#108957=AXIS2_PLACEMENT_3D('',#247452,#135985,#135986);
#108958=AXIS2_PLACEMENT_3D('',#247453,#135987,#135988);
#108959=AXIS2_PLACEMENT_3D('',#247454,#135989,#135990);
#108960=AXIS2_PLACEMENT_3D('',#247455,#135991,#135992);
#108961=AXIS2_PLACEMENT_3D('',#247456,#135993,#135994);
#108962=AXIS2_PLACEMENT_3D('',#247469,#135995,#135996);
#108963=AXIS2_PLACEMENT_3D('',#247470,#135997,#135998);
#108964=AXIS2_PLACEMENT_3D('',#247471,#135999,#136000);
#108965=AXIS2_PLACEMENT_3D('',#247472,#136001,#136002);
#108966=AXIS2_PLACEMENT_3D('',#247473,#136003,#136004);
#108967=AXIS2_PLACEMENT_3D('',#247486,#136005,#136006);
#108968=AXIS2_PLACEMENT_3D('',#247499,#136007,#136008);
#108969=AXIS2_PLACEMENT_3D('',#247500,#136009,#136010);
#108970=AXIS2_PLACEMENT_3D('',#247501,#136011,#136012);
#108971=AXIS2_PLACEMENT_3D('',#247502,#136013,#136014);
#108972=AXIS2_PLACEMENT_3D('',#247503,#136015,#136016);
#108973=AXIS2_PLACEMENT_3D('',#247522,#136017,#136018);
#108974=AXIS2_PLACEMENT_3D('',#247523,#136019,#136020);
#108975=AXIS2_PLACEMENT_3D('',#247524,#136021,#136022);
#108976=AXIS2_PLACEMENT_3D('',#247525,#136023,#136024);
#108977=AXIS2_PLACEMENT_3D('',#247526,#136025,#136026);
#108978=AXIS2_PLACEMENT_3D('',#247539,#136027,#136028);
#108979=AXIS2_PLACEMENT_3D('',#247558,#136029,#136030);
#108980=AXIS2_PLACEMENT_3D('',#247559,#136031,#136032);
#108981=AXIS2_PLACEMENT_3D('',#247560,#136033,#136034);
#108982=AXIS2_PLACEMENT_3D('',#247561,#136035,#136036);
#108983=AXIS2_PLACEMENT_3D('',#247562,#136037,#136038);
#108984=AXIS2_PLACEMENT_3D('',#247581,#136039,#136040);
#108985=AXIS2_PLACEMENT_3D('',#247594,#136041,#136042);
#108986=AXIS2_PLACEMENT_3D('',#247595,#136043,#136044);
#108987=AXIS2_PLACEMENT_3D('',#247596,#136045,#136046);
#108988=AXIS2_PLACEMENT_3D('',#247597,#136047,#136048);
#108989=AXIS2_PLACEMENT_3D('',#247598,#136049,#136050);
#108990=AXIS2_PLACEMENT_3D('',#247617,#136051,#136052);
#108991=AXIS2_PLACEMENT_3D('',#247618,#136053,#136054);
#108992=AXIS2_PLACEMENT_3D('',#247619,#136055,#136056);
#108993=AXIS2_PLACEMENT_3D('',#247620,#136057,#136058);
#108994=AXIS2_PLACEMENT_3D('',#247621,#136059,#136060);
#108995=AXIS2_PLACEMENT_3D('',#247634,#136061,#136062);
#108996=AXIS2_PLACEMENT_3D('',#247647,#136063,#136064);
#108997=AXIS2_PLACEMENT_3D('',#247648,#136065,#136066);
#108998=AXIS2_PLACEMENT_3D('',#247649,#136067,#136068);
#108999=AXIS2_PLACEMENT_3D('',#247650,#136069,#136070);
#109000=AXIS2_PLACEMENT_3D('',#247651,#136071,#136072);
#109001=AXIS2_PLACEMENT_3D('',#247664,#136073,#136074);
#109002=AXIS2_PLACEMENT_3D('',#247665,#136075,#136076);
#109003=AXIS2_PLACEMENT_3D('',#247666,#136077,#136078);
#109004=AXIS2_PLACEMENT_3D('',#247667,#136079,#136080);
#109005=AXIS2_PLACEMENT_3D('',#247668,#136081,#136082);
#109006=AXIS2_PLACEMENT_3D('',#247681,#136083,#136084);
#109007=AXIS2_PLACEMENT_3D('',#247682,#136085,#136086);
#109008=AXIS2_PLACEMENT_3D('',#247683,#136087,#136088);
#109009=AXIS2_PLACEMENT_3D('',#247684,#136089,#136090);
#109010=AXIS2_PLACEMENT_3D('',#247685,#136091,#136092);
#109011=AXIS2_PLACEMENT_3D('',#247698,#136093,#136094);
#109012=AXIS2_PLACEMENT_3D('',#247711,#136095,#136096);
#109013=AXIS2_PLACEMENT_3D('',#247712,#136097,#136098);
#109014=AXIS2_PLACEMENT_3D('',#247713,#136099,#136100);
#109015=AXIS2_PLACEMENT_3D('',#247714,#136101,#136102);
#109016=AXIS2_PLACEMENT_3D('',#247715,#136103,#136104);
#109017=AXIS2_PLACEMENT_3D('',#247734,#136105,#136106);
#109018=AXIS2_PLACEMENT_3D('',#247735,#136107,#136108);
#109019=AXIS2_PLACEMENT_3D('',#247736,#136109,#136110);
#109020=AXIS2_PLACEMENT_3D('',#247737,#136111,#136112);
#109021=AXIS2_PLACEMENT_3D('',#247738,#136113,#136114);
#109022=AXIS2_PLACEMENT_3D('',#247751,#136115,#136116);
#109023=AXIS2_PLACEMENT_3D('',#247770,#136117,#136118);
#109024=AXIS2_PLACEMENT_3D('',#247771,#136119,#136120);
#109025=AXIS2_PLACEMENT_3D('',#247772,#136121,#136122);
#109026=AXIS2_PLACEMENT_3D('',#247773,#136123,#136124);
#109027=AXIS2_PLACEMENT_3D('',#247774,#136125,#136126);
#109028=AXIS2_PLACEMENT_3D('',#247793,#136127,#136128);
#109029=AXIS2_PLACEMENT_3D('',#247806,#136129,#136130);
#109030=AXIS2_PLACEMENT_3D('',#247807,#136131,#136132);
#109031=AXIS2_PLACEMENT_3D('',#247808,#136133,#136134);
#109032=AXIS2_PLACEMENT_3D('',#247809,#136135,#136136);
#109033=AXIS2_PLACEMENT_3D('',#247810,#136137,#136138);
#109034=AXIS2_PLACEMENT_3D('',#247829,#136139,#136140);
#109035=AXIS2_PLACEMENT_3D('',#247830,#136141,#136142);
#109036=AXIS2_PLACEMENT_3D('',#247831,#136143,#136144);
#109037=AXIS2_PLACEMENT_3D('',#247832,#136145,#136146);
#109038=AXIS2_PLACEMENT_3D('',#247833,#136147,#136148);
#109039=AXIS2_PLACEMENT_3D('',#247846,#136149,#136150);
#109040=AXIS2_PLACEMENT_3D('',#247859,#136151,#136152);
#109041=AXIS2_PLACEMENT_3D('',#247860,#136153,#136154);
#109042=AXIS2_PLACEMENT_3D('',#247861,#136155,#136156);
#109043=AXIS2_PLACEMENT_3D('',#247862,#136157,#136158);
#109044=AXIS2_PLACEMENT_3D('',#247863,#136159,#136160);
#109045=AXIS2_PLACEMENT_3D('',#247876,#136161,#136162);
#109046=AXIS2_PLACEMENT_3D('',#247877,#136163,#136164);
#109047=AXIS2_PLACEMENT_3D('',#247878,#136165,#136166);
#109048=AXIS2_PLACEMENT_3D('',#247879,#136167,#136168);
#109049=AXIS2_PLACEMENT_3D('',#247880,#136169,#136170);
#109050=AXIS2_PLACEMENT_3D('',#247893,#136171,#136172);
#109051=AXIS2_PLACEMENT_3D('',#247894,#136173,#136174);
#109052=AXIS2_PLACEMENT_3D('',#247895,#136175,#136176);
#109053=AXIS2_PLACEMENT_3D('',#247896,#136177,#136178);
#109054=AXIS2_PLACEMENT_3D('',#247897,#136179,#136180);
#109055=AXIS2_PLACEMENT_3D('',#247910,#136181,#136182);
#109056=AXIS2_PLACEMENT_3D('',#247923,#136183,#136184);
#109057=AXIS2_PLACEMENT_3D('',#247924,#136185,#136186);
#109058=AXIS2_PLACEMENT_3D('',#247925,#136187,#136188);
#109059=AXIS2_PLACEMENT_3D('',#247926,#136189,#136190);
#109060=AXIS2_PLACEMENT_3D('',#247927,#136191,#136192);
#109061=AXIS2_PLACEMENT_3D('',#247946,#136193,#136194);
#109062=AXIS2_PLACEMENT_3D('',#247947,#136195,#136196);
#109063=AXIS2_PLACEMENT_3D('',#247948,#136197,#136198);
#109064=AXIS2_PLACEMENT_3D('',#247949,#136199,#136200);
#109065=AXIS2_PLACEMENT_3D('',#247950,#136201,#136202);
#109066=AXIS2_PLACEMENT_3D('',#247963,#136203,#136204);
#109067=AXIS2_PLACEMENT_3D('',#247982,#136205,#136206);
#109068=AXIS2_PLACEMENT_3D('',#247983,#136207,#136208);
#109069=AXIS2_PLACEMENT_3D('',#247984,#136209,#136210);
#109070=AXIS2_PLACEMENT_3D('',#247985,#136211,#136212);
#109071=AXIS2_PLACEMENT_3D('',#247986,#136213,#136214);
#109072=AXIS2_PLACEMENT_3D('',#248005,#136215,#136216);
#109073=AXIS2_PLACEMENT_3D('',#248018,#136217,#136218);
#109074=AXIS2_PLACEMENT_3D('',#248019,#136219,#136220);
#109075=AXIS2_PLACEMENT_3D('',#248020,#136221,#136222);
#109076=AXIS2_PLACEMENT_3D('',#248021,#136223,#136224);
#109077=AXIS2_PLACEMENT_3D('',#248022,#136225,#136226);
#109078=AXIS2_PLACEMENT_3D('',#248041,#136227,#136228);
#109079=AXIS2_PLACEMENT_3D('',#248042,#136229,#136230);
#109080=AXIS2_PLACEMENT_3D('',#248043,#136231,#136232);
#109081=AXIS2_PLACEMENT_3D('',#248044,#136233,#136234);
#109082=AXIS2_PLACEMENT_3D('',#248045,#136235,#136236);
#109083=AXIS2_PLACEMENT_3D('',#248058,#136237,#136238);
#109084=AXIS2_PLACEMENT_3D('',#248071,#136239,#136240);
#109085=AXIS2_PLACEMENT_3D('',#248072,#136241,#136242);
#109086=AXIS2_PLACEMENT_3D('',#248073,#136243,#136244);
#109087=AXIS2_PLACEMENT_3D('',#248074,#136245,#136246);
#109088=AXIS2_PLACEMENT_3D('',#248075,#136247,#136248);
#109089=AXIS2_PLACEMENT_3D('',#248088,#136249,#136250);
#109090=AXIS2_PLACEMENT_3D('',#248089,#136251,#136252);
#109091=AXIS2_PLACEMENT_3D('',#248090,#136253,#136254);
#109092=AXIS2_PLACEMENT_3D('',#248091,#136255,#136256);
#109093=AXIS2_PLACEMENT_3D('',#248092,#136257,#136258);
#109094=AXIS2_PLACEMENT_3D('',#248105,#136259,#136260);
#109095=AXIS2_PLACEMENT_3D('',#248106,#136261,#136262);
#109096=AXIS2_PLACEMENT_3D('',#248107,#136263,#136264);
#109097=AXIS2_PLACEMENT_3D('',#248108,#136265,#136266);
#109098=AXIS2_PLACEMENT_3D('',#248109,#136267,#136268);
#109099=AXIS2_PLACEMENT_3D('',#248122,#136269,#136270);
#109100=AXIS2_PLACEMENT_3D('',#248135,#136271,#136272);
#109101=AXIS2_PLACEMENT_3D('',#248136,#136273,#136274);
#109102=AXIS2_PLACEMENT_3D('',#248137,#136275,#136276);
#109103=AXIS2_PLACEMENT_3D('',#248138,#136277,#136278);
#109104=AXIS2_PLACEMENT_3D('',#248139,#136279,#136280);
#109105=AXIS2_PLACEMENT_3D('',#248158,#136281,#136282);
#109106=AXIS2_PLACEMENT_3D('',#248159,#136283,#136284);
#109107=AXIS2_PLACEMENT_3D('',#248160,#136285,#136286);
#109108=AXIS2_PLACEMENT_3D('',#248161,#136287,#136288);
#109109=AXIS2_PLACEMENT_3D('',#248162,#136289,#136290);
#109110=AXIS2_PLACEMENT_3D('',#248175,#136291,#136292);
#109111=AXIS2_PLACEMENT_3D('',#248194,#136293,#136294);
#109112=AXIS2_PLACEMENT_3D('',#248195,#136295,#136296);
#109113=AXIS2_PLACEMENT_3D('',#248196,#136297,#136298);
#109114=AXIS2_PLACEMENT_3D('',#248197,#136299,#136300);
#109115=AXIS2_PLACEMENT_3D('',#248198,#136301,#136302);
#109116=AXIS2_PLACEMENT_3D('',#248217,#136303,#136304);
#109117=AXIS2_PLACEMENT_3D('',#248230,#136305,#136306);
#109118=AXIS2_PLACEMENT_3D('',#248231,#136307,#136308);
#109119=AXIS2_PLACEMENT_3D('',#248232,#136309,#136310);
#109120=AXIS2_PLACEMENT_3D('',#248233,#136311,#136312);
#109121=AXIS2_PLACEMENT_3D('',#248234,#136313,#136314);
#109122=AXIS2_PLACEMENT_3D('',#248253,#136315,#136316);
#109123=AXIS2_PLACEMENT_3D('',#248254,#136317,#136318);
#109124=AXIS2_PLACEMENT_3D('',#248255,#136319,#136320);
#109125=AXIS2_PLACEMENT_3D('',#248256,#136321,#136322);
#109126=AXIS2_PLACEMENT_3D('',#248257,#136323,#136324);
#109127=AXIS2_PLACEMENT_3D('',#248270,#136325,#136326);
#109128=AXIS2_PLACEMENT_3D('',#248283,#136327,#136328);
#109129=AXIS2_PLACEMENT_3D('',#248284,#136329,#136330);
#109130=AXIS2_PLACEMENT_3D('',#248285,#136331,#136332);
#109131=AXIS2_PLACEMENT_3D('',#248286,#136333,#136334);
#109132=AXIS2_PLACEMENT_3D('',#248287,#136335,#136336);
#109133=AXIS2_PLACEMENT_3D('',#248300,#136337,#136338);
#109134=AXIS2_PLACEMENT_3D('',#248301,#136339,#136340);
#109135=AXIS2_PLACEMENT_3D('',#248302,#136341,#136342);
#109136=AXIS2_PLACEMENT_3D('',#248303,#136343,#136344);
#109137=AXIS2_PLACEMENT_3D('',#248304,#136345,#136346);
#109138=AXIS2_PLACEMENT_3D('',#248317,#136347,#136348);
#109139=AXIS2_PLACEMENT_3D('',#248318,#136349,#136350);
#109140=AXIS2_PLACEMENT_3D('',#248319,#136351,#136352);
#109141=AXIS2_PLACEMENT_3D('',#248320,#136353,#136354);
#109142=AXIS2_PLACEMENT_3D('',#248321,#136355,#136356);
#109143=AXIS2_PLACEMENT_3D('',#248334,#136357,#136358);
#109144=AXIS2_PLACEMENT_3D('',#248347,#136359,#136360);
#109145=AXIS2_PLACEMENT_3D('',#248348,#136361,#136362);
#109146=AXIS2_PLACEMENT_3D('',#248349,#136363,#136364);
#109147=AXIS2_PLACEMENT_3D('',#248350,#136365,#136366);
#109148=AXIS2_PLACEMENT_3D('',#248351,#136367,#136368);
#109149=AXIS2_PLACEMENT_3D('',#248370,#136369,#136370);
#109150=AXIS2_PLACEMENT_3D('',#248371,#136371,#136372);
#109151=AXIS2_PLACEMENT_3D('',#248372,#136373,#136374);
#109152=AXIS2_PLACEMENT_3D('',#248373,#136375,#136376);
#109153=AXIS2_PLACEMENT_3D('',#248374,#136377,#136378);
#109154=AXIS2_PLACEMENT_3D('',#248387,#136379,#136380);
#109155=AXIS2_PLACEMENT_3D('',#248406,#136381,#136382);
#109156=AXIS2_PLACEMENT_3D('',#248407,#136383,#136384);
#109157=AXIS2_PLACEMENT_3D('',#248408,#136385,#136386);
#109158=AXIS2_PLACEMENT_3D('',#248409,#136387,#136388);
#109159=AXIS2_PLACEMENT_3D('',#248410,#136389,#136390);
#109160=AXIS2_PLACEMENT_3D('',#248429,#136391,#136392);
#109161=AXIS2_PLACEMENT_3D('',#248442,#136393,#136394);
#109162=AXIS2_PLACEMENT_3D('',#248443,#136395,#136396);
#109163=AXIS2_PLACEMENT_3D('',#248444,#136397,#136398);
#109164=AXIS2_PLACEMENT_3D('',#248445,#136399,#136400);
#109165=AXIS2_PLACEMENT_3D('',#248446,#136401,#136402);
#109166=AXIS2_PLACEMENT_3D('',#248465,#136403,#136404);
#109167=AXIS2_PLACEMENT_3D('',#248466,#136405,#136406);
#109168=AXIS2_PLACEMENT_3D('',#248467,#136407,#136408);
#109169=AXIS2_PLACEMENT_3D('',#248468,#136409,#136410);
#109170=AXIS2_PLACEMENT_3D('',#248469,#136411,#136412);
#109171=AXIS2_PLACEMENT_3D('',#248482,#136413,#136414);
#109172=AXIS2_PLACEMENT_3D('',#248495,#136415,#136416);
#109173=AXIS2_PLACEMENT_3D('',#248496,#136417,#136418);
#109174=AXIS2_PLACEMENT_3D('',#248497,#136419,#136420);
#109175=AXIS2_PLACEMENT_3D('',#248498,#136421,#136422);
#109176=AXIS2_PLACEMENT_3D('',#248499,#136423,#136424);
#109177=AXIS2_PLACEMENT_3D('',#248512,#136425,#136426);
#109178=AXIS2_PLACEMENT_3D('',#248513,#136427,#136428);
#109179=AXIS2_PLACEMENT_3D('',#248514,#136429,#136430);
#109180=AXIS2_PLACEMENT_3D('',#248515,#136431,#136432);
#109181=AXIS2_PLACEMENT_3D('',#248516,#136433,#136434);
#109182=AXIS2_PLACEMENT_3D('',#248529,#136435,#136436);
#109183=AXIS2_PLACEMENT_3D('',#248530,#136437,#136438);
#109184=AXIS2_PLACEMENT_3D('',#248531,#136439,#136440);
#109185=AXIS2_PLACEMENT_3D('',#248532,#136441,#136442);
#109186=AXIS2_PLACEMENT_3D('',#248533,#136443,#136444);
#109187=AXIS2_PLACEMENT_3D('',#248546,#136445,#136446);
#109188=AXIS2_PLACEMENT_3D('',#248559,#136447,#136448);
#109189=AXIS2_PLACEMENT_3D('',#248560,#136449,#136450);
#109190=AXIS2_PLACEMENT_3D('',#248561,#136451,#136452);
#109191=AXIS2_PLACEMENT_3D('',#248562,#136453,#136454);
#109192=AXIS2_PLACEMENT_3D('',#248563,#136455,#136456);
#109193=AXIS2_PLACEMENT_3D('',#248582,#136457,#136458);
#109194=AXIS2_PLACEMENT_3D('',#248583,#136459,#136460);
#109195=AXIS2_PLACEMENT_3D('',#248584,#136461,#136462);
#109196=AXIS2_PLACEMENT_3D('',#248585,#136463,#136464);
#109197=AXIS2_PLACEMENT_3D('',#248586,#136465,#136466);
#109198=AXIS2_PLACEMENT_3D('',#248599,#136467,#136468);
#109199=AXIS2_PLACEMENT_3D('',#248618,#136469,#136470);
#109200=AXIS2_PLACEMENT_3D('',#248619,#136471,#136472);
#109201=AXIS2_PLACEMENT_3D('',#248620,#136473,#136474);
#109202=AXIS2_PLACEMENT_3D('',#248621,#136475,#136476);
#109203=AXIS2_PLACEMENT_3D('',#248622,#136477,#136478);
#109204=AXIS2_PLACEMENT_3D('',#248641,#136479,#136480);
#109205=AXIS2_PLACEMENT_3D('',#248654,#136481,#136482);
#109206=AXIS2_PLACEMENT_3D('',#248655,#136483,#136484);
#109207=AXIS2_PLACEMENT_3D('',#248656,#136485,#136486);
#109208=AXIS2_PLACEMENT_3D('',#248657,#136487,#136488);
#109209=AXIS2_PLACEMENT_3D('',#248658,#136489,#136490);
#109210=AXIS2_PLACEMENT_3D('',#248677,#136491,#136492);
#109211=AXIS2_PLACEMENT_3D('',#248678,#136493,#136494);
#109212=AXIS2_PLACEMENT_3D('',#248679,#136495,#136496);
#109213=AXIS2_PLACEMENT_3D('',#248680,#136497,#136498);
#109214=AXIS2_PLACEMENT_3D('',#248681,#136499,#136500);
#109215=AXIS2_PLACEMENT_3D('',#248694,#136501,#136502);
#109216=AXIS2_PLACEMENT_3D('',#248707,#136503,#136504);
#109217=AXIS2_PLACEMENT_3D('',#248708,#136505,#136506);
#109218=AXIS2_PLACEMENT_3D('',#248709,#136507,#136508);
#109219=AXIS2_PLACEMENT_3D('',#248710,#136509,#136510);
#109220=AXIS2_PLACEMENT_3D('',#248711,#136511,#136512);
#109221=AXIS2_PLACEMENT_3D('',#248724,#136513,#136514);
#109222=AXIS2_PLACEMENT_3D('',#248725,#136515,#136516);
#109223=AXIS2_PLACEMENT_3D('',#248726,#136517,#136518);
#109224=AXIS2_PLACEMENT_3D('',#248727,#136519,#136520);
#109225=AXIS2_PLACEMENT_3D('',#248728,#136521,#136522);
#109226=AXIS2_PLACEMENT_3D('',#248741,#136523,#136524);
#109227=AXIS2_PLACEMENT_3D('',#248742,#136525,#136526);
#109228=AXIS2_PLACEMENT_3D('',#248743,#136527,#136528);
#109229=AXIS2_PLACEMENT_3D('',#248744,#136529,#136530);
#109230=AXIS2_PLACEMENT_3D('',#248745,#136531,#136532);
#109231=AXIS2_PLACEMENT_3D('',#248758,#136533,#136534);
#109232=AXIS2_PLACEMENT_3D('',#248771,#136535,#136536);
#109233=AXIS2_PLACEMENT_3D('',#248772,#136537,#136538);
#109234=AXIS2_PLACEMENT_3D('',#248773,#136539,#136540);
#109235=AXIS2_PLACEMENT_3D('',#248774,#136541,#136542);
#109236=AXIS2_PLACEMENT_3D('',#248775,#136543,#136544);
#109237=AXIS2_PLACEMENT_3D('',#248794,#136545,#136546);
#109238=AXIS2_PLACEMENT_3D('',#248795,#136547,#136548);
#109239=AXIS2_PLACEMENT_3D('',#248796,#136549,#136550);
#109240=AXIS2_PLACEMENT_3D('',#248797,#136551,#136552);
#109241=AXIS2_PLACEMENT_3D('',#248798,#136553,#136554);
#109242=AXIS2_PLACEMENT_3D('',#248811,#136555,#136556);
#109243=AXIS2_PLACEMENT_3D('',#248830,#136557,#136558);
#109244=AXIS2_PLACEMENT_3D('',#248831,#136559,#136560);
#109245=AXIS2_PLACEMENT_3D('',#248832,#136561,#136562);
#109246=AXIS2_PLACEMENT_3D('',#248833,#136563,#136564);
#109247=AXIS2_PLACEMENT_3D('',#248834,#136565,#136566);
#109248=AXIS2_PLACEMENT_3D('',#248853,#136567,#136568);
#109249=AXIS2_PLACEMENT_3D('',#248866,#136569,#136570);
#109250=AXIS2_PLACEMENT_3D('',#248867,#136571,#136572);
#109251=AXIS2_PLACEMENT_3D('',#248868,#136573,#136574);
#109252=AXIS2_PLACEMENT_3D('',#248869,#136575,#136576);
#109253=AXIS2_PLACEMENT_3D('',#248870,#136577,#136578);
#109254=AXIS2_PLACEMENT_3D('',#248889,#136579,#136580);
#109255=AXIS2_PLACEMENT_3D('',#248890,#136581,#136582);
#109256=AXIS2_PLACEMENT_3D('',#248891,#136583,#136584);
#109257=AXIS2_PLACEMENT_3D('',#248892,#136585,#136586);
#109258=AXIS2_PLACEMENT_3D('',#248893,#136587,#136588);
#109259=AXIS2_PLACEMENT_3D('',#248906,#136589,#136590);
#109260=AXIS2_PLACEMENT_3D('',#248919,#136591,#136592);
#109261=AXIS2_PLACEMENT_3D('',#248920,#136593,#136594);
#109262=AXIS2_PLACEMENT_3D('',#248921,#136595,#136596);
#109263=AXIS2_PLACEMENT_3D('',#248922,#136597,#136598);
#109264=AXIS2_PLACEMENT_3D('',#248923,#136599,#136600);
#109265=AXIS2_PLACEMENT_3D('',#248936,#136601,#136602);
#109266=AXIS2_PLACEMENT_3D('',#248937,#136603,#136604);
#109267=AXIS2_PLACEMENT_3D('',#248938,#136605,#136606);
#109268=AXIS2_PLACEMENT_3D('',#248939,#136607,#136608);
#109269=AXIS2_PLACEMENT_3D('',#248940,#136609,#136610);
#109270=AXIS2_PLACEMENT_3D('',#248953,#136611,#136612);
#109271=AXIS2_PLACEMENT_3D('',#248954,#136613,#136614);
#109272=AXIS2_PLACEMENT_3D('',#248955,#136615,#136616);
#109273=AXIS2_PLACEMENT_3D('',#248956,#136617,#136618);
#109274=AXIS2_PLACEMENT_3D('',#248957,#136619,#136620);
#109275=AXIS2_PLACEMENT_3D('',#248970,#136621,#136622);
#109276=AXIS2_PLACEMENT_3D('',#248983,#136623,#136624);
#109277=AXIS2_PLACEMENT_3D('',#248984,#136625,#136626);
#109278=AXIS2_PLACEMENT_3D('',#248985,#136627,#136628);
#109279=AXIS2_PLACEMENT_3D('',#248986,#136629,#136630);
#109280=AXIS2_PLACEMENT_3D('',#248987,#136631,#136632);
#109281=AXIS2_PLACEMENT_3D('',#249006,#136633,#136634);
#109282=AXIS2_PLACEMENT_3D('',#249007,#136635,#136636);
#109283=AXIS2_PLACEMENT_3D('',#249008,#136637,#136638);
#109284=AXIS2_PLACEMENT_3D('',#249009,#136639,#136640);
#109285=AXIS2_PLACEMENT_3D('',#249010,#136641,#136642);
#109286=AXIS2_PLACEMENT_3D('',#249023,#136643,#136644);
#109287=AXIS2_PLACEMENT_3D('',#249042,#136645,#136646);
#109288=AXIS2_PLACEMENT_3D('',#249043,#136647,#136648);
#109289=AXIS2_PLACEMENT_3D('',#249044,#136649,#136650);
#109290=AXIS2_PLACEMENT_3D('',#249045,#136651,#136652);
#109291=AXIS2_PLACEMENT_3D('',#249046,#136653,#136654);
#109292=AXIS2_PLACEMENT_3D('',#249065,#136655,#136656);
#109293=AXIS2_PLACEMENT_3D('',#249078,#136657,#136658);
#109294=AXIS2_PLACEMENT_3D('',#249079,#136659,#136660);
#109295=AXIS2_PLACEMENT_3D('',#249080,#136661,#136662);
#109296=AXIS2_PLACEMENT_3D('',#249081,#136663,#136664);
#109297=AXIS2_PLACEMENT_3D('',#249082,#136665,#136666);
#109298=AXIS2_PLACEMENT_3D('',#249101,#136667,#136668);
#109299=AXIS2_PLACEMENT_3D('',#249102,#136669,#136670);
#109300=AXIS2_PLACEMENT_3D('',#249103,#136671,#136672);
#109301=AXIS2_PLACEMENT_3D('',#249104,#136673,#136674);
#109302=AXIS2_PLACEMENT_3D('',#249105,#136675,#136676);
#109303=AXIS2_PLACEMENT_3D('',#249118,#136677,#136678);
#109304=AXIS2_PLACEMENT_3D('',#249131,#136679,#136680);
#109305=AXIS2_PLACEMENT_3D('',#249132,#136681,#136682);
#109306=AXIS2_PLACEMENT_3D('',#249133,#136683,#136684);
#109307=AXIS2_PLACEMENT_3D('',#249134,#136685,#136686);
#109308=AXIS2_PLACEMENT_3D('',#249135,#136687,#136688);
#109309=AXIS2_PLACEMENT_3D('',#249148,#136689,#136690);
#109310=AXIS2_PLACEMENT_3D('',#249149,#136691,#136692);
#109311=AXIS2_PLACEMENT_3D('',#249150,#136693,#136694);
#109312=AXIS2_PLACEMENT_3D('',#249151,#136695,#136696);
#109313=AXIS2_PLACEMENT_3D('',#249152,#136697,#136698);
#109314=AXIS2_PLACEMENT_3D('',#249165,#136699,#136700);
#109315=AXIS2_PLACEMENT_3D('',#249166,#136701,#136702);
#109316=AXIS2_PLACEMENT_3D('',#249167,#136703,#136704);
#109317=AXIS2_PLACEMENT_3D('',#249168,#136705,#136706);
#109318=AXIS2_PLACEMENT_3D('',#249169,#136707,#136708);
#109319=AXIS2_PLACEMENT_3D('',#249182,#136709,#136710);
#109320=AXIS2_PLACEMENT_3D('',#249195,#136711,#136712);
#109321=AXIS2_PLACEMENT_3D('',#249196,#136713,#136714);
#109322=AXIS2_PLACEMENT_3D('',#249197,#136715,#136716);
#109323=AXIS2_PLACEMENT_3D('',#249198,#136717,#136718);
#109324=AXIS2_PLACEMENT_3D('',#249199,#136719,#136720);
#109325=AXIS2_PLACEMENT_3D('',#249218,#136721,#136722);
#109326=AXIS2_PLACEMENT_3D('',#249219,#136723,#136724);
#109327=AXIS2_PLACEMENT_3D('',#249220,#136725,#136726);
#109328=AXIS2_PLACEMENT_3D('',#249221,#136727,#136728);
#109329=AXIS2_PLACEMENT_3D('',#249222,#136729,#136730);
#109330=AXIS2_PLACEMENT_3D('',#249235,#136731,#136732);
#109331=AXIS2_PLACEMENT_3D('',#249254,#136733,#136734);
#109332=AXIS2_PLACEMENT_3D('',#249255,#136735,#136736);
#109333=AXIS2_PLACEMENT_3D('',#249256,#136737,#136738);
#109334=AXIS2_PLACEMENT_3D('',#249257,#136739,#136740);
#109335=AXIS2_PLACEMENT_3D('',#249258,#136741,#136742);
#109336=AXIS2_PLACEMENT_3D('',#249277,#136743,#136744);
#109337=AXIS2_PLACEMENT_3D('',#249290,#136745,#136746);
#109338=AXIS2_PLACEMENT_3D('',#249291,#136747,#136748);
#109339=AXIS2_PLACEMENT_3D('',#249292,#136749,#136750);
#109340=AXIS2_PLACEMENT_3D('',#249293,#136751,#136752);
#109341=AXIS2_PLACEMENT_3D('',#249294,#136753,#136754);
#109342=AXIS2_PLACEMENT_3D('',#249313,#136755,#136756);
#109343=AXIS2_PLACEMENT_3D('',#249314,#136757,#136758);
#109344=AXIS2_PLACEMENT_3D('',#249315,#136759,#136760);
#109345=AXIS2_PLACEMENT_3D('',#249316,#136761,#136762);
#109346=AXIS2_PLACEMENT_3D('',#249317,#136763,#136764);
#109347=AXIS2_PLACEMENT_3D('',#249330,#136765,#136766);
#109348=AXIS2_PLACEMENT_3D('',#249343,#136767,#136768);
#109349=AXIS2_PLACEMENT_3D('',#249344,#136769,#136770);
#109350=AXIS2_PLACEMENT_3D('',#249345,#136771,#136772);
#109351=AXIS2_PLACEMENT_3D('',#249346,#136773,#136774);
#109352=AXIS2_PLACEMENT_3D('',#249347,#136775,#136776);
#109353=AXIS2_PLACEMENT_3D('',#249360,#136777,#136778);
#109354=AXIS2_PLACEMENT_3D('',#249361,#136779,#136780);
#109355=AXIS2_PLACEMENT_3D('',#249362,#136781,#136782);
#109356=AXIS2_PLACEMENT_3D('',#249363,#136783,#136784);
#109357=AXIS2_PLACEMENT_3D('',#249364,#136785,#136786);
#109358=AXIS2_PLACEMENT_3D('',#249377,#136787,#136788);
#109359=AXIS2_PLACEMENT_3D('',#249378,#136789,#136790);
#109360=AXIS2_PLACEMENT_3D('',#249379,#136791,#136792);
#109361=AXIS2_PLACEMENT_3D('',#249380,#136793,#136794);
#109362=AXIS2_PLACEMENT_3D('',#249381,#136795,#136796);
#109363=AXIS2_PLACEMENT_3D('',#249394,#136797,#136798);
#109364=AXIS2_PLACEMENT_3D('',#249407,#136799,#136800);
#109365=AXIS2_PLACEMENT_3D('',#249408,#136801,#136802);
#109366=AXIS2_PLACEMENT_3D('',#249409,#136803,#136804);
#109367=AXIS2_PLACEMENT_3D('',#249410,#136805,#136806);
#109368=AXIS2_PLACEMENT_3D('',#249411,#136807,#136808);
#109369=AXIS2_PLACEMENT_3D('',#249430,#136809,#136810);
#109370=AXIS2_PLACEMENT_3D('',#249431,#136811,#136812);
#109371=AXIS2_PLACEMENT_3D('',#249432,#136813,#136814);
#109372=AXIS2_PLACEMENT_3D('',#249433,#136815,#136816);
#109373=AXIS2_PLACEMENT_3D('',#249434,#136817,#136818);
#109374=AXIS2_PLACEMENT_3D('',#249447,#136819,#136820);
#109375=AXIS2_PLACEMENT_3D('',#249466,#136821,#136822);
#109376=AXIS2_PLACEMENT_3D('',#249467,#136823,#136824);
#109377=AXIS2_PLACEMENT_3D('',#249468,#136825,#136826);
#109378=AXIS2_PLACEMENT_3D('',#249469,#136827,#136828);
#109379=AXIS2_PLACEMENT_3D('',#249470,#136829,#136830);
#109380=AXIS2_PLACEMENT_3D('',#249489,#136831,#136832);
#109381=AXIS2_PLACEMENT_3D('',#249502,#136833,#136834);
#109382=AXIS2_PLACEMENT_3D('',#249503,#136835,#136836);
#109383=AXIS2_PLACEMENT_3D('',#249504,#136837,#136838);
#109384=AXIS2_PLACEMENT_3D('',#249505,#136839,#136840);
#109385=AXIS2_PLACEMENT_3D('',#249506,#136841,#136842);
#109386=AXIS2_PLACEMENT_3D('',#249525,#136843,#136844);
#109387=AXIS2_PLACEMENT_3D('',#249526,#136845,#136846);
#109388=AXIS2_PLACEMENT_3D('',#249527,#136847,#136848);
#109389=AXIS2_PLACEMENT_3D('',#249528,#136849,#136850);
#109390=AXIS2_PLACEMENT_3D('',#249529,#136851,#136852);
#109391=AXIS2_PLACEMENT_3D('',#249542,#136853,#136854);
#109392=AXIS2_PLACEMENT_3D('',#249555,#136855,#136856);
#109393=AXIS2_PLACEMENT_3D('',#249556,#136857,#136858);
#109394=AXIS2_PLACEMENT_3D('',#249557,#136859,#136860);
#109395=AXIS2_PLACEMENT_3D('',#249558,#136861,#136862);
#109396=AXIS2_PLACEMENT_3D('',#249559,#136863,#136864);
#109397=AXIS2_PLACEMENT_3D('',#249572,#136865,#136866);
#109398=AXIS2_PLACEMENT_3D('',#249573,#136867,#136868);
#109399=AXIS2_PLACEMENT_3D('',#249574,#136869,#136870);
#109400=AXIS2_PLACEMENT_3D('',#249575,#136871,#136872);
#109401=AXIS2_PLACEMENT_3D('',#249576,#136873,#136874);
#109402=AXIS2_PLACEMENT_3D('',#249589,#136875,#136876);
#109403=AXIS2_PLACEMENT_3D('',#249590,#136877,#136878);
#109404=AXIS2_PLACEMENT_3D('',#249591,#136879,#136880);
#109405=AXIS2_PLACEMENT_3D('',#249592,#136881,#136882);
#109406=AXIS2_PLACEMENT_3D('',#249593,#136883,#136884);
#109407=AXIS2_PLACEMENT_3D('',#249606,#136885,#136886);
#109408=AXIS2_PLACEMENT_3D('',#249619,#136887,#136888);
#109409=AXIS2_PLACEMENT_3D('',#249620,#136889,#136890);
#109410=AXIS2_PLACEMENT_3D('',#249621,#136891,#136892);
#109411=AXIS2_PLACEMENT_3D('',#249622,#136893,#136894);
#109412=AXIS2_PLACEMENT_3D('',#249623,#136895,#136896);
#109413=AXIS2_PLACEMENT_3D('',#249642,#136897,#136898);
#109414=AXIS2_PLACEMENT_3D('',#249643,#136899,#136900);
#109415=AXIS2_PLACEMENT_3D('',#249644,#136901,#136902);
#109416=AXIS2_PLACEMENT_3D('',#249645,#136903,#136904);
#109417=AXIS2_PLACEMENT_3D('',#249646,#136905,#136906);
#109418=AXIS2_PLACEMENT_3D('',#249659,#136907,#136908);
#109419=AXIS2_PLACEMENT_3D('',#249678,#136909,#136910);
#109420=AXIS2_PLACEMENT_3D('',#249679,#136911,#136912);
#109421=AXIS2_PLACEMENT_3D('',#249680,#136913,#136914);
#109422=AXIS2_PLACEMENT_3D('',#249681,#136915,#136916);
#109423=AXIS2_PLACEMENT_3D('',#249682,#136917,#136918);
#109424=AXIS2_PLACEMENT_3D('',#249701,#136919,#136920);
#109425=AXIS2_PLACEMENT_3D('',#249714,#136921,#136922);
#109426=AXIS2_PLACEMENT_3D('',#249715,#136923,#136924);
#109427=AXIS2_PLACEMENT_3D('',#249716,#136925,#136926);
#109428=AXIS2_PLACEMENT_3D('',#249717,#136927,#136928);
#109429=AXIS2_PLACEMENT_3D('',#249718,#136929,#136930);
#109430=AXIS2_PLACEMENT_3D('',#249737,#136931,#136932);
#109431=AXIS2_PLACEMENT_3D('',#249738,#136933,#136934);
#109432=AXIS2_PLACEMENT_3D('',#249739,#136935,#136936);
#109433=AXIS2_PLACEMENT_3D('',#249740,#136937,#136938);
#109434=AXIS2_PLACEMENT_3D('',#249741,#136939,#136940);
#109435=AXIS2_PLACEMENT_3D('',#249754,#136941,#136942);
#109436=AXIS2_PLACEMENT_3D('',#249767,#136943,#136944);
#109437=AXIS2_PLACEMENT_3D('',#249768,#136945,#136946);
#109438=AXIS2_PLACEMENT_3D('',#249769,#136947,#136948);
#109439=AXIS2_PLACEMENT_3D('',#249770,#136949,#136950);
#109440=AXIS2_PLACEMENT_3D('',#249771,#136951,#136952);
#109441=AXIS2_PLACEMENT_3D('',#249784,#136953,#136954);
#109442=AXIS2_PLACEMENT_3D('',#249785,#136955,#136956);
#109443=AXIS2_PLACEMENT_3D('',#249786,#136957,#136958);
#109444=AXIS2_PLACEMENT_3D('',#249787,#136959,#136960);
#109445=AXIS2_PLACEMENT_3D('',#249788,#136961,#136962);
#109446=AXIS2_PLACEMENT_3D('',#249801,#136963,#136964);
#109447=AXIS2_PLACEMENT_3D('',#249802,#136965,#136966);
#109448=AXIS2_PLACEMENT_3D('',#249803,#136967,#136968);
#109449=AXIS2_PLACEMENT_3D('',#249804,#136969,#136970);
#109450=AXIS2_PLACEMENT_3D('',#249805,#136971,#136972);
#109451=AXIS2_PLACEMENT_3D('',#249818,#136973,#136974);
#109452=AXIS2_PLACEMENT_3D('',#249831,#136975,#136976);
#109453=AXIS2_PLACEMENT_3D('',#249832,#136977,#136978);
#109454=AXIS2_PLACEMENT_3D('',#249833,#136979,#136980);
#109455=AXIS2_PLACEMENT_3D('',#249834,#136981,#136982);
#109456=AXIS2_PLACEMENT_3D('',#249835,#136983,#136984);
#109457=AXIS2_PLACEMENT_3D('',#249854,#136985,#136986);
#109458=AXIS2_PLACEMENT_3D('',#249855,#136987,#136988);
#109459=AXIS2_PLACEMENT_3D('',#249856,#136989,#136990);
#109460=AXIS2_PLACEMENT_3D('',#249857,#136991,#136992);
#109461=AXIS2_PLACEMENT_3D('',#249858,#136993,#136994);
#109462=AXIS2_PLACEMENT_3D('',#249871,#136995,#136996);
#109463=AXIS2_PLACEMENT_3D('',#249890,#136997,#136998);
#109464=AXIS2_PLACEMENT_3D('',#249891,#136999,#137000);
#109465=AXIS2_PLACEMENT_3D('',#249892,#137001,#137002);
#109466=AXIS2_PLACEMENT_3D('',#249893,#137003,#137004);
#109467=AXIS2_PLACEMENT_3D('',#249894,#137005,#137006);
#109468=AXIS2_PLACEMENT_3D('',#249913,#137007,#137008);
#109469=AXIS2_PLACEMENT_3D('',#249926,#137009,#137010);
#109470=AXIS2_PLACEMENT_3D('',#249927,#137011,#137012);
#109471=AXIS2_PLACEMENT_3D('',#249928,#137013,#137014);
#109472=AXIS2_PLACEMENT_3D('',#249929,#137015,#137016);
#109473=AXIS2_PLACEMENT_3D('',#249930,#137017,#137018);
#109474=AXIS2_PLACEMENT_3D('',#249949,#137019,#137020);
#109475=AXIS2_PLACEMENT_3D('',#249950,#137021,#137022);
#109476=AXIS2_PLACEMENT_3D('',#249951,#137023,#137024);
#109477=AXIS2_PLACEMENT_3D('',#249952,#137025,#137026);
#109478=AXIS2_PLACEMENT_3D('',#249953,#137027,#137028);
#109479=AXIS2_PLACEMENT_3D('',#249966,#137029,#137030);
#109480=AXIS2_PLACEMENT_3D('',#249979,#137031,#137032);
#109481=AXIS2_PLACEMENT_3D('',#249980,#137033,#137034);
#109482=AXIS2_PLACEMENT_3D('',#249981,#137035,#137036);
#109483=AXIS2_PLACEMENT_3D('',#249982,#137037,#137038);
#109484=AXIS2_PLACEMENT_3D('',#249983,#137039,#137040);
#109485=AXIS2_PLACEMENT_3D('',#249996,#137041,#137042);
#109486=AXIS2_PLACEMENT_3D('',#249997,#137043,#137044);
#109487=AXIS2_PLACEMENT_3D('',#249998,#137045,#137046);
#109488=AXIS2_PLACEMENT_3D('',#249999,#137047,#137048);
#109489=AXIS2_PLACEMENT_3D('',#250000,#137049,#137050);
#109490=AXIS2_PLACEMENT_3D('',#250013,#137051,#137052);
#109491=AXIS2_PLACEMENT_3D('',#250014,#137053,#137054);
#109492=AXIS2_PLACEMENT_3D('',#250015,#137055,#137056);
#109493=AXIS2_PLACEMENT_3D('',#250016,#137057,#137058);
#109494=AXIS2_PLACEMENT_3D('',#250017,#137059,#137060);
#109495=AXIS2_PLACEMENT_3D('',#250030,#137061,#137062);
#109496=AXIS2_PLACEMENT_3D('',#250043,#137063,#137064);
#109497=AXIS2_PLACEMENT_3D('',#250044,#137065,#137066);
#109498=AXIS2_PLACEMENT_3D('',#250045,#137067,#137068);
#109499=AXIS2_PLACEMENT_3D('',#250046,#137069,#137070);
#109500=AXIS2_PLACEMENT_3D('',#250047,#137071,#137072);
#109501=AXIS2_PLACEMENT_3D('',#250066,#137073,#137074);
#109502=AXIS2_PLACEMENT_3D('',#250067,#137075,#137076);
#109503=AXIS2_PLACEMENT_3D('',#250068,#137077,#137078);
#109504=AXIS2_PLACEMENT_3D('',#250069,#137079,#137080);
#109505=AXIS2_PLACEMENT_3D('',#250070,#137081,#137082);
#109506=AXIS2_PLACEMENT_3D('',#250083,#137083,#137084);
#109507=AXIS2_PLACEMENT_3D('',#250102,#137085,#137086);
#109508=AXIS2_PLACEMENT_3D('',#250103,#137087,#137088);
#109509=AXIS2_PLACEMENT_3D('',#250104,#137089,#137090);
#109510=AXIS2_PLACEMENT_3D('',#250105,#137091,#137092);
#109511=AXIS2_PLACEMENT_3D('',#250106,#137093,#137094);
#109512=AXIS2_PLACEMENT_3D('',#250125,#137095,#137096);
#109513=AXIS2_PLACEMENT_3D('',#250138,#137097,#137098);
#109514=AXIS2_PLACEMENT_3D('',#250139,#137099,#137100);
#109515=AXIS2_PLACEMENT_3D('',#250140,#137101,#137102);
#109516=AXIS2_PLACEMENT_3D('',#250141,#137103,#137104);
#109517=AXIS2_PLACEMENT_3D('',#250142,#137105,#137106);
#109518=AXIS2_PLACEMENT_3D('',#250161,#137107,#137108);
#109519=AXIS2_PLACEMENT_3D('',#250162,#137109,#137110);
#109520=AXIS2_PLACEMENT_3D('',#250163,#137111,#137112);
#109521=AXIS2_PLACEMENT_3D('',#250164,#137113,#137114);
#109522=AXIS2_PLACEMENT_3D('',#250165,#137115,#137116);
#109523=AXIS2_PLACEMENT_3D('',#250178,#137117,#137118);
#109524=AXIS2_PLACEMENT_3D('',#250191,#137119,#137120);
#109525=AXIS2_PLACEMENT_3D('',#250192,#137121,#137122);
#109526=AXIS2_PLACEMENT_3D('',#250193,#137123,#137124);
#109527=AXIS2_PLACEMENT_3D('',#250194,#137125,#137126);
#109528=AXIS2_PLACEMENT_3D('',#250195,#137127,#137128);
#109529=AXIS2_PLACEMENT_3D('',#250208,#137129,#137130);
#109530=AXIS2_PLACEMENT_3D('',#250209,#137131,#137132);
#109531=AXIS2_PLACEMENT_3D('',#250210,#137133,#137134);
#109532=AXIS2_PLACEMENT_3D('',#250211,#137135,#137136);
#109533=AXIS2_PLACEMENT_3D('',#250212,#137137,#137138);
#109534=AXIS2_PLACEMENT_3D('',#250225,#137139,#137140);
#109535=AXIS2_PLACEMENT_3D('',#250226,#137141,#137142);
#109536=AXIS2_PLACEMENT_3D('',#250227,#137143,#137144);
#109537=AXIS2_PLACEMENT_3D('',#250228,#137145,#137146);
#109538=AXIS2_PLACEMENT_3D('',#250229,#137147,#137148);
#109539=AXIS2_PLACEMENT_3D('',#250242,#137149,#137150);
#109540=AXIS2_PLACEMENT_3D('',#250255,#137151,#137152);
#109541=AXIS2_PLACEMENT_3D('',#250256,#137153,#137154);
#109542=AXIS2_PLACEMENT_3D('',#250257,#137155,#137156);
#109543=AXIS2_PLACEMENT_3D('',#250258,#137157,#137158);
#109544=AXIS2_PLACEMENT_3D('',#250259,#137159,#137160);
#109545=AXIS2_PLACEMENT_3D('',#250278,#137161,#137162);
#109546=AXIS2_PLACEMENT_3D('',#250279,#137163,#137164);
#109547=AXIS2_PLACEMENT_3D('',#250292,#137165,#137166);
#109548=AXIS2_PLACEMENT_3D('',#250311,#137167,#137168);
#109549=AXIS2_PLACEMENT_3D('',#250312,#137169,#137170);
#109550=AXIS2_PLACEMENT_3D('',#250313,#137171,#137172);
#109551=AXIS2_PLACEMENT_3D('',#250314,#137173,#137174);
#109552=AXIS2_PLACEMENT_3D('',#250315,#137175,#137176);
#109553=AXIS2_PLACEMENT_3D('',#250346,#137177,#137178);
#109554=AXIS2_PLACEMENT_3D('',#250347,#137179,#137180);
#109555=AXIS2_PLACEMENT_3D('',#250348,#137181,#137182);
#109556=AXIS2_PLACEMENT_3D('',#250367,#137183,#137184);
#109557=AXIS2_PLACEMENT_3D('',#250368,#137185,#137186);
#109558=AXIS2_PLACEMENT_3D('',#250369,#137187,#137188);
#109559=AXIS2_PLACEMENT_3D('',#250370,#137189,#137190);
#109560=AXIS2_PLACEMENT_3D('',#250371,#137191,#137192);
#109561=AXIS2_PLACEMENT_3D('',#250384,#137193,#137194);
#109562=AXIS2_PLACEMENT_3D('',#250397,#137195,#137196);
#109563=AXIS2_PLACEMENT_3D('',#250398,#137197,#137198);
#109564=AXIS2_PLACEMENT_3D('',#250399,#137199,#137200);
#109565=AXIS2_PLACEMENT_3D('',#250400,#137201,#137202);
#109566=AXIS2_PLACEMENT_3D('',#250401,#137203,#137204);
#109567=AXIS2_PLACEMENT_3D('',#250414,#137205,#137206);
#109568=AXIS2_PLACEMENT_3D('',#250415,#137207,#137208);
#109569=AXIS2_PLACEMENT_3D('',#250416,#137209,#137210);
#109570=AXIS2_PLACEMENT_3D('',#250417,#137211,#137212);
#109571=AXIS2_PLACEMENT_3D('',#250418,#137213,#137214);
#109572=AXIS2_PLACEMENT_3D('',#250431,#137215,#137216);
#109573=AXIS2_PLACEMENT_3D('',#250432,#137217,#137218);
#109574=AXIS2_PLACEMENT_3D('',#250433,#137219,#137220);
#109575=AXIS2_PLACEMENT_3D('',#250434,#137221,#137222);
#109576=AXIS2_PLACEMENT_3D('',#250435,#137223,#137224);
#109577=AXIS2_PLACEMENT_3D('',#250448,#137225,#137226);
#109578=AXIS2_PLACEMENT_3D('',#250461,#137227,#137228);
#109579=AXIS2_PLACEMENT_3D('',#250462,#137229,#137230);
#109580=AXIS2_PLACEMENT_3D('',#250463,#137231,#137232);
#109581=AXIS2_PLACEMENT_3D('',#250464,#137233,#137234);
#109582=AXIS2_PLACEMENT_3D('',#250465,#137235,#137236);
#109583=AXIS2_PLACEMENT_3D('',#250484,#137237,#137238);
#109584=AXIS2_PLACEMENT_3D('',#250485,#137239,#137240);
#109585=AXIS2_PLACEMENT_3D('',#250486,#137241,#137242);
#109586=AXIS2_PLACEMENT_3D('',#250487,#137243,#137244);
#109587=AXIS2_PLACEMENT_3D('',#250488,#137245,#137246);
#109588=AXIS2_PLACEMENT_3D('',#250501,#137247,#137248);
#109589=AXIS2_PLACEMENT_3D('',#250520,#137249,#137250);
#109590=AXIS2_PLACEMENT_3D('',#250521,#137251,#137252);
#109591=AXIS2_PLACEMENT_3D('',#250522,#137253,#137254);
#109592=AXIS2_PLACEMENT_3D('',#250523,#137255,#137256);
#109593=AXIS2_PLACEMENT_3D('',#250524,#137257,#137258);
#109594=AXIS2_PLACEMENT_3D('',#250543,#137259,#137260);
#109595=AXIS2_PLACEMENT_3D('',#250556,#137261,#137262);
#109596=AXIS2_PLACEMENT_3D('',#250557,#137263,#137264);
#109597=AXIS2_PLACEMENT_3D('',#250558,#137265,#137266);
#109598=AXIS2_PLACEMENT_3D('',#250559,#137267,#137268);
#109599=AXIS2_PLACEMENT_3D('',#250560,#137269,#137270);
#109600=AXIS2_PLACEMENT_3D('',#250579,#137271,#137272);
#109601=AXIS2_PLACEMENT_3D('',#250580,#137273,#137274);
#109602=AXIS2_PLACEMENT_3D('',#250581,#137275,#137276);
#109603=AXIS2_PLACEMENT_3D('',#250582,#137277,#137278);
#109604=AXIS2_PLACEMENT_3D('',#250583,#137279,#137280);
#109605=AXIS2_PLACEMENT_3D('',#250596,#137281,#137282);
#109606=AXIS2_PLACEMENT_3D('',#250609,#137283,#137284);
#109607=AXIS2_PLACEMENT_3D('',#250610,#137285,#137286);
#109608=AXIS2_PLACEMENT_3D('',#250611,#137287,#137288);
#109609=AXIS2_PLACEMENT_3D('',#250612,#137289,#137290);
#109610=AXIS2_PLACEMENT_3D('',#250613,#137291,#137292);
#109611=AXIS2_PLACEMENT_3D('',#250626,#137293,#137294);
#109612=AXIS2_PLACEMENT_3D('',#250627,#137295,#137296);
#109613=AXIS2_PLACEMENT_3D('',#250628,#137297,#137298);
#109614=AXIS2_PLACEMENT_3D('',#250629,#137299,#137300);
#109615=AXIS2_PLACEMENT_3D('',#250630,#137301,#137302);
#109616=AXIS2_PLACEMENT_3D('',#250643,#137303,#137304);
#109617=AXIS2_PLACEMENT_3D('',#250644,#137305,#137306);
#109618=AXIS2_PLACEMENT_3D('',#250645,#137307,#137308);
#109619=AXIS2_PLACEMENT_3D('',#250646,#137309,#137310);
#109620=AXIS2_PLACEMENT_3D('',#250647,#137311,#137312);
#109621=AXIS2_PLACEMENT_3D('',#250660,#137313,#137314);
#109622=AXIS2_PLACEMENT_3D('',#250673,#137315,#137316);
#109623=AXIS2_PLACEMENT_3D('',#250674,#137317,#137318);
#109624=AXIS2_PLACEMENT_3D('',#250675,#137319,#137320);
#109625=AXIS2_PLACEMENT_3D('',#250676,#137321,#137322);
#109626=AXIS2_PLACEMENT_3D('',#250677,#137323,#137324);
#109627=AXIS2_PLACEMENT_3D('',#250696,#137325,#137326);
#109628=AXIS2_PLACEMENT_3D('',#250697,#137327,#137328);
#109629=AXIS2_PLACEMENT_3D('',#250698,#137329,#137330);
#109630=AXIS2_PLACEMENT_3D('',#250699,#137331,#137332);
#109631=AXIS2_PLACEMENT_3D('',#250700,#137333,#137334);
#109632=AXIS2_PLACEMENT_3D('',#250713,#137335,#137336);
#109633=AXIS2_PLACEMENT_3D('',#250732,#137337,#137338);
#109634=AXIS2_PLACEMENT_3D('',#250733,#137339,#137340);
#109635=AXIS2_PLACEMENT_3D('',#250734,#137341,#137342);
#109636=AXIS2_PLACEMENT_3D('',#250735,#137343,#137344);
#109637=AXIS2_PLACEMENT_3D('',#250736,#137345,#137346);
#109638=AXIS2_PLACEMENT_3D('',#250755,#137347,#137348);
#109639=AXIS2_PLACEMENT_3D('',#250768,#137349,#137350);
#109640=AXIS2_PLACEMENT_3D('',#250769,#137351,#137352);
#109641=AXIS2_PLACEMENT_3D('',#250770,#137353,#137354);
#109642=AXIS2_PLACEMENT_3D('',#250771,#137355,#137356);
#109643=AXIS2_PLACEMENT_3D('',#250772,#137357,#137358);
#109644=AXIS2_PLACEMENT_3D('',#250791,#137359,#137360);
#109645=AXIS2_PLACEMENT_3D('',#250792,#137361,#137362);
#109646=AXIS2_PLACEMENT_3D('',#250793,#137363,#137364);
#109647=AXIS2_PLACEMENT_3D('',#250794,#137365,#137366);
#109648=AXIS2_PLACEMENT_3D('',#250795,#137367,#137368);
#109649=AXIS2_PLACEMENT_3D('',#250808,#137369,#137370);
#109650=AXIS2_PLACEMENT_3D('',#250821,#137371,#137372);
#109651=AXIS2_PLACEMENT_3D('',#250822,#137373,#137374);
#109652=AXIS2_PLACEMENT_3D('',#250823,#137375,#137376);
#109653=AXIS2_PLACEMENT_3D('',#250824,#137377,#137378);
#109654=AXIS2_PLACEMENT_3D('',#250825,#137379,#137380);
#109655=AXIS2_PLACEMENT_3D('',#250838,#137381,#137382);
#109656=AXIS2_PLACEMENT_3D('',#250839,#137383,#137384);
#109657=AXIS2_PLACEMENT_3D('',#250840,#137385,#137386);
#109658=AXIS2_PLACEMENT_3D('',#250841,#137387,#137388);
#109659=AXIS2_PLACEMENT_3D('',#250842,#137389,#137390);
#109660=AXIS2_PLACEMENT_3D('',#250855,#137391,#137392);
#109661=AXIS2_PLACEMENT_3D('',#250856,#137393,#137394);
#109662=AXIS2_PLACEMENT_3D('',#250857,#137395,#137396);
#109663=AXIS2_PLACEMENT_3D('',#250858,#137397,#137398);
#109664=AXIS2_PLACEMENT_3D('',#250859,#137399,#137400);
#109665=AXIS2_PLACEMENT_3D('',#250872,#137401,#137402);
#109666=AXIS2_PLACEMENT_3D('',#250885,#137403,#137404);
#109667=AXIS2_PLACEMENT_3D('',#250886,#137405,#137406);
#109668=AXIS2_PLACEMENT_3D('',#250887,#137407,#137408);
#109669=AXIS2_PLACEMENT_3D('',#250888,#137409,#137410);
#109670=AXIS2_PLACEMENT_3D('',#250889,#137411,#137412);
#109671=AXIS2_PLACEMENT_3D('',#250908,#137413,#137414);
#109672=AXIS2_PLACEMENT_3D('',#250909,#137415,#137416);
#109673=AXIS2_PLACEMENT_3D('',#250910,#137417,#137418);
#109674=AXIS2_PLACEMENT_3D('',#250911,#137419,#137420);
#109675=AXIS2_PLACEMENT_3D('',#250912,#137421,#137422);
#109676=AXIS2_PLACEMENT_3D('',#250925,#137423,#137424);
#109677=AXIS2_PLACEMENT_3D('',#250944,#137425,#137426);
#109678=AXIS2_PLACEMENT_3D('',#250945,#137427,#137428);
#109679=AXIS2_PLACEMENT_3D('',#250946,#137429,#137430);
#109680=AXIS2_PLACEMENT_3D('',#250947,#137431,#137432);
#109681=AXIS2_PLACEMENT_3D('',#250948,#137433,#137434);
#109682=AXIS2_PLACEMENT_3D('',#250967,#137435,#137436);
#109683=AXIS2_PLACEMENT_3D('',#250980,#137437,#137438);
#109684=AXIS2_PLACEMENT_3D('',#250981,#137439,#137440);
#109685=AXIS2_PLACEMENT_3D('',#250982,#137441,#137442);
#109686=AXIS2_PLACEMENT_3D('',#250983,#137443,#137444);
#109687=AXIS2_PLACEMENT_3D('',#250984,#137445,#137446);
#109688=AXIS2_PLACEMENT_3D('',#251003,#137447,#137448);
#109689=AXIS2_PLACEMENT_3D('',#251004,#137449,#137450);
#109690=AXIS2_PLACEMENT_3D('',#251005,#137451,#137452);
#109691=AXIS2_PLACEMENT_3D('',#251006,#137453,#137454);
#109692=AXIS2_PLACEMENT_3D('',#251007,#137455,#137456);
#109693=AXIS2_PLACEMENT_3D('',#251020,#137457,#137458);
#109694=AXIS2_PLACEMENT_3D('',#251033,#137459,#137460);
#109695=AXIS2_PLACEMENT_3D('',#251034,#137461,#137462);
#109696=AXIS2_PLACEMENT_3D('',#251035,#137463,#137464);
#109697=AXIS2_PLACEMENT_3D('',#251036,#137465,#137466);
#109698=AXIS2_PLACEMENT_3D('',#251037,#137467,#137468);
#109699=AXIS2_PLACEMENT_3D('',#251050,#137469,#137470);
#109700=AXIS2_PLACEMENT_3D('',#251051,#137471,#137472);
#109701=AXIS2_PLACEMENT_3D('',#251052,#137473,#137474);
#109702=AXIS2_PLACEMENT_3D('',#251053,#137475,#137476);
#109703=AXIS2_PLACEMENT_3D('',#251054,#137477,#137478);
#109704=AXIS2_PLACEMENT_3D('',#251067,#137479,#137480);
#109705=AXIS2_PLACEMENT_3D('',#251068,#137481,#137482);
#109706=AXIS2_PLACEMENT_3D('',#251069,#137483,#137484);
#109707=AXIS2_PLACEMENT_3D('',#251070,#137485,#137486);
#109708=AXIS2_PLACEMENT_3D('',#251071,#137487,#137488);
#109709=AXIS2_PLACEMENT_3D('',#251084,#137489,#137490);
#109710=AXIS2_PLACEMENT_3D('',#251097,#137491,#137492);
#109711=AXIS2_PLACEMENT_3D('',#251098,#137493,#137494);
#109712=AXIS2_PLACEMENT_3D('',#251099,#137495,#137496);
#109713=AXIS2_PLACEMENT_3D('',#251100,#137497,#137498);
#109714=AXIS2_PLACEMENT_3D('',#251101,#137499,#137500);
#109715=AXIS2_PLACEMENT_3D('',#251120,#137501,#137502);
#109716=AXIS2_PLACEMENT_3D('',#251121,#137503,#137504);
#109717=AXIS2_PLACEMENT_3D('',#251122,#137505,#137506);
#109718=AXIS2_PLACEMENT_3D('',#251123,#137507,#137508);
#109719=AXIS2_PLACEMENT_3D('',#251124,#137509,#137510);
#109720=AXIS2_PLACEMENT_3D('',#251137,#137511,#137512);
#109721=AXIS2_PLACEMENT_3D('',#251156,#137513,#137514);
#109722=AXIS2_PLACEMENT_3D('',#251157,#137515,#137516);
#109723=AXIS2_PLACEMENT_3D('',#251158,#137517,#137518);
#109724=AXIS2_PLACEMENT_3D('',#251159,#137519,#137520);
#109725=AXIS2_PLACEMENT_3D('',#251160,#137521,#137522);
#109726=AXIS2_PLACEMENT_3D('',#251179,#137523,#137524);
#109727=AXIS2_PLACEMENT_3D('',#251192,#137525,#137526);
#109728=AXIS2_PLACEMENT_3D('',#251193,#137527,#137528);
#109729=AXIS2_PLACEMENT_3D('',#251194,#137529,#137530);
#109730=AXIS2_PLACEMENT_3D('',#251195,#137531,#137532);
#109731=AXIS2_PLACEMENT_3D('',#251196,#137533,#137534);
#109732=AXIS2_PLACEMENT_3D('',#251215,#137535,#137536);
#109733=AXIS2_PLACEMENT_3D('',#251216,#137537,#137538);
#109734=AXIS2_PLACEMENT_3D('',#251217,#137539,#137540);
#109735=AXIS2_PLACEMENT_3D('',#251218,#137541,#137542);
#109736=AXIS2_PLACEMENT_3D('',#251219,#137543,#137544);
#109737=AXIS2_PLACEMENT_3D('',#251232,#137545,#137546);
#109738=AXIS2_PLACEMENT_3D('',#251245,#137547,#137548);
#109739=AXIS2_PLACEMENT_3D('',#251246,#137549,#137550);
#109740=AXIS2_PLACEMENT_3D('',#251247,#137551,#137552);
#109741=AXIS2_PLACEMENT_3D('',#251248,#137553,#137554);
#109742=AXIS2_PLACEMENT_3D('',#251249,#137555,#137556);
#109743=AXIS2_PLACEMENT_3D('',#251262,#137557,#137558);
#109744=AXIS2_PLACEMENT_3D('',#251263,#137559,#137560);
#109745=AXIS2_PLACEMENT_3D('',#251264,#137561,#137562);
#109746=AXIS2_PLACEMENT_3D('',#251265,#137563,#137564);
#109747=AXIS2_PLACEMENT_3D('',#251266,#137565,#137566);
#109748=AXIS2_PLACEMENT_3D('',#251279,#137567,#137568);
#109749=AXIS2_PLACEMENT_3D('',#251280,#137569,#137570);
#109750=AXIS2_PLACEMENT_3D('',#251281,#137571,#137572);
#109751=AXIS2_PLACEMENT_3D('',#251282,#137573,#137574);
#109752=AXIS2_PLACEMENT_3D('',#251283,#137575,#137576);
#109753=AXIS2_PLACEMENT_3D('',#251296,#137577,#137578);
#109754=AXIS2_PLACEMENT_3D('',#251309,#137579,#137580);
#109755=AXIS2_PLACEMENT_3D('',#251310,#137581,#137582);
#109756=AXIS2_PLACEMENT_3D('',#251311,#137583,#137584);
#109757=AXIS2_PLACEMENT_3D('',#251312,#137585,#137586);
#109758=AXIS2_PLACEMENT_3D('',#251313,#137587,#137588);
#109759=AXIS2_PLACEMENT_3D('',#251332,#137589,#137590);
#109760=AXIS2_PLACEMENT_3D('',#251333,#137591,#137592);
#109761=AXIS2_PLACEMENT_3D('',#251334,#137593,#137594);
#109762=AXIS2_PLACEMENT_3D('',#251335,#137595,#137596);
#109763=AXIS2_PLACEMENT_3D('',#251336,#137597,#137598);
#109764=AXIS2_PLACEMENT_3D('',#251349,#137599,#137600);
#109765=AXIS2_PLACEMENT_3D('',#251368,#137601,#137602);
#109766=AXIS2_PLACEMENT_3D('',#251369,#137603,#137604);
#109767=AXIS2_PLACEMENT_3D('',#251370,#137605,#137606);
#109768=AXIS2_PLACEMENT_3D('',#251371,#137607,#137608);
#109769=AXIS2_PLACEMENT_3D('',#251372,#137609,#137610);
#109770=AXIS2_PLACEMENT_3D('',#251391,#137611,#137612);
#109771=AXIS2_PLACEMENT_3D('',#251404,#137613,#137614);
#109772=AXIS2_PLACEMENT_3D('',#251405,#137615,#137616);
#109773=AXIS2_PLACEMENT_3D('',#251406,#137617,#137618);
#109774=AXIS2_PLACEMENT_3D('',#251407,#137619,#137620);
#109775=AXIS2_PLACEMENT_3D('',#251408,#137621,#137622);
#109776=AXIS2_PLACEMENT_3D('',#251427,#137623,#137624);
#109777=AXIS2_PLACEMENT_3D('',#251428,#137625,#137626);
#109778=AXIS2_PLACEMENT_3D('',#251429,#137627,#137628);
#109779=AXIS2_PLACEMENT_3D('',#251430,#137629,#137630);
#109780=AXIS2_PLACEMENT_3D('',#251431,#137631,#137632);
#109781=AXIS2_PLACEMENT_3D('',#251444,#137633,#137634);
#109782=AXIS2_PLACEMENT_3D('',#251457,#137635,#137636);
#109783=AXIS2_PLACEMENT_3D('',#251458,#137637,#137638);
#109784=AXIS2_PLACEMENT_3D('',#251459,#137639,#137640);
#109785=AXIS2_PLACEMENT_3D('',#251460,#137641,#137642);
#109786=AXIS2_PLACEMENT_3D('',#251461,#137643,#137644);
#109787=AXIS2_PLACEMENT_3D('',#251474,#137645,#137646);
#109788=AXIS2_PLACEMENT_3D('',#251475,#137647,#137648);
#109789=AXIS2_PLACEMENT_3D('',#251476,#137649,#137650);
#109790=AXIS2_PLACEMENT_3D('',#251477,#137651,#137652);
#109791=AXIS2_PLACEMENT_3D('',#251478,#137653,#137654);
#109792=AXIS2_PLACEMENT_3D('',#251491,#137655,#137656);
#109793=AXIS2_PLACEMENT_3D('',#251492,#137657,#137658);
#109794=AXIS2_PLACEMENT_3D('',#251493,#137659,#137660);
#109795=AXIS2_PLACEMENT_3D('',#251494,#137661,#137662);
#109796=AXIS2_PLACEMENT_3D('',#251495,#137663,#137664);
#109797=AXIS2_PLACEMENT_3D('',#251508,#137665,#137666);
#109798=AXIS2_PLACEMENT_3D('',#251521,#137667,#137668);
#109799=AXIS2_PLACEMENT_3D('',#251522,#137669,#137670);
#109800=AXIS2_PLACEMENT_3D('',#251523,#137671,#137672);
#109801=AXIS2_PLACEMENT_3D('',#251524,#137673,#137674);
#109802=AXIS2_PLACEMENT_3D('',#251525,#137675,#137676);
#109803=AXIS2_PLACEMENT_3D('',#251544,#137677,#137678);
#109804=AXIS2_PLACEMENT_3D('',#251545,#137679,#137680);
#109805=AXIS2_PLACEMENT_3D('',#251546,#137681,#137682);
#109806=AXIS2_PLACEMENT_3D('',#251547,#137683,#137684);
#109807=AXIS2_PLACEMENT_3D('',#251548,#137685,#137686);
#109808=AXIS2_PLACEMENT_3D('',#251561,#137687,#137688);
#109809=AXIS2_PLACEMENT_3D('',#251580,#137689,#137690);
#109810=AXIS2_PLACEMENT_3D('',#251581,#137691,#137692);
#109811=AXIS2_PLACEMENT_3D('',#251582,#137693,#137694);
#109812=AXIS2_PLACEMENT_3D('',#251583,#137695,#137696);
#109813=AXIS2_PLACEMENT_3D('',#251584,#137697,#137698);
#109814=AXIS2_PLACEMENT_3D('',#251603,#137699,#137700);
#109815=AXIS2_PLACEMENT_3D('',#251616,#137701,#137702);
#109816=AXIS2_PLACEMENT_3D('',#251617,#137703,#137704);
#109817=AXIS2_PLACEMENT_3D('',#251618,#137705,#137706);
#109818=AXIS2_PLACEMENT_3D('',#251619,#137707,#137708);
#109819=AXIS2_PLACEMENT_3D('',#251620,#137709,#137710);
#109820=AXIS2_PLACEMENT_3D('',#251639,#137711,#137712);
#109821=AXIS2_PLACEMENT_3D('',#251640,#137713,#137714);
#109822=AXIS2_PLACEMENT_3D('',#251641,#137715,#137716);
#109823=AXIS2_PLACEMENT_3D('',#251642,#137717,#137718);
#109824=AXIS2_PLACEMENT_3D('',#251643,#137719,#137720);
#109825=AXIS2_PLACEMENT_3D('',#251656,#137721,#137722);
#109826=AXIS2_PLACEMENT_3D('',#251669,#137723,#137724);
#109827=AXIS2_PLACEMENT_3D('',#251670,#137725,#137726);
#109828=AXIS2_PLACEMENT_3D('',#251671,#137727,#137728);
#109829=AXIS2_PLACEMENT_3D('',#251672,#137729,#137730);
#109830=AXIS2_PLACEMENT_3D('',#251673,#137731,#137732);
#109831=AXIS2_PLACEMENT_3D('',#251686,#137733,#137734);
#109832=AXIS2_PLACEMENT_3D('',#251687,#137735,#137736);
#109833=AXIS2_PLACEMENT_3D('',#251688,#137737,#137738);
#109834=AXIS2_PLACEMENT_3D('',#251689,#137739,#137740);
#109835=AXIS2_PLACEMENT_3D('',#251690,#137741,#137742);
#109836=AXIS2_PLACEMENT_3D('',#251703,#137743,#137744);
#109837=AXIS2_PLACEMENT_3D('',#251704,#137745,#137746);
#109838=AXIS2_PLACEMENT_3D('',#251705,#137747,#137748);
#109839=AXIS2_PLACEMENT_3D('',#251706,#137749,#137750);
#109840=AXIS2_PLACEMENT_3D('',#251707,#137751,#137752);
#109841=AXIS2_PLACEMENT_3D('',#251720,#137753,#137754);
#109842=AXIS2_PLACEMENT_3D('',#251733,#137755,#137756);
#109843=AXIS2_PLACEMENT_3D('',#251734,#137757,#137758);
#109844=AXIS2_PLACEMENT_3D('',#251735,#137759,#137760);
#109845=AXIS2_PLACEMENT_3D('',#251736,#137761,#137762);
#109846=AXIS2_PLACEMENT_3D('',#251737,#137763,#137764);
#109847=AXIS2_PLACEMENT_3D('',#251756,#137765,#137766);
#109848=AXIS2_PLACEMENT_3D('',#251757,#137767,#137768);
#109849=AXIS2_PLACEMENT_3D('',#251758,#137769,#137770);
#109850=AXIS2_PLACEMENT_3D('',#251759,#137771,#137772);
#109851=AXIS2_PLACEMENT_3D('',#251760,#137773,#137774);
#109852=AXIS2_PLACEMENT_3D('',#251773,#137775,#137776);
#109853=AXIS2_PLACEMENT_3D('',#251792,#137777,#137778);
#109854=AXIS2_PLACEMENT_3D('',#251793,#137779,#137780);
#109855=AXIS2_PLACEMENT_3D('',#251794,#137781,#137782);
#109856=AXIS2_PLACEMENT_3D('',#251795,#137783,#137784);
#109857=AXIS2_PLACEMENT_3D('',#251796,#137785,#137786);
#109858=AXIS2_PLACEMENT_3D('',#251815,#137787,#137788);
#109859=AXIS2_PLACEMENT_3D('',#251828,#137789,#137790);
#109860=AXIS2_PLACEMENT_3D('',#251829,#137791,#137792);
#109861=AXIS2_PLACEMENT_3D('',#251830,#137793,#137794);
#109862=AXIS2_PLACEMENT_3D('',#251831,#137795,#137796);
#109863=AXIS2_PLACEMENT_3D('',#251832,#137797,#137798);
#109864=AXIS2_PLACEMENT_3D('',#251851,#137799,#137800);
#109865=AXIS2_PLACEMENT_3D('',#251852,#137801,#137802);
#109866=AXIS2_PLACEMENT_3D('',#251853,#137803,#137804);
#109867=AXIS2_PLACEMENT_3D('',#251854,#137805,#137806);
#109868=AXIS2_PLACEMENT_3D('',#251855,#137807,#137808);
#109869=AXIS2_PLACEMENT_3D('',#251868,#137809,#137810);
#109870=AXIS2_PLACEMENT_3D('',#251881,#137811,#137812);
#109871=AXIS2_PLACEMENT_3D('',#251882,#137813,#137814);
#109872=AXIS2_PLACEMENT_3D('',#251883,#137815,#137816);
#109873=AXIS2_PLACEMENT_3D('',#251884,#137817,#137818);
#109874=AXIS2_PLACEMENT_3D('',#251885,#137819,#137820);
#109875=AXIS2_PLACEMENT_3D('',#251898,#137821,#137822);
#109876=AXIS2_PLACEMENT_3D('',#251899,#137823,#137824);
#109877=AXIS2_PLACEMENT_3D('',#251900,#137825,#137826);
#109878=AXIS2_PLACEMENT_3D('',#251901,#137827,#137828);
#109879=AXIS2_PLACEMENT_3D('',#251902,#137829,#137830);
#109880=AXIS2_PLACEMENT_3D('',#251915,#137831,#137832);
#109881=AXIS2_PLACEMENT_3D('',#251916,#137833,#137834);
#109882=AXIS2_PLACEMENT_3D('',#251917,#137835,#137836);
#109883=AXIS2_PLACEMENT_3D('',#251918,#137837,#137838);
#109884=AXIS2_PLACEMENT_3D('',#251919,#137839,#137840);
#109885=AXIS2_PLACEMENT_3D('',#251932,#137841,#137842);
#109886=AXIS2_PLACEMENT_3D('',#251945,#137843,#137844);
#109887=AXIS2_PLACEMENT_3D('',#251946,#137845,#137846);
#109888=AXIS2_PLACEMENT_3D('',#251947,#137847,#137848);
#109889=AXIS2_PLACEMENT_3D('',#251948,#137849,#137850);
#109890=AXIS2_PLACEMENT_3D('',#251949,#137851,#137852);
#109891=AXIS2_PLACEMENT_3D('',#251968,#137853,#137854);
#109892=AXIS2_PLACEMENT_3D('',#251969,#137855,#137856);
#109893=AXIS2_PLACEMENT_3D('',#251970,#137857,#137858);
#109894=AXIS2_PLACEMENT_3D('',#251971,#137859,#137860);
#109895=AXIS2_PLACEMENT_3D('',#251972,#137861,#137862);
#109896=AXIS2_PLACEMENT_3D('',#251985,#137863,#137864);
#109897=AXIS2_PLACEMENT_3D('',#252004,#137865,#137866);
#109898=AXIS2_PLACEMENT_3D('',#252005,#137867,#137868);
#109899=AXIS2_PLACEMENT_3D('',#252006,#137869,#137870);
#109900=AXIS2_PLACEMENT_3D('',#252007,#137871,#137872);
#109901=AXIS2_PLACEMENT_3D('',#252008,#137873,#137874);
#109902=AXIS2_PLACEMENT_3D('',#252027,#137875,#137876);
#109903=AXIS2_PLACEMENT_3D('',#252040,#137877,#137878);
#109904=AXIS2_PLACEMENT_3D('',#252041,#137879,#137880);
#109905=AXIS2_PLACEMENT_3D('',#252042,#137881,#137882);
#109906=AXIS2_PLACEMENT_3D('',#252043,#137883,#137884);
#109907=AXIS2_PLACEMENT_3D('',#252044,#137885,#137886);
#109908=AXIS2_PLACEMENT_3D('',#252063,#137887,#137888);
#109909=AXIS2_PLACEMENT_3D('',#252064,#137889,#137890);
#109910=AXIS2_PLACEMENT_3D('',#252065,#137891,#137892);
#109911=AXIS2_PLACEMENT_3D('',#252066,#137893,#137894);
#109912=AXIS2_PLACEMENT_3D('',#252067,#137895,#137896);
#109913=AXIS2_PLACEMENT_3D('',#252080,#137897,#137898);
#109914=AXIS2_PLACEMENT_3D('',#252093,#137899,#137900);
#109915=AXIS2_PLACEMENT_3D('',#252094,#137901,#137902);
#109916=AXIS2_PLACEMENT_3D('',#252095,#137903,#137904);
#109917=AXIS2_PLACEMENT_3D('',#252096,#137905,#137906);
#109918=AXIS2_PLACEMENT_3D('',#252097,#137907,#137908);
#109919=AXIS2_PLACEMENT_3D('',#252110,#137909,#137910);
#109920=AXIS2_PLACEMENT_3D('',#252111,#137911,#137912);
#109921=AXIS2_PLACEMENT_3D('',#252112,#137913,#137914);
#109922=AXIS2_PLACEMENT_3D('',#252113,#137915,#137916);
#109923=AXIS2_PLACEMENT_3D('',#252114,#137917,#137918);
#109924=AXIS2_PLACEMENT_3D('',#252127,#137919,#137920);
#109925=AXIS2_PLACEMENT_3D('',#252128,#137921,#137922);
#109926=AXIS2_PLACEMENT_3D('',#252129,#137923,#137924);
#109927=AXIS2_PLACEMENT_3D('',#252130,#137925,#137926);
#109928=AXIS2_PLACEMENT_3D('',#252131,#137927,#137928);
#109929=AXIS2_PLACEMENT_3D('',#252144,#137929,#137930);
#109930=AXIS2_PLACEMENT_3D('',#252157,#137931,#137932);
#109931=AXIS2_PLACEMENT_3D('',#252158,#137933,#137934);
#109932=AXIS2_PLACEMENT_3D('',#252159,#137935,#137936);
#109933=AXIS2_PLACEMENT_3D('',#252160,#137937,#137938);
#109934=AXIS2_PLACEMENT_3D('',#252161,#137939,#137940);
#109935=AXIS2_PLACEMENT_3D('',#252180,#137941,#137942);
#109936=AXIS2_PLACEMENT_3D('',#252181,#137943,#137944);
#109937=AXIS2_PLACEMENT_3D('',#252182,#137945,#137946);
#109938=AXIS2_PLACEMENT_3D('',#252183,#137947,#137948);
#109939=AXIS2_PLACEMENT_3D('',#252184,#137949,#137950);
#109940=AXIS2_PLACEMENT_3D('',#252197,#137951,#137952);
#109941=AXIS2_PLACEMENT_3D('',#252216,#137953,#137954);
#109942=AXIS2_PLACEMENT_3D('',#252217,#137955,#137956);
#109943=AXIS2_PLACEMENT_3D('',#252218,#137957,#137958);
#109944=AXIS2_PLACEMENT_3D('',#252219,#137959,#137960);
#109945=AXIS2_PLACEMENT_3D('',#252220,#137961,#137962);
#109946=AXIS2_PLACEMENT_3D('',#252239,#137963,#137964);
#109947=AXIS2_PLACEMENT_3D('',#252252,#137965,#137966);
#109948=AXIS2_PLACEMENT_3D('',#252253,#137967,#137968);
#109949=AXIS2_PLACEMENT_3D('',#252254,#137969,#137970);
#109950=AXIS2_PLACEMENT_3D('',#252255,#137971,#137972);
#109951=AXIS2_PLACEMENT_3D('',#252256,#137973,#137974);
#109952=AXIS2_PLACEMENT_3D('',#252275,#137975,#137976);
#109953=AXIS2_PLACEMENT_3D('',#252276,#137977,#137978);
#109954=AXIS2_PLACEMENT_3D('',#252277,#137979,#137980);
#109955=AXIS2_PLACEMENT_3D('',#252278,#137981,#137982);
#109956=AXIS2_PLACEMENT_3D('',#252279,#137983,#137984);
#109957=AXIS2_PLACEMENT_3D('',#252292,#137985,#137986);
#109958=AXIS2_PLACEMENT_3D('',#252305,#137987,#137988);
#109959=AXIS2_PLACEMENT_3D('',#252306,#137989,#137990);
#109960=AXIS2_PLACEMENT_3D('',#252307,#137991,#137992);
#109961=AXIS2_PLACEMENT_3D('',#252308,#137993,#137994);
#109962=AXIS2_PLACEMENT_3D('',#252309,#137995,#137996);
#109963=AXIS2_PLACEMENT_3D('',#252322,#137997,#137998);
#109964=AXIS2_PLACEMENT_3D('',#252323,#137999,#138000);
#109965=AXIS2_PLACEMENT_3D('',#252324,#138001,#138002);
#109966=AXIS2_PLACEMENT_3D('',#252325,#138003,#138004);
#109967=AXIS2_PLACEMENT_3D('',#252326,#138005,#138006);
#109968=AXIS2_PLACEMENT_3D('',#252339,#138007,#138008);
#109969=AXIS2_PLACEMENT_3D('',#252340,#138009,#138010);
#109970=AXIS2_PLACEMENT_3D('',#252341,#138011,#138012);
#109971=AXIS2_PLACEMENT_3D('',#252342,#138013,#138014);
#109972=AXIS2_PLACEMENT_3D('',#252343,#138015,#138016);
#109973=AXIS2_PLACEMENT_3D('',#252356,#138017,#138018);
#109974=AXIS2_PLACEMENT_3D('',#252369,#138019,#138020);
#109975=AXIS2_PLACEMENT_3D('',#252370,#138021,#138022);
#109976=AXIS2_PLACEMENT_3D('',#252371,#138023,#138024);
#109977=AXIS2_PLACEMENT_3D('',#252372,#138025,#138026);
#109978=AXIS2_PLACEMENT_3D('',#252373,#138027,#138028);
#109979=AXIS2_PLACEMENT_3D('',#252392,#138029,#138030);
#109980=AXIS2_PLACEMENT_3D('',#252393,#138031,#138032);
#109981=AXIS2_PLACEMENT_3D('',#252394,#138033,#138034);
#109982=AXIS2_PLACEMENT_3D('',#252395,#138035,#138036);
#109983=AXIS2_PLACEMENT_3D('',#252396,#138037,#138038);
#109984=AXIS2_PLACEMENT_3D('',#252409,#138039,#138040);
#109985=AXIS2_PLACEMENT_3D('',#252428,#138041,#138042);
#109986=AXIS2_PLACEMENT_3D('',#252429,#138043,#138044);
#109987=AXIS2_PLACEMENT_3D('',#252430,#138045,#138046);
#109988=AXIS2_PLACEMENT_3D('',#252431,#138047,#138048);
#109989=AXIS2_PLACEMENT_3D('',#252432,#138049,#138050);
#109990=AXIS2_PLACEMENT_3D('',#252451,#138051,#138052);
#109991=AXIS2_PLACEMENT_3D('',#252464,#138053,#138054);
#109992=AXIS2_PLACEMENT_3D('',#252465,#138055,#138056);
#109993=AXIS2_PLACEMENT_3D('',#252466,#138057,#138058);
#109994=AXIS2_PLACEMENT_3D('',#252467,#138059,#138060);
#109995=AXIS2_PLACEMENT_3D('',#252468,#138061,#138062);
#109996=AXIS2_PLACEMENT_3D('',#252487,#138063,#138064);
#109997=AXIS2_PLACEMENT_3D('',#252488,#138065,#138066);
#109998=AXIS2_PLACEMENT_3D('',#252489,#138067,#138068);
#109999=AXIS2_PLACEMENT_3D('',#252490,#138069,#138070);
#110000=AXIS2_PLACEMENT_3D('',#252491,#138071,#138072);
#110001=AXIS2_PLACEMENT_3D('',#252504,#138073,#138074);
#110002=AXIS2_PLACEMENT_3D('',#252517,#138075,#138076);
#110003=AXIS2_PLACEMENT_3D('',#252518,#138077,#138078);
#110004=AXIS2_PLACEMENT_3D('',#252519,#138079,#138080);
#110005=AXIS2_PLACEMENT_3D('',#252520,#138081,#138082);
#110006=AXIS2_PLACEMENT_3D('',#252521,#138083,#138084);
#110007=AXIS2_PLACEMENT_3D('',#252534,#138085,#138086);
#110008=AXIS2_PLACEMENT_3D('',#252535,#138087,#138088);
#110009=AXIS2_PLACEMENT_3D('',#252536,#138089,#138090);
#110010=AXIS2_PLACEMENT_3D('',#252537,#138091,#138092);
#110011=AXIS2_PLACEMENT_3D('',#252538,#138093,#138094);
#110012=AXIS2_PLACEMENT_3D('',#252551,#138095,#138096);
#110013=AXIS2_PLACEMENT_3D('',#252552,#138097,#138098);
#110014=AXIS2_PLACEMENT_3D('',#252553,#138099,#138100);
#110015=AXIS2_PLACEMENT_3D('',#252554,#138101,#138102);
#110016=AXIS2_PLACEMENT_3D('',#252555,#138103,#138104);
#110017=AXIS2_PLACEMENT_3D('',#252568,#138105,#138106);
#110018=AXIS2_PLACEMENT_3D('',#252581,#138107,#138108);
#110019=AXIS2_PLACEMENT_3D('',#252582,#138109,#138110);
#110020=AXIS2_PLACEMENT_3D('',#252583,#138111,#138112);
#110021=AXIS2_PLACEMENT_3D('',#252584,#138113,#138114);
#110022=AXIS2_PLACEMENT_3D('',#252585,#138115,#138116);
#110023=AXIS2_PLACEMENT_3D('',#252604,#138117,#138118);
#110024=AXIS2_PLACEMENT_3D('',#252605,#138119,#138120);
#110025=AXIS2_PLACEMENT_3D('',#252606,#138121,#138122);
#110026=AXIS2_PLACEMENT_3D('',#252607,#138123,#138124);
#110027=AXIS2_PLACEMENT_3D('',#252608,#138125,#138126);
#110028=AXIS2_PLACEMENT_3D('',#252621,#138127,#138128);
#110029=AXIS2_PLACEMENT_3D('',#252640,#138129,#138130);
#110030=AXIS2_PLACEMENT_3D('',#252641,#138131,#138132);
#110031=AXIS2_PLACEMENT_3D('',#252642,#138133,#138134);
#110032=AXIS2_PLACEMENT_3D('',#252643,#138135,#138136);
#110033=AXIS2_PLACEMENT_3D('',#252644,#138137,#138138);
#110034=AXIS2_PLACEMENT_3D('',#252663,#138139,#138140);
#110035=AXIS2_PLACEMENT_3D('',#252676,#138141,#138142);
#110036=AXIS2_PLACEMENT_3D('',#252677,#138143,#138144);
#110037=AXIS2_PLACEMENT_3D('',#252678,#138145,#138146);
#110038=AXIS2_PLACEMENT_3D('',#252679,#138147,#138148);
#110039=AXIS2_PLACEMENT_3D('',#252680,#138149,#138150);
#110040=AXIS2_PLACEMENT_3D('',#252699,#138151,#138152);
#110041=AXIS2_PLACEMENT_3D('',#252700,#138153,#138154);
#110042=AXIS2_PLACEMENT_3D('',#252701,#138155,#138156);
#110043=AXIS2_PLACEMENT_3D('',#252702,#138157,#138158);
#110044=AXIS2_PLACEMENT_3D('',#252703,#138159,#138160);
#110045=AXIS2_PLACEMENT_3D('',#252716,#138161,#138162);
#110046=AXIS2_PLACEMENT_3D('',#252729,#138163,#138164);
#110047=AXIS2_PLACEMENT_3D('',#252730,#138165,#138166);
#110048=AXIS2_PLACEMENT_3D('',#252731,#138167,#138168);
#110049=AXIS2_PLACEMENT_3D('',#252732,#138169,#138170);
#110050=AXIS2_PLACEMENT_3D('',#252733,#138171,#138172);
#110051=AXIS2_PLACEMENT_3D('',#252746,#138173,#138174);
#110052=AXIS2_PLACEMENT_3D('',#252747,#138175,#138176);
#110053=AXIS2_PLACEMENT_3D('',#252748,#138177,#138178);
#110054=AXIS2_PLACEMENT_3D('',#252749,#138179,#138180);
#110055=AXIS2_PLACEMENT_3D('',#252750,#138181,#138182);
#110056=AXIS2_PLACEMENT_3D('',#252763,#138183,#138184);
#110057=AXIS2_PLACEMENT_3D('',#252764,#138185,#138186);
#110058=AXIS2_PLACEMENT_3D('',#252765,#138187,#138188);
#110059=AXIS2_PLACEMENT_3D('',#252766,#138189,#138190);
#110060=AXIS2_PLACEMENT_3D('',#252767,#138191,#138192);
#110061=AXIS2_PLACEMENT_3D('',#252780,#138193,#138194);
#110062=AXIS2_PLACEMENT_3D('',#252793,#138195,#138196);
#110063=AXIS2_PLACEMENT_3D('',#252794,#138197,#138198);
#110064=AXIS2_PLACEMENT_3D('',#252795,#138199,#138200);
#110065=AXIS2_PLACEMENT_3D('',#252796,#138201,#138202);
#110066=AXIS2_PLACEMENT_3D('',#252797,#138203,#138204);
#110067=AXIS2_PLACEMENT_3D('',#252816,#138205,#138206);
#110068=AXIS2_PLACEMENT_3D('',#252817,#138207,#138208);
#110069=AXIS2_PLACEMENT_3D('',#252818,#138209,#138210);
#110070=AXIS2_PLACEMENT_3D('',#252819,#138211,#138212);
#110071=AXIS2_PLACEMENT_3D('',#252820,#138213,#138214);
#110072=AXIS2_PLACEMENT_3D('',#252833,#138215,#138216);
#110073=AXIS2_PLACEMENT_3D('',#252852,#138217,#138218);
#110074=AXIS2_PLACEMENT_3D('',#252853,#138219,#138220);
#110075=AXIS2_PLACEMENT_3D('',#252854,#138221,#138222);
#110076=AXIS2_PLACEMENT_3D('',#252855,#138223,#138224);
#110077=AXIS2_PLACEMENT_3D('',#252856,#138225,#138226);
#110078=AXIS2_PLACEMENT_3D('',#252875,#138227,#138228);
#110079=AXIS2_PLACEMENT_3D('',#252888,#138229,#138230);
#110080=AXIS2_PLACEMENT_3D('',#252889,#138231,#138232);
#110081=AXIS2_PLACEMENT_3D('',#252890,#138233,#138234);
#110082=AXIS2_PLACEMENT_3D('',#252891,#138235,#138236);
#110083=AXIS2_PLACEMENT_3D('',#252892,#138237,#138238);
#110084=AXIS2_PLACEMENT_3D('',#252911,#138239,#138240);
#110085=AXIS2_PLACEMENT_3D('',#252912,#138241,#138242);
#110086=AXIS2_PLACEMENT_3D('',#252913,#138243,#138244);
#110087=AXIS2_PLACEMENT_3D('',#252914,#138245,#138246);
#110088=AXIS2_PLACEMENT_3D('',#252915,#138247,#138248);
#110089=AXIS2_PLACEMENT_3D('',#252928,#138249,#138250);
#110090=AXIS2_PLACEMENT_3D('',#252941,#138251,#138252);
#110091=AXIS2_PLACEMENT_3D('',#252942,#138253,#138254);
#110092=AXIS2_PLACEMENT_3D('',#252943,#138255,#138256);
#110093=AXIS2_PLACEMENT_3D('',#252944,#138257,#138258);
#110094=AXIS2_PLACEMENT_3D('',#252945,#138259,#138260);
#110095=AXIS2_PLACEMENT_3D('',#252958,#138261,#138262);
#110096=AXIS2_PLACEMENT_3D('',#252959,#138263,#138264);
#110097=AXIS2_PLACEMENT_3D('',#252960,#138265,#138266);
#110098=AXIS2_PLACEMENT_3D('',#252961,#138267,#138268);
#110099=AXIS2_PLACEMENT_3D('',#252962,#138269,#138270);
#110100=AXIS2_PLACEMENT_3D('',#252975,#138271,#138272);
#110101=AXIS2_PLACEMENT_3D('',#252976,#138273,#138274);
#110102=AXIS2_PLACEMENT_3D('',#252977,#138275,#138276);
#110103=AXIS2_PLACEMENT_3D('',#252978,#138277,#138278);
#110104=AXIS2_PLACEMENT_3D('',#252979,#138279,#138280);
#110105=AXIS2_PLACEMENT_3D('',#252992,#138281,#138282);
#110106=AXIS2_PLACEMENT_3D('',#253005,#138283,#138284);
#110107=AXIS2_PLACEMENT_3D('',#253006,#138285,#138286);
#110108=AXIS2_PLACEMENT_3D('',#253007,#138287,#138288);
#110109=AXIS2_PLACEMENT_3D('',#253008,#138289,#138290);
#110110=AXIS2_PLACEMENT_3D('',#253009,#138291,#138292);
#110111=AXIS2_PLACEMENT_3D('',#253028,#138293,#138294);
#110112=AXIS2_PLACEMENT_3D('',#253029,#138295,#138296);
#110113=AXIS2_PLACEMENT_3D('',#253030,#138297,#138298);
#110114=AXIS2_PLACEMENT_3D('',#253031,#138299,#138300);
#110115=AXIS2_PLACEMENT_3D('',#253032,#138301,#138302);
#110116=AXIS2_PLACEMENT_3D('',#253045,#138303,#138304);
#110117=AXIS2_PLACEMENT_3D('',#253064,#138305,#138306);
#110118=AXIS2_PLACEMENT_3D('',#253065,#138307,#138308);
#110119=AXIS2_PLACEMENT_3D('',#253066,#138309,#138310);
#110120=AXIS2_PLACEMENT_3D('',#253067,#138311,#138312);
#110121=AXIS2_PLACEMENT_3D('',#253068,#138313,#138314);
#110122=AXIS2_PLACEMENT_3D('',#253087,#138315,#138316);
#110123=AXIS2_PLACEMENT_3D('',#253100,#138317,#138318);
#110124=AXIS2_PLACEMENT_3D('',#253101,#138319,#138320);
#110125=AXIS2_PLACEMENT_3D('',#253102,#138321,#138322);
#110126=AXIS2_PLACEMENT_3D('',#253103,#138323,#138324);
#110127=AXIS2_PLACEMENT_3D('',#253104,#138325,#138326);
#110128=AXIS2_PLACEMENT_3D('',#253123,#138327,#138328);
#110129=AXIS2_PLACEMENT_3D('',#253124,#138329,#138330);
#110130=AXIS2_PLACEMENT_3D('',#253125,#138331,#138332);
#110131=AXIS2_PLACEMENT_3D('',#253126,#138333,#138334);
#110132=AXIS2_PLACEMENT_3D('',#253127,#138335,#138336);
#110133=AXIS2_PLACEMENT_3D('',#253140,#138337,#138338);
#110134=AXIS2_PLACEMENT_3D('',#253153,#138339,#138340);
#110135=AXIS2_PLACEMENT_3D('',#253154,#138341,#138342);
#110136=AXIS2_PLACEMENT_3D('',#253155,#138343,#138344);
#110137=AXIS2_PLACEMENT_3D('',#253156,#138345,#138346);
#110138=AXIS2_PLACEMENT_3D('',#253157,#138347,#138348);
#110139=AXIS2_PLACEMENT_3D('',#253170,#138349,#138350);
#110140=AXIS2_PLACEMENT_3D('',#253171,#138351,#138352);
#110141=AXIS2_PLACEMENT_3D('',#253172,#138353,#138354);
#110142=AXIS2_PLACEMENT_3D('',#253173,#138355,#138356);
#110143=AXIS2_PLACEMENT_3D('',#253174,#138357,#138358);
#110144=AXIS2_PLACEMENT_3D('',#253187,#138359,#138360);
#110145=AXIS2_PLACEMENT_3D('',#253188,#138361,#138362);
#110146=AXIS2_PLACEMENT_3D('',#253189,#138363,#138364);
#110147=AXIS2_PLACEMENT_3D('',#253190,#138365,#138366);
#110148=AXIS2_PLACEMENT_3D('',#253191,#138367,#138368);
#110149=AXIS2_PLACEMENT_3D('',#253204,#138369,#138370);
#110150=AXIS2_PLACEMENT_3D('',#253217,#138371,#138372);
#110151=AXIS2_PLACEMENT_3D('',#253218,#138373,#138374);
#110152=AXIS2_PLACEMENT_3D('',#253219,#138375,#138376);
#110153=AXIS2_PLACEMENT_3D('',#253220,#138377,#138378);
#110154=AXIS2_PLACEMENT_3D('',#253221,#138379,#138380);
#110155=AXIS2_PLACEMENT_3D('',#253240,#138381,#138382);
#110156=AXIS2_PLACEMENT_3D('',#253241,#138383,#138384);
#110157=AXIS2_PLACEMENT_3D('',#253242,#138385,#138386);
#110158=AXIS2_PLACEMENT_3D('',#253243,#138387,#138388);
#110159=AXIS2_PLACEMENT_3D('',#253244,#138389,#138390);
#110160=AXIS2_PLACEMENT_3D('',#253257,#138391,#138392);
#110161=AXIS2_PLACEMENT_3D('',#253276,#138393,#138394);
#110162=AXIS2_PLACEMENT_3D('',#253277,#138395,#138396);
#110163=AXIS2_PLACEMENT_3D('',#253278,#138397,#138398);
#110164=AXIS2_PLACEMENT_3D('',#253279,#138399,#138400);
#110165=AXIS2_PLACEMENT_3D('',#253280,#138401,#138402);
#110166=AXIS2_PLACEMENT_3D('',#253299,#138403,#138404);
#110167=AXIS2_PLACEMENT_3D('',#253312,#138405,#138406);
#110168=AXIS2_PLACEMENT_3D('',#253313,#138407,#138408);
#110169=AXIS2_PLACEMENT_3D('',#253314,#138409,#138410);
#110170=AXIS2_PLACEMENT_3D('',#253315,#138411,#138412);
#110171=AXIS2_PLACEMENT_3D('',#253316,#138413,#138414);
#110172=AXIS2_PLACEMENT_3D('',#253335,#138415,#138416);
#110173=AXIS2_PLACEMENT_3D('',#253336,#138417,#138418);
#110174=AXIS2_PLACEMENT_3D('',#253337,#138419,#138420);
#110175=AXIS2_PLACEMENT_3D('',#253338,#138421,#138422);
#110176=AXIS2_PLACEMENT_3D('',#253339,#138423,#138424);
#110177=AXIS2_PLACEMENT_3D('',#253352,#138425,#138426);
#110178=AXIS2_PLACEMENT_3D('',#253365,#138427,#138428);
#110179=AXIS2_PLACEMENT_3D('',#253366,#138429,#138430);
#110180=AXIS2_PLACEMENT_3D('',#253367,#138431,#138432);
#110181=AXIS2_PLACEMENT_3D('',#253368,#138433,#138434);
#110182=AXIS2_PLACEMENT_3D('',#253369,#138435,#138436);
#110183=AXIS2_PLACEMENT_3D('',#253382,#138437,#138438);
#110184=AXIS2_PLACEMENT_3D('',#253383,#138439,#138440);
#110185=AXIS2_PLACEMENT_3D('',#253384,#138441,#138442);
#110186=AXIS2_PLACEMENT_3D('',#253386,#138443,#138444);
#110187=AXIS2_PLACEMENT_3D('',#253388,#138445,#138446);
#110188=AXIS2_PLACEMENT_3D('',#253389,#138447,#138448);
#110189=AXIS2_PLACEMENT_3D('',#253390,#138449,#138450);
#110190=AXIS2_PLACEMENT_3D('',#253392,#138451,#138452);
#110191=AXIS2_PLACEMENT_3D('',#253394,#138453,#138454);
#110192=AXIS2_PLACEMENT_3D('',#253395,#138455,#138456);
#110193=AXIS2_PLACEMENT_3D('',#253396,#138457,#138458);
#110194=AXIS2_PLACEMENT_3D('',#253398,#138459,#138460);
#110195=AXIS2_PLACEMENT_3D('',#253400,#138461,#138462);
#110196=AXIS2_PLACEMENT_3D('',#253402,#138463,#138464);
#110197=AXIS2_PLACEMENT_3D('',#253403,#138465,#138466);
#110198=AXIS2_PLACEMENT_3D('',#253404,#138467,#138468);
#110199=AXIS2_PLACEMENT_3D('',#253406,#138469,#138470);
#110200=AXIS2_PLACEMENT_3D('',#253408,#138472,#138473);
#110201=AXIS2_PLACEMENT_3D('',#253410,#138475,#138476);
#110202=AXIS2_PLACEMENT_3D('',#253412,#138477,#138478);
#110203=AXIS2_PLACEMENT_3D('',#253415,#138480,#138481);
#110204=AXIS2_PLACEMENT_3D('',#253416,#138482,#138483);
#110205=AXIS2_PLACEMENT_3D('',#253417,#138484,#138485);
#110206=AXIS2_PLACEMENT_3D('',#253418,#138486,#138487);
#110207=AXIS2_PLACEMENT_3D('',#253419,#138488,#138489);
#110208=AXIS2_PLACEMENT_3D('',#253421,#138490,#138491);
#110209=AXIS2_PLACEMENT_3D('',#253423,#138492,#138493);
#110210=AXIS2_PLACEMENT_3D('',#253424,#138494,#138495);
#110211=AXIS2_PLACEMENT_3D('',#253425,#138496,#138497);
#110212=AXIS2_PLACEMENT_3D('',#253427,#138498,#138499);
#110213=AXIS2_PLACEMENT_3D('',#253429,#138500,#138501);
#110214=AXIS2_PLACEMENT_3D('',#253430,#138502,#138503);
#110215=AXIS2_PLACEMENT_3D('',#253431,#138504,#138505);
#110216=AXIS2_PLACEMENT_3D('',#253433,#138506,#138507);
#110217=AXIS2_PLACEMENT_3D('',#253435,#138509,#138510);
#110218=AXIS2_PLACEMENT_3D('',#253438,#138512,#138513);
#110219=AXIS2_PLACEMENT_3D('',#253439,#138514,#138515);
#110220=AXIS2_PLACEMENT_3D('',#253440,#138516,#138517);
#110221=AXIS2_PLACEMENT_3D('',#253441,#138518,#138519);
#110222=AXIS2_PLACEMENT_3D('',#253443,#138520,#138521);
#110223=AXIS2_PLACEMENT_3D('',#253445,#138522,#138523);
#110224=AXIS2_PLACEMENT_3D('',#253446,#138524,#138525);
#110225=AXIS2_PLACEMENT_3D('',#253447,#138526,#138527);
#110226=AXIS2_PLACEMENT_3D('',#253450,#138528,#138529);
#110227=AXIS2_PLACEMENT_3D('',#253452,#138530,#138531);
#110228=AXIS2_PLACEMENT_3D('',#253454,#138532,#138533);
#110229=AXIS2_PLACEMENT_3D('',#253455,#138534,#138535);
#110230=AXIS2_PLACEMENT_3D('',#253456,#138536,#138537);
#110231=AXIS2_PLACEMENT_3D('',#253459,#138538,#138539);
#110232=AXIS2_PLACEMENT_3D('',#253461,#138540,#138541);
#110233=AXIS2_PLACEMENT_3D('',#253463,#138542,#138543);
#110234=AXIS2_PLACEMENT_3D('',#253464,#138544,#138545);
#110235=AXIS2_PLACEMENT_3D('',#253465,#138546,#138547);
#110236=AXIS2_PLACEMENT_3D('',#253468,#138548,#138549);
#110237=AXIS2_PLACEMENT_3D('',#253470,#138550,#138551);
#110238=AXIS2_PLACEMENT_3D('',#253472,#138552,#138553);
#110239=AXIS2_PLACEMENT_3D('',#253473,#138554,#138555);
#110240=AXIS2_PLACEMENT_3D('',#253485,#138556,#138557);
#110241=AXIS2_PLACEMENT_3D('',#253487,#138558,#138559);
#110242=AXIS2_PLACEMENT_3D('',#253489,#138560,#138561);
#110243=AXIS2_PLACEMENT_3D('',#253490,#138562,#138563);
#110244=AXIS2_PLACEMENT_3D('',#253502,#138564,#138565);
#110245=AXIS2_PLACEMENT_3D('',#253504,#138566,#138567);
#110246=AXIS2_PLACEMENT_3D('',#253506,#138568,#138569);
#110247=AXIS2_PLACEMENT_3D('',#253507,#138570,#138571);
#110248=AXIS2_PLACEMENT_3D('',#253519,#138572,#138573);
#110249=AXIS2_PLACEMENT_3D('',#253521,#138574,#138575);
#110250=AXIS2_PLACEMENT_3D('',#253523,#138576,#138577);
#110251=AXIS2_PLACEMENT_3D('',#253524,#138578,#138579);
#110252=AXIS2_PLACEMENT_3D('',#253525,#138580,#138581);
#110253=AXIS2_PLACEMENT_3D('',#253527,#138582,#138583);
#110254=AXIS2_PLACEMENT_3D('',#253529,#138584,#138585);
#110255=AXIS2_PLACEMENT_3D('',#253530,#138586,#138587);
#110256=AXIS2_PLACEMENT_3D('',#253541,#138588,#138589);
#110257=AXIS2_PLACEMENT_3D('',#253543,#138590,#138591);
#110258=AXIS2_PLACEMENT_3D('',#253544,#138592,#138593);
#110259=AXIS2_PLACEMENT_3D('',#253545,#138594,#138595);
#110260=AXIS2_PLACEMENT_3D('',#253549,#138597,#138598);
#110261=AXIS2_PLACEMENT_3D('',#253579,#138600,#138601);
#110262=AXIS2_PLACEMENT_3D('',#253629,#138603,#138604);
#110263=AXIS2_PLACEMENT_3D('',#253631,#138606,#138607);
#110264=AXIS2_PLACEMENT_3D('',#253634,#138608,#138609);
#110265=AXIS2_PLACEMENT_3D('',#253639,#138610,#138611);
#110266=AXIS2_PLACEMENT_3D('',#253644,#138612,#138613);
#110267=AXIS2_PLACEMENT_3D('',#253646,#138614,#138615);
#110268=AXIS2_PLACEMENT_3D('',#253649,#138617,#138618);
#110269=AXIS2_PLACEMENT_3D('',#253650,#138619,#138620);
#110270=AXIS2_PLACEMENT_3D('',#253652,#138621,#138622);
#110271=AXIS2_PLACEMENT_3D('',#253655,#138624,#138625);
#110272=AXIS2_PLACEMENT_3D('',#253656,#138626,#138627);
#110273=AXIS2_PLACEMENT_3D('',#253658,#138628,#138629);
#110274=AXIS2_PLACEMENT_3D('',#253661,#138631,#138632);
#110275=AXIS2_PLACEMENT_3D('',#253662,#138633,#138634);
#110276=AXIS2_PLACEMENT_3D('',#253664,#138635,#138636);
#110277=AXIS2_PLACEMENT_3D('',#253667,#138638,#138639);
#110278=AXIS2_PLACEMENT_3D('',#253668,#138640,#138641);
#110279=AXIS2_PLACEMENT_3D('',#253670,#138642,#138643);
#110280=AXIS2_PLACEMENT_3D('',#253673,#138645,#138646);
#110281=AXIS2_PLACEMENT_3D('',#253674,#138647,#138648);
#110282=AXIS2_PLACEMENT_3D('',#253678,#138650,#138651);
#110283=AXIS2_PLACEMENT_3D('',#253680,#138653,#138654);
#110284=AXIS2_PLACEMENT_3D('',#253693,#138655,#138656);
#110285=AXIS2_PLACEMENT_3D('',#253756,#138657,#138658);
#110286=AXIS2_PLACEMENT_3D('',#253873,#138659,#138660);
#110287=AXIS2_PLACEMENT_3D('',#253930,#138661,#138662);
#110288=AXIS2_PLACEMENT_3D('',#253993,#138663,#138664);
#110289=AXIS2_PLACEMENT_3D('',#254050,#138665,#138666);
#110290=AXIS2_PLACEMENT_3D('',#254107,#138667,#138668);
#110291=AXIS2_PLACEMENT_3D('',#254164,#138669,#138670);
#110292=AXIS2_PLACEMENT_3D('',#254175,#138671,#138672);
#110293=AXIS2_PLACEMENT_3D('',#254178,#138673,#138674);
#110294=AXIS2_PLACEMENT_3D('',#254182,#138676,#138677);
#110295=AXIS2_PLACEMENT_3D('',#254193,#138679,#138680);
#110296=AXIS2_PLACEMENT_3D('',#254250,#138682,#138683);
#110297=AXIS2_PLACEMENT_3D('',#254252,#138685,#138686);
#110298=AXIS2_PLACEMENT_3D('',#254255,#138687,#138688);
#110299=AXIS2_PLACEMENT_3D('',#254259,#138690,#138691);
#110300=AXIS2_PLACEMENT_3D('',#254322,#138693,#138694);
#110301=AXIS2_PLACEMENT_3D('',#254379,#138696,#138697);
#110302=AXIS2_PLACEMENT_3D('',#254381,#138699,#138700);
#110303=AXIS2_PLACEMENT_3D('',#254387,#138704,#138705);
#110304=AXIS2_PLACEMENT_3D('',#254390,#138708,#138709);
#110305=AXIS2_PLACEMENT_3D('',#254399,#138714,#138715);
#110306=AXIS2_PLACEMENT_3D('',#254405,#138718,#138719);
#110307=AXIS2_PLACEMENT_3D('',#254464,#138720,#138721);
#110308=AXIS2_PLACEMENT_3D('',#254518,#138722,#138723);
#110309=AXIS2_PLACEMENT_3D('',#254519,#138724,#138725);
#110310=AXIS2_PLACEMENT_3D('',#254525,#138728,#138729);
#110311=AXIS2_PLACEMENT_3D('',#254585,#138730,#138731);
#110312=AXIS2_PLACEMENT_3D('',#254595,#138733,#138734);
#110313=AXIS2_PLACEMENT_3D('',#254596,#138735,#138736);
#110314=AXIS2_PLACEMENT_3D('',#254660,#138740,#138741);
#110315=AXIS2_PLACEMENT_3D('',#254665,#138743,#138744);
#110316=AXIS2_PLACEMENT_3D('',#254668,#138746,#138747);
#110317=AXIS2_PLACEMENT_3D('',#254669,#138748,#138749);
#110318=AXIS2_PLACEMENT_3D('',#254675,#138753,#138754);
#110319=AXIS2_PLACEMENT_3D('',#254677,#138755,#138756);
#110320=AXIS2_PLACEMENT_3D('',#254680,#138758,#138759);
#110321=AXIS2_PLACEMENT_3D('',#254681,#138760,#138761);
#110322=AXIS2_PLACEMENT_3D('',#254687,#138765,#138766);
#110323=AXIS2_PLACEMENT_3D('',#254689,#138767,#138768);
#110324=AXIS2_PLACEMENT_3D('',#254692,#138770,#138771);
#110325=AXIS2_PLACEMENT_3D('',#254693,#138772,#138773);
#110326=AXIS2_PLACEMENT_3D('',#254699,#138777,#138778);
#110327=AXIS2_PLACEMENT_3D('',#254701,#138779,#138780);
#110328=AXIS2_PLACEMENT_3D('',#254704,#138782,#138783);
#110329=AXIS2_PLACEMENT_3D('',#254705,#138784,#138785);
#110330=AXIS2_PLACEMENT_3D('',#254708,#138788,#138789);
#110331=AXIS2_PLACEMENT_3D('',#254759,#138791,#138792);
#110332=AXIS2_PLACEMENT_3D('',#254808,#138794,#138795);
#110333=AXIS2_PLACEMENT_3D('',#254847,#138799,#138800);
#110334=AXIS2_PLACEMENT_3D('',#254848,#138801,#138802);
#110335=AXIS2_PLACEMENT_3D('',#254860,#138805,#138806);
#110336=AXIS2_PLACEMENT_3D('',#254888,#138808,#138809);
#110337=AXIS2_PLACEMENT_3D('',#254889,#138810,#138811);
#110338=AXIS2_PLACEMENT_3D('',#254993,#138812,#138813);
#110339=AXIS2_PLACEMENT_3D('',#254996,#138814,#138815);
#110340=AXIS2_PLACEMENT_3D('',#255000,#138817,#138818);
#110341=AXIS2_PLACEMENT_3D('',#255002,#138820,#138821);
#110342=AXIS2_PLACEMENT_3D('',#255022,#138823,#138824);
#110343=AXIS2_PLACEMENT_3D('',#255024,#138825,#138826);
#110344=AXIS2_PLACEMENT_3D('',#255026,#138828,#138829);
#110345=AXIS2_PLACEMENT_3D('',#255029,#138830,#138831);
#110346=AXIS2_PLACEMENT_3D('',#255048,#138834,#138835);
#110347=AXIS2_PLACEMENT_3D('',#255049,#138836,#138837);
#110348=AXIS2_PLACEMENT_3D('',#255050,#138838,#138839);
#110349=AXIS2_PLACEMENT_3D('',#255053,#138840,#138841);
#110350=AXIS2_PLACEMENT_3D('',#255056,#138844,#138845);
#110351=AXIS2_PLACEMENT_3D('',#255061,#138847,#138848);
#110352=AXIS2_PLACEMENT_3D('',#255064,#138850,#138851);
#110353=AXIS2_PLACEMENT_3D('',#255065,#138852,#138853);
#110354=AXIS2_PLACEMENT_3D('',#255066,#138854,#138855);
#110355=AXIS2_PLACEMENT_3D('',#255067,#138856,#138857);
#110356=AXIS2_PLACEMENT_3D('',#255072,#138859,#138860);
#110357=AXIS2_PLACEMENT_3D('',#255075,#138862,#138863);
#110358=AXIS2_PLACEMENT_3D('',#255076,#138864,#138865);
#110359=AXIS2_PLACEMENT_3D('',#255081,#138867,#138868);
#110360=AXIS2_PLACEMENT_3D('',#255084,#138870,#138871);
#110361=AXIS2_PLACEMENT_3D('',#255085,#138872,#138873);
#110362=AXIS2_PLACEMENT_3D('',#255089,#138875,#138876);
#110363=AXIS2_PLACEMENT_3D('',#255091,#138878,#138879);
#110364=AXIS2_PLACEMENT_3D('',#255095,#138881,#138882);
#110365=AXIS2_PLACEMENT_3D('',#255097,#138884,#138885);
#110366=AXIS2_PLACEMENT_3D('',#255162,#138888,#138889);
#110367=AXIS2_PLACEMENT_3D('',#255224,#138892,#138893);
#110368=AXIS2_PLACEMENT_3D('',#255288,#138896,#138897);
#110369=AXIS2_PLACEMENT_3D('',#255291,#138898,#138899);
#110370=AXIS2_PLACEMENT_3D('',#255295,#138901,#138902);
#110371=AXIS2_PLACEMENT_3D('',#255297,#138904,#138905);
#110372=AXIS2_PLACEMENT_3D('',#255299,#138907,#138908);
#110373=AXIS2_PLACEMENT_3D('',#255360,#138911,#138912);
#110374=AXIS2_PLACEMENT_3D('',#255427,#138916,#138917);
#110375=AXIS2_PLACEMENT_3D('',#255430,#138918,#138919);
#110376=AXIS2_PLACEMENT_3D('',#255434,#138921,#138922);
#110377=AXIS2_PLACEMENT_3D('',#255438,#138924,#138925);
#110378=AXIS2_PLACEMENT_3D('',#255440,#138926,#138927);
#110379=AXIS2_PLACEMENT_3D('',#255442,#138928,#138929);
#110380=AXIS2_PLACEMENT_3D('',#255444,#138931,#138932);
#110381=AXIS2_PLACEMENT_3D('',#255508,#138936,#138937);
#110382=AXIS2_PLACEMENT_3D('',#255574,#138941,#138942);
#110383=AXIS2_PLACEMENT_3D('',#255577,#138943,#138944);
#110384=AXIS2_PLACEMENT_3D('',#255581,#138946,#138947);
#110385=AXIS2_PLACEMENT_3D('',#255584,#138950,#138951);
#110386=AXIS2_PLACEMENT_3D('',#255588,#138953,#138954);
#110387=AXIS2_PLACEMENT_3D('',#255591,#138957,#138958);
#110388=AXIS2_PLACEMENT_3D('',#255592,#138959,#138960);
#110389=AXIS2_PLACEMENT_3D('',#255593,#138961,#138962);
#110390=AXIS2_PLACEMENT_3D('',#255594,#138963,#138964);
#110391=AXIS2_PLACEMENT_3D('',#255595,#138965,#138966);
#110392=AXIS2_PLACEMENT_3D('',#255600,#138967,#138968);
#110393=AXIS2_PLACEMENT_3D('',#255601,#138969,#138970);
#110394=AXIS2_PLACEMENT_3D('',#255606,#138971,#138972);
#110395=AXIS2_PLACEMENT_3D('',#255615,#138973,#138974);
#110396=AXIS2_PLACEMENT_3D('',#255624,#138975,#138976);
#110397=AXIS2_PLACEMENT_3D('',#255626,#138977,#138978);
#110398=AXIS2_PLACEMENT_3D('',#255694,#138979,#138980);
#110399=AXIS2_PLACEMENT_3D('',#255719,#138981,#138982);
#110400=AXIS2_PLACEMENT_3D('',#255788,#138983,#138984);
#110401=AXIS2_PLACEMENT_3D('',#255789,#138985,#138986);
#110402=AXIS2_PLACEMENT_3D('',#255814,#138987,#138988);
#110403=AXIS2_PLACEMENT_3D('',#255816,#138989,#138990);
#110404=AXIS2_PLACEMENT_3D('',#255908,#138991,#138992);
#110405=AXIS2_PLACEMENT_3D('',#255941,#138993,#138994);
#110406=AXIS2_PLACEMENT_3D('',#255966,#138995,#138996);
#110407=AXIS2_PLACEMENT_3D('',#255968,#138997,#138998);
#110408=AXIS2_PLACEMENT_3D('',#256060,#138999,#139000);
#110409=AXIS2_PLACEMENT_3D('',#256129,#139001,#139002);
#110410=AXIS2_PLACEMENT_3D('',#256211,#139003,#139004);
#110411=AXIS2_PLACEMENT_3D('',#256212,#139005,#139006);
#110412=AXIS2_PLACEMENT_3D('',#256213,#139007,#139008);
#110413=AXIS2_PLACEMENT_3D('',#256214,#139009,#139010);
#110414=AXIS2_PLACEMENT_3D('',#256215,#139011,#139012);
#110415=AXIS2_PLACEMENT_3D('',#256216,#139013,#139014);
#110416=AXIS2_PLACEMENT_3D('',#256217,#139015,#139016);
#110417=AXIS2_PLACEMENT_3D('',#256218,#139017,#139018);
#110418=AXIS2_PLACEMENT_3D('',#256228,#139019,#139020);
#110419=AXIS2_PLACEMENT_3D('',#256320,#139021,#139022);
#110420=AXIS2_PLACEMENT_3D('',#256321,#139023,#139024);
#110421=AXIS2_PLACEMENT_3D('',#256322,#139025,#139026);
#110422=AXIS2_PLACEMENT_3D('',#256372,#139027,#139028);
#110423=AXIS2_PLACEMENT_3D('',#256373,#139029,#139030);
#110424=AXIS2_PLACEMENT_3D('',#256416,#139031,#139032);
#110425=AXIS2_PLACEMENT_3D('',#256417,#139033,#139034);
#110426=AXIS2_PLACEMENT_3D('',#256418,#139035,#139036);
#110427=AXIS2_PLACEMENT_3D('',#256419,#139037,#139038);
#110428=AXIS2_PLACEMENT_3D('',#256511,#139039,#139040);
#110429=AXIS2_PLACEMENT_3D('',#256512,#139041,#139042);
#110430=AXIS2_PLACEMENT_3D('',#256513,#139043,#139044);
#110431=AXIS2_PLACEMENT_3D('',#256563,#139045,#139046);
#110432=AXIS2_PLACEMENT_3D('',#256564,#139047,#139048);
#110433=AXIS2_PLACEMENT_3D('',#256607,#139049,#139050);
#110434=AXIS2_PLACEMENT_3D('',#256608,#139051,#139052);
#110435=AXIS2_PLACEMENT_3D('',#256609,#139053,#139054);
#110436=AXIS2_PLACEMENT_3D('',#256610,#139055,#139056);
#110437=AXIS2_PLACEMENT_3D('',#256611,#139057,#139058);
#110438=AXIS2_PLACEMENT_3D('',#256703,#139059,#139060);
#110439=AXIS2_PLACEMENT_3D('',#256704,#139061,#139062);
#110440=AXIS2_PLACEMENT_3D('',#256705,#139063,#139064);
#110441=AXIS2_PLACEMENT_3D('',#256755,#139065,#139066);
#110442=AXIS2_PLACEMENT_3D('',#256756,#139067,#139068);
#110443=AXIS2_PLACEMENT_3D('',#256799,#139069,#139070);
#110444=AXIS2_PLACEMENT_3D('',#256800,#139071,#139072);
#110445=AXIS2_PLACEMENT_3D('',#256843,#139073,#139074);
#110446=AXIS2_PLACEMENT_3D('',#256844,#139075,#139076);
#110447=AXIS2_PLACEMENT_3D('',#256845,#139077,#139078);
#110448=AXIS2_PLACEMENT_3D('',#256846,#139079,#139080);
#110449=AXIS2_PLACEMENT_3D('',#256847,#139081,#139082);
#110450=AXIS2_PLACEMENT_3D('',#256948,#139083,#139084);
#110451=AXIS2_PLACEMENT_3D('',#256949,#139085,#139086);
#110452=AXIS2_PLACEMENT_3D('',#256950,#139087,#139088);
#110453=AXIS2_PLACEMENT_3D('',#256951,#139089,#139090);
#110454=AXIS2_PLACEMENT_3D('',#257052,#139091,#139092);
#110455=AXIS2_PLACEMENT_3D('',#257153,#139093,#139094);
#110456=AXIS2_PLACEMENT_3D('',#257245,#139095,#139096);
#110457=AXIS2_PLACEMENT_3D('',#257346,#139097,#139098);
#110458=AXIS2_PLACEMENT_3D('',#257447,#139099,#139100);
#110459=AXIS2_PLACEMENT_3D('',#257548,#139101,#139102);
#110460=AXIS2_PLACEMENT_3D('',#257549,#139103,#139104);
#110461=AXIS2_PLACEMENT_3D('',#257550,#139105,#139106);
#110462=AXIS2_PLACEMENT_3D('',#257551,#139107,#139108);
#110463=AXIS2_PLACEMENT_3D('',#257889,#139109,#139110);
#110464=AXIS2_PLACEMENT_3D('',#257890,#139111,#139112);
#110465=AXIS2_PLACEMENT_3D('',#257891,#139113,#139114);
#110466=AXIS2_PLACEMENT_3D('',#258357,#139115,#139116);
#110467=AXIS2_PLACEMENT_3D('',#258358,#139117,#139118);
#110468=AXIS2_PLACEMENT_3D('',#258359,#139119,#139120);
#110469=AXIS2_PLACEMENT_3D('',#258825,#139121,#139122);
#110470=AXIS2_PLACEMENT_3D('',#258826,#139123,#139124);
#110471=AXIS2_PLACEMENT_3D('',#258827,#139125,#139126);
#110472=AXIS2_PLACEMENT_3D('',#259006,#139127,#139128);
#110473=AXIS2_PLACEMENT_3D('',#259235,#139129,#139130);
#110474=AXIS2_PLACEMENT_3D('',#259236,#139131,#139132);
#110475=AXIS2_PLACEMENT_3D('',#259237,#139133,#139134);
#110476=AXIS2_PLACEMENT_3D('',#259539,#139135,#139136);
#110477=AXIS2_PLACEMENT_3D('',#259552,#139137,#139138);
#110478=AXIS2_PLACEMENT_3D('',#259553,#139139,#139140);
#110479=AXIS2_PLACEMENT_3D('',#259612,#139141,#139142);
#110480=AXIS2_PLACEMENT_3D('',#259625,#139143,#139144);
#110481=AXIS2_PLACEMENT_3D('',#259626,#139145,#139146);
#110482=AXIS2_PLACEMENT_3D('',#259651,#139147,#139148);
#110483=AXIS2_PLACEMENT_3D('',#259652,#139149,#139150);
#110484=AXIS2_PLACEMENT_3D('',#259671,#139151,#139152);
#110485=AXIS2_PLACEMENT_3D('',#259672,#139153,#139154);
#110486=AXIS2_PLACEMENT_3D('',#259737,#139155,#139156);
#110487=AXIS2_PLACEMENT_3D('',#259810,#139157,#139158);
#110488=AXIS2_PLACEMENT_3D('',#259823,#139159,#139160);
#110489=AXIS2_PLACEMENT_3D('',#259944,#139161,#139162);
#110490=AXIS2_PLACEMENT_3D('',#259957,#139163,#139164);
#110491=AXIS2_PLACEMENT_3D('',#260084,#139165,#139166);
#110492=AXIS2_PLACEMENT_3D('',#260097,#139167,#139168);
#110493=AXIS2_PLACEMENT_3D('',#260218,#139169,#139170);
#110494=AXIS2_PLACEMENT_3D('',#260231,#139171,#139172);
#110495=AXIS2_PLACEMENT_3D('',#260358,#139173,#139174);
#110496=AXIS2_PLACEMENT_3D('',#260371,#139175,#139176);
#110497=AXIS2_PLACEMENT_3D('',#260492,#139177,#139178);
#110498=AXIS2_PLACEMENT_3D('',#260505,#139179,#139180);
#110499=AXIS2_PLACEMENT_3D('',#260530,#139181,#139182);
#110500=AXIS2_PLACEMENT_3D('',#260543,#139183,#139184);
#110501=AXIS2_PLACEMENT_3D('',#260766,#139185,#139186);
#110502=AXIS2_PLACEMENT_3D('',#260779,#139187,#139188);
#110503=AXIS2_PLACEMENT_3D('',#260834,#139189,#139190);
#110504=AXIS2_PLACEMENT_3D('',#260835,#139191,#139192);
#110505=AXIS2_PLACEMENT_3D('',#260892,#139193,#139194);
#110506=AXIS2_PLACEMENT_3D('',#260893,#139195,#139196);
#110507=AXIS2_PLACEMENT_3D('',#260908,#139197,#139198);
#110508=AXIS2_PLACEMENT_3D('',#260909,#139199,#139200);
#110509=AXIS2_PLACEMENT_3D('',#260912,#139201,#139202);
#110510=AXIS2_PLACEMENT_3D('',#260913,#139203,#139204);
#110511=AXIS2_PLACEMENT_3D('',#260916,#139205,#139206);
#110512=AXIS2_PLACEMENT_3D('',#260918,#139207,#139208);
#110513=AXIS2_PLACEMENT_3D('',#260919,#139209,#139210);
#110514=AXIS2_PLACEMENT_3D('',#260920,#139211,#139212);
#110515=AXIS2_PLACEMENT_3D('',#260921,#139213,#139214);
#110516=AXIS2_PLACEMENT_3D('',#260924,#139215,#139216);
#110517=AXIS2_PLACEMENT_3D('',#260926,#139217,#139218);
#110518=AXIS2_PLACEMENT_3D('',#260927,#139219,#139220);
#110519=AXIS2_PLACEMENT_3D('',#260928,#139221,#139222);
#110520=AXIS2_PLACEMENT_3D('',#261224,#139223,#139224);
#110521=AXIS2_PLACEMENT_3D('',#261264,#139225,#139226);
#110522=AXIS2_PLACEMENT_3D('',#261266,#139227,#139228);
#110523=AXIS2_PLACEMENT_3D('',#261273,#139229,#139230);
#110524=AXIS2_PLACEMENT_3D('',#261324,#139231,#139232);
#110525=AXIS2_PLACEMENT_3D('',#261326,#139233,#139234);
#110526=AXIS2_PLACEMENT_3D('',#261329,#139236,#139237);
#110527=AXIS2_PLACEMENT_3D('',#261410,#139238,#139239);
#110528=AXIS2_PLACEMENT_3D('',#261412,#139241,#139242);
#110529=AXIS2_PLACEMENT_3D('',#261414,#139243,#139244);
#110530=AXIS2_PLACEMENT_3D('',#261415,#139245,#139246);
#110531=AXIS2_PLACEMENT_3D('',#261476,#139247,#139248);
#110532=AXIS2_PLACEMENT_3D('',#261479,#139249,#139250);
#110533=AXIS2_PLACEMENT_3D('',#261481,#139251,#139252);
#110534=AXIS2_PLACEMENT_3D('',#261482,#139253,#139254);
#110535=AXIS2_PLACEMENT_3D('',#261483,#139255,#139256);
#110536=AXIS2_PLACEMENT_3D('',#261484,#139257,#139258);
#110537=AXIS2_PLACEMENT_3D('',#261486,#139259,#139260);
#110538=AXIS2_PLACEMENT_3D('',#261488,#139261,#139262);
#110539=AXIS2_PLACEMENT_3D('',#261490,#139263,#139264);
#110540=AXIS2_PLACEMENT_3D('',#261491,#139265,#139266);
#110541=AXIS2_PLACEMENT_3D('',#261492,#139267,#139268);
#110542=AXIS2_PLACEMENT_3D('',#261568,#139270,#139271);
#110543=AXIS2_PLACEMENT_3D('',#261570,#139272,#139273);
#110544=AXIS2_PLACEMENT_3D('',#261572,#139275,#139276);
#110545=AXIS2_PLACEMENT_3D('',#261575,#139278,#139279);
#110546=AXIS2_PLACEMENT_3D('',#261576,#139280,#139281);
#110547=AXIS2_PLACEMENT_3D('',#261577,#139282,#139283);
#110548=AXIS2_PLACEMENT_3D('',#261578,#139284,#139285);
#110549=AXIS2_PLACEMENT_3D('',#261580,#139286,#139287);
#110550=AXIS2_PLACEMENT_3D('',#261582,#139288,#139289);
#110551=AXIS2_PLACEMENT_3D('',#261583,#139290,#139291);
#110552=AXIS2_PLACEMENT_3D('',#261584,#139292,#139293);
#110553=AXIS2_PLACEMENT_3D('',#261586,#139294,#139295);
#110554=AXIS2_PLACEMENT_3D('',#261588,#139296,#139297);
#110555=AXIS2_PLACEMENT_3D('',#261590,#139298,#139299);
#110556=AXIS2_PLACEMENT_3D('',#261591,#139300,#139301);
#110557=AXIS2_PLACEMENT_3D('',#261592,#139302,#139303);
#110558=AXIS2_PLACEMENT_3D('',#261595,#139304,#139305);
#110559=AXIS2_PLACEMENT_3D('',#261596,#139306,#139307);
#110560=AXIS2_PLACEMENT_3D('',#261598,#139308,#139309);
#110561=AXIS2_PLACEMENT_3D('',#261599,#139310,#139311);
#110562=AXIS2_PLACEMENT_3D('',#261600,#139312,#139313);
#110563=AXIS2_PLACEMENT_3D('',#261602,#139314,#139315);
#110564=AXIS2_PLACEMENT_3D('',#261604,#139316,#139317);
#110565=AXIS2_PLACEMENT_3D('',#261605,#139318,#139319);
#110566=AXIS2_PLACEMENT_3D('',#261606,#139320,#139321);
#110567=AXIS2_PLACEMENT_3D('',#261608,#139322,#139323);
#110568=AXIS2_PLACEMENT_3D('',#261610,#139324,#139325);
#110569=AXIS2_PLACEMENT_3D('',#261611,#139326,#139327);
#110570=AXIS2_PLACEMENT_3D('',#261612,#139328,#139329);
#110571=AXIS2_PLACEMENT_3D('',#261614,#139330,#139331);
#110572=AXIS2_PLACEMENT_3D('',#261617,#139333,#139334);
#110573=AXIS2_PLACEMENT_3D('',#261618,#139335,#139336);
#110574=AXIS2_PLACEMENT_3D('',#261620,#139338,#139339);
#110575=AXIS2_PLACEMENT_3D('',#261622,#139341,#139342);
#110576=AXIS2_PLACEMENT_3D('',#261624,#139343,#139344);
#110577=AXIS2_PLACEMENT_3D('',#261626,#139346,#139347);
#110578=AXIS2_PLACEMENT_3D('',#261629,#139349,#139350);
#110579=AXIS2_PLACEMENT_3D('',#261630,#139351,#139352);
#110580=AXIS2_PLACEMENT_3D('',#261632,#139353,#139354);
#110581=AXIS2_PLACEMENT_3D('',#261635,#139356,#139357);
#110582=AXIS2_PLACEMENT_3D('',#261636,#139358,#139359);
#110583=AXIS2_PLACEMENT_3D('',#261637,#139360,#139361);
#110584=AXIS2_PLACEMENT_3D('',#261638,#139362,#139363);
#110585=AXIS2_PLACEMENT_3D('',#261639,#139364,#139365);
#110586=AXIS2_PLACEMENT_3D('',#261640,#139366,#139367);
#110587=AXIS2_PLACEMENT_3D('',#261641,#139368,#139369);
#110588=AXIS2_PLACEMENT_3D('',#261662,#139371,#139372);
#110589=AXIS2_PLACEMENT_3D('',#261678,#139373,#139374);
#110590=AXIS2_PLACEMENT_3D('',#261716,#139376,#139377);
#110591=AXIS2_PLACEMENT_3D('',#261754,#139379,#139380);
#110592=AXIS2_PLACEMENT_3D('',#261792,#139382,#139383);
#110593=AXIS2_PLACEMENT_3D('',#261830,#139385,#139386);
#110594=AXIS2_PLACEMENT_3D('',#261868,#139388,#139389);
#110595=AXIS2_PLACEMENT_3D('',#261883,#139391,#139392);
#110596=AXIS2_PLACEMENT_3D('',#261884,#139393,#139394);
#110597=AXIS2_PLACEMENT_3D('',#261925,#139396,#139397);
#110598=AXIS2_PLACEMENT_3D('',#261938,#139398,#139399);
#110599=AXIS2_PLACEMENT_3D('',#262014,#139401,#139402);
#110600=AXIS2_PLACEMENT_3D('',#262090,#139404,#139405);
#110601=AXIS2_PLACEMENT_3D('',#262166,#139407,#139408);
#110602=AXIS2_PLACEMENT_3D('',#262242,#139410,#139411);
#110603=AXIS2_PLACEMENT_3D('',#262320,#139413,#139414);
#110604=AXIS2_PLACEMENT_3D('',#262325,#139416,#139417);
#110605=AXIS2_PLACEMENT_3D('',#262386,#139418,#139419);
#110606=AXIS2_PLACEMENT_3D('',#262388,#139420,#139421);
#110607=AXIS2_PLACEMENT_3D('',#262390,#139422,#139423);
#110608=AXIS2_PLACEMENT_3D('',#262391,#139424,#139425);
#110609=AXIS2_PLACEMENT_3D('',#262394,#139427,#139428);
#110610=AXIS2_PLACEMENT_3D('',#262395,#139429,#139430);
#110611=AXIS2_PLACEMENT_3D('',#262398,#139431,#139432);
#110612=AXIS2_PLACEMENT_3D('',#262399,#139433,#139434);
#110613=AXIS2_PLACEMENT_3D('',#262400,#139435,#139436);
#110614=AXIS2_PLACEMENT_3D('',#262401,#139437,#139438);
#110615=AXIS2_PLACEMENT_3D('',#262404,#139440,#139441);
#110616=AXIS2_PLACEMENT_3D('',#262405,#139442,#139443);
#110617=AXIS2_PLACEMENT_3D('',#262426,#139444,#139445);
#110618=AXIS2_PLACEMENT_3D('',#262427,#139446,#139447);
#110619=AXIS2_PLACEMENT_3D('',#262430,#139448,#139449);
#110620=AXIS2_PLACEMENT_3D('',#262432,#139450,#139451);
#110621=AXIS2_PLACEMENT_3D('',#262434,#139452,#139453);
#110622=AXIS2_PLACEMENT_3D('',#262436,#139454,#139455);
#110623=AXIS2_PLACEMENT_3D('',#262438,#139456,#139457);
#110624=AXIS2_PLACEMENT_3D('',#262439,#139458,#139459);
#110625=AXIS2_PLACEMENT_3D('',#262440,#139460,#139461);
#110626=AXIS2_PLACEMENT_3D('',#262444,#139462,#139463);
#110627=AXIS2_PLACEMENT_3D('',#262448,#139464,#139465);
#110628=AXIS2_PLACEMENT_3D('',#262452,#139466,#139467);
#110629=AXIS2_PLACEMENT_3D('',#262456,#139468,#139469);
#110630=AXIS2_PLACEMENT_3D('',#262460,#139470,#139471);
#110631=AXIS2_PLACEMENT_3D('',#262464,#139472,#139473);
#110632=AXIS2_PLACEMENT_3D('',#262477,#139480,#139481);
#110633=AXIS2_PLACEMENT_3D('',#262480,#139484,#139485);
#110634=AXIS2_PLACEMENT_3D('',#262482,#139487,#139488);
#110635=AXIS2_PLACEMENT_3D('',#262484,#139490,#139491);
#110636=AXIS2_PLACEMENT_3D('',#262486,#139493,#139494);
#110637=AXIS2_PLACEMENT_3D('',#262488,#139496,#139497);
#110638=AXIS2_PLACEMENT_3D('',#262828,#139498,#139499);
#110639=AXIS2_PLACEMENT_3D('',#263168,#139500,#139501);
#110640=AXIS2_PLACEMENT_3D('',#263189,#139503,#139504);
#110641=AXIS2_PLACEMENT_3D('',#263205,#139505,#139506);
#110642=AXIS2_PLACEMENT_3D('',#263243,#139508,#139509);
#110643=AXIS2_PLACEMENT_3D('',#263281,#139511,#139512);
#110644=AXIS2_PLACEMENT_3D('',#263319,#139514,#139515);
#110645=AXIS2_PLACEMENT_3D('',#263357,#139517,#139518);
#110646=AXIS2_PLACEMENT_3D('',#263395,#139520,#139521);
#110647=AXIS2_PLACEMENT_3D('',#263410,#139523,#139524);
#110648=AXIS2_PLACEMENT_3D('',#263411,#139525,#139526);
#110649=AXIS2_PLACEMENT_3D('',#263452,#139528,#139529);
#110650=AXIS2_PLACEMENT_3D('',#263465,#139530,#139531);
#110651=AXIS2_PLACEMENT_3D('',#263541,#139533,#139534);
#110652=AXIS2_PLACEMENT_3D('',#263617,#139536,#139537);
#110653=AXIS2_PLACEMENT_3D('',#263693,#139539,#139540);
#110654=AXIS2_PLACEMENT_3D('',#263769,#139542,#139543);
#110655=AXIS2_PLACEMENT_3D('',#263847,#139545,#139546);
#110656=AXIS2_PLACEMENT_3D('',#263852,#139548,#139549);
#110657=AXIS2_PLACEMENT_3D('',#263913,#139550,#139551);
#110658=AXIS2_PLACEMENT_3D('',#263915,#139552,#139553);
#110659=AXIS2_PLACEMENT_3D('',#263917,#139554,#139555);
#110660=AXIS2_PLACEMENT_3D('',#263918,#139556,#139557);
#110661=AXIS2_PLACEMENT_3D('',#263921,#139559,#139560);
#110662=AXIS2_PLACEMENT_3D('',#263922,#139561,#139562);
#110663=AXIS2_PLACEMENT_3D('',#263925,#139563,#139564);
#110664=AXIS2_PLACEMENT_3D('',#263926,#139565,#139566);
#110665=AXIS2_PLACEMENT_3D('',#263927,#139567,#139568);
#110666=AXIS2_PLACEMENT_3D('',#263928,#139569,#139570);
#110667=AXIS2_PLACEMENT_3D('',#263931,#139572,#139573);
#110668=AXIS2_PLACEMENT_3D('',#263932,#139574,#139575);
#110669=AXIS2_PLACEMENT_3D('',#263953,#139576,#139577);
#110670=AXIS2_PLACEMENT_3D('',#263954,#139578,#139579);
#110671=AXIS2_PLACEMENT_3D('',#263957,#139580,#139581);
#110672=AXIS2_PLACEMENT_3D('',#263959,#139582,#139583);
#110673=AXIS2_PLACEMENT_3D('',#263961,#139584,#139585);
#110674=AXIS2_PLACEMENT_3D('',#263963,#139586,#139587);
#110675=AXIS2_PLACEMENT_3D('',#263965,#139588,#139589);
#110676=AXIS2_PLACEMENT_3D('',#263966,#139590,#139591);
#110677=AXIS2_PLACEMENT_3D('',#263967,#139592,#139593);
#110678=AXIS2_PLACEMENT_3D('',#263971,#139594,#139595);
#110679=AXIS2_PLACEMENT_3D('',#263975,#139596,#139597);
#110680=AXIS2_PLACEMENT_3D('',#263979,#139598,#139599);
#110681=AXIS2_PLACEMENT_3D('',#263983,#139600,#139601);
#110682=AXIS2_PLACEMENT_3D('',#263987,#139602,#139603);
#110683=AXIS2_PLACEMENT_3D('',#263991,#139604,#139605);
#110684=AXIS2_PLACEMENT_3D('',#264004,#139612,#139613);
#110685=AXIS2_PLACEMENT_3D('',#264007,#139616,#139617);
#110686=AXIS2_PLACEMENT_3D('',#264009,#139619,#139620);
#110687=AXIS2_PLACEMENT_3D('',#264011,#139622,#139623);
#110688=AXIS2_PLACEMENT_3D('',#264013,#139625,#139626);
#110689=AXIS2_PLACEMENT_3D('',#264015,#139628,#139629);
#110690=AXIS2_PLACEMENT_3D('',#264355,#139630,#139631);
#110691=AXIS2_PLACEMENT_3D('',#264695,#139632,#139633);
#110692=AXIS2_PLACEMENT_3D('',#264697,#139634,#139635);
#110693=AXIS2_PLACEMENT_3D('',#264700,#139637,#139638);
#110694=AXIS2_PLACEMENT_3D('',#264701,#139639,#139640);
#110695=AXIS2_PLACEMENT_3D('',#264704,#139641,#139642);
#110696=AXIS2_PLACEMENT_3D('',#264705,#139643,#139644);
#110697=AXIS2_PLACEMENT_3D('',#264708,#139646,#139647);
#110698=AXIS2_PLACEMENT_3D('',#264709,#139648,#139649);
#110699=AXIS2_PLACEMENT_3D('',#264711,#139650,#139651);
#110700=AXIS2_PLACEMENT_3D('',#264714,#139653,#139654);
#110701=AXIS2_PLACEMENT_3D('',#264715,#139655,#139656);
#110702=AXIS2_PLACEMENT_3D('',#264718,#139657,#139658);
#110703=AXIS2_PLACEMENT_3D('',#264719,#139659,#139660);
#110704=AXIS2_PLACEMENT_3D('',#264722,#139662,#139663);
#110705=AXIS2_PLACEMENT_3D('',#264723,#139664,#139665);
#110706=AXIS2_PLACEMENT_3D('',#264804,#139668,#139669);
#110707=AXIS2_PLACEMENT_3D('',#264841,#139671,#139672);
#110708=AXIS2_PLACEMENT_3D('',#264882,#139674,#139675);
#110709=AXIS2_PLACEMENT_3D('',#264885,#139678,#139679);
#110710=AXIS2_PLACEMENT_3D('',#264886,#139680,#139681);
#110711=AXIS2_PLACEMENT_3D('',#264887,#139682,#139683);
#110712=AXIS2_PLACEMENT_3D('',#264889,#139684,#139685);
#110713=AXIS2_PLACEMENT_3D('',#264892,#139687,#139688);
#110714=AXIS2_PLACEMENT_3D('',#264893,#139689,#139690);
#110715=AXIS2_PLACEMENT_3D('',#264895,#139691,#139692);
#110716=AXIS2_PLACEMENT_3D('',#264898,#139694,#139695);
#110717=AXIS2_PLACEMENT_3D('',#264899,#139696,#139697);
#110718=AXIS2_PLACEMENT_3D('',#264901,#139698,#139699);
#110719=AXIS2_PLACEMENT_3D('',#264903,#139700,#139701);
#110720=AXIS2_PLACEMENT_3D('',#264905,#139702,#139703);
#110721=AXIS2_PLACEMENT_3D('',#264906,#139704,#139705);
#110722=AXIS2_PLACEMENT_3D('',#264907,#139706,#139707);
#110723=AXIS2_PLACEMENT_3D('',#264909,#139708,#139709);
#110724=AXIS2_PLACEMENT_3D('',#264911,#139711,#139712);
#110725=AXIS2_PLACEMENT_3D('',#264914,#139713,#139714);
#110726=AXIS2_PLACEMENT_3D('',#264918,#139716,#139717);
#110727=AXIS2_PLACEMENT_3D('',#264920,#139719,#139720);
#110728=AXIS2_PLACEMENT_3D('',#264922,#139721,#139722);
#110729=AXIS2_PLACEMENT_3D('',#264925,#139724,#139725);
#110730=AXIS2_PLACEMENT_3D('',#264926,#139726,#139727);
#110731=AXIS2_PLACEMENT_3D('',#264928,#139728,#139729);
#110732=AXIS2_PLACEMENT_3D('',#264931,#139731,#139732);
#110733=AXIS2_PLACEMENT_3D('',#264932,#139733,#139734);
#110734=AXIS2_PLACEMENT_3D('',#264934,#139735,#139736);
#110735=AXIS2_PLACEMENT_3D('',#264937,#139738,#139739);
#110736=AXIS2_PLACEMENT_3D('',#264938,#139740,#139741);
#110737=AXIS2_PLACEMENT_3D('',#264940,#139742,#139743);
#110738=AXIS2_PLACEMENT_3D('',#264943,#139745,#139746);
#110739=AXIS2_PLACEMENT_3D('',#264944,#139747,#139748);
#110740=AXIS2_PLACEMENT_3D('',#264946,#139749,#139750);
#110741=AXIS2_PLACEMENT_3D('',#264949,#139752,#139753);
#110742=AXIS2_PLACEMENT_3D('',#264950,#139754,#139755);
#110743=AXIS2_PLACEMENT_3D('',#264952,#139756,#139757);
#110744=AXIS2_PLACEMENT_3D('',#264955,#139759,#139760);
#110745=AXIS2_PLACEMENT_3D('',#264956,#139761,#139762);
#110746=AXIS2_PLACEMENT_3D('',#264958,#139763,#139764);
#110747=AXIS2_PLACEMENT_3D('',#264961,#139766,#139767);
#110748=AXIS2_PLACEMENT_3D('',#264962,#139768,#139769);
#110749=AXIS2_PLACEMENT_3D('',#264964,#139770,#139771);
#110750=AXIS2_PLACEMENT_3D('',#264967,#139773,#139774);
#110751=AXIS2_PLACEMENT_3D('',#264968,#139775,#139776);
#110752=AXIS2_PLACEMENT_3D('',#264970,#139777,#139778);
#110753=AXIS2_PLACEMENT_3D('',#264973,#139780,#139781);
#110754=AXIS2_PLACEMENT_3D('',#264974,#139782,#139783);
#110755=AXIS2_PLACEMENT_3D('',#264976,#139784,#139785);
#110756=AXIS2_PLACEMENT_3D('',#264979,#139787,#139788);
#110757=AXIS2_PLACEMENT_3D('',#264980,#139789,#139790);
#110758=AXIS2_PLACEMENT_3D('',#264985,#139792,#139793);
#110759=AXIS2_PLACEMENT_3D('',#264988,#139795,#139796);
#110760=AXIS2_PLACEMENT_3D('',#264989,#139797,#139798);
#110761=AXIS2_PLACEMENT_3D('',#264995,#139802,#139803);
#110762=AXIS2_PLACEMENT_3D('',#264997,#139804,#139805);
#110763=AXIS2_PLACEMENT_3D('',#265000,#139807,#139808);
#110764=AXIS2_PLACEMENT_3D('',#265001,#139809,#139810);
#110765=AXIS2_PLACEMENT_3D('',#265007,#139814,#139815);
#110766=AXIS2_PLACEMENT_3D('',#265009,#139816,#139817);
#110767=AXIS2_PLACEMENT_3D('',#265012,#139819,#139820);
#110768=AXIS2_PLACEMENT_3D('',#265013,#139821,#139822);
#110769=AXIS2_PLACEMENT_3D('',#265019,#139826,#139827);
#110770=AXIS2_PLACEMENT_3D('',#265021,#139828,#139829);
#110771=AXIS2_PLACEMENT_3D('',#265024,#139831,#139832);
#110772=AXIS2_PLACEMENT_3D('',#265025,#139833,#139834);
#110773=AXIS2_PLACEMENT_3D('',#265028,#139837,#139838);
#110774=AXIS2_PLACEMENT_3D('',#265033,#139840,#139841);
#110775=AXIS2_PLACEMENT_3D('',#265037,#139843,#139844);
#110776=AXIS2_PLACEMENT_3D('',#265041,#139846,#139847);
#110777=AXIS2_PLACEMENT_3D('',#265044,#139849,#139850);
#110778=AXIS2_PLACEMENT_3D('',#265045,#139851,#139852);
#110779=AXIS2_PLACEMENT_3D('',#265046,#139853,#139854);
#110780=AXIS2_PLACEMENT_3D('',#265047,#139855,#139856);
#110781=AXIS2_PLACEMENT_3D('',#265048,#139857,#139858);
#110782=AXIS2_PLACEMENT_3D('',#265049,#139859,#139860);
#110783=AXIS2_PLACEMENT_3D('',#265052,#139861,#139862);
#110784=AXIS2_PLACEMENT_3D('',#265056,#139864,#139865);
#110785=AXIS2_PLACEMENT_3D('',#265060,#139867,#139868);
#110786=AXIS2_PLACEMENT_3D('',#265064,#139870,#139871);
#110787=AXIS2_PLACEMENT_3D('',#265066,#139873,#139874);
#110788=AXIS2_PLACEMENT_3D('',#265070,#139876,#139877);
#110789=AXIS2_PLACEMENT_3D('',#265072,#139879,#139880);
#110790=AXIS2_PLACEMENT_3D('',#265076,#139883,#139884);
#110791=AXIS2_PLACEMENT_3D('',#265079,#139886,#139887);
#110792=AXIS2_PLACEMENT_3D('',#265080,#139888,#139889);
#110793=AXIS2_PLACEMENT_3D('',#265084,#139892,#139893);
#110794=AXIS2_PLACEMENT_3D('',#265087,#139895,#139896);
#110795=AXIS2_PLACEMENT_3D('',#265088,#139897,#139898);
#110796=AXIS2_PLACEMENT_3D('',#265092,#139901,#139902);
#110797=AXIS2_PLACEMENT_3D('',#265095,#139904,#139905);
#110798=AXIS2_PLACEMENT_3D('',#265096,#139906,#139907);
#110799=AXIS2_PLACEMENT_3D('',#265098,#139909,#139910);
#110800=AXIS2_PLACEMENT_3D('',#265099,#139911,#139912);
#110801=AXIS2_PLACEMENT_3D('',#265100,#139913,#139914);
#110802=AXIS2_PLACEMENT_3D('',#265101,#139915,#139916);
#110803=AXIS2_PLACEMENT_3D('',#265102,#139917,#139918);
#110804=AXIS2_PLACEMENT_3D('',#265103,#139919,#139920);
#110805=AXIS2_PLACEMENT_3D('',#265104,#139921,#139922);
#110806=AXIS2_PLACEMENT_3D('',#265105,#139923,#139924);
#110807=AXIS2_PLACEMENT_3D('',#265106,#139925,#139926);
#110808=AXIS2_PLACEMENT_3D('',#265107,#139927,#139928);
#110809=AXIS2_PLACEMENT_3D('',#265108,#139929,#139930);
#110810=AXIS2_PLACEMENT_3D('',#265109,#139931,#139932);
#110811=AXIS2_PLACEMENT_3D('',#265110,#139933,#139934);
#110812=AXIS2_PLACEMENT_3D('',#265111,#139935,#139936);
#110813=AXIS2_PLACEMENT_3D('',#265112,#139937,#139938);
#110814=AXIS2_PLACEMENT_3D('',#265113,#139939,#139940);
#110815=AXIS2_PLACEMENT_3D('',#265114,#139941,#139942);
#110816=AXIS2_PLACEMENT_3D('',#265115,#139943,#139944);
#110817=AXIS2_PLACEMENT_3D('',#265120,#139946,#139947);
#110818=AXIS2_PLACEMENT_3D('',#265123,#139949,#139950);
#110819=AXIS2_PLACEMENT_3D('',#265124,#139951,#139952);
#110820=AXIS2_PLACEMENT_3D('',#265128,#139954,#139955);
#110821=AXIS2_PLACEMENT_3D('',#265133,#139958,#139959);
#110822=AXIS2_PLACEMENT_3D('',#265135,#139961,#139962);
#110823=AXIS2_PLACEMENT_3D('',#265136,#139963,#139964);
#110824=AXIS2_PLACEMENT_3D('',#265137,#139965,#139966);
#110825=AXIS2_PLACEMENT_3D('',#265138,#139967,#139968);
#110826=AXIS2_PLACEMENT_3D('',#265142,#139970,#139971);
#110827=AXIS2_PLACEMENT_3D('',#265144,#139973,#139974);
#110828=AXIS2_PLACEMENT_3D('',#265146,#139976,#139977);
#110829=AXIS2_PLACEMENT_3D('',#265148,#139979,#139980);
#110830=AXIS2_PLACEMENT_3D('',#265152,#139982,#139983);
#110831=AXIS2_PLACEMENT_3D('',#265154,#139985,#139986);
#110832=AXIS2_PLACEMENT_3D('',#265157,#139989,#139990);
#110833=AXIS2_PLACEMENT_3D('',#265158,#139991,#139992);
#110834=AXIS2_PLACEMENT_3D('',#265159,#139993,#139994);
#110835=AXIS2_PLACEMENT_3D('',#265862,#140001,#140002);
#110836=AXIS2_PLACEMENT_3D('',#265863,#140003,#140004);
#110837=AXIS2_PLACEMENT_3D('',#266566,#140011,#140012);
#110838=AXIS2_PLACEMENT_3D('',#266567,#140013,#140014);
#110839=AXIS2_PLACEMENT_3D('',#266568,#140015,#140016);
#110840=AXIS2_PLACEMENT_3D('',#266570,#140017,#140018);
#110841=AXIS2_PLACEMENT_3D('',#266573,#140020,#140021);
#110842=AXIS2_PLACEMENT_3D('',#266574,#140022,#140023);
#110843=AXIS2_PLACEMENT_3D('',#266577,#140025,#140026);
#110844=AXIS2_PLACEMENT_3D('',#266615,#140028,#140029);
#110845=AXIS2_PLACEMENT_3D('',#266652,#140030,#140031);
#110846=AXIS2_PLACEMENT_3D('',#266676,#140033,#140034);
#110847=AXIS2_PLACEMENT_3D('',#266731,#140035,#140036);
#110848=AXIS2_PLACEMENT_3D('',#266754,#140038,#140039);
#110849=AXIS2_PLACEMENT_3D('',#266810,#140040,#140041);
#110850=AXIS2_PLACEMENT_3D('',#266833,#140043,#140044);
#110851=AXIS2_PLACEMENT_3D('',#266889,#140045,#140046);
#110852=AXIS2_PLACEMENT_3D('',#266912,#140048,#140049);
#110853=AXIS2_PLACEMENT_3D('',#267004,#140050,#140051);
#110854=AXIS2_PLACEMENT_3D('',#267028,#140053,#140054);
#110855=AXIS2_PLACEMENT_3D('',#267119,#140055,#140056);
#110856=AXIS2_PLACEMENT_3D('',#267120,#140057,#140058);
#110857=AXIS2_PLACEMENT_3D('',#267125,#140062,#140063);
#110858=AXIS2_PLACEMENT_3D('',#267126,#140064,#140065);
#110859=AXIS2_PLACEMENT_3D('',#268099,#140066,#140067);
#110860=AXIS2_PLACEMENT_3D('',#268291,#140070,#140071);
#110861=AXIS2_PLACEMENT_3D('',#268616,#140072,#140073);
#110862=AXIS2_PLACEMENT_3D('',#271695,#140074,#140075);
#110863=AXIS2_PLACEMENT_3D('',#271887,#140078,#140079);
#110864=AXIS2_PLACEMENT_3D('',#272212,#140080,#140081);
#110865=AXIS2_PLACEMENT_3D('',#272375,#140082,#140083);
#110866=AXIS2_PLACEMENT_3D('',#272553,#140085,#140086);
#110867=AXIS2_PLACEMENT_3D('',#272716,#140087,#140088);
#110868=AXIS2_PLACEMENT_3D('',#272894,#140090,#140091);
#110869=AXIS2_PLACEMENT_3D('',#273057,#140092,#140093);
#110870=AXIS2_PLACEMENT_3D('',#273235,#140095,#140096);
#110871=AXIS2_PLACEMENT_3D('',#273398,#140097,#140098);
#110872=AXIS2_PLACEMENT_3D('',#273576,#140100,#140101);
#110873=AXIS2_PLACEMENT_3D('',#273739,#140102,#140103);
#110874=AXIS2_PLACEMENT_3D('',#273740,#140104,#140105);
#110875=AXIS2_PLACEMENT_3D('',#273741,#140106,#140107);
#110876=AXIS2_PLACEMENT_3D('',#273742,#140108,#140109);
#110877=AXIS2_PLACEMENT_3D('',#273751,#140114,#140115);
#110878=AXIS2_PLACEMENT_3D('',#273756,#140117,#140118);
#110879=AXIS2_PLACEMENT_3D('',#273763,#140122,#140123);
#110880=AXIS2_PLACEMENT_3D('',#273764,#140124,#140125);
#110881=AXIS2_PLACEMENT_3D('',#273778,#140133,#140134);
#110882=AXIS2_PLACEMENT_3D('',#273787,#140139,#140140);
#110883=AXIS2_PLACEMENT_3D('',#273801,#140148,#140149);
#110884=AXIS2_PLACEMENT_3D('',#273810,#140154,#140155);
#110885=AXIS2_PLACEMENT_3D('',#273815,#140157,#140158);
#110886=AXIS2_PLACEMENT_3D('',#273819,#140160,#140161);
#110887=AXIS2_PLACEMENT_3D('',#273823,#140163,#140164);
#110888=AXIS2_PLACEMENT_3D('',#273826,#140166,#140167);
#110889=AXIS2_PLACEMENT_3D('',#273831,#140169,#140170);
#110890=AXIS2_PLACEMENT_3D('',#273835,#140172,#140173);
#110891=AXIS2_PLACEMENT_3D('',#273839,#140175,#140176);
#110892=AXIS2_PLACEMENT_3D('',#273842,#140178,#140179);
#110893=AXIS2_PLACEMENT_3D('',#273843,#140180,#140181);
#110894=AXIS2_PLACEMENT_3D('',#273852,#140186,#140187);
#110895=AXIS2_PLACEMENT_3D('',#273861,#140192,#140193);
#110896=AXIS2_PLACEMENT_3D('',#273870,#140198,#140199);
#110897=AXIS2_PLACEMENT_3D('',#273879,#140204,#140205);
#110898=AXIS2_PLACEMENT_3D('',#273880,#140206,#140207);
#110899=AXIS2_PLACEMENT_3D('',#273881,#140208,#140209);
#110900=AXIS2_PLACEMENT_3D('',#273882,#140210,#140211);
#110901=AXIS2_PLACEMENT_3D('',#273883,#140212,#140213);
#110902=AXIS2_PLACEMENT_3D('',#273884,#140214,#140215);
#110903=AXIS2_PLACEMENT_3D('',#273885,#140216,#140217);
#110904=AXIS2_PLACEMENT_3D('',#273886,#140218,#140219);
#110905=AXIS2_PLACEMENT_3D('',#273887,#140220,#140221);
#110906=AXIS2_PLACEMENT_3D('',#273888,#140222,#140223);
#110907=AXIS2_PLACEMENT_3D('',#273889,#140224,#140225);
#110908=AXIS2_PLACEMENT_3D('',#273890,#140226,#140227);
#110909=AXIS2_PLACEMENT_3D('',#273900,#140228,#140229);
#110910=AXIS2_PLACEMENT_3D('',#273901,#140230,#140231);
#110911=AXIS2_PLACEMENT_3D('',#273902,#140232,#140233);
#110912=AXIS2_PLACEMENT_3D('',#273903,#140234,#140235);
#110913=AXIS2_PLACEMENT_3D('',#273904,#140236,#140237);
#110914=AXIS2_PLACEMENT_3D('',#273905,#140238,#140239);
#110915=AXIS2_PLACEMENT_3D('',#273915,#140240,#140241);
#110916=AXIS2_PLACEMENT_3D('',#273925,#140242,#140243);
#110917=AXIS2_PLACEMENT_3D('',#273926,#140244,#140245);
#110918=AXIS2_PLACEMENT_3D('',#273927,#140246,#140247);
#110919=AXIS2_PLACEMENT_3D('',#273928,#140248,#140249);
#110920=AXIS2_PLACEMENT_3D('',#273929,#140250,#140251);
#110921=AXIS2_PLACEMENT_3D('',#273939,#140252,#140253);
#110922=AXIS2_PLACEMENT_3D('',#273940,#140254,#140255);
#110923=AXIS2_PLACEMENT_3D('',#273942,#140256,#140257);
#110924=AXIS2_PLACEMENT_3D('',#273953,#140258,#140259);
#110925=AXIS2_PLACEMENT_3D('',#273954,#140260,#140261);
#110926=AXIS2_PLACEMENT_3D('',#273966,#140262,#140263);
#110927=AXIS2_PLACEMENT_3D('',#273967,#140264,#140265);
#110928=AXIS2_PLACEMENT_3D('',#273968,#140266,#140267);
#110929=AXIS2_PLACEMENT_3D('',#273980,#140268,#140269);
#110930=AXIS2_PLACEMENT_3D('',#273981,#140270,#140271);
#110931=AXIS2_PLACEMENT_3D('',#273982,#140272,#140273);
#110932=AXIS2_PLACEMENT_3D('',#273984,#140274,#140275);
#110933=AXIS2_PLACEMENT_3D('',#273995,#140276,#140277);
#110934=AXIS2_PLACEMENT_3D('',#274001,#140281,#140282);
#110935=AXIS2_PLACEMENT_3D('',#274013,#140289,#140290);
#110936=AXIS2_PLACEMENT_3D('',#274019,#140294,#140295);
#110937=AXIS2_PLACEMENT_3D('',#274028,#140301,#140302);
#110938=AXIS2_PLACEMENT_3D('',#274032,#140304,#140305);
#110939=AXIS2_PLACEMENT_3D('',#274033,#140306,#140307);
#110940=AXIS2_PLACEMENT_3D('',#274034,#140308,#140309);
#110941=AXIS2_PLACEMENT_3D('',#274035,#140310,#140311);
#110942=AXIS2_PLACEMENT_3D('',#274036,#140312,#140313);
#110943=AXIS2_PLACEMENT_3D('',#274037,#140314,#140315);
#110944=AXIS2_PLACEMENT_3D('',#274038,#140316,#140317);
#110945=AXIS2_PLACEMENT_3D('',#274039,#140318,#140319);
#110946=AXIS2_PLACEMENT_3D('',#274040,#140320,#140321);
#110947=AXIS2_PLACEMENT_3D('',#274041,#140322,#140323);
#110948=AXIS2_PLACEMENT_3D('',#274042,#140324,#140325);
#110949=AXIS2_PLACEMENT_3D('',#274043,#140326,#140327);
#110950=AXIS2_PLACEMENT_3D('',#274044,#140328,#140329);
#110951=AXIS2_PLACEMENT_3D('',#274045,#140330,#140331);
#110952=AXIS2_PLACEMENT_3D('',#274046,#140332,#140333);
#110953=AXIS2_PLACEMENT_3D('',#274047,#140334,#140335);
#110954=AXIS2_PLACEMENT_3D('',#274048,#140336,#140337);
#110955=AXIS2_PLACEMENT_3D('',#274049,#140338,#140339);
#110956=AXIS2_PLACEMENT_3D('',#274050,#140340,#140341);
#110957=AXIS2_PLACEMENT_3D('',#274051,#140342,#140343);
#110958=AXIS2_PLACEMENT_3D('',#274052,#140344,#140345);
#110959=AXIS2_PLACEMENT_3D('',#274065,#140346,#140347);
#110960=AXIS2_PLACEMENT_3D('',#274066,#140348,#140349);
#110961=AXIS2_PLACEMENT_3D('',#274067,#140350,#140351);
#110962=AXIS2_PLACEMENT_3D('',#274068,#140352,#140353);
#110963=AXIS2_PLACEMENT_3D('',#274069,#140354,#140355);
#110964=AXIS2_PLACEMENT_3D('',#274070,#140356,#140357);
#110965=AXIS2_PLACEMENT_3D('',#274071,#140358,#140359);
#110966=AXIS2_PLACEMENT_3D('',#274084,#140360,#140361);
#110967=AXIS2_PLACEMENT_3D('',#274097,#140362,#140363);
#110968=AXIS2_PLACEMENT_3D('',#274098,#140364,#140365);
#110969=AXIS2_PLACEMENT_3D('',#274099,#140366,#140367);
#110970=AXIS2_PLACEMENT_3D('',#274100,#140368,#140369);
#110971=AXIS2_PLACEMENT_3D('',#274101,#140370,#140371);
#110972=AXIS2_PLACEMENT_3D('',#274102,#140372,#140373);
#110973=AXIS2_PLACEMENT_3D('',#274103,#140374,#140375);
#110974=AXIS2_PLACEMENT_3D('',#274116,#140376,#140377);
#110975=AXIS2_PLACEMENT_3D('',#274117,#140378,#140379);
#110976=AXIS2_PLACEMENT_3D('',#274118,#140380,#140381);
#110977=AXIS2_PLACEMENT_3D('',#274127,#140386,#140387);
#110978=AXIS2_PLACEMENT_3D('',#274133,#140391,#140392);
#110979=AXIS2_PLACEMENT_3D('',#274137,#140395,#140396);
#110980=AXIS2_PLACEMENT_3D('',#274141,#140399,#140400);
#110981=AXIS2_PLACEMENT_3D('',#274143,#140402,#140403);
#110982=AXIS2_PLACEMENT_3D('',#274144,#140404,#140405);
#110983=AXIS2_PLACEMENT_3D('',#274146,#140407,#140408);
#110984=AXIS2_PLACEMENT_3D('',#274147,#140409,#140410);
#110985=AXIS2_PLACEMENT_3D('',#274149,#140412,#140413);
#110986=AXIS2_PLACEMENT_3D('',#274150,#140414,#140415);
#110987=AXIS2_PLACEMENT_3D('',#274151,#140416,#140417);
#110988=AXIS2_PLACEMENT_3D('',#274154,#140418,#140419);
#110989=AXIS2_PLACEMENT_3D('',#274158,#140421,#140422);
#110990=AXIS2_PLACEMENT_3D('',#274160,#140424,#140425);
#110991=AXIS2_PLACEMENT_3D('',#274163,#140426,#140427);
#110992=AXIS2_PLACEMENT_3D('',#274167,#140429,#140430);
#110993=AXIS2_PLACEMENT_3D('',#274171,#140432,#140433);
#110994=AXIS2_PLACEMENT_3D('',#274175,#140435,#140436);
#110995=AXIS2_PLACEMENT_3D('',#274179,#140438,#140439);
#110996=AXIS2_PLACEMENT_3D('',#274183,#140441,#140442);
#110997=AXIS2_PLACEMENT_3D('',#274187,#140444,#140445);
#110998=AXIS2_PLACEMENT_3D('',#274190,#140448,#140449);
#110999=AXIS2_PLACEMENT_3D('',#274194,#140452,#140453);
#111000=AXIS2_PLACEMENT_3D('',#274198,#140456,#140457);
#111001=AXIS2_PLACEMENT_3D('',#274201,#140459,#140460);
#111002=AXIS2_PLACEMENT_3D('',#274202,#140461,#140462);
#111003=AXIS2_PLACEMENT_3D('',#274206,#140465,#140466);
#111004=AXIS2_PLACEMENT_3D('',#274209,#140468,#140469);
#111005=AXIS2_PLACEMENT_3D('',#274210,#140470,#140471);
#111006=AXIS2_PLACEMENT_3D('',#274214,#140474,#140475);
#111007=AXIS2_PLACEMENT_3D('',#274217,#140477,#140478);
#111008=AXIS2_PLACEMENT_3D('',#274218,#140479,#140480);
#111009=AXIS2_PLACEMENT_3D('',#274222,#140483,#140484);
#111010=AXIS2_PLACEMENT_3D('',#274225,#140486,#140487);
#111011=AXIS2_PLACEMENT_3D('',#274226,#140488,#140489);
#111012=AXIS2_PLACEMENT_3D('',#274230,#140492,#140493);
#111013=AXIS2_PLACEMENT_3D('',#274233,#140495,#140496);
#111014=AXIS2_PLACEMENT_3D('',#274234,#140497,#140498);
#111015=AXIS2_PLACEMENT_3D('',#274238,#140501,#140502);
#111016=AXIS2_PLACEMENT_3D('',#274241,#140504,#140505);
#111017=AXIS2_PLACEMENT_3D('',#274242,#140506,#140507);
#111018=AXIS2_PLACEMENT_3D('',#274246,#140510,#140511);
#111019=AXIS2_PLACEMENT_3D('',#274247,#140512,#140513);
#111020=AXIS2_PLACEMENT_3D('',#274248,#140514,#140515);
#111021=AXIS2_PLACEMENT_3D('',#274249,#140516,#140517);
#111022=AXIS2_PLACEMENT_3D('',#274252,#140518,#140519);
#111023=AXIS2_PLACEMENT_3D('',#274256,#140521,#140522);
#111024=AXIS2_PLACEMENT_3D('',#274260,#140524,#140525);
#111025=AXIS2_PLACEMENT_3D('',#274264,#140527,#140528);
#111026=AXIS2_PLACEMENT_3D('',#274266,#140530,#140531);
#111027=AXIS2_PLACEMENT_3D('',#274272,#140535,#140536);
#111028=AXIS2_PLACEMENT_3D('',#274275,#140538,#140539);
#111029=AXIS2_PLACEMENT_3D('',#274276,#140540,#140541);
#111030=AXIS2_PLACEMENT_3D('',#274280,#140544,#140545);
#111031=AXIS2_PLACEMENT_3D('',#274283,#140547,#140548);
#111032=AXIS2_PLACEMENT_3D('',#274284,#140549,#140550);
#111033=AXIS2_PLACEMENT_3D('',#274288,#140553,#140554);
#111034=AXIS2_PLACEMENT_3D('',#274291,#140556,#140557);
#111035=AXIS2_PLACEMENT_3D('',#274292,#140558,#140559);
#111036=AXIS2_PLACEMENT_3D('',#274296,#140562,#140563);
#111037=AXIS2_PLACEMENT_3D('',#274297,#140564,#140565);
#111038=AXIS2_PLACEMENT_3D('',#274298,#140566,#140567);
#111039=AXIS2_PLACEMENT_3D('',#274299,#140568,#140569);
#111040=AXIS2_PLACEMENT_3D('',#274302,#140570,#140571);
#111041=AXIS2_PLACEMENT_3D('',#274306,#140573,#140574);
#111042=AXIS2_PLACEMENT_3D('',#274310,#140576,#140577);
#111043=AXIS2_PLACEMENT_3D('',#274314,#140579,#140580);
#111044=AXIS2_PLACEMENT_3D('',#274322,#140584,#140585);
#111045=AXIS2_PLACEMENT_3D('',#274326,#140587,#140588);
#111046=AXIS2_PLACEMENT_3D('',#274330,#140590,#140591);
#111047=AXIS2_PLACEMENT_3D('',#274334,#140593,#140594);
#111048=AXIS2_PLACEMENT_3D('',#274338,#140596,#140597);
#111049=AXIS2_PLACEMENT_3D('',#274342,#140599,#140600);
#111050=AXIS2_PLACEMENT_3D('',#274350,#140604,#140605);
#111051=AXIS2_PLACEMENT_3D('',#274354,#140607,#140608);
#111052=AXIS2_PLACEMENT_3D('',#274358,#140610,#140611);
#111053=AXIS2_PLACEMENT_3D('',#274362,#140613,#140614);
#111054=AXIS2_PLACEMENT_3D('',#274366,#140616,#140617);
#111055=AXIS2_PLACEMENT_3D('',#274370,#140619,#140620);
#111056=AXIS2_PLACEMENT_3D('',#274378,#140624,#140625);
#111057=AXIS2_PLACEMENT_3D('',#274382,#140627,#140628);
#111058=AXIS2_PLACEMENT_3D('',#274386,#140630,#140631);
#111059=AXIS2_PLACEMENT_3D('',#274390,#140633,#140634);
#111060=AXIS2_PLACEMENT_3D('',#274394,#140636,#140637);
#111061=AXIS2_PLACEMENT_3D('',#274398,#140639,#140640);
#111062=AXIS2_PLACEMENT_3D('',#274406,#140644,#140645);
#111063=AXIS2_PLACEMENT_3D('',#274410,#140647,#140648);
#111064=AXIS2_PLACEMENT_3D('',#274412,#140650,#140651);
#111065=AXIS2_PLACEMENT_3D('',#274415,#140652,#140653);
#111066=AXIS2_PLACEMENT_3D('',#274419,#140655,#140656);
#111067=AXIS2_PLACEMENT_3D('',#274423,#140658,#140659);
#111068=AXIS2_PLACEMENT_3D('',#274427,#140661,#140662);
#111069=AXIS2_PLACEMENT_3D('',#274435,#140666,#140667);
#111070=AXIS2_PLACEMENT_3D('',#274439,#140669,#140670);
#111071=AXIS2_PLACEMENT_3D('',#274443,#140672,#140673);
#111072=AXIS2_PLACEMENT_3D('',#274447,#140675,#140676);
#111073=AXIS2_PLACEMENT_3D('',#274451,#140678,#140679);
#111074=AXIS2_PLACEMENT_3D('',#274455,#140681,#140682);
#111075=AXIS2_PLACEMENT_3D('',#274463,#140686,#140687);
#111076=AXIS2_PLACEMENT_3D('',#274467,#140689,#140690);
#111077=AXIS2_PLACEMENT_3D('',#274471,#140692,#140693);
#111078=AXIS2_PLACEMENT_3D('',#274475,#140695,#140696);
#111079=AXIS2_PLACEMENT_3D('',#274479,#140698,#140699);
#111080=AXIS2_PLACEMENT_3D('',#274483,#140701,#140702);
#111081=AXIS2_PLACEMENT_3D('',#274491,#140706,#140707);
#111082=AXIS2_PLACEMENT_3D('',#274495,#140709,#140710);
#111083=AXIS2_PLACEMENT_3D('',#274499,#140712,#140713);
#111084=AXIS2_PLACEMENT_3D('',#274503,#140715,#140716);
#111085=AXIS2_PLACEMENT_3D('',#274507,#140718,#140719);
#111086=AXIS2_PLACEMENT_3D('',#274511,#140721,#140722);
#111087=AXIS2_PLACEMENT_3D('',#274519,#140726,#140727);
#111088=AXIS2_PLACEMENT_3D('',#274523,#140729,#140730);
#111089=AXIS2_PLACEMENT_3D('',#274525,#140732,#140733);
#111090=AXIS2_PLACEMENT_3D('',#274528,#140736,#140737);
#111091=AXIS2_PLACEMENT_3D('',#274530,#140739,#140740);
#111092=AXIS2_PLACEMENT_3D('',#274532,#140742,#140743);
#111093=AXIS2_PLACEMENT_3D('',#274534,#140745,#140746);
#111094=AXIS2_PLACEMENT_3D('',#274536,#140748,#140749);
#111095=AXIS2_PLACEMENT_3D('',#274538,#140751,#140752);
#111096=AXIS2_PLACEMENT_3D('',#274540,#140754,#140755);
#111097=AXIS2_PLACEMENT_3D('',#274542,#140757,#140758);
#111098=AXIS2_PLACEMENT_3D('',#274544,#140760,#140761);
#111099=AXIS2_PLACEMENT_3D('',#274546,#140763,#140764);
#111100=AXIS2_PLACEMENT_3D('',#274548,#140766,#140767);
#111101=AXIS2_PLACEMENT_3D('',#274550,#140769,#140770);
#111102=AXIS2_PLACEMENT_3D('',#274552,#140772,#140773);
#111103=AXIS2_PLACEMENT_3D('',#274554,#140775,#140776);
#111104=AXIS2_PLACEMENT_3D('',#274556,#140778,#140779);
#111105=AXIS2_PLACEMENT_3D('',#274558,#140781,#140782);
#111106=AXIS2_PLACEMENT_3D('',#274560,#140784,#140785);
#111107=AXIS2_PLACEMENT_3D('',#274562,#140787,#140788);
#111108=AXIS2_PLACEMENT_3D('',#274564,#140790,#140791);
#111109=AXIS2_PLACEMENT_3D('',#274566,#140793,#140794);
#111110=AXIS2_PLACEMENT_3D('',#274568,#140796,#140797);
#111111=AXIS2_PLACEMENT_3D('',#274570,#140799,#140800);
#111112=AXIS2_PLACEMENT_3D('',#274572,#140802,#140803);
#111113=AXIS2_PLACEMENT_3D('',#274574,#140805,#140806);
#111114=AXIS2_PLACEMENT_3D('',#274576,#140808,#140809);
#111115=AXIS2_PLACEMENT_3D('',#274578,#140811,#140812);
#111116=AXIS2_PLACEMENT_3D('',#274580,#140814,#140815);
#111117=AXIS2_PLACEMENT_3D('',#274582,#140817,#140818);
#111118=AXIS2_PLACEMENT_3D('',#274584,#140820,#140821);
#111119=AXIS2_PLACEMENT_3D('',#274586,#140823,#140824);
#111120=AXIS2_PLACEMENT_3D('',#274588,#140826,#140827);
#111121=AXIS2_PLACEMENT_3D('',#274590,#140829,#140830);
#111122=AXIS2_PLACEMENT_3D('',#274592,#140832,#140833);
#111123=AXIS2_PLACEMENT_3D('',#274594,#140835,#140836);
#111124=AXIS2_PLACEMENT_3D('',#274596,#140838,#140839);
#111125=AXIS2_PLACEMENT_3D('',#274598,#140841,#140842);
#111126=AXIS2_PLACEMENT_3D('',#274600,#140844,#140845);
#111127=AXIS2_PLACEMENT_3D('',#274602,#140847,#140848);
#111128=AXIS2_PLACEMENT_3D('',#274604,#140850,#140851);
#111129=AXIS2_PLACEMENT_3D('',#274606,#140853,#140854);
#111130=AXIS2_PLACEMENT_3D('',#274608,#140856,#140857);
#111131=AXIS2_PLACEMENT_3D('',#274610,#140859,#140860);
#111132=AXIS2_PLACEMENT_3D('',#274612,#140862,#140863);
#111133=AXIS2_PLACEMENT_3D('',#274614,#140865,#140866);
#111134=AXIS2_PLACEMENT_3D('',#274616,#140868,#140869);
#111135=AXIS2_PLACEMENT_3D('',#274618,#140871,#140872);
#111136=AXIS2_PLACEMENT_3D('',#274620,#140874,#140875);
#111137=AXIS2_PLACEMENT_3D('',#274622,#140877,#140878);
#111138=AXIS2_PLACEMENT_3D('',#274624,#140880,#140881);
#111139=AXIS2_PLACEMENT_3D('',#274626,#140883,#140884);
#111140=AXIS2_PLACEMENT_3D('',#274628,#140886,#140887);
#111141=AXIS2_PLACEMENT_3D('',#274630,#140889,#140890);
#111142=AXIS2_PLACEMENT_3D('',#274632,#140892,#140893);
#111143=AXIS2_PLACEMENT_3D('',#274634,#140895,#140896);
#111144=AXIS2_PLACEMENT_3D('',#274636,#140898,#140899);
#111145=AXIS2_PLACEMENT_3D('',#274637,#140900,#140901);
#111146=AXIS2_PLACEMENT_3D('',#274640,#140902,#140903);
#111147=AXIS2_PLACEMENT_3D('',#274644,#140905,#140906);
#111148=AXIS2_PLACEMENT_3D('',#274646,#140908,#140909);
#111149=AXIS2_PLACEMENT_3D('',#274649,#140910,#140911);
#111150=AXIS2_PLACEMENT_3D('',#274653,#140913,#140914);
#111151=AXIS2_PLACEMENT_3D('',#274657,#140916,#140917);
#111152=AXIS2_PLACEMENT_3D('',#274662,#140920,#140921);
#111153=AXIS2_PLACEMENT_3D('',#274666,#140923,#140924);
#111154=AXIS2_PLACEMENT_3D('',#274670,#140926,#140927);
#111155=AXIS2_PLACEMENT_3D('',#274674,#140929,#140930);
#111156=AXIS2_PLACEMENT_3D('',#274676,#140932,#140933);
#111157=AXIS2_PLACEMENT_3D('',#274682,#140937,#140938);
#111158=AXIS2_PLACEMENT_3D('',#274685,#140940,#140941);
#111159=AXIS2_PLACEMENT_3D('',#274686,#140942,#140943);
#111160=AXIS2_PLACEMENT_3D('',#274690,#140946,#140947);
#111161=AXIS2_PLACEMENT_3D('',#274693,#140949,#140950);
#111162=AXIS2_PLACEMENT_3D('',#274694,#140951,#140952);
#111163=AXIS2_PLACEMENT_3D('',#274698,#140955,#140956);
#111164=AXIS2_PLACEMENT_3D('',#274701,#140958,#140959);
#111165=AXIS2_PLACEMENT_3D('',#274702,#140960,#140961);
#111166=AXIS2_PLACEMENT_3D('',#274706,#140964,#140965);
#111167=AXIS2_PLACEMENT_3D('',#274709,#140967,#140968);
#111168=AXIS2_PLACEMENT_3D('',#274710,#140969,#140970);
#111169=AXIS2_PLACEMENT_3D('',#274712,#140972,#140973);
#111170=AXIS2_PLACEMENT_3D('',#274716,#140976,#140977);
#111171=AXIS2_PLACEMENT_3D('',#274719,#140979,#140980);
#111172=AXIS2_PLACEMENT_3D('',#274720,#140981,#140982);
#111173=AXIS2_PLACEMENT_3D('',#274724,#140985,#140986);
#111174=AXIS2_PLACEMENT_3D('',#274727,#140988,#140989);
#111175=AXIS2_PLACEMENT_3D('',#274728,#140990,#140991);
#111176=AXIS2_PLACEMENT_3D('',#274732,#140994,#140995);
#111177=AXIS2_PLACEMENT_3D('',#274733,#140996,#140997);
#111178=AXIS2_PLACEMENT_3D('',#274734,#140998,#140999);
#111179=AXIS2_PLACEMENT_3D('',#274735,#141000,#141001);
#111180=AXIS2_PLACEMENT_3D('',#274738,#141002,#141003);
#111181=AXIS2_PLACEMENT_3D('',#274742,#141005,#141006);
#111182=AXIS2_PLACEMENT_3D('',#274746,#141008,#141009);
#111183=AXIS2_PLACEMENT_3D('',#274750,#141011,#141012);
#111184=AXIS2_PLACEMENT_3D('',#274752,#141014,#141015);
#111185=AXIS2_PLACEMENT_3D('',#274758,#141019,#141020);
#111186=AXIS2_PLACEMENT_3D('',#274761,#141022,#141023);
#111187=AXIS2_PLACEMENT_3D('',#274762,#141024,#141025);
#111188=AXIS2_PLACEMENT_3D('',#274766,#141028,#141029);
#111189=AXIS2_PLACEMENT_3D('',#274769,#141031,#141032);
#111190=AXIS2_PLACEMENT_3D('',#274770,#141033,#141034);
#111191=AXIS2_PLACEMENT_3D('',#274774,#141037,#141038);
#111192=AXIS2_PLACEMENT_3D('',#274777,#141040,#141041);
#111193=AXIS2_PLACEMENT_3D('',#274778,#141042,#141043);
#111194=AXIS2_PLACEMENT_3D('',#274782,#141046,#141047);
#111195=AXIS2_PLACEMENT_3D('',#274783,#141048,#141049);
#111196=AXIS2_PLACEMENT_3D('',#274784,#141050,#141051);
#111197=AXIS2_PLACEMENT_3D('',#274785,#141052,#141053);
#111198=AXIS2_PLACEMENT_3D('',#274788,#141054,#141055);
#111199=AXIS2_PLACEMENT_3D('',#274792,#141057,#141058);
#111200=AXIS2_PLACEMENT_3D('',#274794,#141060,#141061);
#111201=AXIS2_PLACEMENT_3D('',#274797,#141062,#141063);
#111202=AXIS2_PLACEMENT_3D('',#274802,#141066,#141067);
#111203=AXIS2_PLACEMENT_3D('',#274806,#141069,#141070);
#111204=AXIS2_PLACEMENT_3D('',#274810,#141072,#141073);
#111205=AXIS2_PLACEMENT_3D('',#274814,#141075,#141076);
#111206=AXIS2_PLACEMENT_3D('',#274818,#141078,#141079);
#111207=AXIS2_PLACEMENT_3D('',#274822,#141081,#141082);
#111208=AXIS2_PLACEMENT_3D('',#274824,#141084,#141085);
#111209=AXIS2_PLACEMENT_3D('',#274830,#141089,#141090);
#111210=AXIS2_PLACEMENT_3D('',#274833,#141092,#141093);
#111211=AXIS2_PLACEMENT_3D('',#274834,#141094,#141095);
#111212=AXIS2_PLACEMENT_3D('',#274838,#141098,#141099);
#111213=AXIS2_PLACEMENT_3D('',#274841,#141101,#141102);
#111214=AXIS2_PLACEMENT_3D('',#274842,#141103,#141104);
#111215=AXIS2_PLACEMENT_3D('',#274846,#141107,#141108);
#111216=AXIS2_PLACEMENT_3D('',#274849,#141110,#141111);
#111217=AXIS2_PLACEMENT_3D('',#274850,#141112,#141113);
#111218=AXIS2_PLACEMENT_3D('',#274854,#141116,#141117);
#111219=AXIS2_PLACEMENT_3D('',#274857,#141119,#141120);
#111220=AXIS2_PLACEMENT_3D('',#274858,#141121,#141122);
#111221=AXIS2_PLACEMENT_3D('',#274862,#141125,#141126);
#111222=AXIS2_PLACEMENT_3D('',#274865,#141128,#141129);
#111223=AXIS2_PLACEMENT_3D('',#274866,#141130,#141131);
#111224=AXIS2_PLACEMENT_3D('',#274870,#141134,#141135);
#111225=AXIS2_PLACEMENT_3D('',#274873,#141137,#141138);
#111226=AXIS2_PLACEMENT_3D('',#274874,#141139,#141140);
#111227=AXIS2_PLACEMENT_3D('',#274876,#141142,#141143);
#111228=AXIS2_PLACEMENT_3D('',#274880,#141146,#141147);
#111229=AXIS2_PLACEMENT_3D('',#274881,#141148,#141149);
#111230=AXIS2_PLACEMENT_3D('',#274882,#141150,#141151);
#111231=AXIS2_PLACEMENT_3D('',#274883,#141152,#141153);
#111232=AXIS2_PLACEMENT_3D('',#274886,#141154,#141155);
#111233=AXIS2_PLACEMENT_3D('',#274890,#141157,#141158);
#111234=AXIS2_PLACEMENT_3D('',#274894,#141160,#141161);
#111235=AXIS2_PLACEMENT_3D('',#274898,#141163,#141164);
#111236=AXIS2_PLACEMENT_3D('',#274900,#141166,#141167);
#111237=AXIS2_PLACEMENT_3D('',#274906,#141171,#141172);
#111238=AXIS2_PLACEMENT_3D('',#274909,#141174,#141175);
#111239=AXIS2_PLACEMENT_3D('',#274910,#141176,#141177);
#111240=AXIS2_PLACEMENT_3D('',#274914,#141180,#141181);
#111241=AXIS2_PLACEMENT_3D('',#274917,#141183,#141184);
#111242=AXIS2_PLACEMENT_3D('',#274918,#141185,#141186);
#111243=AXIS2_PLACEMENT_3D('',#274922,#141189,#141190);
#111244=AXIS2_PLACEMENT_3D('',#274925,#141192,#141193);
#111245=AXIS2_PLACEMENT_3D('',#274926,#141194,#141195);
#111246=AXIS2_PLACEMENT_3D('',#274930,#141198,#141199);
#111247=AXIS2_PLACEMENT_3D('',#274931,#141200,#141201);
#111248=AXIS2_PLACEMENT_3D('',#274932,#141202,#141203);
#111249=AXIS2_PLACEMENT_3D('',#274933,#141204,#141205);
#111250=AXIS2_PLACEMENT_3D('',#274936,#141206,#141207);
#111251=AXIS2_PLACEMENT_3D('',#274940,#141209,#141210);
#111252=AXIS2_PLACEMENT_3D('',#274942,#141212,#141213);
#111253=AXIS2_PLACEMENT_3D('',#274945,#141214,#141215);
#111254=AXIS2_PLACEMENT_3D('',#274950,#141218,#141219);
#111255=AXIS2_PLACEMENT_3D('',#274954,#141221,#141222);
#111256=AXIS2_PLACEMENT_3D('',#274958,#141224,#141225);
#111257=AXIS2_PLACEMENT_3D('',#274962,#141227,#141228);
#111258=AXIS2_PLACEMENT_3D('',#274966,#141230,#141231);
#111259=AXIS2_PLACEMENT_3D('',#274970,#141233,#141234);
#111260=AXIS2_PLACEMENT_3D('',#274972,#141236,#141237);
#111261=AXIS2_PLACEMENT_3D('',#274978,#141241,#141242);
#111262=AXIS2_PLACEMENT_3D('',#274981,#141244,#141245);
#111263=AXIS2_PLACEMENT_3D('',#274982,#141246,#141247);
#111264=AXIS2_PLACEMENT_3D('',#274986,#141250,#141251);
#111265=AXIS2_PLACEMENT_3D('',#274989,#141253,#141254);
#111266=AXIS2_PLACEMENT_3D('',#274990,#141255,#141256);
#111267=AXIS2_PLACEMENT_3D('',#274994,#141259,#141260);
#111268=AXIS2_PLACEMENT_3D('',#274997,#141262,#141263);
#111269=AXIS2_PLACEMENT_3D('',#274998,#141264,#141265);
#111270=AXIS2_PLACEMENT_3D('',#275002,#141268,#141269);
#111271=AXIS2_PLACEMENT_3D('',#275005,#141271,#141272);
#111272=AXIS2_PLACEMENT_3D('',#275006,#141273,#141274);
#111273=AXIS2_PLACEMENT_3D('',#275010,#141277,#141278);
#111274=AXIS2_PLACEMENT_3D('',#275013,#141280,#141281);
#111275=AXIS2_PLACEMENT_3D('',#275014,#141282,#141283);
#111276=AXIS2_PLACEMENT_3D('',#275018,#141286,#141287);
#111277=AXIS2_PLACEMENT_3D('',#275021,#141289,#141290);
#111278=AXIS2_PLACEMENT_3D('',#275022,#141291,#141292);
#111279=AXIS2_PLACEMENT_3D('',#275024,#141294,#141295);
#111280=AXIS2_PLACEMENT_3D('',#275028,#141298,#141299);
#111281=AXIS2_PLACEMENT_3D('',#275029,#141300,#141301);
#111282=AXIS2_PLACEMENT_3D('',#275030,#141302,#141303);
#111283=AXIS2_PLACEMENT_3D('',#275031,#141304,#141305);
#111284=AXIS2_PLACEMENT_3D('',#275034,#141306,#141307);
#111285=AXIS2_PLACEMENT_3D('',#275038,#141309,#141310);
#111286=AXIS2_PLACEMENT_3D('',#275042,#141312,#141313);
#111287=AXIS2_PLACEMENT_3D('',#275046,#141315,#141316);
#111288=AXIS2_PLACEMENT_3D('',#275048,#141318,#141319);
#111289=AXIS2_PLACEMENT_3D('',#275054,#141323,#141324);
#111290=AXIS2_PLACEMENT_3D('',#275057,#141326,#141327);
#111291=AXIS2_PLACEMENT_3D('',#275058,#141328,#141329);
#111292=AXIS2_PLACEMENT_3D('',#275062,#141332,#141333);
#111293=AXIS2_PLACEMENT_3D('',#275065,#141335,#141336);
#111294=AXIS2_PLACEMENT_3D('',#275066,#141337,#141338);
#111295=AXIS2_PLACEMENT_3D('',#275070,#141341,#141342);
#111296=AXIS2_PLACEMENT_3D('',#275073,#141344,#141345);
#111297=AXIS2_PLACEMENT_3D('',#275074,#141346,#141347);
#111298=AXIS2_PLACEMENT_3D('',#275078,#141350,#141351);
#111299=AXIS2_PLACEMENT_3D('',#275079,#141352,#141353);
#111300=AXIS2_PLACEMENT_3D('',#275080,#141354,#141355);
#111301=AXIS2_PLACEMENT_3D('',#275081,#141356,#141357);
#111302=AXIS2_PLACEMENT_3D('',#275090,#141362,#141363);
#111303=AXIS2_PLACEMENT_3D('',#275099,#141368,#141369);
#111304=AXIS2_PLACEMENT_3D('',#275108,#141374,#141375);
#111305=AXIS2_PLACEMENT_3D('',#275114,#141379,#141380);
#111306=AXIS2_PLACEMENT_3D('',#275120,#141384,#141385);
#111307=AXIS2_PLACEMENT_3D('',#275122,#141386,#141387);
#111308=AXIS2_PLACEMENT_3D('',#275124,#141388,#141389);
#111309=AXIS2_PLACEMENT_3D('',#275126,#141391,#141392);
#111310=AXIS2_PLACEMENT_3D('',#275132,#141396,#141397);
#111311=AXIS2_PLACEMENT_3D('',#275134,#141398,#141399);
#111312=AXIS2_PLACEMENT_3D('',#275136,#141400,#141401);
#111313=AXIS2_PLACEMENT_3D('',#275138,#141403,#141404);
#111314=AXIS2_PLACEMENT_3D('',#275144,#141408,#141409);
#111315=AXIS2_PLACEMENT_3D('',#275146,#141410,#141411);
#111316=AXIS2_PLACEMENT_3D('',#275148,#141412,#141413);
#111317=AXIS2_PLACEMENT_3D('',#275150,#141415,#141416);
#111318=AXIS2_PLACEMENT_3D('',#275156,#141420,#141421);
#111319=AXIS2_PLACEMENT_3D('',#275158,#141422,#141423);
#111320=AXIS2_PLACEMENT_3D('',#275160,#141424,#141425);
#111321=AXIS2_PLACEMENT_3D('',#275162,#141427,#141428);
#111322=AXIS2_PLACEMENT_3D('',#275168,#141432,#141433);
#111323=AXIS2_PLACEMENT_3D('',#275174,#141437,#141438);
#111324=AXIS2_PLACEMENT_3D('',#275180,#141442,#141443);
#111325=AXIS2_PLACEMENT_3D('',#275186,#141447,#141448);
#111326=AXIS2_PLACEMENT_3D('',#275195,#141453,#141454);
#111327=AXIS2_PLACEMENT_3D('',#275201,#141458,#141459);
#111328=AXIS2_PLACEMENT_3D('',#275207,#141463,#141464);
#111329=AXIS2_PLACEMENT_3D('',#275213,#141468,#141469);
#111330=AXIS2_PLACEMENT_3D('',#275215,#141470,#141471);
#111331=AXIS2_PLACEMENT_3D('',#275217,#141472,#141473);
#111332=AXIS2_PLACEMENT_3D('',#275219,#141475,#141476);
#111333=AXIS2_PLACEMENT_3D('',#275225,#141480,#141481);
#111334=AXIS2_PLACEMENT_3D('',#275227,#141482,#141483);
#111335=AXIS2_PLACEMENT_3D('',#275229,#141484,#141485);
#111336=AXIS2_PLACEMENT_3D('',#275231,#141487,#141488);
#111337=AXIS2_PLACEMENT_3D('',#275237,#141492,#141493);
#111338=AXIS2_PLACEMENT_3D('',#275239,#141494,#141495);
#111339=AXIS2_PLACEMENT_3D('',#275241,#141496,#141497);
#111340=AXIS2_PLACEMENT_3D('',#275243,#141499,#141500);
#111341=AXIS2_PLACEMENT_3D('',#275249,#141504,#141505);
#111342=AXIS2_PLACEMENT_3D('',#275251,#141506,#141507);
#111343=AXIS2_PLACEMENT_3D('',#275253,#141508,#141509);
#111344=AXIS2_PLACEMENT_3D('',#275255,#141511,#141512);
#111345=AXIS2_PLACEMENT_3D('',#275261,#141516,#141517);
#111346=AXIS2_PLACEMENT_3D('',#275267,#141521,#141522);
#111347=AXIS2_PLACEMENT_3D('',#275273,#141526,#141527);
#111348=AXIS2_PLACEMENT_3D('',#275279,#141531,#141532);
#111349=AXIS2_PLACEMENT_3D('',#275281,#141533,#141534);
#111350=AXIS2_PLACEMENT_3D('',#275283,#141535,#141536);
#111351=AXIS2_PLACEMENT_3D('',#275285,#141538,#141539);
#111352=AXIS2_PLACEMENT_3D('',#275291,#141543,#141544);
#111353=AXIS2_PLACEMENT_3D('',#275293,#141545,#141546);
#111354=AXIS2_PLACEMENT_3D('',#275295,#141547,#141548);
#111355=AXIS2_PLACEMENT_3D('',#275297,#141550,#141551);
#111356=AXIS2_PLACEMENT_3D('',#275303,#141555,#141556);
#111357=AXIS2_PLACEMENT_3D('',#275304,#141557,#141558);
#111358=AXIS2_PLACEMENT_3D('',#275305,#141559,#141560);
#111359=AXIS2_PLACEMENT_3D('',#275306,#141561,#141562);
#111360=AXIS2_PLACEMENT_3D('',#275315,#141567,#141568);
#111361=AXIS2_PLACEMENT_3D('',#275317,#141569,#141570);
#111362=AXIS2_PLACEMENT_3D('',#275319,#141571,#141572);
#111363=AXIS2_PLACEMENT_3D('',#275321,#141574,#141575);
#111364=AXIS2_PLACEMENT_3D('',#275327,#141579,#141580);
#111365=AXIS2_PLACEMENT_3D('',#275333,#141584,#141585);
#111366=AXIS2_PLACEMENT_3D('',#275339,#141589,#141590);
#111367=AXIS2_PLACEMENT_3D('',#275345,#141594,#141595);
#111368=AXIS2_PLACEMENT_3D('',#275347,#141596,#141597);
#111369=AXIS2_PLACEMENT_3D('',#275349,#141598,#141599);
#111370=AXIS2_PLACEMENT_3D('',#275351,#141601,#141602);
#111371=AXIS2_PLACEMENT_3D('',#275357,#141606,#141607);
#111372=AXIS2_PLACEMENT_3D('',#275363,#141611,#141612);
#111373=AXIS2_PLACEMENT_3D('',#275369,#141616,#141617);
#111374=AXIS2_PLACEMENT_3D('',#275375,#141621,#141622);
#111375=AXIS2_PLACEMENT_3D('',#275377,#141623,#141624);
#111376=AXIS2_PLACEMENT_3D('',#275379,#141625,#141626);
#111377=AXIS2_PLACEMENT_3D('',#275381,#141628,#141629);
#111378=AXIS2_PLACEMENT_3D('',#275387,#141633,#141634);
#111379=AXIS2_PLACEMENT_3D('',#275389,#141635,#141636);
#111380=AXIS2_PLACEMENT_3D('',#275391,#141637,#141638);
#111381=AXIS2_PLACEMENT_3D('',#275393,#141640,#141641);
#111382=AXIS2_PLACEMENT_3D('',#275399,#141645,#141646);
#111383=AXIS2_PLACEMENT_3D('',#275401,#141647,#141648);
#111384=AXIS2_PLACEMENT_3D('',#275403,#141649,#141650);
#111385=AXIS2_PLACEMENT_3D('',#275405,#141652,#141653);
#111386=AXIS2_PLACEMENT_3D('',#275411,#141657,#141658);
#111387=AXIS2_PLACEMENT_3D('',#275413,#141659,#141660);
#111388=AXIS2_PLACEMENT_3D('',#275415,#141661,#141662);
#111389=AXIS2_PLACEMENT_3D('',#275417,#141664,#141665);
#111390=AXIS2_PLACEMENT_3D('',#275420,#141668,#141669);
#111391=AXIS2_PLACEMENT_3D('',#275429,#141674,#141675);
#111392=AXIS2_PLACEMENT_3D('',#275435,#141679,#141680);
#111393=AXIS2_PLACEMENT_3D('',#275441,#141684,#141685);
#111394=AXIS2_PLACEMENT_3D('',#275443,#141686,#141687);
#111395=AXIS2_PLACEMENT_3D('',#275445,#141688,#141689);
#111396=AXIS2_PLACEMENT_3D('',#275447,#141691,#141692);
#111397=AXIS2_PLACEMENT_3D('',#275453,#141696,#141697);
#111398=AXIS2_PLACEMENT_3D('',#275455,#141698,#141699);
#111399=AXIS2_PLACEMENT_3D('',#275457,#141700,#141701);
#111400=AXIS2_PLACEMENT_3D('',#275459,#141703,#141704);
#111401=AXIS2_PLACEMENT_3D('',#275465,#141708,#141709);
#111402=AXIS2_PLACEMENT_3D('',#275467,#141710,#141711);
#111403=AXIS2_PLACEMENT_3D('',#275469,#141712,#141713);
#111404=AXIS2_PLACEMENT_3D('',#275471,#141715,#141716);
#111405=AXIS2_PLACEMENT_3D('',#275477,#141720,#141721);
#111406=AXIS2_PLACEMENT_3D('',#275479,#141722,#141723);
#111407=AXIS2_PLACEMENT_3D('',#275481,#141724,#141725);
#111408=AXIS2_PLACEMENT_3D('',#275483,#141727,#141728);
#111409=AXIS2_PLACEMENT_3D('',#275489,#141732,#141733);
#111410=AXIS2_PLACEMENT_3D('',#275495,#141737,#141738);
#111411=AXIS2_PLACEMENT_3D('',#275498,#141741,#141742);
#111412=AXIS2_PLACEMENT_3D('',#275507,#141747,#141748);
#111413=AXIS2_PLACEMENT_3D('',#275513,#141752,#141753);
#111414=AXIS2_PLACEMENT_3D('',#275519,#141757,#141758);
#111415=AXIS2_PLACEMENT_3D('',#275525,#141762,#141763);
#111416=AXIS2_PLACEMENT_3D('',#275527,#141764,#141765);
#111417=AXIS2_PLACEMENT_3D('',#275529,#141766,#141767);
#111418=AXIS2_PLACEMENT_3D('',#275531,#141769,#141770);
#111419=AXIS2_PLACEMENT_3D('',#275537,#141774,#141775);
#111420=AXIS2_PLACEMENT_3D('',#275539,#141776,#141777);
#111421=AXIS2_PLACEMENT_3D('',#275541,#141778,#141779);
#111422=AXIS2_PLACEMENT_3D('',#275543,#141781,#141782);
#111423=AXIS2_PLACEMENT_3D('',#275549,#141786,#141787);
#111424=AXIS2_PLACEMENT_3D('',#275551,#141788,#141789);
#111425=AXIS2_PLACEMENT_3D('',#275553,#141790,#141791);
#111426=AXIS2_PLACEMENT_3D('',#275555,#141793,#141794);
#111427=AXIS2_PLACEMENT_3D('',#275561,#141798,#141799);
#111428=AXIS2_PLACEMENT_3D('',#275563,#141800,#141801);
#111429=AXIS2_PLACEMENT_3D('',#275565,#141802,#141803);
#111430=AXIS2_PLACEMENT_3D('',#275567,#141805,#141806);
#111431=AXIS2_PLACEMENT_3D('',#275573,#141810,#141811);
#111432=AXIS2_PLACEMENT_3D('',#275579,#141815,#141816);
#111433=AXIS2_PLACEMENT_3D('',#275585,#141820,#141821);
#111434=AXIS2_PLACEMENT_3D('',#275591,#141825,#141826);
#111435=AXIS2_PLACEMENT_3D('',#275593,#141827,#141828);
#111436=AXIS2_PLACEMENT_3D('',#275595,#141829,#141830);
#111437=AXIS2_PLACEMENT_3D('',#275597,#141832,#141833);
#111438=AXIS2_PLACEMENT_3D('',#275603,#141837,#141838);
#111439=AXIS2_PLACEMENT_3D('',#275605,#141839,#141840);
#111440=AXIS2_PLACEMENT_3D('',#275607,#141841,#141842);
#111441=AXIS2_PLACEMENT_3D('',#275609,#141844,#141845);
#111442=AXIS2_PLACEMENT_3D('',#275615,#141849,#141850);
#111443=AXIS2_PLACEMENT_3D('',#275617,#141851,#141852);
#111444=AXIS2_PLACEMENT_3D('',#275619,#141853,#141854);
#111445=AXIS2_PLACEMENT_3D('',#275621,#141856,#141857);
#111446=AXIS2_PLACEMENT_3D('',#275627,#141861,#141862);
#111447=AXIS2_PLACEMENT_3D('',#275629,#141863,#141864);
#111448=AXIS2_PLACEMENT_3D('',#275631,#141865,#141866);
#111449=AXIS2_PLACEMENT_3D('',#275633,#141868,#141869);
#111450=AXIS2_PLACEMENT_3D('',#275639,#141873,#141874);
#111451=AXIS2_PLACEMENT_3D('',#275645,#141878,#141879);
#111452=AXIS2_PLACEMENT_3D('',#275651,#141883,#141884);
#111453=AXIS2_PLACEMENT_3D('',#275657,#141888,#141889);
#111454=AXIS2_PLACEMENT_3D('',#275659,#141890,#141891);
#111455=AXIS2_PLACEMENT_3D('',#275661,#141892,#141893);
#111456=AXIS2_PLACEMENT_3D('',#275663,#141895,#141896);
#111457=AXIS2_PLACEMENT_3D('',#275669,#141900,#141901);
#111458=AXIS2_PLACEMENT_3D('',#275675,#141905,#141906);
#111459=AXIS2_PLACEMENT_3D('',#275681,#141910,#141911);
#111460=AXIS2_PLACEMENT_3D('',#275687,#141915,#141916);
#111461=AXIS2_PLACEMENT_3D('',#275689,#141917,#141918);
#111462=AXIS2_PLACEMENT_3D('',#275691,#141919,#141920);
#111463=AXIS2_PLACEMENT_3D('',#275693,#141922,#141923);
#111464=AXIS2_PLACEMENT_3D('',#275699,#141927,#141928);
#111465=AXIS2_PLACEMENT_3D('',#275701,#141929,#141930);
#111466=AXIS2_PLACEMENT_3D('',#275703,#141931,#141932);
#111467=AXIS2_PLACEMENT_3D('',#275705,#141934,#141935);
#111468=AXIS2_PLACEMENT_3D('',#275711,#141939,#141940);
#111469=AXIS2_PLACEMENT_3D('',#275713,#141941,#141942);
#111470=AXIS2_PLACEMENT_3D('',#275715,#141943,#141944);
#111471=AXIS2_PLACEMENT_3D('',#275717,#141946,#141947);
#111472=AXIS2_PLACEMENT_3D('',#275723,#141951,#141952);
#111473=AXIS2_PLACEMENT_3D('',#275725,#141953,#141954);
#111474=AXIS2_PLACEMENT_3D('',#275727,#141955,#141956);
#111475=AXIS2_PLACEMENT_3D('',#275729,#141958,#141959);
#111476=AXIS2_PLACEMENT_3D('',#275732,#141962,#141963);
#111477=AXIS2_PLACEMENT_3D('',#275741,#141968,#141969);
#111478=AXIS2_PLACEMENT_3D('',#275747,#141973,#141974);
#111479=AXIS2_PLACEMENT_3D('',#275753,#141978,#141979);
#111480=AXIS2_PLACEMENT_3D('',#275755,#141980,#141981);
#111481=AXIS2_PLACEMENT_3D('',#275757,#141982,#141983);
#111482=AXIS2_PLACEMENT_3D('',#275759,#141985,#141986);
#111483=AXIS2_PLACEMENT_3D('',#275765,#141990,#141991);
#111484=AXIS2_PLACEMENT_3D('',#275767,#141992,#141993);
#111485=AXIS2_PLACEMENT_3D('',#275769,#141994,#141995);
#111486=AXIS2_PLACEMENT_3D('',#275771,#141997,#141998);
#111487=AXIS2_PLACEMENT_3D('',#275777,#142002,#142003);
#111488=AXIS2_PLACEMENT_3D('',#275779,#142004,#142005);
#111489=AXIS2_PLACEMENT_3D('',#275781,#142006,#142007);
#111490=AXIS2_PLACEMENT_3D('',#275783,#142009,#142010);
#111491=AXIS2_PLACEMENT_3D('',#275789,#142014,#142015);
#111492=AXIS2_PLACEMENT_3D('',#275791,#142016,#142017);
#111493=AXIS2_PLACEMENT_3D('',#275793,#142018,#142019);
#111494=AXIS2_PLACEMENT_3D('',#275795,#142021,#142022);
#111495=AXIS2_PLACEMENT_3D('',#275801,#142026,#142027);
#111496=AXIS2_PLACEMENT_3D('',#275807,#142031,#142032);
#111497=AXIS2_PLACEMENT_3D('',#275810,#142035,#142036);
#111498=AXIS2_PLACEMENT_3D('',#275819,#142041,#142042);
#111499=AXIS2_PLACEMENT_3D('',#275825,#142046,#142047);
#111500=AXIS2_PLACEMENT_3D('',#275831,#142051,#142052);
#111501=AXIS2_PLACEMENT_3D('',#275837,#142056,#142057);
#111502=AXIS2_PLACEMENT_3D('',#275839,#142058,#142059);
#111503=AXIS2_PLACEMENT_3D('',#275841,#142060,#142061);
#111504=AXIS2_PLACEMENT_3D('',#275843,#142063,#142064);
#111505=AXIS2_PLACEMENT_3D('',#275849,#142068,#142069);
#111506=AXIS2_PLACEMENT_3D('',#275851,#142070,#142071);
#111507=AXIS2_PLACEMENT_3D('',#275853,#142072,#142073);
#111508=AXIS2_PLACEMENT_3D('',#275855,#142075,#142076);
#111509=AXIS2_PLACEMENT_3D('',#275861,#142080,#142081);
#111510=AXIS2_PLACEMENT_3D('',#275863,#142082,#142083);
#111511=AXIS2_PLACEMENT_3D('',#275865,#142084,#142085);
#111512=AXIS2_PLACEMENT_3D('',#275867,#142087,#142088);
#111513=AXIS2_PLACEMENT_3D('',#275873,#142092,#142093);
#111514=AXIS2_PLACEMENT_3D('',#275875,#142094,#142095);
#111515=AXIS2_PLACEMENT_3D('',#275877,#142096,#142097);
#111516=AXIS2_PLACEMENT_3D('',#275879,#142099,#142100);
#111517=AXIS2_PLACEMENT_3D('',#275885,#142104,#142105);
#111518=AXIS2_PLACEMENT_3D('',#275891,#142109,#142110);
#111519=AXIS2_PLACEMENT_3D('',#275897,#142114,#142115);
#111520=AXIS2_PLACEMENT_3D('',#275903,#142119,#142120);
#111521=AXIS2_PLACEMENT_3D('',#275905,#142121,#142122);
#111522=AXIS2_PLACEMENT_3D('',#275907,#142123,#142124);
#111523=AXIS2_PLACEMENT_3D('',#275909,#142126,#142127);
#111524=AXIS2_PLACEMENT_3D('',#275915,#142131,#142132);
#111525=AXIS2_PLACEMENT_3D('',#275917,#142133,#142134);
#111526=AXIS2_PLACEMENT_3D('',#275919,#142135,#142136);
#111527=AXIS2_PLACEMENT_3D('',#275921,#142138,#142139);
#111528=AXIS2_PLACEMENT_3D('',#275927,#142143,#142144);
#111529=AXIS2_PLACEMENT_3D('',#275929,#142145,#142146);
#111530=AXIS2_PLACEMENT_3D('',#275931,#142147,#142148);
#111531=AXIS2_PLACEMENT_3D('',#275933,#142150,#142151);
#111532=AXIS2_PLACEMENT_3D('',#275939,#142155,#142156);
#111533=AXIS2_PLACEMENT_3D('',#275941,#142157,#142158);
#111534=AXIS2_PLACEMENT_3D('',#275943,#142159,#142160);
#111535=AXIS2_PLACEMENT_3D('',#275945,#142162,#142163);
#111536=AXIS2_PLACEMENT_3D('',#275951,#142167,#142168);
#111537=AXIS2_PLACEMENT_3D('',#275957,#142172,#142173);
#111538=AXIS2_PLACEMENT_3D('',#275963,#142177,#142178);
#111539=AXIS2_PLACEMENT_3D('',#275969,#142182,#142183);
#111540=AXIS2_PLACEMENT_3D('',#275971,#142184,#142185);
#111541=AXIS2_PLACEMENT_3D('',#275973,#142186,#142187);
#111542=AXIS2_PLACEMENT_3D('',#275975,#142189,#142190);
#111543=AXIS2_PLACEMENT_3D('',#275981,#142194,#142195);
#111544=AXIS2_PLACEMENT_3D('',#275987,#142199,#142200);
#111545=AXIS2_PLACEMENT_3D('',#275993,#142204,#142205);
#111546=AXIS2_PLACEMENT_3D('',#275999,#142209,#142210);
#111547=AXIS2_PLACEMENT_3D('',#276001,#142211,#142212);
#111548=AXIS2_PLACEMENT_3D('',#276003,#142213,#142214);
#111549=AXIS2_PLACEMENT_3D('',#276005,#142216,#142217);
#111550=AXIS2_PLACEMENT_3D('',#276011,#142221,#142222);
#111551=AXIS2_PLACEMENT_3D('',#276013,#142223,#142224);
#111552=AXIS2_PLACEMENT_3D('',#276015,#142225,#142226);
#111553=AXIS2_PLACEMENT_3D('',#276017,#142228,#142229);
#111554=AXIS2_PLACEMENT_3D('',#276023,#142233,#142234);
#111555=AXIS2_PLACEMENT_3D('',#276025,#142235,#142236);
#111556=AXIS2_PLACEMENT_3D('',#276027,#142237,#142238);
#111557=AXIS2_PLACEMENT_3D('',#276029,#142240,#142241);
#111558=AXIS2_PLACEMENT_3D('',#276035,#142245,#142246);
#111559=AXIS2_PLACEMENT_3D('',#276037,#142247,#142248);
#111560=AXIS2_PLACEMENT_3D('',#276039,#142249,#142250);
#111561=AXIS2_PLACEMENT_3D('',#276041,#142252,#142253);
#111562=AXIS2_PLACEMENT_3D('',#276044,#142256,#142257);
#111563=AXIS2_PLACEMENT_3D('',#276053,#142262,#142263);
#111564=AXIS2_PLACEMENT_3D('',#276059,#142267,#142268);
#111565=AXIS2_PLACEMENT_3D('',#276065,#142272,#142273);
#111566=AXIS2_PLACEMENT_3D('',#276067,#142274,#142275);
#111567=AXIS2_PLACEMENT_3D('',#276069,#142276,#142277);
#111568=AXIS2_PLACEMENT_3D('',#276071,#142279,#142280);
#111569=AXIS2_PLACEMENT_3D('',#276077,#142284,#142285);
#111570=AXIS2_PLACEMENT_3D('',#276079,#142286,#142287);
#111571=AXIS2_PLACEMENT_3D('',#276081,#142288,#142289);
#111572=AXIS2_PLACEMENT_3D('',#276083,#142291,#142292);
#111573=AXIS2_PLACEMENT_3D('',#276089,#142296,#142297);
#111574=AXIS2_PLACEMENT_3D('',#276091,#142298,#142299);
#111575=AXIS2_PLACEMENT_3D('',#276093,#142300,#142301);
#111576=AXIS2_PLACEMENT_3D('',#276095,#142303,#142304);
#111577=AXIS2_PLACEMENT_3D('',#276101,#142308,#142309);
#111578=AXIS2_PLACEMENT_3D('',#276103,#142310,#142311);
#111579=AXIS2_PLACEMENT_3D('',#276105,#142312,#142313);
#111580=AXIS2_PLACEMENT_3D('',#276107,#142315,#142316);
#111581=AXIS2_PLACEMENT_3D('',#276113,#142320,#142321);
#111582=AXIS2_PLACEMENT_3D('',#276119,#142325,#142326);
#111583=AXIS2_PLACEMENT_3D('',#276122,#142329,#142330);
#111584=AXIS2_PLACEMENT_3D('',#276128,#142334,#142335);
#111585=AXIS2_PLACEMENT_3D('',#276134,#142339,#142340);
#111586=AXIS2_PLACEMENT_3D('',#276140,#142344,#142345);
#111587=AXIS2_PLACEMENT_3D('',#276142,#142346,#142347);
#111588=AXIS2_PLACEMENT_3D('',#276144,#142348,#142349);
#111589=AXIS2_PLACEMENT_3D('',#276146,#142351,#142352);
#111590=AXIS2_PLACEMENT_3D('',#276152,#142356,#142357);
#111591=AXIS2_PLACEMENT_3D('',#276154,#142358,#142359);
#111592=AXIS2_PLACEMENT_3D('',#276156,#142360,#142361);
#111593=AXIS2_PLACEMENT_3D('',#276158,#142363,#142364);
#111594=AXIS2_PLACEMENT_3D('',#276164,#142368,#142369);
#111595=AXIS2_PLACEMENT_3D('',#276166,#142370,#142371);
#111596=AXIS2_PLACEMENT_3D('',#276168,#142372,#142373);
#111597=AXIS2_PLACEMENT_3D('',#276170,#142375,#142376);
#111598=AXIS2_PLACEMENT_3D('',#276176,#142380,#142381);
#111599=AXIS2_PLACEMENT_3D('',#276178,#142382,#142383);
#111600=AXIS2_PLACEMENT_3D('',#276180,#142384,#142385);
#111601=AXIS2_PLACEMENT_3D('',#276182,#142387,#142388);
#111602=AXIS2_PLACEMENT_3D('',#276188,#142392,#142393);
#111603=AXIS2_PLACEMENT_3D('',#276194,#142397,#142398);
#111604=AXIS2_PLACEMENT_3D('',#276200,#142402,#142403);
#111605=AXIS2_PLACEMENT_3D('',#276206,#142407,#142408);
#111606=AXIS2_PLACEMENT_3D('',#276208,#142409,#142410);
#111607=AXIS2_PLACEMENT_3D('',#276210,#142411,#142412);
#111608=AXIS2_PLACEMENT_3D('',#276212,#142414,#142415);
#111609=AXIS2_PLACEMENT_3D('',#276218,#142419,#142420);
#111610=AXIS2_PLACEMENT_3D('',#276220,#142421,#142422);
#111611=AXIS2_PLACEMENT_3D('',#276222,#142423,#142424);
#111612=AXIS2_PLACEMENT_3D('',#276224,#142426,#142427);
#111613=AXIS2_PLACEMENT_3D('',#276230,#142431,#142432);
#111614=AXIS2_PLACEMENT_3D('',#276232,#142433,#142434);
#111615=AXIS2_PLACEMENT_3D('',#276234,#142435,#142436);
#111616=AXIS2_PLACEMENT_3D('',#276236,#142438,#142439);
#111617=AXIS2_PLACEMENT_3D('',#276242,#142443,#142444);
#111618=AXIS2_PLACEMENT_3D('',#276244,#142445,#142446);
#111619=AXIS2_PLACEMENT_3D('',#276246,#142447,#142448);
#111620=AXIS2_PLACEMENT_3D('',#276248,#142450,#142451);
#111621=AXIS2_PLACEMENT_3D('',#276254,#142455,#142456);
#111622=AXIS2_PLACEMENT_3D('',#276260,#142460,#142461);
#111623=AXIS2_PLACEMENT_3D('',#276266,#142465,#142466);
#111624=AXIS2_PLACEMENT_3D('',#276272,#142470,#142471);
#111625=AXIS2_PLACEMENT_3D('',#276274,#142472,#142473);
#111626=AXIS2_PLACEMENT_3D('',#276276,#142474,#142475);
#111627=AXIS2_PLACEMENT_3D('',#276278,#142477,#142478);
#111628=AXIS2_PLACEMENT_3D('',#276284,#142482,#142483);
#111629=AXIS2_PLACEMENT_3D('',#276290,#142487,#142488);
#111630=AXIS2_PLACEMENT_3D('',#276296,#142492,#142493);
#111631=AXIS2_PLACEMENT_3D('',#276302,#142497,#142498);
#111632=AXIS2_PLACEMENT_3D('',#276304,#142499,#142500);
#111633=AXIS2_PLACEMENT_3D('',#276306,#142501,#142502);
#111634=AXIS2_PLACEMENT_3D('',#276308,#142504,#142505);
#111635=AXIS2_PLACEMENT_3D('',#276314,#142509,#142510);
#111636=AXIS2_PLACEMENT_3D('',#276316,#142511,#142512);
#111637=AXIS2_PLACEMENT_3D('',#276318,#142513,#142514);
#111638=AXIS2_PLACEMENT_3D('',#276320,#142516,#142517);
#111639=AXIS2_PLACEMENT_3D('',#276326,#142521,#142522);
#111640=AXIS2_PLACEMENT_3D('',#276328,#142523,#142524);
#111641=AXIS2_PLACEMENT_3D('',#276330,#142525,#142526);
#111642=AXIS2_PLACEMENT_3D('',#276332,#142528,#142529);
#111643=AXIS2_PLACEMENT_3D('',#276338,#142533,#142534);
#111644=AXIS2_PLACEMENT_3D('',#276340,#142535,#142536);
#111645=AXIS2_PLACEMENT_3D('',#276342,#142537,#142538);
#111646=AXIS2_PLACEMENT_3D('',#276344,#142540,#142541);
#111647=AXIS2_PLACEMENT_3D('',#276347,#142544,#142545);
#111648=AXIS2_PLACEMENT_3D('',#276353,#142549,#142550);
#111649=AXIS2_PLACEMENT_3D('',#276356,#142553,#142554);
#111650=AXIS2_PLACEMENT_3D('',#276362,#142558,#142559);
#111651=AXIS2_PLACEMENT_3D('',#276365,#142562,#142563);
#111652=AXIS2_PLACEMENT_3D('',#276382,#142572,#142573);
#111653=AXIS2_PLACEMENT_3D('',#276388,#142577,#142578);
#111654=AXIS2_PLACEMENT_3D('',#276392,#142581,#142582);
#111655=AXIS2_PLACEMENT_3D('',#276396,#142585,#142586);
#111656=AXIS2_PLACEMENT_3D('',#276400,#142589,#142590);
#111657=AXIS2_PLACEMENT_3D('',#276404,#142593,#142594);
#111658=AXIS2_PLACEMENT_3D('',#276408,#142597,#142598);
#111659=AXIS2_PLACEMENT_3D('',#276412,#142601,#142602);
#111660=AXIS2_PLACEMENT_3D('',#276414,#142604,#142605);
#111661=AXIS2_PLACEMENT_3D('',#276415,#142606,#142607);
#111662=AXIS2_PLACEMENT_3D('',#276424,#142612,#142613);
#111663=AXIS2_PLACEMENT_3D('',#276430,#142617,#142618);
#111664=AXIS2_PLACEMENT_3D('',#276436,#142622,#142623);
#111665=AXIS2_PLACEMENT_3D('',#276439,#142626,#142627);
#111666=AXIS2_PLACEMENT_3D('',#276440,#142628,#142629);
#111667=AXIS2_PLACEMENT_3D('',#276441,#142630,#142631);
#111668=AXIS2_PLACEMENT_3D('',#276442,#142632,#142633);
#111669=AXIS2_PLACEMENT_3D('',#276443,#142634,#142635);
#111670=AXIS2_PLACEMENT_3D('',#276444,#142636,#142637);
#111671=AXIS2_PLACEMENT_3D('',#276445,#142638,#142639);
#111672=AXIS2_PLACEMENT_3D('',#276446,#142640,#142641);
#111673=DIRECTION('axis',(0.,0.,1.));
#111674=DIRECTION('refdir',(1.,0.,0.));
#111675=DIRECTION('axis',(0.,0.,1.));
#111676=DIRECTION('refdir',(1.,0.,0.));
#111677=DIRECTION('center_axis',(0.,-1.,0.));
#111678=DIRECTION('ref_axis',(0.,0.,-1.));
#111679=DIRECTION('center_axis',(0.,1.,0.));
#111680=DIRECTION('ref_axis',(0.,0.,-1.));
#111681=DIRECTION('',(0.,-1.,0.));
#111682=DIRECTION('center_axis',(0.,-1.,0.));
#111683=DIRECTION('ref_axis',(0.,0.,-1.));
#111684=DIRECTION('center_axis',(0.,-1.,0.));
#111685=DIRECTION('ref_axis',(0.,0.,-1.));
#111686=DIRECTION('center_axis',(0.,1.,0.));
#111687=DIRECTION('ref_axis',(0.,0.,-1.));
#111688=DIRECTION('',(0.,-1.,0.));
#111689=DIRECTION('center_axis',(0.,-1.,0.));
#111690=DIRECTION('ref_axis',(0.,0.,-1.));
#111691=DIRECTION('center_axis',(0.,-1.,0.));
#111692=DIRECTION('ref_axis',(0.,0.,-1.));
#111693=DIRECTION('center_axis',(0.,1.,0.));
#111694=DIRECTION('ref_axis',(0.,0.,-1.));
#111695=DIRECTION('',(0.,-1.,0.));
#111696=DIRECTION('center_axis',(0.,-1.,0.));
#111697=DIRECTION('ref_axis',(0.,0.,-1.));
#111698=DIRECTION('center_axis',(0.,-1.,0.));
#111699=DIRECTION('ref_axis',(0.,0.,-1.));
#111700=DIRECTION('center_axis',(0.,1.,0.));
#111701=DIRECTION('ref_axis',(0.,0.,-1.));
#111702=DIRECTION('',(0.,-1.,0.));
#111703=DIRECTION('center_axis',(0.,-1.,0.));
#111704=DIRECTION('ref_axis',(0.,0.,-1.));
#111705=DIRECTION('center_axis',(1.,0.,-2.17690789142188E-16));
#111706=DIRECTION('ref_axis',(-2.17690789142188E-16,0.,-1.));
#111707=DIRECTION('',(-2.17690789142188E-16,0.,-1.));
#111708=DIRECTION('',(0.,1.,0.));
#111709=DIRECTION('',(-2.17690789142188E-16,-1.23259516440783E-32,-1.));
#111710=DIRECTION('',(0.,1.,0.));
#111711=DIRECTION('center_axis',(0.,0.,1.));
#111712=DIRECTION('ref_axis',(1.,0.,0.));
#111713=DIRECTION('',(1.,0.,0.));
#111714=DIRECTION('',(0.,1.,0.));
#111715=DIRECTION('',(1.,0.,0.));
#111716=DIRECTION('center_axis',(-1.,0.,1.08845394571094E-16));
#111717=DIRECTION('ref_axis',(1.08845394571094E-16,0.,1.));
#111718=DIRECTION('',(1.08845394571094E-16,0.,1.));
#111719=DIRECTION('',(0.,1.,0.));
#111720=DIRECTION('',(1.08845394571094E-16,-6.16297582203916E-33,1.));
#111721=DIRECTION('center_axis',(0.,0.,-1.));
#111722=DIRECTION('ref_axis',(-1.,0.,0.));
#111723=DIRECTION('',(-1.,0.,0.));
#111724=DIRECTION('',(-1.,0.,0.));
#111725=DIRECTION('center_axis',(0.,1.,0.));
#111726=DIRECTION('ref_axis',(0.,0.,1.));
#111727=DIRECTION('',(-2.17690789142188E-16,0.,-1.));
#111728=DIRECTION('',(1.,0.,0.));
#111729=DIRECTION('',(1.08845394571094E-16,0.,1.));
#111730=DIRECTION('',(-1.,0.,0.));
#111731=DIRECTION('center_axis',(0.,-0.456804684992628,-0.889567018143538));
#111732=DIRECTION('ref_axis',(0.,0.889567018143538,-0.456804684992628));
#111733=DIRECTION('',(-0.415505315998661,0.809141931155286,-0.415505315998661));
#111734=DIRECTION('',(0.415505315998661,0.809141931155287,-0.415505315998661));
#111735=DIRECTION('',(1.,0.,0.));
#111736=DIRECTION('center_axis',(0.889567018143538,-0.456804684992628,-1.9365054617453E-16));
#111737=DIRECTION('ref_axis',(0.456804684992628,0.889567018143538,1.95408218286693E-33));
#111738=DIRECTION('',(0.415505315998661,0.809141931155287,0.415505315998661));
#111739=DIRECTION('',(2.17690789142188E-16,0.,1.));
#111740=DIRECTION('center_axis',(-0.889567018143538,-0.456804684992628,
9.68252730872648E-17));
#111741=DIRECTION('ref_axis',(0.456804684992628,-0.889567018143538,-8.78056366297357E-35));
#111742=DIRECTION('',(-0.415505315998661,0.809141931155287,0.415505315998661));
#111743=DIRECTION('',(-1.08845394571094E-16,0.,-1.));
#111744=DIRECTION('center_axis',(0.,-0.456804684992628,0.889567018143538));
#111745=DIRECTION('ref_axis',(0.,-0.889567018143538,-0.456804684992628));
#111746=DIRECTION('',(-1.,0.,0.));
#111747=DIRECTION('center_axis',(1.,0.,-2.17690789142188E-16));
#111748=DIRECTION('ref_axis',(-2.17690789142188E-16,0.,-1.));
#111749=DIRECTION('',(0.,1.,0.));
#111750=DIRECTION('',(-2.17690789142188E-16,0.,-1.));
#111751=DIRECTION('',(0.,1.,0.));
#111752=DIRECTION('center_axis',(0.,0.,1.));
#111753=DIRECTION('ref_axis',(1.,0.,0.));
#111754=DIRECTION('',(1.,0.,0.));
#111755=DIRECTION('',(0.,1.,0.));
#111756=DIRECTION('center_axis',(-1.,0.,1.08845394571094E-16));
#111757=DIRECTION('ref_axis',(1.08845394571094E-16,0.,1.));
#111758=DIRECTION('',(1.08845394571094E-16,0.,1.));
#111759=DIRECTION('',(0.,1.,0.));
#111760=DIRECTION('center_axis',(0.,0.,-1.));
#111761=DIRECTION('ref_axis',(-1.,0.,0.));
#111762=DIRECTION('',(-1.,0.,0.));
#111763=DIRECTION('center_axis',(0.,-0.456804684992628,-0.889567018143538));
#111764=DIRECTION('ref_axis',(0.,0.889567018143538,-0.456804684992628));
#111765=DIRECTION('',(-0.415505315998661,0.809141931155286,-0.415505315998661));
#111766=DIRECTION('',(1.,0.,0.));
#111767=DIRECTION('',(0.41550531599866,0.809141931155286,-0.415505315998661));
#111768=DIRECTION('center_axis',(0.889567018143538,-0.456804684992628,-1.9365054617453E-16));
#111769=DIRECTION('ref_axis',(0.456804684992628,0.889567018143538,1.95408218286693E-33));
#111770=DIRECTION('',(0.,0.,1.));
#111771=DIRECTION('',(0.415505315998661,0.809141931155286,0.415505315998661));
#111772=DIRECTION('center_axis',(-0.889567018143538,-0.456804684992628,
9.68252730872648E-17));
#111773=DIRECTION('ref_axis',(0.456804684992628,-0.889567018143538,-8.78056366297357E-35));
#111774=DIRECTION('',(-0.415505315998661,0.809141931155287,0.415505315998661));
#111775=DIRECTION('',(2.1350442781253E-16,0.,-1.));
#111776=DIRECTION('center_axis',(0.,-0.456804684992628,0.889567018143538));
#111777=DIRECTION('ref_axis',(0.,-0.889567018143538,-0.456804684992628));
#111778=DIRECTION('',(-1.,0.,0.));
#111779=DIRECTION('center_axis',(0.,0.,-1.));
#111780=DIRECTION('ref_axis',(-1.,0.,0.));
#111781=DIRECTION('',(0.,1.,0.));
#111782=DIRECTION('',(1.,0.,0.));
#111783=DIRECTION('',(0.,1.,0.));
#111784=DIRECTION('center_axis',(1.,0.,0.));
#111785=DIRECTION('ref_axis',(0.,0.,-1.));
#111786=DIRECTION('',(0.,0.,1.));
#111787=DIRECTION('',(0.,1.,0.));
#111788=DIRECTION('center_axis',(0.,0.,1.));
#111789=DIRECTION('ref_axis',(1.,0.,0.));
#111790=DIRECTION('',(-1.,0.,0.));
#111791=DIRECTION('',(0.,1.,0.));
#111792=DIRECTION('center_axis',(-1.,0.,-2.1350442781253E-16));
#111793=DIRECTION('ref_axis',(-2.1350442781253E-16,0.,1.));
#111794=DIRECTION('',(0.,0.,-1.));
#111795=DIRECTION('center_axis',(0.,-1.,0.));
#111796=DIRECTION('ref_axis',(0.,0.,-1.));
#111797=DIRECTION('',(0.,0.,-1.));
#111798=DIRECTION('center_axis',(0.,1.,0.));
#111799=DIRECTION('ref_axis',(0.,0.,-1.));
#111800=DIRECTION('',(-1.,0.,0.));
#111801=DIRECTION('center_axis',(0.,1.,0.));
#111802=DIRECTION('ref_axis',(0.,0.,-1.));
#111803=DIRECTION('',(0.,0.,1.));
#111804=DIRECTION('center_axis',(0.,1.,0.));
#111805=DIRECTION('ref_axis',(0.,0.,-1.));
#111806=DIRECTION('',(1.,0.,0.));
#111807=DIRECTION('center_axis',(0.,1.,0.));
#111808=DIRECTION('ref_axis',(0.,0.,-1.));
#111809=DIRECTION('center_axis',(0.,-1.,0.));
#111810=DIRECTION('ref_axis',(0.,0.,-1.));
#111811=DIRECTION('',(0.,0.,1.));
#111812=DIRECTION('center_axis',(0.,-1.,0.));
#111813=DIRECTION('ref_axis',(0.,0.,-1.));
#111814=DIRECTION('',(-1.,0.,0.));
#111815=DIRECTION('center_axis',(0.,-1.,0.));
#111816=DIRECTION('ref_axis',(0.,0.,-1.));
#111817=DIRECTION('',(0.,0.,-1.));
#111818=DIRECTION('center_axis',(0.,-1.,0.));
#111819=DIRECTION('ref_axis',(0.,0.,-1.));
#111820=DIRECTION('',(1.,0.,0.));
#111821=DIRECTION('center_axis',(0.,-1.,0.));
#111822=DIRECTION('ref_axis',(0.,0.,-1.));
#111823=DIRECTION('center_axis',(-1.,0.,0.));
#111824=DIRECTION('ref_axis',(0.,0.,1.));
#111825=DIRECTION('',(0.,1.,0.));
#111826=DIRECTION('',(0.,0.,1.));
#111827=DIRECTION('',(0.,-1.,0.));
#111828=DIRECTION('center_axis',(0.,0.,-1.));
#111829=DIRECTION('ref_axis',(-1.,0.,0.));
#111830=DIRECTION('',(0.,1.,0.));
#111831=DIRECTION('',(-1.,0.,0.));
#111832=DIRECTION('',(0.,-1.,0.));
#111833=DIRECTION('center_axis',(1.,0.,0.));
#111834=DIRECTION('ref_axis',(0.,0.,-1.));
#111835=DIRECTION('',(0.,1.,0.));
#111836=DIRECTION('',(0.,0.,-1.));
#111837=DIRECTION('',(0.,-1.,0.));
#111838=DIRECTION('center_axis',(0.,0.,1.));
#111839=DIRECTION('ref_axis',(1.,0.,0.));
#111840=DIRECTION('',(0.,1.,0.));
#111841=DIRECTION('',(1.,0.,0.));
#111842=DIRECTION('',(0.,-1.,0.));
#111843=DIRECTION('center_axis',(0.,1.,0.));
#111844=DIRECTION('ref_axis',(0.,0.,1.));
#111845=DIRECTION('center_axis',(0.,-1.,0.));
#111846=DIRECTION('ref_axis',(0.,0.,-1.));
#111847=DIRECTION('center_axis',(0.,1.,0.));
#111848=DIRECTION('ref_axis',(0.,0.,1.));
#111849=DIRECTION('center_axis',(0.,-1.,0.));
#111850=DIRECTION('ref_axis',(0.,0.,-1.));
#111851=DIRECTION('center_axis',(0.,1.,0.));
#111852=DIRECTION('ref_axis',(0.,0.,1.));
#111853=DIRECTION('center_axis',(0.,-1.,0.));
#111854=DIRECTION('ref_axis',(0.,0.,-1.));
#111855=DIRECTION('center_axis',(0.,1.,0.));
#111856=DIRECTION('ref_axis',(0.,0.,1.));
#111857=DIRECTION('center_axis',(0.,-1.,0.));
#111858=DIRECTION('ref_axis',(0.,0.,-1.));
#111859=DIRECTION('center_axis',(0.,-1.,0.));
#111860=DIRECTION('ref_axis',(0.,0.,-1.));
#111861=DIRECTION('center_axis',(0.,0.,-1.));
#111862=DIRECTION('ref_axis',(-1.,0.,0.));
#111863=DIRECTION('center_axis',(1.,0.,0.));
#111864=DIRECTION('ref_axis',(0.,0.,-1.));
#111865=DIRECTION('center_axis',(-1.,0.,0.));
#111866=DIRECTION('ref_axis',(0.,0.,1.));
#111867=DIRECTION('center_axis',(1.,0.,0.));
#111868=DIRECTION('ref_axis',(0.,0.,-1.));
#111869=DIRECTION('center_axis',(0.,0.,-1.));
#111870=DIRECTION('ref_axis',(-1.,0.,0.));
#111871=DIRECTION('center_axis',(0.,0.,-1.));
#111872=DIRECTION('ref_axis',(-1.,0.,0.));
#111873=DIRECTION('center_axis',(0.,-1.,0.));
#111874=DIRECTION('ref_axis',(0.,0.,-1.));
#111875=DIRECTION('center_axis',(0.,0.,-1.));
#111876=DIRECTION('ref_axis',(-1.,0.,0.));
#111877=DIRECTION('center_axis',(0.,-1.,0.));
#111878=DIRECTION('ref_axis',(0.,0.,-1.));
#111879=DIRECTION('center_axis',(1.,0.,0.));
#111880=DIRECTION('ref_axis',(0.,0.,-1.));
#111881=DIRECTION('center_axis',(0.,0.,1.));
#111882=DIRECTION('ref_axis',(1.,0.,0.));
#111883=DIRECTION('center_axis',(0.,0.,-1.));
#111884=DIRECTION('ref_axis',(-1.,0.,0.));
#111885=DIRECTION('center_axis',(1.,0.,0.));
#111886=DIRECTION('ref_axis',(0.,0.,-1.));
#111887=DIRECTION('center_axis',(1.,0.,0.));
#111888=DIRECTION('ref_axis',(0.,0.,-1.));
#111889=DIRECTION('center_axis',(0.,-1.,0.));
#111890=DIRECTION('ref_axis',(0.,0.,-1.));
#111891=DIRECTION('axis',(0.,0.,1.));
#111892=DIRECTION('refdir',(1.,0.,0.));
#111893=DIRECTION('center_axis',(0.,-1.21968337170492E-16,1.));
#111894=DIRECTION('ref_axis',(0.,-1.,0.));
#111895=DIRECTION('center_axis',(0.,-1.21968337170492E-16,1.));
#111896=DIRECTION('ref_axis',(0.,-1.,-1.21968337170492E-16));
#111897=DIRECTION('center_axis',(0.,-1.21968337170492E-16,1.));
#111898=DIRECTION('ref_axis',(0.,-1.,-1.21968337170492E-16));
#111899=DIRECTION('center_axis',(-1.,-1.22464679914735E-16,-1.49368133713168E-32));
#111900=DIRECTION('ref_axis',(-1.22464679914735E-16,1.,0.));
#111901=DIRECTION('center_axis',(0.,1.21968337170492E-16,-1.));
#111902=DIRECTION('ref_axis',(0.,-1.,-1.21968337170492E-16));
#111903=DIRECTION('center_axis',(0.,-1.21968337170492E-16,1.));
#111904=DIRECTION('ref_axis',(0.,-1.,0.));
#111905=DIRECTION('center_axis',(0.,-1.21968337170492E-16,1.));
#111906=DIRECTION('ref_axis',(0.,-1.,-1.21968337170492E-16));
#111907=DIRECTION('center_axis',(-1.,-1.22464679914735E-16,-1.49368133713168E-32));
#111908=DIRECTION('ref_axis',(-1.22464679914735E-16,1.,0.));
#111909=DIRECTION('center_axis',(0.,1.21968337170492E-16,-1.));
#111910=DIRECTION('ref_axis',(0.,-1.,-1.21968337170492E-16));
#111911=DIRECTION('center_axis',(0.,1.21968337170492E-16,-1.));
#111912=DIRECTION('ref_axis',(0.,-1.,-1.21968337170492E-16));
#111913=DIRECTION('center_axis',(1.,-6.08557808619092E-15,0.));
#111914=DIRECTION('ref_axis',(6.08557808619092E-15,1.,0.));
#111915=DIRECTION('',(1.,-6.08557808619092E-15,0.));
#111916=DIRECTION('center_axis',(1.,-6.08557808619092E-15,0.));
#111917=DIRECTION('ref_axis',(6.08557808619092E-15,1.,0.));
#111918=DIRECTION('',(1.,-6.08557808619092E-15,0.));
#111919=DIRECTION('center_axis',(0.,-1.,0.));
#111920=DIRECTION('ref_axis',(0.,0.,-1.));
#111921=DIRECTION('',(0.,-1.,0.));
#111922=DIRECTION('center_axis',(0.,-1.,0.));
#111923=DIRECTION('ref_axis',(0.,0.,-1.));
#111924=DIRECTION('',(0.,-1.,0.));
#111925=DIRECTION('center_axis',(0.,1.21968337170492E-16,-1.));
#111926=DIRECTION('ref_axis',(0.,1.,1.21968337170492E-16));
#111927=DIRECTION('center_axis',(0.,1.21968337170492E-16,-1.));
#111928=DIRECTION('ref_axis',(0.,1.,1.21968337170492E-16));
#111929=DIRECTION('',(0.,-1.21968337170492E-16,1.));
#111930=DIRECTION('',(0.,-1.21968337170492E-16,1.));
#111931=DIRECTION('center_axis',(0.,1.21968337170492E-16,-1.));
#111932=DIRECTION('ref_axis',(0.,1.,1.21968337170492E-16));
#111933=DIRECTION('',(0.,1.21968337170492E-16,-1.));
#111934=DIRECTION('',(0.,1.21968337170492E-16,-1.));
#111935=DIRECTION('center_axis',(0.,1.21968337170492E-16,-1.));
#111936=DIRECTION('ref_axis',(0.,1.,1.21968337170492E-16));
#111937=DIRECTION('center_axis',(0.,-1.21968337170492E-16,1.));
#111938=DIRECTION('ref_axis',(0.,-1.,-1.21968337170492E-16));
#111939=DIRECTION('center_axis',(0.,1.21968337170492E-16,-1.));
#111940=DIRECTION('ref_axis',(0.,1.,1.21968337170492E-16));
#111941=DIRECTION('center_axis',(0.,0.,1.));
#111942=DIRECTION('ref_axis',(-2.97930117404573E-15,-1.,0.));
#111943=DIRECTION('',(0.,0.,1.));
#111944=DIRECTION('',(0.,0.,-1.));
#111945=DIRECTION('center_axis',(0.,0.,1.));
#111946=DIRECTION('ref_axis',(-2.97930117404573E-15,-1.,0.));
#111947=DIRECTION('',(0.,0.,1.));
#111948=DIRECTION('center_axis',(0.,0.,1.));
#111949=DIRECTION('ref_axis',(-2.97930117404573E-15,-1.,0.));
#111950=DIRECTION('',(0.,0.,1.));
#111951=DIRECTION('center_axis',(0.,0.,1.));
#111952=DIRECTION('ref_axis',(-2.97930117404573E-15,-1.,0.));
#111953=DIRECTION('',(0.,0.,1.));
#111954=DIRECTION('center_axis',(0.,0.,1.));
#111955=DIRECTION('ref_axis',(-2.97930117404573E-15,-1.,0.));
#111956=DIRECTION('',(0.,0.,1.));
#111957=DIRECTION('center_axis',(0.,0.,1.));
#111958=DIRECTION('ref_axis',(-2.97930117404573E-15,-1.,0.));
#111959=DIRECTION('',(0.,0.,1.));
#111960=DIRECTION('center_axis',(0.,0.,1.));
#111961=DIRECTION('ref_axis',(-2.97930117404573E-15,-1.,0.));
#111962=DIRECTION('',(0.,0.,1.));
#111963=DIRECTION('center_axis',(0.,0.,1.));
#111964=DIRECTION('ref_axis',(-2.97930117404573E-15,-1.,0.));
#111965=DIRECTION('',(0.,0.,1.));
#111966=DIRECTION('center_axis',(0.,1.21968337170492E-16,-1.));
#111967=DIRECTION('ref_axis',(0.,1.,1.21968337170492E-16));
#111968=DIRECTION('',(0.,-1.21968337170492E-16,1.));
#111969=DIRECTION('center_axis',(0.,1.21968337170492E-16,-1.));
#111970=DIRECTION('ref_axis',(0.,1.,1.21968337170492E-16));
#111971=DIRECTION('',(0.,-1.9115651027667E-14,1.));
#111972=DIRECTION('',(0.,-1.21968337170492E-16,1.));
#111973=DIRECTION('center_axis',(0.,1.21968337170492E-16,-1.));
#111974=DIRECTION('ref_axis',(0.,1.,1.21968337170492E-16));
#111975=DIRECTION('',(0.,-1.21968337170492E-16,1.));
#111976=DIRECTION('center_axis',(0.,1.21968337170492E-16,-1.));
#111977=DIRECTION('ref_axis',(0.,1.,1.21968337170492E-16));
#111978=DIRECTION('',(0.,-1.21968337170492E-16,1.));
#111979=DIRECTION('center_axis',(0.,1.21968337170492E-16,-1.));
#111980=DIRECTION('ref_axis',(0.,1.,1.21968337170492E-16));
#111981=DIRECTION('',(0.,-1.21968337170492E-16,1.));
#111982=DIRECTION('center_axis',(0.,1.21968337170492E-16,-1.));
#111983=DIRECTION('ref_axis',(0.,1.,1.21968337170492E-16));
#111984=DIRECTION('',(0.,-1.21968337170492E-16,1.));
#111985=DIRECTION('center_axis',(0.,1.21968337170492E-16,-1.));
#111986=DIRECTION('ref_axis',(0.,1.,1.21968337170492E-16));
#111987=DIRECTION('',(0.,-1.21968337170492E-16,1.));
#111988=DIRECTION('center_axis',(0.,1.21968337170492E-16,-1.));
#111989=DIRECTION('ref_axis',(0.,1.,1.21968337170492E-16));
#111990=DIRECTION('',(0.,-1.21968337170492E-16,1.));
#111991=DIRECTION('center_axis',(0.,1.21968337170492E-16,-1.));
#111992=DIRECTION('ref_axis',(0.,1.,1.21968337170492E-16));
#111993=DIRECTION('',(0.,-1.21968337170492E-16,1.));
#111994=DIRECTION('center_axis',(0.,0.,1.));
#111995=DIRECTION('ref_axis',(1.,0.,0.));
#111996=DIRECTION('',(0.,0.,-1.));
#111997=DIRECTION('center_axis',(0.,0.,-1.));
#111998=DIRECTION('ref_axis',(-1.,0.,0.));
#111999=DIRECTION('center_axis',(0.,0.,1.));
#112000=DIRECTION('ref_axis',(1.,0.,0.));
#112001=DIRECTION('',(0.,0.,-1.));
#112002=DIRECTION('center_axis',(0.,0.,1.));
#112003=DIRECTION('ref_axis',(1.,0.,0.));
#112004=DIRECTION('',(0.,0.,-1.));
#112005=DIRECTION('center_axis',(0.,0.,1.));
#112006=DIRECTION('ref_axis',(1.,0.,0.));
#112007=DIRECTION('',(0.,0.,-1.));
#112008=DIRECTION('center_axis',(0.,0.,1.));
#112009=DIRECTION('ref_axis',(1.,0.,0.));
#112010=DIRECTION('',(0.,0.,-1.));
#112011=DIRECTION('center_axis',(0.,0.,1.));
#112012=DIRECTION('ref_axis',(1.,0.,0.));
#112013=DIRECTION('',(0.,0.,-1.));
#112014=DIRECTION('center_axis',(0.,0.,1.));
#112015=DIRECTION('ref_axis',(1.,0.,0.));
#112016=DIRECTION('',(0.,0.,-1.));
#112017=DIRECTION('center_axis',(0.,0.,1.));
#112018=DIRECTION('ref_axis',(1.,0.,0.));
#112019=DIRECTION('',(0.,0.,-1.));
#112020=DIRECTION('center_axis',(1.,-6.08557808619092E-15,0.));
#112021=DIRECTION('ref_axis',(6.08557808619092E-15,1.,0.));
#112022=DIRECTION('',(1.,-6.08557808619092E-15,0.));
#112023=DIRECTION('center_axis',(1.,-6.08557808619092E-15,0.));
#112024=DIRECTION('ref_axis',(6.08557808619092E-15,1.,0.));
#112025=DIRECTION('',(1.,-6.08557808619092E-15,0.));
#112026=DIRECTION('center_axis',(0.,-1.,0.));
#112027=DIRECTION('ref_axis',(0.,0.,-1.));
#112028=DIRECTION('',(0.,-1.,0.));
#112029=DIRECTION('center_axis',(0.,-1.,0.));
#112030=DIRECTION('ref_axis',(0.,0.,-1.));
#112031=DIRECTION('',(0.,-1.,0.));
#112032=DIRECTION('center_axis',(0.,0.,1.));
#112033=DIRECTION('ref_axis',(1.,0.,0.));
#112034=DIRECTION('',(0.,0.,-1.));
#112035=DIRECTION('center_axis',(0.,1.21968337170492E-16,-1.));
#112036=DIRECTION('ref_axis',(0.,1.,1.21968337170492E-16));
#112037=DIRECTION('center_axis',(0.,0.,1.));
#112038=DIRECTION('ref_axis',(-1.,0.,0.));
#112039=DIRECTION('center_axis',(0.,1.21968337170492E-16,-1.));
#112040=DIRECTION('ref_axis',(0.,1.,1.21968337170492E-16));
#112041=DIRECTION('center_axis',(0.,1.21968337170492E-16,-1.));
#112042=DIRECTION('ref_axis',(0.,1.,1.21968337170492E-16));
#112043=DIRECTION('',(0.,1.21968337170492E-16,-1.));
#112044=DIRECTION('',(0.,1.21968337170492E-16,-1.));
#112045=DIRECTION('center_axis',(0.,0.,-1.));
#112046=DIRECTION('ref_axis',(-1.,0.,0.));
#112047=DIRECTION('center_axis',(-1.33967923098245E-7,-2.70052261735722E-8,
-0.999999999999991));
#112048=DIRECTION('ref_axis',(0.526776707081478,0.850003706389793,-9.352572372367E-8));
#112049=DIRECTION('',(0.,0.999447421660403,-0.0332393040897854));
#112050=DIRECTION('',(0.,-0.999447421660403,-0.0332393040897854));
#112051=DIRECTION('',(0.00929884004822234,0.99995676485224,0.));
#112052=DIRECTION('',(0.,-1.,0.));
#112053=DIRECTION('',(0.,1.,0.));
#112054=DIRECTION('center_axis',(-4.45046801311947E-10,1.54454672436889E-9,
-1.));
#112055=DIRECTION('ref_axis',(-0.292280983426921,0.956332487541332,1.60717892779798E-9));
#112056=DIRECTION('',(0.,0.,-1.));
#112057=DIRECTION('center_axis',(0.,0.,1.));
#112058=DIRECTION('ref_axis',(-2.97930117404573E-15,-1.,0.));
#112059=DIRECTION('center_axis',(2.58127960627592E-11,3.98865904338256E-9,
-1.));
#112060=DIRECTION('ref_axis',(0.00677738398148346,0.999977033269448,3.98874238015561E-9));
#112061=DIRECTION('center_axis',(1.,0.,0.));
#112062=DIRECTION('ref_axis',(0.,0.,-1.));
#112063=DIRECTION('center_axis',(0.,-1.21968337170492E-16,1.));
#112064=DIRECTION('ref_axis',(0.,-1.,-1.21968337170492E-16));
#112065=DIRECTION('center_axis',(0.,0.,-1.));
#112066=DIRECTION('ref_axis',(-1.,0.,0.));
#112067=DIRECTION('axis',(0.,0.,1.));
#112068=DIRECTION('refdir',(1.,0.,0.));
#112069=DIRECTION('center_axis',(0.,1.,0.));
#112070=DIRECTION('ref_axis',(0.,0.,1.));
#112071=DIRECTION('center_axis',(0.,1.,0.));
#112072=DIRECTION('ref_axis',(0.,0.,1.));
#112073=DIRECTION('center_axis',(1.,0.,-1.22464679914735E-16));
#112074=DIRECTION('ref_axis',(-1.22464679914735E-16,0.,-1.));
#112075=DIRECTION('center_axis',(0.,1.,0.));
#112076=DIRECTION('ref_axis',(0.,0.,1.));
#112077=DIRECTION('center_axis',(0.,1.,0.));
#112078=DIRECTION('ref_axis',(0.,0.,1.));
#112079=DIRECTION('center_axis',(0.,-1.,0.));
#112080=DIRECTION('ref_axis',(0.,0.,-1.));
#112081=DIRECTION('',(0.,1.,0.));
#112082=DIRECTION('',(0.,-1.,0.));
#112083=DIRECTION('center_axis',(0.,1.,0.));
#112084=DIRECTION('ref_axis',(0.,0.,-1.));
#112085=DIRECTION('center_axis',(0.,-1.,0.));
#112086=DIRECTION('ref_axis',(0.,0.,-1.));
#112087=DIRECTION('center_axis',(0.,1.,0.));
#112088=DIRECTION('ref_axis',(0.,0.,1.));
#112089=DIRECTION('center_axis',(0.,1.,0.));
#112090=DIRECTION('ref_axis',(0.,0.,1.));
#112091=DIRECTION('',(0.,-1.,0.));
#112092=DIRECTION('center_axis',(0.,1.,0.));
#112093=DIRECTION('ref_axis',(0.,0.,1.));
#112094=DIRECTION('center_axis',(0.,-1.,0.));
#112095=DIRECTION('ref_axis',(0.,0.,1.));
#112096=DIRECTION('center_axis',(0.,1.,0.));
#112097=DIRECTION('ref_axis',(0.,0.,1.));
#112098=DIRECTION('center_axis',(0.,1.,0.));
#112099=DIRECTION('ref_axis',(0.,0.,1.));
#112100=DIRECTION('center_axis',(0.,-1.,0.));
#112101=DIRECTION('ref_axis',(0.,0.,-1.));
#112102=DIRECTION('center_axis',(0.,1.,0.));
#112103=DIRECTION('ref_axis',(0.,0.,1.));
#112104=DIRECTION('center_axis',(0.,1.,0.));
#112105=DIRECTION('ref_axis',(0.,0.,1.));
#112106=DIRECTION('center_axis',(0.,1.,0.));
#112107=DIRECTION('ref_axis',(0.,0.,1.));
#112108=DIRECTION('',(1.1501184830626E-16,0.343526423752935,-0.939143011571464));
#112109=DIRECTION('center_axis',(0.,1.,0.));
#112110=DIRECTION('ref_axis',(0.,0.,1.));
#112111=DIRECTION('center_axis',(0.,1.,0.));
#112112=DIRECTION('ref_axis',(0.,0.,1.));
#112113=DIRECTION('center_axis',(-1.,0.,7.36451384826826E-15));
#112114=DIRECTION('ref_axis',(-6.98296267768626E-15,0.,-1.));
#112115=DIRECTION('center_axis',(0.,1.,0.));
#112116=DIRECTION('ref_axis',(0.,0.,1.));
#112117=DIRECTION('center_axis',(0.,1.,0.));
#112118=DIRECTION('ref_axis',(0.,0.,1.));
#112119=DIRECTION('center_axis',(0.,1.,0.));
#112120=DIRECTION('ref_axis',(0.,0.,1.));
#112121=DIRECTION('center_axis',(0.,1.,0.));
#112122=DIRECTION('ref_axis',(0.,0.,1.));
#112123=DIRECTION('center_axis',(-1.,0.,1.22464679914735E-16));
#112124=DIRECTION('ref_axis',(-1.22464679914735E-16,0.,-1.));
#112125=DIRECTION('center_axis',(0.,-1.,0.));
#112126=DIRECTION('ref_axis',(0.,0.,-1.));
#112127=DIRECTION('',(4.24471087982595E-17,0.938010460718684,-0.34660694681775));
#112128=DIRECTION('center_axis',(0.,1.,0.));
#112129=DIRECTION('ref_axis',(0.,0.,1.));
#112130=DIRECTION('center_axis',(0.,1.,0.));
#112131=DIRECTION('ref_axis',(0.,0.,1.));
#112132=DIRECTION('center_axis',(0.,1.,0.));
#112133=DIRECTION('ref_axis',(0.,0.,1.));
#112134=DIRECTION('center_axis',(0.,1.,0.));
#112135=DIRECTION('ref_axis',(0.,0.,1.));
#112136=DIRECTION('center_axis',(-1.,0.,1.22464679914735E-16));
#112137=DIRECTION('ref_axis',(-1.22464679914735E-16,0.,-1.));
#112138=DIRECTION('center_axis',(0.,1.,0.));
#112139=DIRECTION('ref_axis',(0.,0.,1.));
#112140=DIRECTION('center_axis',(0.,1.,0.));
#112141=DIRECTION('ref_axis',(0.,0.,1.));
#112142=DIRECTION('',(0.,1.,0.));
#112143=DIRECTION('center_axis',(0.,1.,0.));
#112144=DIRECTION('ref_axis',(0.,0.,1.));
#112145=DIRECTION('center_axis',(0.,1.,0.));
#112146=DIRECTION('ref_axis',(0.,0.,1.));
#112147=DIRECTION('center_axis',(0.,1.,0.));
#112148=DIRECTION('ref_axis',(0.,0.,1.));
#112149=DIRECTION('center_axis',(0.,-1.,0.));
#112150=DIRECTION('ref_axis',(-1.65389215948552E-15,0.,-1.));
#112151=DIRECTION('center_axis',(0.,-1.,0.));
#112152=DIRECTION('ref_axis',(0.,0.,1.));
#112153=DIRECTION('center_axis',(0.,-1.,0.));
#112154=DIRECTION('ref_axis',(0.,0.,1.));
#112155=DIRECTION('center_axis',(0.,-1.,0.));
#112156=DIRECTION('ref_axis',(0.,0.,1.));
#112157=DIRECTION('center_axis',(0.,-1.,0.));
#112158=DIRECTION('ref_axis',(0.,0.,1.));
#112159=DIRECTION('center_axis',(0.,-1.,0.));
#112160=DIRECTION('ref_axis',(0.,0.,-1.));
#112161=DIRECTION('center_axis',(0.,-1.,0.));
#112162=DIRECTION('ref_axis',(0.,0.,-1.));
#112163=DIRECTION('center_axis',(0.,-1.,0.));
#112164=DIRECTION('ref_axis',(0.,0.,-1.));
#112165=DIRECTION('center_axis',(0.,-1.,0.));
#112166=DIRECTION('ref_axis',(0.,0.,-1.));
#112167=DIRECTION('center_axis',(0.,-1.,0.));
#112168=DIRECTION('ref_axis',(0.,0.,-1.));
#112169=DIRECTION('center_axis',(0.,-1.,0.));
#112170=DIRECTION('ref_axis',(0.,0.,-1.));
#112171=DIRECTION('center_axis',(0.,-1.,0.));
#112172=DIRECTION('ref_axis',(0.,0.,-1.));
#112173=DIRECTION('center_axis',(0.,1.,0.));
#112174=DIRECTION('ref_axis',(0.,0.,-1.));
#112175=DIRECTION('center_axis',(0.,1.,0.));
#112176=DIRECTION('ref_axis',(0.,0.,-1.));
#112177=DIRECTION('center_axis',(0.,1.,0.));
#112178=DIRECTION('ref_axis',(1.01064309961486E-15,0.,1.));
#112179=DIRECTION('center_axis',(0.,1.,0.));
#112180=DIRECTION('ref_axis',(0.,0.,-1.));
#112181=DIRECTION('center_axis',(0.,1.,0.));
#112182=DIRECTION('ref_axis',(0.,0.,-1.));
#112183=DIRECTION('center_axis',(0.5,0.,-0.866025403784439));
#112184=DIRECTION('ref_axis',(-0.866025403784439,0.,-0.5));
#112185=DIRECTION('',(0.,-1.,0.));
#112186=DIRECTION('center_axis',(1.,0.,0.));
#112187=DIRECTION('ref_axis',(0.,0.,-1.));
#112188=DIRECTION('',(0.,1.,0.));
#112189=DIRECTION('',(0.,-1.,0.));
#112190=DIRECTION('center_axis',(0.5,0.,0.866025403784439));
#112191=DIRECTION('ref_axis',(0.866025403784439,0.,-0.5));
#112192=DIRECTION('',(0.,1.,0.));
#112193=DIRECTION('',(0.,-1.,0.));
#112194=DIRECTION('center_axis',(-0.499999999999999,0.,0.866025403784439));
#112195=DIRECTION('ref_axis',(0.866025403784439,0.,0.499999999999999));
#112196=DIRECTION('',(0.,-1.,0.));
#112197=DIRECTION('',(0.,1.,0.));
#112198=DIRECTION('center_axis',(-1.,0.,0.));
#112199=DIRECTION('ref_axis',(0.,0.,1.));
#112200=DIRECTION('',(0.,-1.,0.));
#112201=DIRECTION('',(0.,1.,0.));
#112202=DIRECTION('center_axis',(-0.5,0.,-0.866025403784439));
#112203=DIRECTION('ref_axis',(-0.866025403784439,0.,0.5));
#112204=DIRECTION('',(0.,1.,0.));
#112205=DIRECTION('center_axis',(0.,-1.,0.));
#112206=DIRECTION('ref_axis',(0.,0.,-1.));
#112207=DIRECTION('center_axis',(0.,-1.,0.));
#112208=DIRECTION('ref_axis',(0.,0.,-1.));
#112209=DIRECTION('center_axis',(0.,-1.,0.));
#112210=DIRECTION('ref_axis',(0.,0.,-1.));
#112211=DIRECTION('center_axis',(0.,-1.,0.));
#112212=DIRECTION('ref_axis',(0.,0.,-1.));
#112213=DIRECTION('center_axis',(0.,-1.,0.));
#112214=DIRECTION('ref_axis',(1.89882151931499E-15,0.,1.));
#112215=DIRECTION('center_axis',(0.,0.,-1.));
#112216=DIRECTION('ref_axis',(-1.,0.,0.));
#112217=DIRECTION('center_axis',(0.,0.,1.));
#112218=DIRECTION('ref_axis',(1.,0.,0.));
#112219=DIRECTION('',(0.,0.,-1.));
#112220=DIRECTION('center_axis',(0.,0.,1.));
#112221=DIRECTION('ref_axis',(1.,0.,0.));
#112222=DIRECTION('center_axis',(0.,0.,-1.));
#112223=DIRECTION('ref_axis',(-1.,0.,0.));
#112224=DIRECTION('center_axis',(0.,0.,1.));
#112225=DIRECTION('ref_axis',(1.,0.,0.));
#112226=DIRECTION('',(0.,0.,1.));
#112227=DIRECTION('center_axis',(0.,0.,1.));
#112228=DIRECTION('ref_axis',(1.,0.,0.));
#112229=DIRECTION('center_axis',(0.,0.,1.));
#112230=DIRECTION('ref_axis',(1.,0.,0.));
#112231=DIRECTION('center_axis',(0.,0.,1.));
#112232=DIRECTION('ref_axis',(1.,0.,0.));
#112233=DIRECTION('center_axis',(0.,0.,-1.));
#112234=DIRECTION('ref_axis',(-1.,0.,0.));
#112235=DIRECTION('center_axis',(0.,0.,1.));
#112236=DIRECTION('ref_axis',(1.,0.,0.));
#112237=DIRECTION('',(0.,0.,-1.));
#112238=DIRECTION('center_axis',(0.,0.,1.));
#112239=DIRECTION('ref_axis',(1.,0.,0.));
#112240=DIRECTION('center_axis',(0.,0.,-1.));
#112241=DIRECTION('ref_axis',(-1.,0.,0.));
#112242=DIRECTION('center_axis',(0.,0.,1.));
#112243=DIRECTION('ref_axis',(1.,0.,0.));
#112244=DIRECTION('',(0.,0.,1.));
#112245=DIRECTION('center_axis',(0.,0.,1.));
#112246=DIRECTION('ref_axis',(1.,0.,0.));
#112247=DIRECTION('center_axis',(0.,0.,1.));
#112248=DIRECTION('ref_axis',(1.,0.,0.));
#112249=DIRECTION('center_axis',(0.,0.,1.));
#112250=DIRECTION('ref_axis',(1.,0.,0.));
#112251=DIRECTION('center_axis',(0.,0.,-1.));
#112252=DIRECTION('ref_axis',(-1.,0.,0.));
#112253=DIRECTION('center_axis',(0.,0.,1.));
#112254=DIRECTION('ref_axis',(1.,0.,0.));
#112255=DIRECTION('',(0.,0.,-1.));
#112256=DIRECTION('center_axis',(0.,0.,1.));
#112257=DIRECTION('ref_axis',(1.,0.,0.));
#112258=DIRECTION('center_axis',(0.,0.,-1.));
#112259=DIRECTION('ref_axis',(-1.,0.,0.));
#112260=DIRECTION('center_axis',(0.,0.,1.));
#112261=DIRECTION('ref_axis',(1.,0.,0.));
#112262=DIRECTION('',(0.,0.,1.));
#112263=DIRECTION('center_axis',(0.,0.,1.));
#112264=DIRECTION('ref_axis',(1.,0.,0.));
#112265=DIRECTION('center_axis',(0.,0.,1.));
#112266=DIRECTION('ref_axis',(1.,0.,0.));
#112267=DIRECTION('center_axis',(0.,0.,1.));
#112268=DIRECTION('ref_axis',(1.,0.,0.));
#112269=DIRECTION('center_axis',(0.,0.,-1.));
#112270=DIRECTION('ref_axis',(-1.,0.,0.));
#112271=DIRECTION('center_axis',(0.,0.,1.));
#112272=DIRECTION('ref_axis',(1.,0.,0.));
#112273=DIRECTION('',(0.,0.,-1.));
#112274=DIRECTION('center_axis',(0.,0.,1.));
#112275=DIRECTION('ref_axis',(1.,0.,0.));
#112276=DIRECTION('center_axis',(0.,0.,-1.));
#112277=DIRECTION('ref_axis',(-1.,0.,0.));
#112278=DIRECTION('center_axis',(0.,0.,1.));
#112279=DIRECTION('ref_axis',(1.,0.,0.));
#112280=DIRECTION('',(0.,0.,1.));
#112281=DIRECTION('center_axis',(0.,0.,1.));
#112282=DIRECTION('ref_axis',(1.,0.,0.));
#112283=DIRECTION('center_axis',(0.,0.,1.));
#112284=DIRECTION('ref_axis',(1.,0.,0.));
#112285=DIRECTION('center_axis',(0.,0.,1.));
#112286=DIRECTION('ref_axis',(1.,0.,0.));
#112287=DIRECTION('center_axis',(0.,0.,-1.));
#112288=DIRECTION('ref_axis',(-1.,0.,0.));
#112289=DIRECTION('center_axis',(0.,0.,-1.));
#112290=DIRECTION('ref_axis',(-1.,0.,0.));
#112291=DIRECTION('center_axis',(0.,0.,-1.));
#112292=DIRECTION('ref_axis',(-1.,0.,0.));
#112293=DIRECTION('center_axis',(-1.22464679914735E-16,-1.,0.));
#112294=DIRECTION('ref_axis',(1.,-1.22464679914735E-16,0.));
#112295=DIRECTION('center_axis',(0.,0.,1.));
#112296=DIRECTION('ref_axis',(-1.,0.,0.));
#112297=DIRECTION('center_axis',(0.,0.,-1.));
#112298=DIRECTION('ref_axis',(-1.,0.,0.));
#112299=DIRECTION('center_axis',(0.,0.,-1.));
#112300=DIRECTION('ref_axis',(-1.,0.,0.));
#112301=DIRECTION('center_axis',(-1.22464679914735E-16,-1.,0.));
#112302=DIRECTION('ref_axis',(1.,-1.22464679914735E-16,0.));
#112303=DIRECTION('center_axis',(0.,0.,1.));
#112304=DIRECTION('ref_axis',(-1.,0.,0.));
#112305=DIRECTION('center_axis',(0.,0.,1.));
#112306=DIRECTION('ref_axis',(-1.,0.,0.));
#112307=DIRECTION('center_axis',(0.,0.,1.));
#112308=DIRECTION('ref_axis',(1.,0.,0.));
#112309=DIRECTION('center_axis',(0.,0.,-1.));
#112310=DIRECTION('ref_axis',(-1.,0.,0.));
#112311=DIRECTION('',(0.,0.,-1.));
#112312=DIRECTION('center_axis',(0.,0.,1.));
#112313=DIRECTION('ref_axis',(1.,0.,0.));
#112314=DIRECTION('',(0.,0.,1.));
#112315=DIRECTION('center_axis',(0.,0.,1.));
#112316=DIRECTION('ref_axis',(-1.,0.,0.));
#112317=DIRECTION('center_axis',(0.,0.,-1.));
#112318=DIRECTION('ref_axis',(-1.,0.,0.));
#112319=DIRECTION('center_axis',(0.,0.,-1.));
#112320=DIRECTION('ref_axis',(-1.,0.,0.));
#112321=DIRECTION('center_axis',(0.,0.,-1.));
#112322=DIRECTION('ref_axis',(-1.,0.,0.));
#112323=DIRECTION('center_axis',(0.,0.,-1.));
#112324=DIRECTION('ref_axis',(-1.,0.,0.));
#112325=DIRECTION('center_axis',(-1.22464679914735E-16,-1.,0.));
#112326=DIRECTION('ref_axis',(1.,-1.22464679914735E-16,0.));
#112327=DIRECTION('center_axis',(0.,0.,1.));
#112328=DIRECTION('ref_axis',(-1.,0.,0.));
#112329=DIRECTION('center_axis',(0.,0.,1.));
#112330=DIRECTION('ref_axis',(-1.,0.,0.));
#112331=DIRECTION('center_axis',(0.,0.,-1.));
#112332=DIRECTION('ref_axis',(-1.,0.,0.));
#112333=DIRECTION('center_axis',(0.,0.,-1.));
#112334=DIRECTION('ref_axis',(-1.,0.,0.));
#112335=DIRECTION('center_axis',(0.,0.,-1.));
#112336=DIRECTION('ref_axis',(-1.,0.,0.));
#112337=DIRECTION('center_axis',(-1.22464679914735E-16,-1.,0.));
#112338=DIRECTION('ref_axis',(1.,-1.22464679914735E-16,0.));
#112339=DIRECTION('center_axis',(0.,0.,1.));
#112340=DIRECTION('ref_axis',(-1.,0.,0.));
#112341=DIRECTION('center_axis',(0.,0.,1.));
#112342=DIRECTION('ref_axis',(1.,0.,0.));
#112343=DIRECTION('center_axis',(0.,0.,-1.));
#112344=DIRECTION('ref_axis',(-1.,0.,0.));
#112345=DIRECTION('',(0.,0.,-1.));
#112346=DIRECTION('center_axis',(0.,0.,1.));
#112347=DIRECTION('ref_axis',(1.,0.,0.));
#112348=DIRECTION('',(0.,0.,1.));
#112349=DIRECTION('center_axis',(0.,0.,-1.));
#112350=DIRECTION('ref_axis',(-1.,0.,0.));
#112351=DIRECTION('center_axis',(0.,0.,-1.));
#112352=DIRECTION('ref_axis',(-1.,0.,0.));
#112353=DIRECTION('center_axis',(0.,0.,-1.));
#112354=DIRECTION('ref_axis',(-1.,0.,0.));
#112355=DIRECTION('center_axis',(0.,0.,1.));
#112356=DIRECTION('ref_axis',(1.,0.,0.));
#112357=DIRECTION('center_axis',(0.,0.,-1.));
#112358=DIRECTION('ref_axis',(-1.,0.,0.));
#112359=DIRECTION('',(0.,0.,1.));
#112360=DIRECTION('center_axis',(0.,0.,-1.));
#112361=DIRECTION('ref_axis',(-1.,0.,0.));
#112362=DIRECTION('center_axis',(0.,0.,1.));
#112363=DIRECTION('ref_axis',(1.,0.,0.));
#112364=DIRECTION('center_axis',(0.,0.,-1.));
#112365=DIRECTION('ref_axis',(-1.,0.,0.));
#112366=DIRECTION('',(0.,0.,-1.));
#112367=DIRECTION('center_axis',(0.,0.,-1.));
#112368=DIRECTION('ref_axis',(-1.,0.,0.));
#112369=DIRECTION('center_axis',(0.,0.,-1.));
#112370=DIRECTION('ref_axis',(-1.,0.,0.));
#112371=DIRECTION('center_axis',(0.,0.,-1.));
#112372=DIRECTION('ref_axis',(-1.,0.,0.));
#112373=DIRECTION('center_axis',(-1.40816906889909E-16,1.4081690688991E-16,
-1.));
#112374=DIRECTION('ref_axis',(0.,1.,1.20114286872534E-16));
#112375=DIRECTION('center_axis',(-1.40816906889909E-16,1.4081690688991E-16,
-1.));
#112376=DIRECTION('ref_axis',(3.27616581394039E-33,1.,1.4081690688991E-16));
#112377=DIRECTION('center_axis',(0.99999996667151,0.00025818012795372,-1.60069213043897E-16));
#112378=DIRECTION('ref_axis',(-0.00025818012795372,0.99999996667151,1.41824142545828E-33));
#112379=DIRECTION('center_axis',(1.4081690688991E-16,0.,1.));
#112380=DIRECTION('ref_axis',(-1.,-4.05186995067197E-12,1.4081690688991E-16));
#112381=DIRECTION('center_axis',(0.99999996667151,-0.000258180127974661,
-1.33391010869915E-16));
#112382=DIRECTION('ref_axis',(0.000258180127974661,0.99999996667151,-9.76420164963656E-34));
#112383=DIRECTION('center_axis',(-1.40816906889909E-16,1.4081690688991E-16,
-1.));
#112384=DIRECTION('ref_axis',(0.,1.,1.12832121675104E-16));
#112385=DIRECTION('center_axis',(-1.4081690688991E-16,0.,-1.));
#112386=DIRECTION('ref_axis',(1.,4.31477076290321E-12,-1.4081690688991E-16));
#112387=DIRECTION('center_axis',(0.999999970597889,0.000242495818320685,
-1.46730112533024E-16));
#112388=DIRECTION('ref_axis',(-0.000242495818320685,0.999999970597889,8.35021668118118E-34));
#112389=DIRECTION('center_axis',(1.40816906889909E-16,-1.4081690688991E-16,
1.));
#112390=DIRECTION('ref_axis',(9.00257646208047E-12,1.,1.40816906888643E-16));
#112391=DIRECTION('center_axis',(0.999999970597889,-0.000242495818341616,
-1.73408314811756E-16));
#112392=DIRECTION('ref_axis',(0.000242495818341616,0.999999970597889,9.96645830604188E-34));
#112393=DIRECTION('center_axis',(-2.81633813779821E-16,0.,-1.));
#112394=DIRECTION('ref_axis',(-1.,0.,2.40228573745067E-16));
#112395=DIRECTION('center_axis',(-2.81633813779821E-16,0.,-1.));
#112396=DIRECTION('ref_axis',(-1.,0.,2.81633813779821E-16));
#112397=DIRECTION('center_axis',(-0.00025818012796419,0.99999996667151,
7.670762046674E-19));
#112398=DIRECTION('ref_axis',(-0.99999996667151,-0.00025818012796419,4.77318454276342E-36));
#112399=DIRECTION('center_axis',(1.4081690688991E-16,0.,1.));
#112400=DIRECTION('ref_axis',(-1.,-2.90079071874061E-12,1.4081690688991E-16));
#112401=DIRECTION('center_axis',(0.00025818012796419,0.99999996667151,-7.670762046674E-19));
#112402=DIRECTION('ref_axis',(-0.99999996667151,0.00025818012796419,4.77318454276342E-36));
#112403=DIRECTION('center_axis',(-2.81633813779821E-16,0.,-1.));
#112404=DIRECTION('ref_axis',(-1.,0.,2.25664243350207E-16));
#112405=DIRECTION('center_axis',(-1.4081690688991E-16,0.,-1.));
#112406=DIRECTION('ref_axis',(1.,0.,-1.4081690688991E-16));
#112407=DIRECTION('center_axis',(-0.000242495818331158,0.999999970597889,
0.));
#112408=DIRECTION('ref_axis',(-0.999999970597889,-0.000242495818331158,
0.));
#112409=DIRECTION('center_axis',(2.81633813779821E-16,0.,1.));
#112410=DIRECTION('ref_axis',(-1.,-9.2414964569798E-12,2.81633813779821E-16));
#112411=DIRECTION('center_axis',(0.00024249581833115,0.999999970597889,
-1.33391011393658E-17));
#112412=DIRECTION('ref_axis',(-0.999999970597889,0.00024249581833115,2.11314776580936E-36));
#112413=DIRECTION('center_axis',(-1.4081690688991E-16,0.,-1.));
#112414=DIRECTION('ref_axis',(1.,0.,-1.4081690688991E-16));
#112415=DIRECTION('center_axis',(-1.4081690688991E-16,0.,-1.));
#112416=DIRECTION('ref_axis',(-1.,0.,1.20729796120972E-16));
#112417=DIRECTION('center_axis',(-1.4081690688991E-16,0.,-1.));
#112418=DIRECTION('ref_axis',(-1.,0.,1.4081690688991E-16));
#112419=DIRECTION('center_axis',(-1.22464679914735E-16,-1.,1.7245097428856E-32));
#112420=DIRECTION('ref_axis',(1.,-1.22464679914735E-16,-1.50912245151216E-16));
#112421=DIRECTION('center_axis',(1.4081690688991E-16,0.,1.));
#112422=DIRECTION('ref_axis',(-1.,0.,1.4081690688991E-16));
#112423=DIRECTION('center_axis',(1.4081690688991E-16,0.,1.));
#112424=DIRECTION('ref_axis',(-1.,0.,1.4081690688991E-16));
#112425=DIRECTION('center_axis',(-1.4081690688991E-16,0.,-1.));
#112426=DIRECTION('ref_axis',(-1.,0.,1.20546251308204E-16));
#112427=DIRECTION('center_axis',(-1.4081690688991E-16,0.,-1.));
#112428=DIRECTION('ref_axis',(1.,0.,-1.4081690688991E-16));
#112429=DIRECTION('center_axis',(-1.22464679914735E-16,-1.,1.7245097428856E-32));
#112430=DIRECTION('ref_axis',(1.,-1.22464679914735E-16,-1.50682814135255E-16));
#112431=DIRECTION('center_axis',(1.4081690688991E-16,0.,1.));
#112432=DIRECTION('ref_axis',(-1.,0.,1.40816906889911E-16));
#112433=DIRECTION('center_axis',(-1.4081690688991E-16,0.,-1.));
#112434=DIRECTION('ref_axis',(-1.,0.,1.10673987086231E-16));
#112435=DIRECTION('center_axis',(-1.4081690688991E-16,0.,-1.));
#112436=DIRECTION('ref_axis',(-1.,0.,1.4081690688991E-16));
#112437=DIRECTION('center_axis',(-1.22464679914735E-16,-1.,1.7245097428856E-32));
#112438=DIRECTION('ref_axis',(1.,-1.22464679914735E-16,-1.38342483857788E-16));
#112439=DIRECTION('center_axis',(1.4081690688991E-16,0.,1.));
#112440=DIRECTION('ref_axis',(-1.,0.,1.40816906889911E-16));
#112441=DIRECTION('center_axis',(1.4081690688991E-16,0.,1.));
#112442=DIRECTION('ref_axis',(-1.,0.,1.40816906889911E-16));
#112443=DIRECTION('center_axis',(-1.4081690688991E-16,0.,-1.));
#112444=DIRECTION('ref_axis',(-1.,0.,1.10519724968194E-16));
#112445=DIRECTION('center_axis',(-1.4081690688991E-16,0.,-1.));
#112446=DIRECTION('ref_axis',(1.,0.,-1.4081690688991E-16));
#112447=DIRECTION('center_axis',(-1.22464679914735E-16,-1.,1.7245097428856E-32));
#112448=DIRECTION('ref_axis',(1.,-1.22464679914735E-16,-1.38149656210243E-16));
#112449=DIRECTION('center_axis',(1.4081690688991E-16,0.,1.));
#112450=DIRECTION('ref_axis',(-1.,0.,1.40816906889911E-16));
#112451=DIRECTION('center_axis',(-1.4081690688991E-16,0.,-1.));
#112452=DIRECTION('ref_axis',(-1.,0.,1.4081690688991E-16));
#112453=DIRECTION('center_axis',(-1.4081690688991E-16,0.,-1.));
#112454=DIRECTION('ref_axis',(-1.,0.,1.4081690688991E-16));
#112455=DIRECTION('',(1.4081690688991E-16,0.,1.));
#112456=DIRECTION('center_axis',(-1.4081690688991E-16,0.,-1.));
#112457=DIRECTION('ref_axis',(-1.,0.,1.4081690688991E-16));
#112458=DIRECTION('center_axis',(-1.4081690688991E-16,0.,-1.));
#112459=DIRECTION('ref_axis',(-1.,0.,1.4081690688991E-16));
#112460=DIRECTION('',(-0.529919264233199,6.48963930749707E-17,0.84804809615643));
#112461=DIRECTION('center_axis',(1.4081690688991E-16,0.,1.));
#112462=DIRECTION('ref_axis',(1.,0.,-1.4081690688991E-16));
#112463=DIRECTION('center_axis',(-1.4081690688991E-16,0.,-1.));
#112464=DIRECTION('ref_axis',(1.,0.,-1.4081690688991E-16));
#112465=DIRECTION('',(-0.529924202082878,-4.6420044039426E-6,-0.848045010612808));
#112466=DIRECTION('center_axis',(-1.4081690688991E-16,0.,-1.));
#112467=DIRECTION('ref_axis',(1.,0.,-1.4081690688991E-16));
#112468=DIRECTION('',(0.527020736635428,-0.0553967790670814,0.848045010612788));
#112469=DIRECTION('center_axis',(-1.4081690688991E-16,0.,-1.));
#112470=DIRECTION('ref_axis',(1.,6.21724893790088E-15,-1.4081690688991E-16));
#112471=DIRECTION('',(-0.527021707078575,0.0553875459170483,-0.848045010612805));
#112472=DIRECTION('center_axis',(-1.4081690688991E-16,0.,-1.));
#112473=DIRECTION('ref_axis',(1.,0.,-1.4081690688991E-16));
#112474=DIRECTION('',(0.518343121711168,-0.11018197742578,0.848045010612801));
#112475=DIRECTION('center_axis',(-1.4081690688991E-16,0.,-1.));
#112476=DIRECTION('ref_axis',(1.,1.24344978758018E-14,-1.4081690688991E-16));
#112477=DIRECTION('',(-0.51834505196515,0.110172896294841,-0.848045010612793));
#112478=DIRECTION('center_axis',(-1.4081690688991E-16,0.,-1.));
#112479=DIRECTION('ref_axis',(1.,0.,-1.4081690688991E-16));
#112480=DIRECTION('',(0.50398643107519,-0.163759998982733,0.848045010612802));
#112481=DIRECTION('center_axis',(-1.4081690688991E-16,0.,-1.));
#112482=DIRECTION('ref_axis',(1.,0.,-1.4081690688991E-16));
#112483=DIRECTION('',(-0.503989299991689,0.163751169365661,-0.848045010612801));
#112484=DIRECTION('center_axis',(-1.4081690688991E-16,0.,-1.));
#112485=DIRECTION('ref_axis',(1.,0.,-1.4081690688991E-16));
#112486=DIRECTION('',(0.484107959634419,-0.215543831721857,0.848045010612797));
#112487=DIRECTION('center_axis',(-1.4081690688991E-16,0.,-1.));
#112488=DIRECTION('ref_axis',(1.,4.79616346638068E-14,-1.4081690688991E-16));
#112489=DIRECTION('',(-0.484111735780994,0.215535350357782,-0.848045010612798));
#112490=DIRECTION('center_axis',(-1.4081690688991E-16,0.,-1.));
#112491=DIRECTION('ref_axis',(1.,8.88178419700125E-16,-1.4081690688991E-16));
#112492=DIRECTION('',(0.458925500081788,-0.26496612113519,0.848045010612793));
#112493=DIRECTION('center_axis',(-1.4081690688991E-16,0.,-1.));
#112494=DIRECTION('ref_axis',(1.,0.,-1.4081690688991E-16));
#112495=DIRECTION('',(-0.458930142086183,0.264958080947708,-0.8480450106128));
#112496=DIRECTION('center_axis',(-1.4081690688991E-16,0.,-1.));
#112497=DIRECTION('ref_axis',(1.,8.88178419700125E-16,-1.4081690688991E-16));
#112498=DIRECTION('',(0.428714956713914,-0.311485386277621,0.848045010612803));
#112499=DIRECTION('center_axis',(-1.4081690688991E-16,0.,-1.));
#112500=DIRECTION('ref_axis',(1.,0.,-1.4081690688991E-16));
#112501=DIRECTION('',(-0.428720413717376,0.311477875356734,-0.848045010612796));
#112502=DIRECTION('center_axis',(-1.4081690688991E-16,0.,-1.));
#112503=DIRECTION('ref_axis',(1.,8.88178419700125E-16,-1.4081690688991E-16));
#112504=DIRECTION('',(0.393807322565914,-0.354591952345506,0.848045010612802));
#112505=DIRECTION('center_axis',(-1.4081690688991E-16,0.,-1.));
#112506=DIRECTION('ref_axis',(1.,0.,-1.4081690688991E-16));
#112507=DIRECTION('',(-0.393813534780369,0.354585052982416,-0.848045010612791));
#112508=DIRECTION('center_axis',(-1.4081690688991E-16,0.,-1.));
#112509=DIRECTION('ref_axis',(1.,8.88178419700125E-16,-1.4081690688991E-16));
#112510=DIRECTION('',(0.354585052982406,-0.39381353478036,0.848045010612799));
#112511=DIRECTION('center_axis',(-1.4081690688991E-16,0.,-1.));
#112512=DIRECTION('ref_axis',(1.,0.,-1.4081690688991E-16));
#112513=DIRECTION('',(-0.354591952345518,0.393807322565912,-0.848045010612799));
#112514=DIRECTION('center_axis',(-1.4081690688991E-16,0.,-1.));
#112515=DIRECTION('ref_axis',(1.,8.88178419700125E-16,-1.4081690688991E-16));
#112516=DIRECTION('',(0.311477875356732,-0.428720413717355,0.848045010612807));
#112517=DIRECTION('center_axis',(-1.4081690688991E-16,0.,-1.));
#112518=DIRECTION('ref_axis',(1.,0.,-1.4081690688991E-16));
#112519=DIRECTION('',(-0.311485386277638,0.428714956713914,-0.848045010612796));
#112520=DIRECTION('center_axis',(-1.4081690688991E-16,0.,-1.));
#112521=DIRECTION('ref_axis',(1.,0.,-1.4081690688991E-16));
#112522=DIRECTION('',(0.264958080947704,-0.458930142086175,0.848045010612805));
#112523=DIRECTION('center_axis',(-1.4081690688991E-16,0.,-1.));
#112524=DIRECTION('ref_axis',(1.,0.,-1.4081690688991E-16));
#112525=DIRECTION('',(-0.264966121135182,0.45892550008177,-0.848045010612805));
#112526=DIRECTION('center_axis',(-1.4081690688991E-16,0.,-1.));
#112527=DIRECTION('ref_axis',(1.,0.,-1.4081690688991E-16));
#112528=DIRECTION('',(0.215535350357774,-0.484111735780989,0.848045010612803));
#112529=DIRECTION('center_axis',(-1.4081690688991E-16,0.,-1.));
#112530=DIRECTION('ref_axis',(1.,0.,-1.4081690688991E-16));
#112531=DIRECTION('',(-0.215543831721856,0.484107959634404,-0.848045010612807));
#112532=DIRECTION('center_axis',(-1.4081690688991E-16,0.,-1.));
#112533=DIRECTION('ref_axis',(1.,0.,-1.4081690688991E-16));
#112534=DIRECTION('',(0.163751169365657,-0.503989299991686,0.848045010612804));
#112535=DIRECTION('center_axis',(-1.4081690688991E-16,0.,-1.));
#112536=DIRECTION('ref_axis',(1.,0.,-1.4081690688991E-16));
#112537=DIRECTION('',(-0.163759998982741,0.503986431075192,-0.8480450106128));
#112538=DIRECTION('center_axis',(-1.4081690688991E-16,0.,-1.));
#112539=DIRECTION('ref_axis',(1.,0.,-1.4081690688991E-16));
#112540=DIRECTION('',(0.110172896294838,-0.518345051965138,0.848045010612801));
#112541=DIRECTION('center_axis',(-1.4081690688991E-16,0.,-1.));
#112542=DIRECTION('ref_axis',(1.,0.,-1.4081690688991E-16));
#112543=DIRECTION('',(-0.110181977425777,0.518343121711181,-0.848045010612794));
#112544=DIRECTION('center_axis',(-1.4081690688991E-16,0.,-1.));
#112545=DIRECTION('ref_axis',(1.,0.,-1.4081690688991E-16));
#112546=DIRECTION('',(0.055387545917043,-0.527021707078587,0.848045010612797));
#112547=DIRECTION('center_axis',(-1.4081690688991E-16,0.,-1.));
#112548=DIRECTION('ref_axis',(1.,0.,-1.4081690688991E-16));
#112549=DIRECTION('',(-0.0553967790670791,0.527020736635425,-0.84804501061279));
#112550=DIRECTION('center_axis',(-1.4081690688991E-16,0.,-1.));
#112551=DIRECTION('ref_axis',(1.,0.,-1.4081690688991E-16));
#112552=DIRECTION('',(-4.64200440569703E-6,-0.529924202082903,0.848045010612792));
#112553=DIRECTION('center_axis',(-1.4081690688991E-16,0.,-1.));
#112554=DIRECTION('ref_axis',(1.,0.,-1.4081690688991E-16));
#112555=DIRECTION('',(-4.6420044022913E-6,0.529924202082884,-0.848045010612804));
#112556=DIRECTION('center_axis',(-1.4081690688991E-16,0.,-1.));
#112557=DIRECTION('ref_axis',(1.,0.,-1.4081690688991E-16));
#112558=DIRECTION('',(-0.0553967790670824,-0.527020736635424,0.84804501061279));
#112559=DIRECTION('center_axis',(-1.4081690688991E-16,0.,-1.));
#112560=DIRECTION('ref_axis',(1.,0.,-1.4081690688991E-16));
#112561=DIRECTION('',(0.0553875459170473,0.527021707078581,-0.848045010612801));
#112562=DIRECTION('center_axis',(-1.4081690688991E-16,0.,-1.));
#112563=DIRECTION('ref_axis',(1.,0.,-1.4081690688991E-16));
#112564=DIRECTION('',(-0.110181977425775,-0.518343121711175,0.848045010612798));
#112565=DIRECTION('center_axis',(-1.4081690688991E-16,0.,-1.));
#112566=DIRECTION('ref_axis',(1.,0.,-1.4081690688991E-16));
#112567=DIRECTION('',(0.110172896294838,0.518345051965151,-0.848045010612793));
#112568=DIRECTION('center_axis',(-1.4081690688991E-16,0.,-1.));
#112569=DIRECTION('ref_axis',(1.,0.,-1.4081690688991E-16));
#112570=DIRECTION('',(-0.163759998982731,-0.503986431075193,0.848045010612801));
#112571=DIRECTION('center_axis',(-1.4081690688991E-16,0.,-1.));
#112572=DIRECTION('ref_axis',(1.,0.,-1.4081690688991E-16));
#112573=DIRECTION('',(0.163751169365665,0.503989299991695,-0.848045010612797));
#112574=DIRECTION('center_axis',(-1.4081690688991E-16,0.,-1.));
#112575=DIRECTION('ref_axis',(1.,0.,-1.4081690688991E-16));
#112576=DIRECTION('',(-0.215543831721855,-0.484107959634416,0.848045010612799));
#112577=DIRECTION('center_axis',(-1.4081690688991E-16,0.,-1.));
#112578=DIRECTION('ref_axis',(1.,0.,-1.4081690688991E-16));
#112579=DIRECTION('',(0.215535350357775,0.484111735780992,-0.848045010612802));
#112580=DIRECTION('center_axis',(-1.4081690688991E-16,0.,-1.));
#112581=DIRECTION('ref_axis',(1.,-4.44089209850063E-15,-1.4081690688991E-16));
#112582=DIRECTION('',(-0.264966121135187,-0.458925500081781,0.848045010612798));
#112583=DIRECTION('center_axis',(-1.4081690688991E-16,0.,-1.));
#112584=DIRECTION('ref_axis',(1.,0.,-1.4081690688991E-16));
#112585=DIRECTION('',(0.264958080947722,0.458930142086184,-0.848045010612795));
#112586=DIRECTION('center_axis',(-1.4081690688991E-16,0.,-1.));
#112587=DIRECTION('ref_axis',(1.,0.,-1.4081690688991E-16));
#112588=DIRECTION('',(-0.31148538627764,-0.428714956713913,0.848045010612796));
#112589=DIRECTION('center_axis',(-1.4081690688991E-16,0.,-1.));
#112590=DIRECTION('ref_axis',(1.,2.01438865587988E-12,-1.4081690688991E-16));
#112591=DIRECTION('',(0.311477875356739,0.428720413717396,-0.848045010612783));
#112592=DIRECTION('center_axis',(-1.4081690688991E-16,0.,-1.));
#112593=DIRECTION('ref_axis',(1.,0.,-1.4081690688991E-16));
#112594=DIRECTION('',(-0.354591952345506,-0.393807322565927,0.848045010612796));
#112595=DIRECTION('center_axis',(-1.4081690688991E-16,0.,-1.));
#112596=DIRECTION('ref_axis',(1.,0.,-1.4081690688991E-16));
#112597=DIRECTION('',(0.354585052982408,0.393813534780362,-0.848045010612797));
#112598=DIRECTION('center_axis',(-1.4081690688991E-16,0.,-1.));
#112599=DIRECTION('ref_axis',(1.,0.,-1.4081690688991E-16));
#112600=DIRECTION('',(-0.393813534780346,-0.354585052982406,0.848045010612805));
#112601=DIRECTION('center_axis',(-1.4081690688991E-16,0.,-1.));
#112602=DIRECTION('ref_axis',(1.,-2.20534701611541E-12,-1.4081690688991E-16));
#112603=DIRECTION('',(0.393807322565923,0.354591952345502,-0.8480450106128));
#112604=DIRECTION('center_axis',(-1.4081690688991E-16,0.,-1.));
#112605=DIRECTION('ref_axis',(1.,1.15463194561016E-14,-1.4081690688991E-16));
#112606=DIRECTION('',(-0.428720413717367,-0.311477875356727,0.848045010612803));
#112607=DIRECTION('center_axis',(-1.4081690688991E-16,0.,-1.));
#112608=DIRECTION('ref_axis',(1.,0.,-1.4081690688991E-16));
#112609=DIRECTION('',(0.428714956713905,0.311485386277624,-0.848045010612805));
#112610=DIRECTION('center_axis',(-1.4081690688991E-16,0.,-1.));
#112611=DIRECTION('ref_axis',(1.,0.,-1.4081690688991E-16));
#112612=DIRECTION('',(-0.458930142086187,-0.264958080947698,0.848045010612801));
#112613=DIRECTION('center_axis',(-1.4081690688991E-16,0.,-1.));
#112614=DIRECTION('ref_axis',(1.,0.,-1.4081690688991E-16));
#112615=DIRECTION('',(0.458925500081769,0.264966121135188,-0.848045010612804));
#112616=DIRECTION('center_axis',(-1.4081690688991E-16,0.,-1.));
#112617=DIRECTION('ref_axis',(1.,0.,-1.4081690688991E-16));
#112618=DIRECTION('',(-0.484111735781008,-0.21553535035777,0.848045010612794));
#112619=DIRECTION('center_axis',(-1.4081690688991E-16,0.,-1.));
#112620=DIRECTION('ref_axis',(1.,0.,-1.4081690688991E-16));
#112621=DIRECTION('',(0.484107959634402,0.215543831721842,-0.848045010612811));
#112622=DIRECTION('center_axis',(-1.4081690688991E-16,0.,-1.));
#112623=DIRECTION('ref_axis',(1.,0.,-1.4081690688991E-16));
#112624=DIRECTION('',(-0.503989299991702,-0.163751169365651,0.848045010612795));
#112625=DIRECTION('center_axis',(-1.4081690688991E-16,0.,-1.));
#112626=DIRECTION('ref_axis',(1.,0.,-1.4081690688991E-16));
#112627=DIRECTION('',(0.503986431075198,0.163759998982739,-0.848045010612796));
#112628=DIRECTION('center_axis',(-1.4081690688991E-16,0.,-1.));
#112629=DIRECTION('ref_axis',(1.,0.,-1.4081690688991E-16));
#112630=DIRECTION('',(-0.518345051965132,-0.110172896294837,0.848045010612804));
#112631=DIRECTION('center_axis',(-1.4081690688991E-16,0.,-1.));
#112632=DIRECTION('ref_axis',(1.,0.,-1.4081690688991E-16));
#112633=DIRECTION('',(0.518343121711172,0.110181977425774,-0.8480450106128));
#112634=DIRECTION('center_axis',(-1.4081690688991E-16,0.,-1.));
#112635=DIRECTION('ref_axis',(1.,0.,-1.4081690688991E-16));
#112636=DIRECTION('',(-0.527021707078582,-0.0553875459170411,0.848045010612801));
#112637=DIRECTION('center_axis',(-1.4081690688991E-16,0.,-1.));
#112638=DIRECTION('ref_axis',(1.,0.,-1.4081690688991E-16));
#112639=DIRECTION('',(0.527020736635406,0.0553967790670803,-0.848045010612802));
#112640=DIRECTION('center_axis',(-1.4081690688991E-16,0.,-1.));
#112641=DIRECTION('ref_axis',(1.,0.,-1.4081690688991E-16));
#112642=DIRECTION('',(-0.529924202082894,4.64200440404571E-6,0.848045010612798));
#112643=DIRECTION('',(-0.529919264233196,-6.48963930749704E-17,0.848048096156432));
#112644=DIRECTION('',(0.529924202082894,4.64200440394251E-6,-0.848045010612798));
#112645=DIRECTION('center_axis',(-1.4081690688991E-16,0.,-1.));
#112646=DIRECTION('ref_axis',(1.,0.,-1.4081690688991E-16));
#112647=DIRECTION('',(-0.527020736635415,0.0553967790670848,0.848045010612796));
#112648=DIRECTION('center_axis',(-1.4081690688991E-16,0.,-1.));
#112649=DIRECTION('ref_axis',(1.,0.,-1.4081690688991E-16));
#112650=DIRECTION('',(0.527021707078572,-0.055387545917048,-0.848045010612806));
#112651=DIRECTION('center_axis',(-1.4081690688991E-16,0.,-1.));
#112652=DIRECTION('ref_axis',(1.,0.,-1.4081690688991E-16));
#112653=DIRECTION('',(-0.518343121711156,0.110181977425777,0.848045010612809));
#112654=DIRECTION('center_axis',(-1.4081690688991E-16,0.,-1.));
#112655=DIRECTION('ref_axis',(1.,0.,-1.4081690688991E-16));
#112656=DIRECTION('',(0.518345051965142,-0.110172896294836,-0.848045010612799));
#112657=DIRECTION('center_axis',(-1.4081690688991E-16,0.,-1.));
#112658=DIRECTION('ref_axis',(1.,0.,-1.4081690688991E-16));
#112659=DIRECTION('',(-0.503986431075197,0.163759998982742,0.848045010612796));
#112660=DIRECTION('center_axis',(-1.4081690688991E-16,0.,-1.));
#112661=DIRECTION('ref_axis',(1.,0.,-1.4081690688991E-16));
#112662=DIRECTION('',(0.503989299991692,-0.163751169365662,-0.848045010612799));
#112663=DIRECTION('center_axis',(-1.4081690688991E-16,0.,-1.));
#112664=DIRECTION('ref_axis',(1.,0.,-1.4081690688991E-16));
#112665=DIRECTION('',(-0.484107959634421,0.215543831721864,0.848045010612794));
#112666=DIRECTION('center_axis',(-1.4081690688991E-16,0.,-1.));
#112667=DIRECTION('ref_axis',(1.,0.,-1.4081690688991E-16));
#112668=DIRECTION('',(0.484111735780995,-0.215535350357796,-0.848045010612794));
#112669=DIRECTION('center_axis',(-1.4081690688991E-16,0.,-1.));
#112670=DIRECTION('ref_axis',(1.,0.,-1.4081690688991E-16));
#112671=DIRECTION('',(-0.45892550008179,0.264966121135192,0.848045010612791));
#112672=DIRECTION('center_axis',(-1.4081690688991E-16,0.,-1.));
#112673=DIRECTION('ref_axis',(1.,0.,-1.4081690688991E-16));
#112674=DIRECTION('',(0.458930142086184,-0.264958080947722,-0.848045010612795));
#112675=DIRECTION('center_axis',(-1.4081690688991E-16,0.,-1.));
#112676=DIRECTION('ref_axis',(1.,0.,-1.4081690688991E-16));
#112677=DIRECTION('',(-0.428714956713903,0.311485386277636,0.848045010612802));
#112678=DIRECTION('center_axis',(-1.4081690688991E-16,0.,-1.));
#112679=DIRECTION('ref_axis',(1.,0.,-1.4081690688991E-16));
#112680=DIRECTION('',(0.428720413717366,-0.311477875356733,-0.848045010612801));
#112681=DIRECTION('center_axis',(-1.4081690688991E-16,0.,-1.));
#112682=DIRECTION('ref_axis',(1.,0.,-1.4081690688991E-16));
#112683=DIRECTION('',(-0.393807322565926,0.354591952345518,0.848045010612792));
#112684=DIRECTION('center_axis',(-1.4081690688991E-16,0.,-1.));
#112685=DIRECTION('ref_axis',(1.,0.,-1.4081690688991E-16));
#112686=DIRECTION('',(0.393813534780356,-0.354585052982416,-0.848045010612797));
#112687=DIRECTION('center_axis',(-1.4081690688991E-16,0.,-1.));
#112688=DIRECTION('ref_axis',(1.,0.,-1.4081690688991E-16));
#112689=DIRECTION('',(-0.35458505298241,0.393813534780351,0.848045010612802));
#112690=DIRECTION('center_axis',(-1.4081690688991E-16,0.,-1.));
#112691=DIRECTION('ref_axis',(1.,0.,-1.4081690688991E-16));
#112692=DIRECTION('',(0.354591952345508,-0.393807322565916,-0.848045010612801));
#112693=DIRECTION('center_axis',(-1.4081690688991E-16,0.,-1.));
#112694=DIRECTION('ref_axis',(1.,0.,-1.4081690688991E-16));
#112695=DIRECTION('',(-0.311477875356733,0.428720413717371,0.848045010612799));
#112696=DIRECTION('center_axis',(-1.4081690688991E-16,0.,-1.));
#112697=DIRECTION('ref_axis',(1.,7.47846229387506E-12,-1.4081690688991E-16));
#112698=DIRECTION('',(0.311485386277631,-0.428714956713909,-0.848045010612801));
#112699=DIRECTION('center_axis',(-1.4081690688991E-16,0.,-1.));
#112700=DIRECTION('ref_axis',(1.,0.,-1.4081690688991E-16));
#112701=DIRECTION('',(-0.264958080947707,0.458930142086206,0.848045010612788));
#112702=DIRECTION('center_axis',(-1.4081690688991E-16,0.,-1.));
#112703=DIRECTION('ref_axis',(1.,3.83604259468484E-12,-1.4081690688991E-16));
#112704=DIRECTION('',(0.26496612113518,-0.458925500081792,-0.848045010612794));
#112705=DIRECTION('center_axis',(-1.4081690688991E-16,0.,-1.));
#112706=DIRECTION('ref_axis',(1.,-3.01980662698043E-14,-1.4081690688991E-16));
#112707=DIRECTION('',(-0.215535350357775,0.484111735780992,0.848045010612802));
#112708=DIRECTION('center_axis',(-1.4081690688991E-16,0.,-1.));
#112709=DIRECTION('ref_axis',(1.,-5.89750470680883E-12,-1.4081690688991E-16));
#112710=DIRECTION('',(0.21554383172186,-0.484107959634426,-0.848045010612793));
#112711=DIRECTION('center_axis',(-1.4081690688991E-16,0.,-1.));
#112712=DIRECTION('ref_axis',(1.,1.06581410364015E-14,-1.4081690688991E-16));
#112713=DIRECTION('',(-0.163751169365653,0.5039892999917,0.848045010612796));
#112714=DIRECTION('center_axis',(-1.4081690688991E-16,0.,-1.));
#112715=DIRECTION('ref_axis',(1.,-6.04050143238055E-12,-1.4081690688991E-16));
#112716=DIRECTION('',(0.163759998982731,-0.503986431075193,-0.848045010612801));
#112717=DIRECTION('center_axis',(-1.4081690688991E-16,0.,-1.));
#112718=DIRECTION('ref_axis',(1.,1.06581410364015E-14,-1.4081690688991E-16));
#112719=DIRECTION('',(-0.110172896294832,0.518345051965141,0.848045010612799));
#112720=DIRECTION('center_axis',(-1.4081690688991E-16,0.,-1.));
#112721=DIRECTION('ref_axis',(1.,-6.18438633637197E-12,-1.4081690688991E-16));
#112722=DIRECTION('',(0.11018197742577,-0.518343121711171,-0.848045010612801));
#112723=DIRECTION('center_axis',(-1.4081690688991E-16,0.,-1.));
#112724=DIRECTION('ref_axis',(1.,1.06581410364015E-14,-1.4081690688991E-16));
#112725=DIRECTION('',(-0.0553875459170391,0.527021707078581,0.848045010612801));
#112726=DIRECTION('center_axis',(-1.4081690688991E-16,0.,-1.));
#112727=DIRECTION('ref_axis',(1.,2.1094237467878E-12,-1.4081690688991E-16));
#112728=DIRECTION('',(0.0553967790670773,-0.527020736635409,-0.8480450106128));
#112729=DIRECTION('center_axis',(-1.4081690688991E-16,0.,-1.));
#112730=DIRECTION('ref_axis',(1.,-3.37507799486048E-14,-1.4081690688991E-16));
#112731=DIRECTION('',(4.64200440982517E-6,0.529924202082893,0.848045010612798));
#112732=DIRECTION('',(4.64200439836961E-6,-0.529924202082884,-0.848045010612804));
#112733=DIRECTION('center_axis',(-1.4081690688991E-16,0.,-1.));
#112734=DIRECTION('ref_axis',(1.,-3.37507799486048E-14,-1.4081690688991E-16));
#112735=DIRECTION('',(0.0553967790670853,0.527020736635434,0.848045010612784));
#112736=DIRECTION('center_axis',(-1.4081690688991E-16,0.,-1.));
#112737=DIRECTION('ref_axis',(1.,0.,-1.4081690688991E-16));
#112738=DIRECTION('',(-0.0553875459170506,-0.527021707078581,-0.848045010612801));
#112739=DIRECTION('center_axis',(-1.4081690688991E-16,0.,-1.));
#112740=DIRECTION('ref_axis',(1.,1.06581410364015E-14,-1.4081690688991E-16));
#112741=DIRECTION('',(0.110181977425778,0.518343121711174,0.848045010612798));
#112742=DIRECTION('center_axis',(-1.4081690688991E-16,0.,-1.));
#112743=DIRECTION('ref_axis',(1.,0.,-1.4081690688991E-16));
#112744=DIRECTION('',(-0.110172896294837,-0.518345051965147,-0.848045010612795));
#112745=DIRECTION('center_axis',(-1.4081690688991E-16,0.,-1.));
#112746=DIRECTION('ref_axis',(1.,0.,-1.4081690688991E-16));
#112747=DIRECTION('',(0.163759998982748,0.503986431075194,0.848045010612797));
#112748=DIRECTION('center_axis',(-1.4081690688991E-16,0.,-1.));
#112749=DIRECTION('ref_axis',(1.,0.,-1.4081690688991E-16));
#112750=DIRECTION('',(-0.163751169365666,-0.503989299991698,-0.848045010612795));
#112751=DIRECTION('center_axis',(-1.4081690688991E-16,0.,-1.));
#112752=DIRECTION('ref_axis',(1.,-3.5527136788005E-14,-1.4081690688991E-16));
#112753=DIRECTION('',(0.215543831721856,0.484107959634404,0.848045010612807));
#112754=DIRECTION('center_axis',(-1.4081690688991E-16,0.,-1.));
#112755=DIRECTION('ref_axis',(1.,2.34923192010683E-12,-1.4081690688991E-16));
#112756=DIRECTION('',(-0.215535350357785,-0.484111735780998,-0.848045010612796));
#112757=DIRECTION('center_axis',(-1.4081690688991E-16,0.,-1.));
#112758=DIRECTION('ref_axis',(1.,-3.5527136788005E-14,-1.4081690688991E-16));
#112759=DIRECTION('',(0.264966121135194,0.458925500081769,0.848045010612802));
#112760=DIRECTION('center_axis',(-1.4081690688991E-16,0.,-1.));
#112761=DIRECTION('ref_axis',(1.,0.,-1.4081690688991E-16));
#112762=DIRECTION('',(-0.264958080947704,-0.458930142086175,-0.848045010612805));
#112763=DIRECTION('center_axis',(-1.4081690688991E-16,0.,-1.));
#112764=DIRECTION('ref_axis',(1.,-4.2632564145606E-14,-1.4081690688991E-16));
#112765=DIRECTION('',(0.311485386277635,0.428714956713893,0.848045010612808));
#112766=DIRECTION('center_axis',(-1.4081690688991E-16,0.,-1.));
#112767=DIRECTION('ref_axis',(1.,2.44515518943444E-12,-1.4081690688991E-16));
#112768=DIRECTION('',(-0.311477875356743,-0.428720413717361,-0.8480450106128));
#112769=DIRECTION('center_axis',(-1.4081690688991E-16,0.,-1.));
#112770=DIRECTION('ref_axis',(1.,-2.48689957516035E-14,-1.4081690688991E-16));
#112771=DIRECTION('',(0.354591952345522,0.393807322565903,0.848045010612801));
#112772=DIRECTION('center_axis',(-1.4081690688991E-16,0.,-1.));
#112773=DIRECTION('ref_axis',(1.,-4.9862336481965E-12,-1.4081690688991E-16));
#112774=DIRECTION('',(-0.354585052982408,-0.393813534780349,-0.848045010612804));
#112775=DIRECTION('center_axis',(-1.4081690688991E-16,0.,-1.));
#112776=DIRECTION('ref_axis',(1.,0.,-1.4081690688991E-16));
#112777=DIRECTION('',(0.39381353478036,0.354585052982406,0.848045010612799));
#112778=DIRECTION('center_axis',(-1.4081690688991E-16,0.,-1.));
#112779=DIRECTION('ref_axis',(1.,1.27009514017118E-12,-1.4081690688991E-16));
#112780=DIRECTION('',(-0.393807322565912,-0.354591952345518,-0.848045010612799));
#112781=DIRECTION('center_axis',(-1.4081690688991E-16,0.,-1.));
#112782=DIRECTION('ref_axis',(1.,1.33226762955019E-14,-1.4081690688991E-16));
#112783=DIRECTION('',(0.428720413717364,0.311477875356725,0.848045010612805));
#112784=DIRECTION('center_axis',(-1.4081690688991E-16,0.,-1.));
#112785=DIRECTION('ref_axis',(1.,1.29407595750308E-12,-1.4081690688991E-16));
#112786=DIRECTION('',(-0.428714956713912,-0.311485386277633,-0.848045010612799));
#112787=DIRECTION('center_axis',(-1.4081690688991E-16,0.,-1.));
#112788=DIRECTION('ref_axis',(1.,-4.08562073062058E-14,-1.4081690688991E-16));
#112789=DIRECTION('',(0.458930142086183,0.264958080947708,0.8480450106128));
#112790=DIRECTION('center_axis',(-1.4081690688991E-16,0.,-1.));
#112791=DIRECTION('ref_axis',(1.,1.31805677483499E-12,-1.4081690688991E-16));
#112792=DIRECTION('',(-0.458925500081773,-0.264966121135183,-0.848045010612804));
#112793=DIRECTION('center_axis',(-1.4081690688991E-16,0.,-1.));
#112794=DIRECTION('ref_axis',(1.,9.76996261670138E-15,-1.4081690688991E-16));
#112795=DIRECTION('',(0.48411173578099,0.215535350357767,0.848045010612805));
#112796=DIRECTION('center_axis',(-1.4081690688991E-16,0.,-1.));
#112797=DIRECTION('ref_axis',(1.,2.01350047746018E-12,-1.4081690688991E-16));
#112798=DIRECTION('',(-0.484107959634414,-0.215543831721854,-0.848045010612801));
#112799=DIRECTION('center_axis',(-1.4081690688991E-16,0.,-1.));
#112800=DIRECTION('ref_axis',(1.,1.4210854715202E-14,-1.4081690688991E-16));
#112801=DIRECTION('',(0.503989299991708,0.163751169365662,0.848045010612789));
#112802=DIRECTION('center_axis',(-1.4081690688991E-16,0.,-1.));
#112803=DIRECTION('ref_axis',(1.,1.36601840949879E-12,-1.4081690688991E-16));
#112804=DIRECTION('',(-0.503986431075205,-0.163759998982731,-0.848045010612794));
#112805=DIRECTION('center_axis',(-1.4081690688991E-16,0.,-1.));
#112806=DIRECTION('ref_axis',(1.,1.24344978758018E-14,-1.4081690688991E-16));
#112807=DIRECTION('',(0.518345051965145,0.11017289629483,0.848045010612797));
#112808=DIRECTION('center_axis',(-1.4081690688991E-16,0.,-1.));
#112809=DIRECTION('ref_axis',(1.,2.78088663208109E-12,-1.4081690688991E-16));
#112810=DIRECTION('',(-0.518343121711179,-0.110181977425766,-0.848045010612796));
#112811=DIRECTION('center_axis',(-1.4081690688991E-16,0.,-1.));
#112812=DIRECTION('ref_axis',(1.,1.50990331349021E-14,-1.4081690688991E-16));
#112813=DIRECTION('',(0.527021707078575,0.0553875459170368,0.848045010612805));
#112814=DIRECTION('center_axis',(-1.4081690688991E-16,0.,-1.));
#112815=DIRECTION('ref_axis',(1.,2.65121258280487E-12,-1.4081690688991E-16));
#112816=DIRECTION('',(-0.527020736635419,-0.0553967790670736,-0.848045010612794));
#112817=DIRECTION('center_axis',(-1.4081690688991E-16,0.,-1.));
#112818=DIRECTION('ref_axis',(1.,2.8421709430404E-14,-1.4081690688991E-16));
#112819=DIRECTION('',(0.529924202082878,-4.64200440404581E-6,0.848045010612808));
#112820=DIRECTION('center_axis',(-1.4081690688991E-16,0.,-1.));
#112821=DIRECTION('ref_axis',(-1.,0.,1.4081690688991E-16));
#112822=DIRECTION('',(-0.529924689637704,-5.13655126081386E-6,-0.848044705947746));
#112823=DIRECTION('center_axis',(1.4081690688991E-16,0.,1.));
#112824=DIRECTION('ref_axis',(-1.,0.,1.4081690688991E-16));
#112825=DIRECTION('',(0.527022243656738,0.0553871050427197,0.848044705947749));
#112826=DIRECTION('center_axis',(1.4081690688991E-16,0.,1.));
#112827=DIRECTION('ref_axis',(-1.,0.,1.4081690688991E-16));
#112828=DIRECTION('',(-0.527021169825119,-0.0553973218681122,-0.848044705947749));
#112829=DIRECTION('center_axis',(1.4081690688991E-16,0.,1.));
#112830=DIRECTION('ref_axis',(-1.,0.,1.4081690688991E-16));
#112831=DIRECTION('',(0.518345631687774,0.110172513923361,0.848044705947752));
#112832=DIRECTION('center_axis',(1.4081690688991E-16,0.,1.));
#112833=DIRECTION('ref_axis',(-1.,-1.06581410364015E-14,1.4081690688991E-16));
#112834=DIRECTION('',(-0.51834349578966,-0.110182562533937,-0.848044705947753));
#112835=DIRECTION('center_axis',(1.4081690688991E-16,0.,1.));
#112836=DIRECTION('ref_axis',(-1.,0.,1.4081690688991E-16));
#112837=DIRECTION('',(0.503989916507264,0.163750849686365,0.848044705947744));
#112838=DIRECTION('center_axis',(1.4081690688991E-16,0.,1.));
#112839=DIRECTION('ref_axis',(-1.,-3.37507799486048E-14,1.4081690688991E-16));
#112840=DIRECTION('',(-0.503986741943991,-0.163760619987463,-0.848044705947748));
#112841=DIRECTION('center_axis',(1.4081690688991E-16,0.,1.));
#112842=DIRECTION('ref_axis',(-1.,0.,1.4081690688991E-16));
#112843=DIRECTION('',(0.484112382334809,0.215535096873149,0.848044705947745));
#112844=DIRECTION('center_axis',(1.4081690688991E-16,0.,1.));
#112845=DIRECTION('ref_axis',(-1.,4.52970994047064E-14,1.4081690688991E-16));
#112846=DIRECTION('',(-0.484108203887568,-0.215544481819287,-0.848044705947751));
#112847=DIRECTION('center_axis',(1.4081690688991E-16,0.,1.));
#112848=DIRECTION('ref_axis',(-1.,8.88178419700125E-16,1.4081690688991E-16));
#112849=DIRECTION('',(0.458930811594459,0.264957896434965,0.848044705947752));
#112850=DIRECTION('center_axis',(1.4081690688991E-16,0.,1.));
#112851=DIRECTION('ref_axis',(-1.,0.,1.4081690688991E-16));
#112852=DIRECTION('',(-0.458925675043201,-0.264966793202732,-0.848044705947748));
#112853=DIRECTION('center_axis',(1.4081690688991E-16,0.,1.));
#112854=DIRECTION('ref_axis',(-1.,8.88178419700125E-16,1.4081690688991E-16));
#112855=DIRECTION('',(0.428721098844843,0.311477761837432,0.848044705947755));
#112856=DIRECTION('center_axis',(1.4081690688991E-16,0.,1.));
#112857=DIRECTION('ref_axis',(-1.,0.,1.4081690688991E-16));
#112858=DIRECTION('',(-0.428715060466688,-0.311486072951955,-0.848044705947755));
#112859=DIRECTION('center_axis',(1.4081690688991E-16,0.,1.));
#112860=DIRECTION('ref_axis',(-1.,0.,1.4081690688991E-16));
#112861=DIRECTION('',(0.393814228020629,0.35458501170031,0.84804470594775));
#112862=DIRECTION('center_axis',(1.4081690688991E-16,0.,1.));
#112863=DIRECTION('ref_axis',(-1.,1.58095758706622E-13,1.4081690688991E-16));
#112864=DIRECTION('',(-0.393807353973302,-0.354592646103312,-0.848044705947745));
#112865=DIRECTION('center_axis',(1.4081690688991E-16,0.,1.));
#112866=DIRECTION('ref_axis',(-1.,0.,1.4081690688991E-16));
#112867=DIRECTION('',(0.354592646103303,0.393807353973298,0.848044705947751));
#112868=DIRECTION('center_axis',(1.4081690688991E-16,0.,1.));
#112869=DIRECTION('ref_axis',(-1.,0.,1.4081690688991E-16));
#112870=DIRECTION('',(-0.354585011700314,-0.39381422802064,-0.848044705947744));
#112871=DIRECTION('center_axis',(1.4081690688991E-16,0.,1.));
#112872=DIRECTION('ref_axis',(-1.,0.,1.4081690688991E-16));
#112873=DIRECTION('',(0.311486072951974,0.428715060466701,0.848044705947741));
#112874=DIRECTION('center_axis',(1.4081690688991E-16,0.,1.));
#112875=DIRECTION('ref_axis',(-1.,0.,1.4081690688991E-16));
#112876=DIRECTION('',(-0.311477761837448,-0.428721098844851,-0.848044705947745));
#112877=DIRECTION('center_axis',(1.4081690688991E-16,0.,1.));
#112878=DIRECTION('ref_axis',(-1.,0.,1.4081690688991E-16));
#112879=DIRECTION('',(0.264966793202734,0.458925675043206,0.848044705947745));
#112880=DIRECTION('center_axis',(1.4081690688991E-16,0.,1.));
#112881=DIRECTION('ref_axis',(-1.,0.,1.4081690688991E-16));
#112882=DIRECTION('',(-0.264957896434977,-0.458930811594472,-0.848044705947741));
#112883=DIRECTION('center_axis',(1.4081690688991E-16,0.,1.));
#112884=DIRECTION('ref_axis',(-1.,0.,1.4081690688991E-16));
#112885=DIRECTION('',(0.215544481819297,0.484108203887561,0.848044705947752));
#112886=DIRECTION('center_axis',(1.4081690688991E-16,0.,1.));
#112887=DIRECTION('ref_axis',(-1.,0.,1.4081690688991E-16));
#112888=DIRECTION('',(-0.215535096873163,-0.484112382334796,-0.848044705947749));
#112889=DIRECTION('center_axis',(1.4081690688991E-16,0.,1.));
#112890=DIRECTION('ref_axis',(-1.,0.,1.4081690688991E-16));
#112891=DIRECTION('',(0.163760619987462,0.503986741944001,0.848044705947743));
#112892=DIRECTION('center_axis',(1.4081690688991E-16,0.,1.));
#112893=DIRECTION('ref_axis',(-1.,0.,1.4081690688991E-16));
#112894=DIRECTION('',(-0.163750849686385,-0.50398991650724,-0.848044705947753));
#112895=DIRECTION('center_axis',(1.4081690688991E-16,0.,1.));
#112896=DIRECTION('ref_axis',(-1.,0.,1.4081690688991E-16));
#112897=DIRECTION('',(0.11018256253394,0.518343495789649,0.848044705947759));
#112898=DIRECTION('center_axis',(1.4081690688991E-16,0.,1.));
#112899=DIRECTION('ref_axis',(-1.,0.,1.4081690688991E-16));
#112900=DIRECTION('',(-0.110172513923363,-0.51834563168778,-0.848044705947748));
#112901=DIRECTION('center_axis',(1.4081690688991E-16,0.,1.));
#112902=DIRECTION('ref_axis',(-1.,0.,1.4081690688991E-16));
#112903=DIRECTION('',(0.0553973218681129,0.527021169825112,0.848044705947753));
#112904=DIRECTION('center_axis',(1.4081690688991E-16,0.,1.));
#112905=DIRECTION('ref_axis',(-1.,0.,1.4081690688991E-16));
#112906=DIRECTION('',(-0.0553871050427227,-0.527022243656735,-0.848044705947751));
#112907=DIRECTION('center_axis',(1.4081690688991E-16,0.,1.));
#112908=DIRECTION('ref_axis',(-1.,0.,1.4081690688991E-16));
#112909=DIRECTION('',(5.13655126277483E-6,0.529924689637704,0.848044705947746));
#112910=DIRECTION('center_axis',(1.4081690688991E-16,0.,1.));
#112911=DIRECTION('ref_axis',(-1.,0.,1.4081690688991E-16));
#112912=DIRECTION('',(5.13655125885311E-6,-0.529924689637701,-0.848044705947748));
#112913=DIRECTION('center_axis',(1.4081690688991E-16,0.,1.));
#112914=DIRECTION('ref_axis',(-1.,0.,1.4081690688991E-16));
#112915=DIRECTION('',(-0.0553871050427194,0.527022243656735,0.848044705947751));
#112916=DIRECTION('center_axis',(1.4081690688991E-16,0.,1.));
#112917=DIRECTION('ref_axis',(-1.,0.,1.4081690688991E-16));
#112918=DIRECTION('',(0.05539732186811,-0.527021169825103,-0.848044705947759));
#112919=DIRECTION('center_axis',(1.4081690688991E-16,0.,1.));
#112920=DIRECTION('ref_axis',(-1.,0.,1.4081690688991E-16));
#112921=DIRECTION('',(-0.110172513923355,0.518345631687787,0.848044705947745));
#112922=DIRECTION('center_axis',(1.4081690688991E-16,0.,1.));
#112923=DIRECTION('ref_axis',(-1.,0.,1.4081690688991E-16));
#112924=DIRECTION('',(0.110182562533938,-0.518343495789665,-0.848044705947749));
#112925=DIRECTION('center_axis',(1.4081690688991E-16,0.,1.));
#112926=DIRECTION('ref_axis',(-1.,0.,1.4081690688991E-16));
#112927=DIRECTION('',(-0.163750849686367,0.503989916507261,0.848044705947745));
#112928=DIRECTION('center_axis',(1.4081690688991E-16,0.,1.));
#112929=DIRECTION('ref_axis',(-1.,0.,1.4081690688991E-16));
#112930=DIRECTION('',(0.16376061998747,-0.503986741943981,-0.848044705947753));
#112931=DIRECTION('center_axis',(1.4081690688991E-16,0.,1.));
#112932=DIRECTION('ref_axis',(-1.,0.,1.4081690688991E-16));
#112933=DIRECTION('',(-0.215535096873147,0.484112382334806,0.848044705947747));
#112934=DIRECTION('center_axis',(1.4081690688991E-16,0.,1.));
#112935=DIRECTION('ref_axis',(-1.,0.,1.4081690688991E-16));
#112936=DIRECTION('',(0.215544481819295,-0.48410820388757,-0.848044705947748));
#112937=DIRECTION('center_axis',(1.4081690688991E-16,0.,1.));
#112938=DIRECTION('ref_axis',(-1.,5.32907051820075E-15,1.4081690688991E-16));
#112939=DIRECTION('',(-0.264957896434961,0.458930811594451,0.848044705947758));
#112940=DIRECTION('center_axis',(1.4081690688991E-16,0.,1.));
#112941=DIRECTION('ref_axis',(-1.,1.80122583515185E-12,1.4081690688991E-16));
#112942=DIRECTION('',(0.264966793202732,-0.458925675043203,-0.848044705947747));
#112943=DIRECTION('center_axis',(1.4081690688991E-16,0.,1.));
#112944=DIRECTION('ref_axis',(-1.,1.06581410364015E-14,1.4081690688991E-16));
#112945=DIRECTION('',(-0.311477761837441,0.428721098844847,0.84804470594775));
#112946=DIRECTION('center_axis',(1.4081690688991E-16,0.,1.));
#112947=DIRECTION('ref_axis',(-1.,-1.89182003396127E-12,1.4081690688991E-16));
#112948=DIRECTION('',(0.311486072951959,-0.428715060466685,-0.848044705947755));
#112949=DIRECTION('center_axis',(1.4081690688991E-16,0.,1.));
#112950=DIRECTION('ref_axis',(-1.,1.06581410364015E-14,1.4081690688991E-16));
#112951=DIRECTION('',(-0.354585011700304,0.393814228020636,0.84804470594775));
#112952=DIRECTION('center_axis',(1.4081690688991E-16,0.,1.));
#112953=DIRECTION('ref_axis',(-1.,0.,1.4081690688991E-16));
#112954=DIRECTION('',(0.354592646103297,-0.393807353973294,-0.848044705947755));
#112955=DIRECTION('center_axis',(1.4081690688991E-16,0.,1.));
#112956=DIRECTION('ref_axis',(-1.,0.,1.4081690688991E-16));
#112957=DIRECTION('',(-0.393807353973316,0.354592646103293,0.848044705947747));
#112958=DIRECTION('center_axis',(1.4081690688991E-16,0.,1.));
#112959=DIRECTION('ref_axis',(-1.,0.,1.4081690688991E-16));
#112960=DIRECTION('',(0.39381422802063,-0.354585011700304,-0.848044705947752));
#112961=DIRECTION('center_axis',(1.4081690688991E-16,0.,1.));
#112962=DIRECTION('ref_axis',(-1.,0.,1.4081690688991E-16));
#112963=DIRECTION('',(-0.428715060466685,0.311486072951973,0.848044705947749));
#112964=DIRECTION('center_axis',(1.4081690688991E-16,0.,1.));
#112965=DIRECTION('ref_axis',(-1.,2.1618262735501E-12,1.4081690688991E-16));
#112966=DIRECTION('',(0.428721098844842,-0.311477761837438,-0.848044705947753));
#112967=DIRECTION('center_axis',(1.4081690688991E-16,0.,1.));
#112968=DIRECTION('ref_axis',(-1.,0.,1.4081690688991E-16));
#112969=DIRECTION('',(-0.458925675043201,0.264966793202732,0.848044705947748));
#112970=DIRECTION('center_axis',(1.4081690688991E-16,0.,1.));
#112971=DIRECTION('ref_axis',(-1.,-2.25064411552012E-12,1.4081690688991E-16));
#112972=DIRECTION('',(0.458930811594463,-0.264957896434973,-0.848044705947748));
#112973=DIRECTION('center_axis',(1.4081690688991E-16,0.,1.));
#112974=DIRECTION('ref_axis',(-1.,0.,1.4081690688991E-16));
#112975=DIRECTION('',(-0.484108203887567,0.2155444818193,0.848044705947749));
#112976=DIRECTION('center_axis',(1.4081690688991E-16,0.,1.));
#112977=DIRECTION('ref_axis',(-1.,-2.34123831432953E-12,1.4081690688991E-16));
#112978=DIRECTION('',(0.484112382334804,-0.215535096873146,-0.848044705947749));
#112979=DIRECTION('center_axis',(1.4081690688991E-16,0.,1.));
#112980=DIRECTION('ref_axis',(-1.,0.,1.4081690688991E-16));
#112981=DIRECTION('',(-0.503986741943987,0.163760619987466,0.84804470594775));
#112982=DIRECTION('center_axis',(1.4081690688991E-16,0.,1.));
#112983=DIRECTION('ref_axis',(-1.,-2.43183251313894E-12,1.4081690688991E-16));
#112984=DIRECTION('',(0.503989916507253,-0.163750849686376,-0.848044705947748));
#112985=DIRECTION('center_axis',(1.4081690688991E-16,0.,1.));
#112986=DIRECTION('ref_axis',(-1.,0.,1.4081690688991E-16));
#112987=DIRECTION('',(-0.518343495789665,0.110182562533942,0.848044705947749));
#112988=DIRECTION('center_axis',(1.4081690688991E-16,0.,1.));
#112989=DIRECTION('ref_axis',(-1.,-2.52153853352866E-12,1.4081690688991E-16));
#112990=DIRECTION('',(0.518345631687777,-0.110172513923362,-0.84804470594775));
#112991=DIRECTION('center_axis',(1.4081690688991E-16,0.,1.));
#112992=DIRECTION('ref_axis',(-1.,0.,1.4081690688991E-16));
#112993=DIRECTION('',(-0.527021169825119,0.0553973218681105,0.848044705947749));
#112994=DIRECTION('center_axis',(1.4081690688991E-16,0.,1.));
#112995=DIRECTION('ref_axis',(-1.,0.,1.4081690688991E-16));
#112996=DIRECTION('',(0.527022243656741,-0.055387105042722,-0.848044705947747));
#112997=DIRECTION('center_axis',(1.4081690688991E-16,0.,1.));
#112998=DIRECTION('ref_axis',(-1.,0.,1.4081690688991E-16));
#112999=DIRECTION('',(-0.529924689637701,5.13655126091716E-6,0.848044705947748));
#113000=DIRECTION('center_axis',(1.4081690688991E-16,0.,1.));
#113001=DIRECTION('ref_axis',(-1.,0.,1.4081690688991E-16));
#113002=DIRECTION('',(-0.529919264233204,6.48963930749714E-17,0.848048096156427));
#113003=DIRECTION('center_axis',(1.4081690688991E-16,0.,1.));
#113004=DIRECTION('ref_axis',(-1.,0.,1.4081690688991E-16));
#113005=DIRECTION('',(0.529924689637701,5.13655126091716E-6,-0.848044705947748));
#113006=DIRECTION('center_axis',(1.4081690688991E-16,0.,1.));
#113007=DIRECTION('ref_axis',(-1.,0.,1.4081690688991E-16));
#113008=DIRECTION('',(-0.527022243656751,-0.055387105042715,0.848044705947742));
#113009=DIRECTION('center_axis',(1.4081690688991E-16,0.,1.));
#113010=DIRECTION('ref_axis',(-1.,0.,1.4081690688991E-16));
#113011=DIRECTION('',(0.527021169825119,0.0553973218681073,-0.848044705947749));
#113012=DIRECTION('center_axis',(1.4081690688991E-16,0.,1.));
#113013=DIRECTION('ref_axis',(-1.,0.,1.4081690688991E-16));
#113014=DIRECTION('',(-0.518345631687787,-0.110172513923358,0.848044705947744));
#113015=DIRECTION('center_axis',(1.4081690688991E-16,0.,1.));
#113016=DIRECTION('ref_axis',(-1.,0.,1.4081690688991E-16));
#113017=DIRECTION('',(0.518343495789666,0.110182562533928,-0.84804470594775));
#113018=DIRECTION('center_axis',(1.4081690688991E-16,0.,1.));
#113019=DIRECTION('ref_axis',(-1.,0.,1.4081690688991E-16));
#113020=DIRECTION('',(-0.503989916507255,-0.163750849686357,0.848044705947751));
#113021=DIRECTION('center_axis',(1.4081690688991E-16,0.,1.));
#113022=DIRECTION('ref_axis',(-1.,0.,1.4081690688991E-16));
#113023=DIRECTION('',(0.503986741943982,0.163760619987454,-0.848044705947755));
#113024=DIRECTION('center_axis',(1.4081690688991E-16,0.,1.));
#113025=DIRECTION('ref_axis',(-1.,0.,1.4081690688991E-16));
#113026=DIRECTION('',(-0.48411238233481,-0.215535096873142,0.848044705947747));
#113027=DIRECTION('center_axis',(1.4081690688991E-16,0.,1.));
#113028=DIRECTION('ref_axis',(-1.,0.,1.4081690688991E-16));
#113029=DIRECTION('',(0.484108203887574,0.21554448181929,-0.848044705947747));
#113030=DIRECTION('center_axis',(1.4081690688991E-16,0.,1.));
#113031=DIRECTION('ref_axis',(-1.,0.,1.4081690688991E-16));
#113032=DIRECTION('',(-0.458930811594469,-0.264957896434963,0.848044705947747));
#113033=DIRECTION('center_axis',(1.4081690688991E-16,0.,1.));
#113034=DIRECTION('ref_axis',(-1.,0.,1.4081690688991E-16));
#113035=DIRECTION('',(0.458925675043206,0.264966793202728,-0.848044705947747));
#113036=DIRECTION('center_axis',(1.4081690688991E-16,0.,1.));
#113037=DIRECTION('ref_axis',(-1.,0.,1.4081690688991E-16));
#113038=DIRECTION('',(-0.428721098844847,-0.311477761837441,0.84804470594775));
#113039=DIRECTION('center_axis',(1.4081690688991E-16,0.,1.));
#113040=DIRECTION('ref_axis',(-1.,0.,1.4081690688991E-16));
#113041=DIRECTION('',(0.428715060466699,0.311486072951947,-0.848044705947752));
#113042=DIRECTION('center_axis',(1.4081690688991E-16,0.,1.));
#113043=DIRECTION('ref_axis',(-1.,0.,1.4081690688991E-16));
#113044=DIRECTION('',(-0.393814228020627,-0.354585011700295,0.848044705947758));
#113045=DIRECTION('center_axis',(1.4081690688991E-16,0.,1.));
#113046=DIRECTION('ref_axis',(-1.,0.,1.4081690688991E-16));
#113047=DIRECTION('',(0.393807353973304,0.354592646103301,-0.848044705947749));
#113048=DIRECTION('center_axis',(1.4081690688991E-16,0.,1.));
#113049=DIRECTION('ref_axis',(-1.,0.,1.4081690688991E-16));
#113050=DIRECTION('',(-0.354592646103295,-0.393807353973305,0.848044705947751));
#113051=DIRECTION('center_axis',(1.4081690688991E-16,0.,1.));
#113052=DIRECTION('ref_axis',(-1.,0.,1.4081690688991E-16));
#113053=DIRECTION('',(0.354585011700323,0.393814228020616,-0.848044705947751));
#113054=DIRECTION('center_axis',(1.4081690688991E-16,0.,1.));
#113055=DIRECTION('ref_axis',(-1.,0.,1.4081690688991E-16));
#113056=DIRECTION('',(-0.311486072951976,-0.42871506046669,0.848044705947746));
#113057=DIRECTION('center_axis',(1.4081690688991E-16,0.,1.));
#113058=DIRECTION('ref_axis',(-1.,0.,1.4081690688991E-16));
#113059=DIRECTION('',(0.311477761837442,0.428721098844839,-0.848044705947754));
#113060=DIRECTION('center_axis',(1.4081690688991E-16,0.,1.));
#113061=DIRECTION('ref_axis',(-1.,1.95399252334028E-14,1.4081690688991E-16));
#113062=DIRECTION('',(-0.26496679320274,-0.458925675043192,0.848044705947751));
#113063=DIRECTION('center_axis',(1.4081690688991E-16,0.,1.));
#113064=DIRECTION('ref_axis',(-1.,0.,1.4081690688991E-16));
#113065=DIRECTION('',(0.264957896434973,0.458930811594463,-0.848044705947748));
#113066=DIRECTION('center_axis',(1.4081690688991E-16,0.,1.));
#113067=DIRECTION('ref_axis',(-1.,-1.95399252334028E-14,1.4081690688991E-16));
#113068=DIRECTION('',(-0.215544481819302,-0.484108203887559,0.848044705947752));
#113069=DIRECTION('center_axis',(1.4081690688991E-16,0.,1.));
#113070=DIRECTION('ref_axis',(-1.,0.,1.4081690688991E-16));
#113071=DIRECTION('',(0.215535096873159,0.484112382334815,-0.848044705947739));
#113072=DIRECTION('center_axis',(1.4081690688991E-16,0.,1.));
#113073=DIRECTION('ref_axis',(-1.,-9.76996261670138E-15,1.4081690688991E-16));
#113074=DIRECTION('',(-0.163760619987469,-0.503986741944003,0.84804470594774));
#113075=DIRECTION('center_axis',(1.4081690688991E-16,0.,1.));
#113076=DIRECTION('ref_axis',(-1.,-1.89093185554157E-12,1.4081690688991E-16));
#113077=DIRECTION('',(0.163750849686377,0.50398991650726,-0.848044705947744));
#113078=DIRECTION('center_axis',(1.4081690688991E-16,0.,1.));
#113079=DIRECTION('ref_axis',(-1.,-1.06581410364015E-14,1.4081690688991E-16));
#113080=DIRECTION('',(-0.110182562533945,-0.518343495789678,0.848044705947741));
#113081=DIRECTION('center_axis',(1.4081690688991E-16,0.,1.));
#113082=DIRECTION('ref_axis',(-1.,-1.93622895494627E-12,1.4081690688991E-16));
#113083=DIRECTION('',(0.110172513923367,0.51834563168777,-0.848044705947754));
#113084=DIRECTION('center_axis',(1.4081690688991E-16,0.,1.));
#113085=DIRECTION('ref_axis',(-1.,-1.06581410364015E-14,1.4081690688991E-16));
#113086=DIRECTION('',(-0.0553973218681174,-0.527021169825121,0.848044705947747));
#113087=DIRECTION('center_axis',(1.4081690688991E-16,0.,1.));
#113088=DIRECTION('ref_axis',(-1.,-1.98152605435098E-12,1.4081690688991E-16));
#113089=DIRECTION('',(0.0553871050427276,0.527022243656735,-0.848044705947751));
#113090=DIRECTION('center_axis',(1.4081690688991E-16,0.,1.));
#113091=DIRECTION('ref_axis',(-1.,-1.15463194561016E-14,1.4081690688991E-16));
#113092=DIRECTION('',(-5.13655126618051E-6,-0.529924689637704,0.848044705947746));
#113093=DIRECTION('',(-5.13655125534419E-6,0.52992468963771,-0.848044705947742));
#113094=DIRECTION('center_axis',(1.4081690688991E-16,0.,1.));
#113095=DIRECTION('ref_axis',(-1.,-1.15463194561016E-14,1.4081690688991E-16));
#113096=DIRECTION('',(0.0553871050427145,-0.527022243656735,0.848044705947752));
#113097=DIRECTION('center_axis',(1.4081690688991E-16,0.,1.));
#113098=DIRECTION('ref_axis',(-1.,-2.07123207474069E-12,1.4081690688991E-16));
#113099=DIRECTION('',(-0.0553973218681089,0.527021169825119,-0.848044705947749));
#113100=DIRECTION('center_axis',(1.4081690688991E-16,0.,1.));
#113101=DIRECTION('ref_axis',(-1.,-1.15463194561016E-14,1.4081690688991E-16));
#113102=DIRECTION('',(0.110172513923357,-0.518345631687771,0.848044705947754));
#113103=DIRECTION('center_axis',(1.4081690688991E-16,0.,1.));
#113104=DIRECTION('ref_axis',(-1.,-2.1165291741454E-12,1.4081690688991E-16));
#113105=DIRECTION('',(-0.110182562533934,0.518343495789649,-0.848044705947759));
#113106=DIRECTION('center_axis',(1.4081690688991E-16,0.,1.));
#113107=DIRECTION('ref_axis',(-1.,-1.15463194561016E-14,1.4081690688991E-16));
#113108=DIRECTION('',(0.163750849686358,-0.503989916507253,0.848044705947751));
#113109=DIRECTION('center_axis',(1.4081690688991E-16,0.,1.));
#113110=DIRECTION('ref_axis',(-1.,-4.32276436868051E-12,1.4081690688991E-16));
#113111=DIRECTION('',(-0.163760619987469,0.50398674194399,-0.848044705947747));
#113112=DIRECTION('center_axis',(1.4081690688991E-16,0.,1.));
#113113=DIRECTION('ref_axis',(-1.,-1.15463194561016E-14,1.4081690688991E-16));
#113114=DIRECTION('',(0.21553509687315,-0.484112382334798,0.848044705947752));
#113115=DIRECTION('center_axis',(1.4081690688991E-16,0.,1.));
#113116=DIRECTION('ref_axis',(-1.,-2.20623519453511E-12,1.4081690688991E-16));
#113117=DIRECTION('',(-0.215544481819284,0.484108203887573,-0.848044705947749));
#113118=DIRECTION('center_axis',(1.4081690688991E-16,0.,1.));
#113119=DIRECTION('ref_axis',(-1.,-1.24344978758018E-14,1.4081690688991E-16));
#113120=DIRECTION('',(0.264957896434973,-0.458930811594463,0.848044705947748));
#113121=DIRECTION('center_axis',(1.4081690688991E-16,0.,1.));
#113122=DIRECTION('ref_axis',(-1.,-4.50306458787963E-12,1.4081690688991E-16));
#113123=DIRECTION('',(-0.264966793202732,0.458925675043201,-0.848044705947748));
#113124=DIRECTION('center_axis',(1.4081690688991E-16,0.,1.));
#113125=DIRECTION('ref_axis',(-1.,-1.24344978758018E-14,1.4081690688991E-16));
#113126=DIRECTION('',(0.31147776183743,-0.428721098844854,0.84804470594775));
#113127=DIRECTION('center_axis',(1.4081690688991E-16,0.,1.));
#113128=DIRECTION('ref_axis',(-1.,-2.29682939334452E-12,1.4081690688991E-16));
#113129=DIRECTION('',(-0.31148607295195,0.428715060466704,-0.848044705947748));
#113130=DIRECTION('center_axis',(1.4081690688991E-16,0.,1.));
#113131=DIRECTION('ref_axis',(-1.,-3.19744231092045E-14,1.4081690688991E-16));
#113132=DIRECTION('',(0.354585011700312,-0.393814228020624,0.848044705947752));
#113133=DIRECTION('center_axis',(1.4081690688991E-16,0.,1.));
#113134=DIRECTION('ref_axis',(-1.,7.02460312140829E-12,1.4081690688991E-16));
#113135=DIRECTION('',(-0.354592646103303,0.393807353973293,-0.848044705947754));
#113136=DIRECTION('center_axis',(1.4081690688991E-16,0.,1.));
#113137=DIRECTION('ref_axis',(-1.,0.,1.4081690688991E-16));
#113138=DIRECTION('',(0.393807353973315,-0.354592646103299,0.848044705947745));
#113139=DIRECTION('center_axis',(1.4081690688991E-16,0.,1.));
#113140=DIRECTION('ref_axis',(-1.,-1.19282361765727E-12,1.4081690688991E-16));
#113141=DIRECTION('',(-0.393814228020623,0.354585011700318,-0.84804470594775));
#113142=DIRECTION('center_axis',(1.4081690688991E-16,0.,1.));
#113143=DIRECTION('ref_axis',(-1.,-3.28626015289046E-14,1.4081690688991E-16));
#113144=DIRECTION('',(0.428715060466675,-0.311486072951968,0.848044705947756));
#113145=DIRECTION('center_axis',(1.4081690688991E-16,0.,1.));
#113146=DIRECTION('ref_axis',(-1.,-1.21591625656947E-12,1.4081690688991E-16));
#113147=DIRECTION('',(-0.428721098844844,0.311477761837459,-0.848044705947745));
#113148=DIRECTION('center_axis',(1.4081690688991E-16,0.,1.));
#113149=DIRECTION('ref_axis',(-1.,7.105427357601E-15,1.4081690688991E-16));
#113150=DIRECTION('',(0.458925675043201,-0.264966793202732,0.848044705947748));
#113151=DIRECTION('center_axis',(1.4081690688991E-16,0.,1.));
#113152=DIRECTION('ref_axis',(-1.,-4.9533710466676E-12,1.4081690688991E-16));
#113153=DIRECTION('',(-0.458930811594453,0.264957896434968,-0.848044705947754));
#113154=DIRECTION('center_axis',(1.4081690688991E-16,0.,1.));
#113155=DIRECTION('ref_axis',(-1.,-1.33226762955019E-14,1.4081690688991E-16));
#113156=DIRECTION('',(0.484108203887561,-0.21554448181931,0.848044705947749));
#113157=DIRECTION('center_axis',(1.4081690688991E-16,0.,1.));
#113158=DIRECTION('ref_axis',(-1.,-2.52153853352866E-12,1.4081690688991E-16));
#113159=DIRECTION('',(-0.484112382334809,0.215535096873149,-0.848044705947745));
#113160=DIRECTION('center_axis',(1.4081690688991E-16,0.,1.));
#113161=DIRECTION('ref_axis',(-1.,-4.79616346638068E-14,1.4081690688991E-16));
#113162=DIRECTION('',(0.503986741943987,-0.163760619987463,0.848044705947751));
#113163=DIRECTION('center_axis',(1.4081690688991E-16,0.,1.));
#113164=DIRECTION('ref_axis',(-1.,7.70050689880008E-12,1.4081690688991E-16));
#113165=DIRECTION('',(-0.503989916507244,0.163750849686371,-0.848044705947754));
#113166=DIRECTION('center_axis',(1.4081690688991E-16,0.,1.));
#113167=DIRECTION('ref_axis',(-1.,7.105427357601E-15,1.4081690688991E-16));
#113168=DIRECTION('',(0.518343495789671,-0.110182562533949,0.848044705947744));
#113169=DIRECTION('center_axis',(1.4081690688991E-16,0.,1.));
#113170=DIRECTION('ref_axis',(-1.,-2.28528307388842E-12,1.4081690688991E-16));
#113171=DIRECTION('',(-0.518345631687771,0.110172513923364,-0.848044705947753));
#113172=DIRECTION('center_axis',(1.4081690688991E-16,0.,1.));
#113173=DIRECTION('ref_axis',(-1.,1.33226762955019E-14,1.4081690688991E-16));
#113174=DIRECTION('',(0.527021169825115,-0.0553973218681165,0.848044705947751));
#113175=DIRECTION('center_axis',(1.4081690688991E-16,0.,1.));
#113176=DIRECTION('ref_axis',(-1.,-2.65654165332307E-12,1.4081690688991E-16));
#113177=DIRECTION('',(-0.527022243656726,0.0553871050427283,-0.848044705947756));
#113178=DIRECTION('center_axis',(1.4081690688991E-16,0.,1.));
#113179=DIRECTION('ref_axis',(-1.,5.32907051820075E-15,1.4081690688991E-16));
#113180=DIRECTION('',(0.529924689637697,-5.13655126081405E-6,0.84804470594775));
#113181=DIRECTION('center_axis',(1.4081690688991E-16,0.,1.));
#113182=DIRECTION('ref_axis',(1.,0.,-1.4081690688991E-16));
#113183=DIRECTION('center_axis',(-1.4081690688991E-16,0.,-1.));
#113184=DIRECTION('ref_axis',(-1.,0.,1.4081690688991E-16));
#113185=DIRECTION('',(-0.529919264233204,-6.48963930749714E-17,0.848048096156427));
#113186=DIRECTION('center_axis',(-1.4081690688991E-16,0.,-1.));
#113187=DIRECTION('ref_axis',(-1.,0.,1.4081690688991E-16));
#113188=DIRECTION('center_axis',(-1.4081690688991E-16,0.,-1.));
#113189=DIRECTION('ref_axis',(-1.,0.,1.4081690688991E-16));
#113190=DIRECTION('',(-1.40816906889911E-16,0.,-1.));
#113191=DIRECTION('center_axis',(-1.4081690688991E-16,0.,-1.));
#113192=DIRECTION('ref_axis',(-1.,0.,1.4081690688991E-16));
#113193=DIRECTION('center_axis',(-1.4081690688991E-16,0.,-1.));
#113194=DIRECTION('ref_axis',(-1.,0.,1.40816906889911E-16));
#113195=DIRECTION('center_axis',(-1.4081690688991E-16,0.,-1.));
#113196=DIRECTION('ref_axis',(-1.,0.,1.4081690688991E-16));
#113197=DIRECTION('',(-0.994521895368275,-0.10452846326764,1.40045497140052E-16));
#113198=DIRECTION('center_axis',(-1.4081690688991E-16,0.,-1.));
#113199=DIRECTION('ref_axis',(-1.,0.,1.4081690688991E-16));
#113200=DIRECTION('',(1.,0.,-1.40816906889911E-16));
#113201=DIRECTION('center_axis',(-1.4081690688991E-16,0.,-1.));
#113202=DIRECTION('ref_axis',(-1.,0.,1.4081690688991E-16));
#113203=DIRECTION('center_axis',(-1.4081690688991E-16,0.,-1.));
#113204=DIRECTION('ref_axis',(-1.,0.,1.4081690688991E-16));
#113205=DIRECTION('center_axis',(1.4081690688991E-16,0.,1.));
#113206=DIRECTION('ref_axis',(1.,0.,-1.4081690688991E-16));
#113207=DIRECTION('center_axis',(1.4081690688991E-16,0.,1.));
#113208=DIRECTION('ref_axis',(-1.,0.,1.40816906889911E-16));
#113209=DIRECTION('',(-0.4972656110608,-0.0522695260941939,-0.866022406579771));
#113210=DIRECTION('',(0.500005191251964,-4.7780011657308E-6,0.866022406579794));
#113211=DIRECTION('center_axis',(-1.4081690688991E-16,0.,-1.));
#113212=DIRECTION('ref_axis',(-1.,0.,1.40816906889911E-16));
#113213=DIRECTION('center_axis',(1.4081690688991E-16,0.,1.));
#113214=DIRECTION('ref_axis',(-1.,0.,1.4081690688991E-16));
#113215=DIRECTION('',(-0.994521895368275,-0.10452846326764,1.40045497140052E-16));
#113216=DIRECTION('center_axis',(-1.4081690688991E-16,0.,-1.));
#113217=DIRECTION('ref_axis',(-1.,0.,1.4081690688991E-16));
#113218=DIRECTION('',(1.,0.,-1.40816906889911E-16));
#113219=DIRECTION('center_axis',(-1.4081690688991E-16,0.,-1.));
#113220=DIRECTION('ref_axis',(-1.,0.,1.4081690688991E-16));
#113221=DIRECTION('center_axis',(-1.4081690688991E-16,0.,-1.));
#113222=DIRECTION('ref_axis',(-1.,0.,1.4081690688991E-16));
#113223=DIRECTION('',(-0.497266395846506,-0.052260151065429,0.86602252174666));
#113224=DIRECTION('center_axis',(-1.4081690688991E-16,0.,-1.));
#113225=DIRECTION('ref_axis',(1.,3.46389583683049E-14,-1.4081690688991E-16));
#113226=DIRECTION('',(0.500004991781248,4.62770265276801E-6,-0.866022521746645));
#113227=DIRECTION('center_axis',(-1.4081690688991E-16,0.,-1.));
#113228=DIRECTION('ref_axis',(-1.,0.,1.4081690688991E-16));
#113229=DIRECTION('center_axis',(-1.4081690688991E-16,0.,-1.));
#113230=DIRECTION('ref_axis',(-1.,0.,1.4081690688991E-16));
#113231=DIRECTION('center_axis',(-1.4081690688991E-16,0.,-1.));
#113232=DIRECTION('ref_axis',(-1.,0.,1.40816906889911E-16));
#113233=DIRECTION('center_axis',(1.4081690688991E-16,0.,1.));
#113234=DIRECTION('ref_axis',(-1.,0.,1.4081690688991E-16));
#113235=DIRECTION('',(-0.994521895368275,-0.10452846326764,1.40045497140052E-16));
#113236=DIRECTION('',(1.,0.,-1.40816906889911E-16));
#113237=DIRECTION('center_axis',(-1.4081690688991E-16,0.,-1.));
#113238=DIRECTION('ref_axis',(-1.,0.,1.17174841180864E-16));
#113239=DIRECTION('center_axis',(-0.103464010407628,0.994633197962203,7.86457232110799E-6));
#113240=DIRECTION('ref_axis',(-0.843493966781864,-0.0877379732620273,-0.529924500330441));
#113241=DIRECTION('center_axis',(0.00107025596476198,-0.999999427244995,
7.86457194324946E-6));
#113242=DIRECTION('ref_axis',(1.47312952164193E-6,-7.86299982088955E-6,
-0.999999999968001));
#113243=DIRECTION('center_axis',(-1.4081690688991E-16,0.,-1.));
#113244=DIRECTION('ref_axis',(-1.,0.,1.13676889660403E-16));
#113245=DIRECTION('center_axis',(-0.103509373496897,0.994628478127797,-9.77051512295647E-6));
#113246=DIRECTION('ref_axis',(0.869950553189208,0.0905391058403171,0.48475633602814));
#113247=DIRECTION('center_axis',(0.00102464806165023,-0.999999475000305,
-9.77058602570879E-6));
#113248=DIRECTION('ref_axis',(0.874641264345339,0.000891463458077043,0.484769908304229));
#113249=DIRECTION('center_axis',(-1.4081690688991E-16,0.,-1.));
#113250=DIRECTION('ref_axis',(-1.,0.,1.15974593313694E-16));
#113251=DIRECTION('center_axis',(0.107112171226392,-0.994246942387258,1.81316452328514E-5));
#113252=DIRECTION('ref_axis',(0.861994650487305,0.0928552846708997,-0.498340364249129));
#113253=DIRECTION('center_axis',(0.0025983123505628,0.999996624215829,1.81624797792123E-5));
#113254=DIRECTION('ref_axis',(0.865241946196498,-0.0022390706427668,-0.501349539846954));
#113255=DIRECTION('center_axis',(-1.4081690688991E-16,0.,-1.));
#113256=DIRECTION('ref_axis',(-1.,0.,1.16261524579732E-16));
#113257=DIRECTION('center_axis',(0.10712560498394,-0.994245495043162,1.85257085273757E-5));
#113258=DIRECTION('ref_axis',(0.860265387812352,0.0926991758191971,0.501348506863744));
#113259=DIRECTION('center_axis',(0.00261182427506424,0.999996589010146,
1.84940601154894E-5));
#113260=DIRECTION('ref_axis',(0.866979057021487,-0.00227362102099331,0.498339387700376));
#113261=DIRECTION('center_axis',(-1.4081690688991E-16,0.,-1.));
#113262=DIRECTION('ref_axis',(-1.,0.,1.40816906889911E-16));
#113263=DIRECTION('center_axis',(-1.4081690688991E-16,0.,-1.));
#113264=DIRECTION('ref_axis',(-1.,0.,1.4081690688991E-16));
#113265=DIRECTION('',(0.994521895368275,0.10452846326764,-1.40045497140052E-16));
#113266=DIRECTION('center_axis',(-1.4081690688991E-16,0.,-1.));
#113267=DIRECTION('ref_axis',(-1.,0.,1.4081690688991E-16));
#113268=DIRECTION('center_axis',(-1.4081690688991E-16,0.,-1.));
#113269=DIRECTION('ref_axis',(-1.,0.,1.4081690688991E-16));
#113270=DIRECTION('center_axis',(-1.4081690688991E-16,0.,-1.));
#113271=DIRECTION('ref_axis',(-1.,0.,1.4081690688991E-16));
#113272=DIRECTION('',(-0.978147600733808,-0.207911690817747,1.37739719617122E-16));
#113273=DIRECTION('center_axis',(1.4081690688991E-16,0.,1.));
#113274=DIRECTION('ref_axis',(1.,0.,-1.4081690688991E-16));
#113275=DIRECTION('',(0.497266609935015,0.0522600224406397,0.866022406579784));
#113276=DIRECTION('center_axis',(1.4081690688991E-16,0.,1.));
#113277=DIRECTION('ref_axis',(-1.,0.,1.40816906889911E-16));
#113278=DIRECTION('',(-0.489077884775286,-0.103961598321231,-0.866022406579776));
#113279=DIRECTION('center_axis',(-1.4081690688991E-16,0.,-1.));
#113280=DIRECTION('ref_axis',(-1.,0.,1.40816906889911E-16));
#113281=DIRECTION('center_axis',(-1.4081690688991E-16,0.,-1.));
#113282=DIRECTION('ref_axis',(-1.,0.,1.4081690688991E-16));
#113283=DIRECTION('',(0.994521895368275,0.10452846326764,-1.40045497140052E-16));
#113284=DIRECTION('center_axis',(1.4081690688991E-16,0.,1.));
#113285=DIRECTION('ref_axis',(-1.,0.,1.4081690688991E-16));
#113286=DIRECTION('',(-0.978147600733808,-0.207911690817747,1.37739719617122E-16));
#113287=DIRECTION('center_axis',(-1.4081690688991E-16,0.,-1.));
#113288=DIRECTION('ref_axis',(-1.,0.,1.4081690688991E-16));
#113289=DIRECTION('center_axis',(-1.4081690688991E-16,0.,-1.));
#113290=DIRECTION('ref_axis',(1.,1.86517468137026E-14,-1.4081690688991E-16));
#113291=DIRECTION('',(0.497265428393217,0.0522693557686574,-0.866022521746658));
#113292=DIRECTION('center_axis',(-1.4081690688991E-16,0.,-1.));
#113293=DIRECTION('ref_axis',(-1.,0.,1.4081690688991E-16));
#113294=DIRECTION('center_axis',(-1.4081690688991E-16,0.,-1.));
#113295=DIRECTION('ref_axis',(-1.,0.,1.4081690688991E-16));
#113296=DIRECTION('center_axis',(-1.4081690688991E-16,0.,-1.));
#113297=DIRECTION('ref_axis',(-1.,0.,1.4081690688991E-16));
#113298=DIRECTION('',(-0.489079645219225,-0.1039523566823,0.866022521746653));
#113299=DIRECTION('center_axis',(-1.4081690688991E-16,0.,-1.));
#113300=DIRECTION('ref_axis',(-1.,0.,1.40816906889911E-16));
#113301=DIRECTION('',(0.994521895368275,0.10452846326764,-1.40045497140052E-16));
#113302=DIRECTION('center_axis',(1.4081690688991E-16,0.,1.));
#113303=DIRECTION('ref_axis',(-1.,0.,1.4081690688991E-16));
#113304=DIRECTION('',(-0.978147600733808,-0.207911690817747,1.37739719617122E-16));
#113305=DIRECTION('center_axis',(-1.4081690688991E-16,0.,-1.));
#113306=DIRECTION('ref_axis',(-1.,0.,1.17174841180864E-16));
#113307=DIRECTION('center_axis',(0.105592796389087,-0.994409453539578,7.8645721102773E-6));
#113308=DIRECTION('ref_axis',(2.28696687445886E-6,-7.66594168623456E-6,
-0.999999999968001));
#113309=DIRECTION('center_axis',(-0.206864703431098,0.978369559222134,7.86457219200017E-6));
#113310=DIRECTION('ref_axis',(-0.829702103060253,-0.175426463587734,-0.529924500330466));
#113311=DIRECTION('center_axis',(-1.4081690688991E-16,0.,-1.));
#113312=DIRECTION('ref_axis',(-1.,0.,1.13676889660403E-16));
#113313=DIRECTION('center_axis',(0.105547443322395,-0.994414268357329,-9.7705855822117E-6));
#113314=DIRECTION('ref_axis',(0.869756704680254,0.0923114872006744,0.484769908301397));
#113315=DIRECTION('center_axis',(-0.206909324659144,0.978360123509556,-9.77051573642606E-6));
#113316=DIRECTION('ref_axis',(0.855720959435962,0.18097771758913,0.484756336026901));
#113317=DIRECTION('center_axis',(-1.4081690688991E-16,0.,-1.));
#113318=DIRECTION('ref_axis',(-1.,0.,1.15974593313694E-16));
#113319=DIRECTION('center_axis',(-0.101944031878512,0.994790135674091,1.81624797640825E-5));
#113320=DIRECTION('ref_axis',(0.860736106896466,0.0882156062110998,-0.501349539847723));
#113321=DIRECTION('center_axis',(0.210452504541384,-0.97760408295153,1.81316452299207E-5));
#113322=DIRECTION('ref_axis',(0.847566533387361,0.182449589866313,-0.498340364248519));
#113323=DIRECTION('center_axis',(-1.4081690688991E-16,0.,-1.));
#113324=DIRECTION('ref_axis',(-1.,0.,1.16261524579732E-16));
#113325=DIRECTION('center_axis',(-0.101930590293366,0.994791513042012,1.84940595419896E-5));
#113326=DIRECTION('ref_axis',(0.862467313148182,0.0883628226288529,0.498339387694789));
#113327=DIRECTION('center_axis',(0.210465713413753,-0.97760123932718,1.85257174127305E-5));
#113328=DIRECTION('ref_axis',(0.845863061616564,0.182113579026111,0.501348506856213));
#113329=DIRECTION('center_axis',(-1.4081690688991E-16,0.,-1.));
#113330=DIRECTION('ref_axis',(-1.,0.,1.40816906889911E-16));
#113331=DIRECTION('center_axis',(-1.4081690688991E-16,0.,-1.));
#113332=DIRECTION('ref_axis',(-1.,0.,1.4081690688991E-16));
#113333=DIRECTION('',(0.978147600733808,0.207911690817747,-1.37739719617122E-16));
#113334=DIRECTION('center_axis',(-1.4081690688991E-16,0.,-1.));
#113335=DIRECTION('ref_axis',(-1.,0.,1.4081690688991E-16));
#113336=DIRECTION('center_axis',(-1.4081690688991E-16,0.,-1.));
#113337=DIRECTION('ref_axis',(-1.,0.,1.4081690688991E-16));
#113338=DIRECTION('center_axis',(-1.4081690688991E-16,0.,-1.));
#113339=DIRECTION('ref_axis',(-1.,0.,1.4081690688991E-16));
#113340=DIRECTION('',(-0.951056516295158,-0.309016994374935,1.33924836902178E-16));
#113341=DIRECTION('center_axis',(1.4081690688991E-16,0.,1.));
#113342=DIRECTION('ref_axis',(1.,0.,-1.4081690688991E-16));
#113343=DIRECTION('',(0.489079871579873,0.103952251140473,0.866022406579786));
#113344=DIRECTION('center_axis',(1.4081690688991E-16,0.,1.));
#113345=DIRECTION('ref_axis',(-1.,0.,1.40816906889911E-16));
#113346=DIRECTION('',(-0.475531718838024,-0.154514645521702,-0.866022406579793));
#113347=DIRECTION('center_axis',(-1.4081690688991E-16,0.,-1.));
#113348=DIRECTION('ref_axis',(-1.,0.,1.40816906889911E-16));
#113349=DIRECTION('center_axis',(-1.4081690688991E-16,0.,-1.));
#113350=DIRECTION('ref_axis',(-1.,0.,1.4081690688991E-16));
#113351=DIRECTION('',(0.978147600733808,0.207911690817747,-1.37739719617122E-16));
#113352=DIRECTION('center_axis',(1.4081690688991E-16,0.,1.));
#113353=DIRECTION('ref_axis',(-1.,0.,1.4081690688991E-16));
#113354=DIRECTION('',(-0.951056516295158,-0.309016994374935,1.33924836902178E-16));
#113355=DIRECTION('center_axis',(-1.4081690688991E-16,0.,-1.));
#113356=DIRECTION('ref_axis',(-1.,0.,1.4081690688991E-16));
#113357=DIRECTION('center_axis',(-1.4081690688991E-16,0.,-1.));
#113358=DIRECTION('ref_axis',(1.,1.4210854715202E-14,-1.4081690688991E-16));
#113359=DIRECTION('',(0.489077720912263,0.103961409834796,-0.866022521746651));
#113360=DIRECTION('center_axis',(-1.4081690688991E-16,0.,-1.));
#113361=DIRECTION('ref_axis',(-1.,0.,1.4081690688991E-16));
#113362=DIRECTION('center_axis',(-1.4081690688991E-16,0.,-1.));
#113363=DIRECTION('ref_axis',(-1.,0.,1.4081690688991E-16));
#113364=DIRECTION('center_axis',(-1.4081690688991E-16,0.,-1.));
#113365=DIRECTION('ref_axis',(-1.,0.,1.4081690688991E-16));
#113366=DIRECTION('',(-0.475534435652402,-0.154505638525938,0.86602252174666));
#113367=DIRECTION('center_axis',(-1.4081690688991E-16,0.,-1.));
#113368=DIRECTION('ref_axis',(-1.,0.,1.40816906889911E-16));
#113369=DIRECTION('',(0.978147600733808,0.207911690817747,-1.37739719617122E-16));
#113370=DIRECTION('center_axis',(1.4081690688991E-16,0.,1.));
#113371=DIRECTION('ref_axis',(-1.,0.,1.4081690688991E-16));
#113372=DIRECTION('',(-0.951056516295158,-0.309016994374935,1.33924836902178E-16));
#113373=DIRECTION('center_axis',(-1.4081690688991E-16,0.,-1.));
#113374=DIRECTION('ref_axis',(-1.,0.,1.17174841180864E-16));
#113375=DIRECTION('center_axis',(0.208958440039433,-0.977924521767624,7.86457212166731E-6));
#113376=DIRECTION('ref_axis',(3.07574774830936E-6,-7.38489373063671E-6,
-0.999999999968002));
#113377=DIRECTION('center_axis',(-0.307998943474316,0.951386698854285,7.86457231463923E-6));
#113378=DIRECTION('ref_axis',(-0.806819849471271,-0.261192944867695,-0.529924500330468));
#113379=DIRECTION('center_axis',(-1.4081690688991E-16,0.,-1.));
#113380=DIRECTION('ref_axis',(-1.,0.,1.13676889660403E-16));
#113381=DIRECTION('center_axis',(0.208913838707158,-0.97793405089565,-9.77058570875104E-6));
#113382=DIRECTION('ref_axis',(0.855342908547131,0.182720126971686,0.484769908304533));
#113383=DIRECTION('center_axis',(-0.308042333962507,0.95137265064299,-9.77051511559201E-6));
#113384=DIRECTION('ref_axis',(0.832115907779592,0.269433499592006,0.48475633602641));
#113385=DIRECTION('center_axis',(-1.4081690688991E-16,0.,-1.));
#113386=DIRECTION('ref_axis',(-1.,0.,1.15974593313694E-16));
#113387=DIRECTION('center_axis',(-0.205369455961159,0.978684518232685,1.81624797493655E-5));
#113388=DIRECTION('ref_axis',(0.846799862694007,0.177703774424036,-0.501349539839084));
#113389=DIRECTION('center_axis',(0.31148707617651,-0.95025038860621,1.81316451190475E-5));
#113390=DIRECTION('ref_axis',(0.82385229998115,0.270044939174584,-0.498340364251145));
#113391=DIRECTION('center_axis',(-1.4081690688991E-16,0.,-1.));
#113392=DIRECTION('ref_axis',(-1.,0.,1.16261524579732E-16));
#113393=DIRECTION('center_axis',(-0.205356231984476,0.9786872930835,1.84940593962113E-5));
#113394=DIRECTION('ref_axis',(0.848506196906012,0.178031144702923,0.498339387694635));
#113395=DIRECTION('center_axis',(0.311499915448403,-0.950246179856797,1.8525719752645E-5));
#113396=DIRECTION('ref_axis',(0.822193282702067,0.269532707749979,0.501348506861807));
#113397=DIRECTION('center_axis',(-1.4081690688991E-16,0.,-1.));
#113398=DIRECTION('ref_axis',(-1.,0.,1.40816906889911E-16));
#113399=DIRECTION('center_axis',(-1.4081690688991E-16,0.,-1.));
#113400=DIRECTION('ref_axis',(-1.,0.,1.4081690688991E-16));
#113401=DIRECTION('',(0.951056516295158,0.309016994374935,-1.33924836902178E-16));
#113402=DIRECTION('center_axis',(-1.4081690688991E-16,0.,-1.));
#113403=DIRECTION('ref_axis',(-1.,0.,1.4081690688991E-16));
#113404=DIRECTION('center_axis',(-1.4081690688991E-16,0.,-1.));
#113405=DIRECTION('ref_axis',(-1.,0.,1.4081690688991E-16));
#113406=DIRECTION('center_axis',(-1.4081690688991E-16,0.,-1.));
#113407=DIRECTION('ref_axis',(-1.,0.,1.4081690688991E-16));
#113408=DIRECTION('',(-0.913545457642606,-0.406736643075789,1.2864264564856E-16));
#113409=DIRECTION('center_axis',(1.4081690688991E-16,0.,1.));
#113410=DIRECTION('ref_axis',(1.,0.,-1.4081690688991E-16));
#113411=DIRECTION('',(0.475534671805143,0.15450555722339,0.866022406579798));
#113412=DIRECTION('center_axis',(1.4081690688991E-16,0.,1.));
#113413=DIRECTION('ref_axis',(-1.,0.,1.40816906889911E-16));
#113414=DIRECTION('',(-0.456775527877824,-0.203374797931539,-0.866022406579784));
#113415=DIRECTION('center_axis',(-1.4081690688991E-16,0.,-1.));
#113416=DIRECTION('ref_axis',(-1.,0.,1.40816906889911E-16));
#113417=DIRECTION('center_axis',(-1.4081690688991E-16,0.,-1.));
#113418=DIRECTION('ref_axis',(-1.,0.,1.4081690688991E-16));
#113419=DIRECTION('',(0.951056516295158,0.309016994374935,-1.33924836902178E-16));
#113420=DIRECTION('center_axis',(1.4081690688991E-16,0.,1.));
#113421=DIRECTION('ref_axis',(-1.,0.,1.4081690688991E-16));
#113422=DIRECTION('',(-0.913545457642606,-0.406736643075789,1.2864264564856E-16));
#113423=DIRECTION('center_axis',(-1.4081690688991E-16,0.,-1.));
#113424=DIRECTION('ref_axis',(-1.,0.,1.4081690688991E-16));
#113425=DIRECTION('center_axis',(-1.4081690688991E-16,0.,-1.));
#113426=DIRECTION('ref_axis',(1.,2.04281036531029E-14,-1.4081690688991E-16));
#113427=DIRECTION('',(0.47553157557488,0.154514440939486,-0.866022521746652));
#113428=DIRECTION('center_axis',(-1.4081690688991E-16,0.,-1.));
#113429=DIRECTION('ref_axis',(-1.,0.,1.4081690688991E-16));
#113430=DIRECTION('center_axis',(-1.4081690688991E-16,0.,-1.));
#113431=DIRECTION('ref_axis',(-1.,0.,1.4081690688991E-16));
#113432=DIRECTION('center_axis',(-1.4081690688991E-16,0.,-1.));
#113433=DIRECTION('ref_axis',(-1.,0.,1.4081690688991E-16));
#113434=DIRECTION('',(-0.456779171296623,-0.203366124261482,0.866022521746654));
#113435=DIRECTION('center_axis',(-1.4081690688991E-16,0.,-1.));
#113436=DIRECTION('ref_axis',(-1.,0.,1.40816906889911E-16));
#113437=DIRECTION('',(0.951056516295158,0.309016994374935,-1.33924836902178E-16));
#113438=DIRECTION('center_axis',(1.4081690688991E-16,0.,1.));
#113439=DIRECTION('ref_axis',(-1.,0.,1.4081690688991E-16));
#113440=DIRECTION('',(-0.913545457642606,-0.406736643075789,1.2864264564856E-16));
#113441=DIRECTION('center_axis',(-1.4081690688991E-16,0.,-1.));
#113442=DIRECTION('ref_axis',(-1.,0.,1.17174841180864E-16));
#113443=DIRECTION('center_axis',(0.310034691293352,-0.950725244291317,7.86457213372142E-6));
#113444=DIRECTION('ref_axis',(3.83083005362731E-6,-7.02293534441516E-6,
-0.999999999968002));
#113445=DIRECTION('center_axis',(-0.405758682640018,0.913980246723301,7.86457234792495E-6));
#113446=DIRECTION('ref_axis',(-0.775097908773559,-0.344097741585692,-0.529924500330455));
#113447=DIRECTION('center_axis',(-1.4081690688991E-16,0.,-1.));
#113448=DIRECTION('ref_axis',(-1.,0.,1.13676889660403E-16));
#113449=DIRECTION('center_axis',(0.309991330356933,-0.950739383326511,-9.77058570930425E-6));
#113450=DIRECTION('ref_axis',(0.831557796517394,0.27112684679503,0.484769908305085));
#113451=DIRECTION('center_axis',(-0.405800366992815,0.913961739928447,-9.77051475421558E-6));
#113452=DIRECTION('ref_axis',(0.799394020106877,0.354937311791151,0.484756336024438));
#113453=DIRECTION('center_axis',(-1.4081690688991E-16,0.,-1.));
#113454=DIRECTION('ref_axis',(-1.,0.,1.15974593313694E-16));
#113455=DIRECTION('center_axis',(-0.306544809307878,0.951856228406644,1.81624797541284E-5));
#113456=DIRECTION('ref_axis',(0.823585901985486,0.265244982896519,-0.501349539841196));
#113457=DIRECTION('center_axis',(0.409108930222434,-0.912485552150553,1.81316453160849E-5));
#113458=DIRECTION('ref_axis',(0.791111768373129,0.354681619617994,-0.498340364255894));
#113459=DIRECTION('center_axis',(-1.4081690688991E-16,0.,-1.));
#113460=DIRECTION('ref_axis',(-1.,0.,1.16261524579732E-16));
#113461=DIRECTION('center_axis',(-0.306531947828759,0.951860370337098,1.84940671411514E-5));
#113462=DIRECTION('ref_axis',(0.825248669203561,0.265748920298447,0.498339387704766));
#113463=DIRECTION('center_axis',(0.409121259222939,-0.912480024388827,1.85257240494735E-5));
#113464=DIRECTION('ref_axis',(0.789515382129665,0.353998779724754,0.501348506863274));
#113465=DIRECTION('center_axis',(-1.4081690688991E-16,0.,-1.));
#113466=DIRECTION('ref_axis',(-1.,0.,1.40816906889911E-16));
#113467=DIRECTION('center_axis',(-1.4081690688991E-16,0.,-1.));
#113468=DIRECTION('ref_axis',(-1.,0.,1.4081690688991E-16));
#113469=DIRECTION('',(0.913545457642606,0.406736643075789,-1.2864264564856E-16));
#113470=DIRECTION('center_axis',(-1.4081690688991E-16,0.,-1.));
#113471=DIRECTION('ref_axis',(-1.,0.,1.4081690688991E-16));
#113472=DIRECTION('center_axis',(-1.4081690688991E-16,0.,-1.));
#113473=DIRECTION('ref_axis',(-1.,0.,1.4081690688991E-16));
#113474=DIRECTION('center_axis',(-1.4081690688991E-16,0.,-1.));
#113475=DIRECTION('ref_axis',(-1.,0.,1.4081690688991E-16));
#113476=DIRECTION('',(-0.866025403784445,-0.499999999999989,1.21951018649011E-16));
#113477=DIRECTION('center_axis',(1.4081690688991E-16,0.,1.));
#113478=DIRECTION('ref_axis',(1.,0.,-1.4081690688991E-16));
#113479=DIRECTION('',(0.45677941465413,0.203366068089046,0.866022406579779));
#113480=DIRECTION('center_axis',(1.4081690688991E-16,0.,1.));
#113481=DIRECTION('ref_axis',(-1.,0.,1.40816906889911E-16));
#113482=DIRECTION('',(-0.433014808647733,-0.250006733496379,-0.866022406579782));
#113483=DIRECTION('center_axis',(-1.4081690688991E-16,0.,-1.));
#113484=DIRECTION('ref_axis',(-1.,0.,1.40816906889911E-16));
#113485=DIRECTION('center_axis',(-1.4081690688991E-16,0.,-1.));
#113486=DIRECTION('ref_axis',(-1.,0.,1.4081690688991E-16));
#113487=DIRECTION('',(0.913545457642606,0.406736643075789,-1.2864264564856E-16));
#113488=DIRECTION('center_axis',(1.4081690688991E-16,0.,1.));
#113489=DIRECTION('ref_axis',(-1.,0.,1.4081690688991E-16));
#113490=DIRECTION('',(-0.866025403784445,-0.499999999999989,1.21951018649011E-16));
#113491=DIRECTION('center_axis',(-1.4081690688991E-16,0.,-1.));
#113492=DIRECTION('ref_axis',(-1.,0.,1.4081690688991E-16));
#113493=DIRECTION('center_axis',(-1.4081690688991E-16,0.,-1.));
#113494=DIRECTION('ref_axis',(1.,2.48689957516035E-14,-1.4081690688991E-16));
#113495=DIRECTION('',(0.456775406784114,0.203374579494995,-0.866022521746659));
#113496=DIRECTION('center_axis',(-1.4081690688991E-16,0.,-1.));
#113497=DIRECTION('ref_axis',(-1.,0.,1.4081690688991E-16));
#113498=DIRECTION('center_axis',(-1.4081690688991E-16,0.,-1.));
#113499=DIRECTION('ref_axis',(-1.,0.,1.4081690688991E-16));
#113500=DIRECTION('center_axis',(-1.4081690688991E-16,0.,-1.));
#113501=DIRECTION('ref_axis',(-1.,0.,1.4081690688991E-16));
#113502=DIRECTION('',(-0.433019338752905,-0.249998488182556,0.866022521746654));
#113503=DIRECTION('center_axis',(-1.4081690688991E-16,0.,-1.));
#113504=DIRECTION('ref_axis',(-1.,0.,1.40816906889911E-16));
#113505=DIRECTION('',(0.913545457642606,0.406736643075789,-1.2864264564856E-16));
#113506=DIRECTION('center_axis',(1.4081690688991E-16,0.,1.));
#113507=DIRECTION('ref_axis',(-1.,0.,1.4081690688991E-16));
#113508=DIRECTION('',(-0.866025403784445,-0.499999999999989,1.21951018649011E-16));
#113509=DIRECTION('center_axis',(-1.4081690688991E-16,0.,-1.));
#113510=DIRECTION('ref_axis',(-1.,0.,1.17174841180864E-16));
#113511=DIRECTION('center_axis',(0.407714137590522,-0.913109622086508,7.86457214212551E-6));
#113512=DIRECTION('ref_axis',(4.54394102509795E-6,-6.58403219129936E-6,
-0.999999999968001));
#113513=DIRECTION('center_axis',(-0.499072844768381,0.866560035746482,7.86457218027767E-6));
#113514=DIRECTION('ref_axis',(-0.73488383318754,-0.423232531439995,-0.529924500330454));
#113515=DIRECTION('center_axis',(-1.4081690688991E-16,0.,-1.));
#113516=DIRECTION('ref_axis',(-1.,0.,1.13676889660403E-16));
#113517=DIRECTION('center_axis',(0.407672492122622,-0.913128216118123,-9.77058808687787E-6));
#113518=DIRECTION('ref_axis',(0.798661963255971,0.356563044148554,0.484769908302521));
#113519=DIRECTION('center_axis',(-0.499112366281653,0.866537273133283,-9.77051754275204E-6));
#113520=DIRECTION('ref_axis',(0.757913804263396,0.436552356525734,0.484756336027508));
#113521=DIRECTION('center_axis',(-1.4081690688991E-16,0.,-1.));
#113522=DIRECTION('ref_axis',(-1.,0.,1.15974593313694E-16));
#113523=DIRECTION('center_axis',(-0.404361593575374,0.914599202553397,1.816247957149E-5));
#113524=DIRECTION('ref_axis',(0.791348561788099,0.349880111829978,-0.50134953984396));
#113525=DIRECTION('center_axis',(0.502248501217063,-0.86472333303575,1.81316453019379E-5));
#113526=DIRECTION('ref_axis',(0.749703650686612,0.435432334018008,-0.498340364247967));
#113527=DIRECTION('center_axis',(-1.4081690688991E-16,0.,-1.));
#113528=DIRECTION('ref_axis',(-1.,0.,1.16261524579732E-16));
#113529=DIRECTION('center_axis',(-0.404349235499867,0.914604666185693,1.84940625621926E-5));
#113530=DIRECTION('ref_axis',(0.792949544399534,0.350555095115829,0.498339387691665));
#113531=DIRECTION('center_axis',(0.502260184874653,-0.864716546821256,1.85257140468035E-5));
#113532=DIRECTION('ref_axis',(0.748187385814963,0.434586366990226,0.501348506862849));
#113533=DIRECTION('center_axis',(-1.4081690688991E-16,0.,-1.));
#113534=DIRECTION('ref_axis',(-1.,0.,1.40816906889911E-16));
#113535=DIRECTION('center_axis',(-1.4081690688991E-16,0.,-1.));
#113536=DIRECTION('ref_axis',(-1.,0.,1.4081690688991E-16));
#113537=DIRECTION('',(0.866025403784445,0.499999999999989,-1.21951018649011E-16));
#113538=DIRECTION('center_axis',(-1.4081690688991E-16,0.,-1.));
#113539=DIRECTION('ref_axis',(-1.,0.,1.4081690688991E-16));
#113540=DIRECTION('center_axis',(-1.4081690688991E-16,0.,-1.));
#113541=DIRECTION('ref_axis',(-1.,0.,1.4081690688991E-16));
#113542=DIRECTION('center_axis',(-1.4081690688991E-16,0.,-1.));
#113543=DIRECTION('ref_axis',(-1.,0.,1.4081690688991E-16));
#113544=DIRECTION('',(-0.809016994374955,-0.587785252292463,1.13923270769253E-16));
#113545=DIRECTION('center_axis',(1.4081690688991E-16,0.,1.));
#113546=DIRECTION('ref_axis',(1.,0.,-1.4081690688991E-16));
#113547=DIRECTION('',(0.433019586648924,0.249998457755589,0.866022406579773));
#113548=DIRECTION('center_axis',(1.4081690688991E-16,0.,1.));
#113549=DIRECTION('ref_axis',(-1.,0.,1.40816906889911E-16));
#113550=DIRECTION('',(-0.404509888559955,-0.293899542971717,-0.866022406579777));
#113551=DIRECTION('center_axis',(-1.4081690688991E-16,0.,-1.));
#113552=DIRECTION('ref_axis',(-1.,0.,1.40816906889911E-16));
#113553=DIRECTION('center_axis',(-1.4081690688991E-16,0.,-1.));
#113554=DIRECTION('ref_axis',(-1.,0.,1.4081690688991E-16));
#113555=DIRECTION('',(0.866025403784445,0.499999999999989,-1.21951018649011E-16));
#113556=DIRECTION('center_axis',(1.4081690688991E-16,0.,1.));
#113557=DIRECTION('ref_axis',(-1.,0.,1.4081690688991E-16));
#113558=DIRECTION('',(-0.809016994374955,-0.587785252292463,1.13923270769253E-16));
#113559=DIRECTION('center_axis',(-1.4081690688991E-16,0.,-1.));
#113560=DIRECTION('ref_axis',(-1.,0.,1.4081690688991E-16));
#113561=DIRECTION('center_axis',(-1.4081690688991E-16,0.,-1.));
#113562=DIRECTION('ref_axis',(1.,1.95399252334028E-14,-1.4081690688991E-16));
#113563=DIRECTION('',(0.433014711050255,0.250006503598669,-0.866022521746653));
#113564=DIRECTION('center_axis',(-1.4081690688991E-16,0.,-1.));
#113565=DIRECTION('ref_axis',(-1.,0.,1.4081690688991E-16));
#113566=DIRECTION('center_axis',(-1.4081690688991E-16,0.,-1.));
#113567=DIRECTION('ref_axis',(-1.,0.,1.4081690688991E-16));
#113568=DIRECTION('center_axis',(-1.4081690688991E-16,0.,-1.));
#113569=DIRECTION('ref_axis',(-1.,0.,1.4081690688991E-16));
#113570=DIRECTION('',(-0.404515255718701,-0.293891816351536,0.866022521746651));
#113571=DIRECTION('center_axis',(-1.4081690688991E-16,0.,-1.));
#113572=DIRECTION('ref_axis',(-1.,0.,1.40816906889911E-16));
#113573=DIRECTION('',(0.866025403784445,0.499999999999989,-1.21951018649011E-16));
#113574=DIRECTION('center_axis',(1.4081690688991E-16,0.,1.));
#113575=DIRECTION('ref_axis',(-1.,0.,1.4081690688991E-16));
#113576=DIRECTION('',(-0.809016994374955,-0.587785252292463,1.13923270769253E-16));
#113577=DIRECTION('center_axis',(-1.4081690688991E-16,0.,-1.));
#113578=DIRECTION('ref_axis',(-1.,0.,1.17174841180864E-16));
#113579=DIRECTION('center_axis',(0.500926582476576,-0.865489779781649,7.86457214533227E-6));
#113580=DIRECTION('ref_axis',(5.20726763301671E-6,-6.0729929870304E-6,-0.999999999968002));
#113581=DIRECTION('center_axis',(-0.586919060371622,0.80964561167874,7.8645721780656E-6));
#113582=DIRECTION('ref_axis',(-0.686618216540878,-0.497730297112552,-0.529924500330447));
#113583=DIRECTION('center_axis',(-1.4081690688991E-16,0.,-1.));
#113584=DIRECTION('ref_axis',(-1.,0.,1.13676889660403E-16));
#113585=DIRECTION('center_axis',(0.500887108754481,-0.865512625088804,-9.77059218766514E-6));
#113586=DIRECTION('ref_axis',(0.757015822392063,0.438092662173902,0.484769908304396));
#113587=DIRECTION('center_axis',(-0.586955986038022,0.809618842640579,-9.77052405936867E-6));
#113588=DIRECTION('ref_axis',(0.708129726178679,0.513384442288736,0.48475633602666));
#113589=DIRECTION('center_axis',(-1.4081690688991E-16,0.,-1.));
#113590=DIRECTION('ref_axis',(-1.,0.,1.15974593313694E-16));
#113591=DIRECTION('center_axis',(-0.497748107605369,0.867321636444865,1.81624798484582E-5));
#113592=DIRECTION('ref_axis',(0.750441041150575,0.430681881042595,-0.501349539840671));
#113593=DIRECTION('center_axis',(0.589885332530237,-0.807487024129141,1.81316453652568E-5));
#113594=DIRECTION('ref_axis',(0.700081622914366,0.511412360645375,-0.498340364245875));
#113595=DIRECTION('center_axis',(-1.4081690688991E-16,0.,-1.));
#113596=DIRECTION('ref_axis',(-1.,0.,1.16261524579732E-16));
#113597=DIRECTION('center_axis',(-0.497736388327921,0.867328361920817,1.84940507090592E-5));
#113598=DIRECTION('ref_axis',(0.751962698442014,0.431520514948995,0.498339387696737));
#113599=DIRECTION('center_axis',(0.589896242826456,-0.807479053818753,1.85257236353235E-5));
#113600=DIRECTION('ref_axis',(0.698662091933123,0.51041253507613,0.501348506862033));
#113601=DIRECTION('center_axis',(-1.4081690688991E-16,0.,-1.));
#113602=DIRECTION('ref_axis',(-1.,0.,1.40816906889911E-16));
#113603=DIRECTION('center_axis',(-1.4081690688991E-16,0.,-1.));
#113604=DIRECTION('ref_axis',(-1.,0.,1.4081690688991E-16));
#113605=DIRECTION('',(0.809016994374955,0.587785252292463,-1.13923270769253E-16));
#113606=DIRECTION('center_axis',(-1.4081690688991E-16,0.,-1.));
#113607=DIRECTION('ref_axis',(-1.,0.,1.4081690688991E-16));
#113608=DIRECTION('center_axis',(-1.4081690688991E-16,0.,-1.));
#113609=DIRECTION('ref_axis',(-1.,0.,1.4081690688991E-16));
#113610=DIRECTION('center_axis',(-1.4081690688991E-16,0.,-1.));
#113611=DIRECTION('ref_axis',(-1.,0.,1.4081690688991E-16));
#113612=DIRECTION('',(-0.743144825477402,-0.66913060635885,1.0464735569497E-16));
#113613=DIRECTION('center_axis',(1.4081690688991E-16,0.,1.));
#113614=DIRECTION('ref_axis',(1.,0.,-1.4081690688991E-16));
#113615=DIRECTION('',(0.404515505437166,0.293891812003437,0.86602240657979));
#113616=DIRECTION('center_axis',(1.4081690688991E-16,0.,1.));
#113617=DIRECTION('ref_axis',(-1.,0.,1.40816906889911E-16));
#113618=DIRECTION('',(-0.371573073483918,-0.334572327551858,-0.866022406579788));
#113619=DIRECTION('center_axis',(-1.4081690688991E-16,0.,-1.));
#113620=DIRECTION('ref_axis',(-1.,0.,1.40816906889911E-16));
#113621=DIRECTION('center_axis',(-1.4081690688991E-16,0.,-1.));
#113622=DIRECTION('ref_axis',(-1.,0.,1.4081690688991E-16));
#113623=DIRECTION('',(0.809016994374955,0.587785252292463,-1.13923270769253E-16));
#113624=DIRECTION('center_axis',(1.4081690688991E-16,0.,1.));
#113625=DIRECTION('ref_axis',(-1.,0.,1.4081690688991E-16));
#113626=DIRECTION('',(-0.743144825477402,-0.66913060635885,1.0464735569497E-16));
#113627=DIRECTION('center_axis',(-1.4081690688991E-16,0.,-1.));
#113628=DIRECTION('ref_axis',(-1.,0.,1.4081690688991E-16));
#113629=DIRECTION('center_axis',(-1.4081690688991E-16,0.,-1.));
#113630=DIRECTION('ref_axis',(1.,1.33226762955019E-14,-1.4081690688991E-16));
#113631=DIRECTION('',(0.404509815527881,0.293899304131705,-0.866022521746692));
#113632=DIRECTION('center_axis',(-1.4081690688991E-16,0.,-1.));
#113633=DIRECTION('ref_axis',(-1.,0.,1.4081690688991E-16));
#113634=DIRECTION('center_axis',(-1.4081690688991E-16,0.,-1.));
#113635=DIRECTION('ref_axis',(-1.,0.,1.4081690688991E-16));
#113636=DIRECTION('center_axis',(-1.4081690688991E-16,0.,-1.));
#113637=DIRECTION('ref_axis',(-1.,0.,1.4081690688991E-16));
#113638=DIRECTION('',(-0.371579218892574,-0.334565204279747,0.866022521746655));
#113639=DIRECTION('center_axis',(-1.4081690688991E-16,0.,-1.));
#113640=DIRECTION('ref_axis',(-1.,0.,1.40816906889911E-16));
#113641=DIRECTION('',(0.809016994374955,0.587785252292463,-1.13923270769253E-16));
#113642=DIRECTION('center_axis',(1.4081690688991E-16,0.,1.));
#113643=DIRECTION('ref_axis',(-1.,0.,1.4081690688991E-16));
#113644=DIRECTION('',(-0.743144825477402,-0.66913060635885,1.0464735569497E-16));
#113645=DIRECTION('center_axis',(-1.4081690688991E-16,0.,-1.));
#113646=DIRECTION('ref_axis',(-1.,0.,1.17174841180864E-16));
#113647=DIRECTION('center_axis',(0.588650770899379,-0.80838745033413,7.86457210154094E-6));
#113648=DIRECTION('ref_axis',(5.81354225308953E-6,-5.4954167984505E-6,-0.999999999968002));
#113649=DIRECTION('center_axis',(-0.668334867928659,0.743860540860268,7.86457229484424E-6));
#113650=DIRECTION('ref_axis',(-0.630829867029782,-0.566774825493071,-0.529924500330459));
#113651=DIRECTION('center_axis',(-1.4081690688991E-16,0.,-1.));
#113652=DIRECTION('ref_axis',(-1.,0.,1.13676889660403E-16));
#113653=DIRECTION('center_axis',(0.588613901402245,-0.808414296620591,-9.77058986000007E-6));
#113654=DIRECTION('ref_axis',(0.70707565776309,0.514822445315893,0.484769908304814));
#113655=DIRECTION('center_axis',(-0.668368793188665,0.743830058680116,-9.77051765906954E-6));
#113656=DIRECTION('ref_axis',(0.650587230627793,0.584591780669081,0.484756336026886));
#113657=DIRECTION('center_axis',(-1.4081690688991E-16,0.,-1.));
#113658=DIRECTION('ref_axis',(-1.,0.,1.15974593313694E-16));
#113659=DIRECTION('center_axis',(-0.585681189208067,0.810541512988662,1.81624795712343E-5));
#113660=DIRECTION('ref_axis',(0.701311531422973,0.506765009438398,-0.501349539844273));
#113661=DIRECTION('center_axis',(0.671059256698672,-0.741403718408715,1.81316452494132E-5));
#113662=DIRECTION('ref_axis',(0.642789354376865,0.581789246427105,-0.498340364250735));
#113663=DIRECTION('center_axis',(-1.4081690688991E-16,0.,-1.));
#113664=DIRECTION('ref_axis',(-1.,0.,1.16261524579732E-16));
#113665=DIRECTION('center_axis',(-0.585670237131424,0.810549426621469,1.84940458788945E-5));
#113666=DIRECTION('ref_axis',(0.702737191804646,0.507758105720061,0.498339387696875));
#113667=DIRECTION('center_axis',(0.671069274101679,-0.741394651325084,1.85257263442263E-5));
#113668=DIRECTION('ref_axis',(0.641482109966447,0.580646516615992,0.501348506863948));
#113669=DIRECTION('center_axis',(-1.4081690688991E-16,0.,-1.));
#113670=DIRECTION('ref_axis',(-1.,0.,1.40816906889911E-16));
#113671=DIRECTION('center_axis',(-1.4081690688991E-16,0.,-1.));
#113672=DIRECTION('ref_axis',(-1.,0.,1.4081690688991E-16));
#113673=DIRECTION('',(0.743144825477402,0.66913060635885,-1.0464735569497E-16));
#113674=DIRECTION('center_axis',(-1.4081690688991E-16,0.,-1.));
#113675=DIRECTION('ref_axis',(-1.,0.,1.4081690688991E-16));
#113676=DIRECTION('center_axis',(-1.4081690688991E-16,0.,-1.));
#113677=DIRECTION('ref_axis',(-1.,0.,1.4081690688991E-16));
#113678=DIRECTION('center_axis',(-1.4081690688991E-16,0.,-1.));
#113679=DIRECTION('ref_axis',(-1.,0.,1.4081690688991E-16));
#113680=DIRECTION('',(-0.669130606358867,-0.743144825477386,9.42249022928259E-17));
#113681=DIRECTION('center_axis',(1.4081690688991E-16,0.,1.));
#113682=DIRECTION('ref_axis',(1.,0.,-1.4081690688991E-16));
#113683=DIRECTION('',(0.371579467697561,0.334565226058171,0.866022406579785));
#113684=DIRECTION('center_axis',(1.4081690688991E-16,0.,1.));
#113685=DIRECTION('ref_axis',(-1.,0.,1.40816906889911E-16));
#113686=DIRECTION('',(-0.334565226058175,-0.371579467697537,-0.866022406579794));
#113687=DIRECTION('center_axis',(-1.4081690688991E-16,0.,-1.));
#113688=DIRECTION('ref_axis',(-1.,0.,1.40816906889911E-16));
#113689=DIRECTION('center_axis',(-1.4081690688991E-16,0.,-1.));
#113690=DIRECTION('ref_axis',(-1.,0.,1.4081690688991E-16));
#113691=DIRECTION('',(0.743144825477402,0.66913060635885,-1.0464735569497E-16));
#113692=DIRECTION('center_axis',(1.4081690688991E-16,0.,1.));
#113693=DIRECTION('ref_axis',(-1.,0.,1.4081690688991E-16));
#113694=DIRECTION('',(-0.669130606358867,-0.743144825477386,9.42249022928259E-17));
#113695=DIRECTION('center_axis',(-1.4081690688991E-16,0.,-1.));
#113696=DIRECTION('ref_axis',(-1.,0.,1.4081690688991E-16));
#113697=DIRECTION('center_axis',(-1.4081690688991E-16,0.,-1.));
#113698=DIRECTION('ref_axis',(1.,1.33226762955019E-14,-1.4081690688991E-16));
#113699=DIRECTION('',(0.371573025817597,0.334572082386321,-0.866022521746655));
#113700=DIRECTION('center_axis',(-1.4081690688991E-16,0.,-1.));
#113701=DIRECTION('ref_axis',(-1.,0.,1.4081690688991E-16));
#113702=DIRECTION('center_axis',(-1.4081690688991E-16,0.,-1.));
#113703=DIRECTION('ref_axis',(-1.,0.,1.4081690688991E-16));
#113704=DIRECTION('center_axis',(-1.4081690688991E-16,0.,-1.));
#113705=DIRECTION('ref_axis',(-1.,0.,1.4081690688991E-16));
#113706=DIRECTION('',(-0.334572082386318,-0.371573025817621,0.866022521746647));
#113707=DIRECTION('center_axis',(-1.4081690688991E-16,0.,-1.));
#113708=DIRECTION('ref_axis',(-1.,0.,1.40816906889911E-16));
#113709=DIRECTION('',(0.743144825477402,0.66913060635885,-1.0464735569497E-16));
#113710=DIRECTION('center_axis',(1.4081690688991E-16,0.,1.));
#113711=DIRECTION('ref_axis',(-1.,0.,1.4081690688991E-16));
#113712=DIRECTION('',(-0.669130606358867,-0.743144825477386,9.42249022928259E-17));
#113713=DIRECTION('center_axis',(-1.4081690688991E-16,0.,-1.));
#113714=DIRECTION('ref_axis',(-1.,0.,1.17174841180864E-16));
#113715=DIRECTION('center_axis',(0.669925578293215,-0.742428258814715,7.86457222451189E-6));
#113716=DIRECTION('ref_axis',(6.35612261558566E-6,-4.85763178434958E-6,
-0.999999999968002));
#113717=DIRECTION('center_axis',(-0.742428258814657,0.66992557829328,7.86457232160625E-6));
#113718=DIRECTION('ref_axis',(-0.568130013485826,-0.629609650280326,-0.529924500330453));
#113719=DIRECTION('center_axis',(-1.4081690688991E-16,0.,-1.));
#113720=DIRECTION('ref_axis',(-1.,0.,1.13676889660403E-16));
#113721=DIRECTION('center_axis',(0.669891716970495,-0.742458811947746,-9.77058614774733E-6));
#113722=DIRECTION('ref_axis',(0.649388624263242,0.585911726014071,0.484769908303626));
#113723=DIRECTION('center_axis',(-0.742458811969737,0.669891716946122,-9.77052681755937E-6));
#113724=DIRECTION('ref_axis',(0.585916765233622,0.649394209166309,0.484756336028146));
#113725=DIRECTION('center_axis',(-1.4081690688991E-16,0.,-1.));
#113726=DIRECTION('ref_axis',(-1.,0.,1.15974593313694E-16));
#113727=DIRECTION('center_axis',(-0.667197425140104,0.744880927099453,1.81624795753533E-5));
#113728=DIRECTION('ref_axis',(0.644498305802597,0.577295914346879,-0.501349539838209));
#113729=DIRECTION('center_axis',(0.744880915222603,-0.667197438400643,1.8131645392797E-5));
#113730=DIRECTION('ref_axis',(0.578454551163898,0.645791927480607,-0.498340364247827));
#113731=DIRECTION('center_axis',(-1.4081690688991E-16,0.,-1.));
#113732=DIRECTION('ref_axis',(-1.,0.,1.16261524579732E-16));
#113733=DIRECTION('center_axis',(-0.667187360268565,0.744889942176584,1.8494066007285E-5));
#113734=DIRECTION('ref_axis',(0.645812349439158,0.578432592431863,0.498339387691189));
#113735=DIRECTION('center_axis',(0.744889929979156,-0.667187373885662,1.85257309138967E-5));
#113736=DIRECTION('ref_axis',(0.577273915764732,0.644518813412092,0.501348506864758));
#113737=DIRECTION('center_axis',(-1.4081690688991E-16,0.,-1.));
#113738=DIRECTION('ref_axis',(-1.,0.,1.40816906889911E-16));
#113739=DIRECTION('center_axis',(-1.4081690688991E-16,0.,-1.));
#113740=DIRECTION('ref_axis',(-1.,0.,1.4081690688991E-16));
#113741=DIRECTION('',(0.669130606358867,0.743144825477386,-9.42249022928259E-17));
#113742=DIRECTION('center_axis',(-1.4081690688991E-16,0.,-1.));
#113743=DIRECTION('ref_axis',(-1.,0.,1.4081690688991E-16));
#113744=DIRECTION('center_axis',(-1.4081690688991E-16,0.,-1.));
#113745=DIRECTION('ref_axis',(-1.,0.,1.4081690688991E-16));
#113746=DIRECTION('center_axis',(-1.4081690688991E-16,0.,-1.));
#113747=DIRECTION('ref_axis',(-1.,0.,1.4081690688991E-16));
#113748=DIRECTION('',(-0.587785252292482,-0.809016994374941,8.2770101143333E-17));
#113749=DIRECTION('center_axis',(1.4081690688991E-16,0.,1.));
#113750=DIRECTION('ref_axis',(1.,0.,-1.4081690688991E-16));
#113751=DIRECTION('',(0.334572327551885,0.371573073483891,0.866022406579789));
#113752=DIRECTION('center_axis',(1.4081690688991E-16,0.,1.));
#113753=DIRECTION('ref_axis',(-1.,1.86517468137026E-14,1.40816906889911E-16));
#113754=DIRECTION('',(-0.293891812003428,-0.404515505437145,-0.866022406579803));
#113755=DIRECTION('center_axis',(-1.4081690688991E-16,0.,-1.));
#113756=DIRECTION('ref_axis',(-1.,0.,1.40816906889911E-16));
#113757=DIRECTION('center_axis',(-1.4081690688991E-16,0.,-1.));
#113758=DIRECTION('ref_axis',(-1.,0.,1.4081690688991E-16));
#113759=DIRECTION('',(0.669130606358867,0.743144825477386,-9.42249022928259E-17));
#113760=DIRECTION('center_axis',(1.4081690688991E-16,0.,1.));
#113761=DIRECTION('ref_axis',(-1.,1.86517468137026E-14,1.4081690688991E-16));
#113762=DIRECTION('',(-0.587785252292482,-0.809016994374941,8.2770101143333E-17));
#113763=DIRECTION('center_axis',(-1.4081690688991E-16,0.,-1.));
#113764=DIRECTION('ref_axis',(-1.,0.,1.4081690688991E-16));
#113765=DIRECTION('center_axis',(-1.4081690688991E-16,0.,-1.));
#113766=DIRECTION('ref_axis',(1.,-2.66453525910038E-14,-1.4081690688991E-16));
#113767=DIRECTION('',(0.33456520427975,0.371579218892551,-0.866022521746664));
#113768=DIRECTION('center_axis',(-1.4081690688991E-16,0.,-1.));
#113769=DIRECTION('ref_axis',(-1.,0.,1.4081690688991E-16));
#113770=DIRECTION('center_axis',(-1.4081690688991E-16,0.,-1.));
#113771=DIRECTION('ref_axis',(-1.,0.,1.4081690688991E-16));
#113772=DIRECTION('center_axis',(-1.4081690688991E-16,0.,-1.));
#113773=DIRECTION('ref_axis',(-1.,0.,1.4081690688991E-16));
#113774=DIRECTION('',(-0.293899304131723,-0.404509815527924,0.866022521746666));
#113775=DIRECTION('center_axis',(-1.4081690688991E-16,0.,-1.));
#113776=DIRECTION('ref_axis',(-1.,0.,1.40816906889911E-16));
#113777=DIRECTION('',(0.669130606358867,0.743144825477386,-9.42249022928259E-17));
#113778=DIRECTION('center_axis',(1.4081690688991E-16,0.,1.));
#113779=DIRECTION('ref_axis',(-1.,0.,1.4081690688991E-16));
#113780=DIRECTION('',(-0.587785252292482,-0.809016994374941,8.2770101143333E-17));
#113781=DIRECTION('center_axis',(-1.4081690688991E-16,0.,-1.));
#113782=DIRECTION('ref_axis',(-1.,0.,1.17174841180864E-16));
#113783=DIRECTION('center_axis',(0.743860540860151,-0.66833486792879,7.86457201063913E-6));
#113784=DIRECTION('ref_axis',(6.82906374699039E-6,-4.16662528541481E-6,
-0.999999999968002));
#113785=DIRECTION('center_axis',(-0.808387450334093,0.58865077089943,7.86457218447997E-6));
#113786=DIRECTION('ref_axis',(-0.499205608625081,-0.685546339984944,-0.529924500330481));
#113787=DIRECTION('center_axis',(-1.4081690688991E-16,0.,-1.));
#113788=DIRECTION('ref_axis',(-1.,0.,1.13676889660403E-16));
#113789=DIRECTION('center_axis',(0.743830058703253,-0.668368793162915,-9.77058023976066E-6));
#113790=DIRECTION('ref_axis',(0.584586753102912,0.650581635232641,0.484769908301471));
#113791=DIRECTION('center_axis',(-0.808414296642385,0.588613901372314,-9.77052295710416E-6));
#113792=DIRECTION('ref_axis',(0.5148268731491,0.707081738813847,0.484756336028222));
#113793=DIRECTION('center_axis',(-1.4081690688991E-16,0.,-1.));
#113794=DIRECTION('ref_axis',(-1.,0.,1.15974593313694E-16));
#113795=DIRECTION('center_axis',(-0.741403706462291,0.671059269896558,1.8162479572778E-5));
#113796=DIRECTION('ref_axis',(0.58062382187003,0.641501844407687,-0.501349539840793));
#113797=DIRECTION('center_axis',(0.810541502562919,-0.585681203637515,1.81316451184131E-5));
#113798=DIRECTION('ref_axis',(0.507782078838013,0.702719177035393,-0.498340364246813));
#113799=DIRECTION('center_axis',(-1.4081690688991E-16,0.,-1.));
#113800=DIRECTION('ref_axis',(-1.,0.,1.16261524579732E-16));
#113801=DIRECTION('center_axis',(-0.741394639060127,0.671069287652828,1.84940680536415E-5));
#113802=DIRECTION('ref_axis',(0.581811851823624,0.642769650612115,0.498339387696322));
#113803=DIRECTION('center_axis',(0.810549415916517,-0.585670251945744,1.85257039599468E-5));
#113804=DIRECTION('ref_axis',(0.506740987741176,0.701329627215963,0.501348506861461));
#113805=DIRECTION('center_axis',(-1.4081690688991E-16,0.,-1.));
#113806=DIRECTION('ref_axis',(-1.,0.,1.40816906889911E-16));
#113807=DIRECTION('center_axis',(-1.4081690688991E-16,0.,-1.));
#113808=DIRECTION('ref_axis',(-1.,0.,1.4081690688991E-16));
#113809=DIRECTION('',(0.587785252292482,0.809016994374941,-8.2770101143333E-17));
#113810=DIRECTION('center_axis',(-1.4081690688991E-16,0.,-1.));
#113811=DIRECTION('ref_axis',(-1.,0.,1.4081690688991E-16));
#113812=DIRECTION('center_axis',(-1.4081690688991E-16,0.,-1.));
#113813=DIRECTION('ref_axis',(-1.,0.,1.4081690688991E-16));
#113814=DIRECTION('center_axis',(-1.4081690688991E-16,0.,-1.));
#113815=DIRECTION('ref_axis',(-1.,0.,1.4081690688991E-16));
#113816=DIRECTION('',(-0.50000000000001,-0.866025403784433,7.04084534449566E-17));
#113817=DIRECTION('center_axis',(1.4081690688991E-16,0.,1.));
#113818=DIRECTION('ref_axis',(1.,0.,-1.4081690688991E-16));
#113819=DIRECTION('',(0.293899542971749,0.404509888559906,0.866022406579789));
#113820=DIRECTION('center_axis',(1.4081690688991E-16,0.,1.));
#113821=DIRECTION('ref_axis',(-1.,-1.95399252334028E-14,1.40816906889911E-16));
#113822=DIRECTION('',(-0.249998457755608,-0.433019586648879,-0.866022406579791));
#113823=DIRECTION('center_axis',(-1.4081690688991E-16,0.,-1.));
#113824=DIRECTION('ref_axis',(-1.,0.,1.40816906889911E-16));
#113825=DIRECTION('center_axis',(-1.4081690688991E-16,0.,-1.));
#113826=DIRECTION('ref_axis',(-1.,0.,1.4081690688991E-16));
#113827=DIRECTION('',(0.587785252292482,0.809016994374941,-8.2770101143333E-17));
#113828=DIRECTION('center_axis',(1.4081690688991E-16,0.,1.));
#113829=DIRECTION('ref_axis',(-1.,-1.86517468137026E-14,1.4081690688991E-16));
#113830=DIRECTION('',(-0.50000000000001,-0.866025403784433,7.04084534449566E-17));
#113831=DIRECTION('center_axis',(-1.4081690688991E-16,0.,-1.));
#113832=DIRECTION('ref_axis',(-1.,0.,1.4081690688991E-16));
#113833=DIRECTION('center_axis',(-1.4081690688991E-16,0.,-1.));
#113834=DIRECTION('ref_axis',(1.,1.24344978758018E-14,-1.4081690688991E-16));
#113835=DIRECTION('',(0.293891816351536,0.404515255718701,-0.866022521746651));
#113836=DIRECTION('center_axis',(-1.4081690688991E-16,0.,-1.));
#113837=DIRECTION('ref_axis',(-1.,0.,1.4081690688991E-16));
#113838=DIRECTION('center_axis',(-1.4081690688991E-16,0.,-1.));
#113839=DIRECTION('ref_axis',(-1.,0.,1.4081690688991E-16));
#113840=DIRECTION('center_axis',(-1.4081690688991E-16,0.,-1.));
#113841=DIRECTION('ref_axis',(-1.,0.,1.4081690688991E-16));
#113842=DIRECTION('',(-0.250006503598682,-0.433014711050253,0.86602252174665));
#113843=DIRECTION('center_axis',(-1.4081690688991E-16,0.,-1.));
#113844=DIRECTION('ref_axis',(-1.,0.,1.40816906889911E-16));
#113845=DIRECTION('',(0.587785252292482,0.809016994374941,-8.2770101143333E-17));
#113846=DIRECTION('center_axis',(1.4081690688991E-16,0.,1.));
#113847=DIRECTION('ref_axis',(-1.,1.95399252334028E-14,1.4081690688991E-16));
#113848=DIRECTION('',(-0.50000000000001,-0.866025403784433,7.04084534449566E-17));
#113849=DIRECTION('center_axis',(-1.4081690688991E-16,0.,-1.));
#113850=DIRECTION('ref_axis',(-1.,0.,1.17174841180864E-16));
#113851=DIRECTION('center_axis',(0.809645611678693,-0.586919060371687,7.86457198631099E-6));
#113852=DIRECTION('ref_axis',(7.2271843168904E-6,-3.42996854670039E-6,-0.999999999968002));
#113853=DIRECTION('center_axis',(-0.865489779781559,0.50092658247673,7.86457232116346E-6));
#113854=DIRECTION('ref_axis',(-0.424811802651054,-0.733972040528688,-0.529924500330486));
#113855=DIRECTION('center_axis',(-1.4081690688991E-16,0.,-1.));
#113856=DIRECTION('ref_axis',(-1.,0.,1.13676889660403E-16));
#113857=DIRECTION('center_axis',(0.80961884265869,-0.58695598601304,-9.77057981626784E-6));
#113858=DIRECTION('ref_axis',(0.513380027140866,0.70812363591017,0.484769908305172));
#113859=DIRECTION('center_axis',(-0.865512625109973,0.500887108717902,-9.77051588858328E-6));
#113860=DIRECTION('ref_axis',(0.438096430107544,0.757022332963905,0.484756336029672));
#113861=DIRECTION('center_axis',(-1.4081690688991E-16,0.,-1.));
#113862=DIRECTION('ref_axis',(-1.,0.,1.15974593313694E-16));
#113863=DIRECTION('center_axis',(-0.807487013627686,0.589885346904605,1.81624797272146E-5));
#113864=DIRECTION('ref_axis',(0.510387901841611,0.698679346017535,-0.501349539844436));
#113865=DIRECTION('center_axis',(0.867321627584511,-0.497748123045581,1.81316451958916E-5));
#113866=DIRECTION('ref_axis',(0.431546239794257,0.751947288229924,-0.498340364252286));
#113867=DIRECTION('center_axis',(-1.4081690688991E-16,0.,-1.));
#113868=DIRECTION('ref_axis',(-1.,0.,1.16261524579732E-16));
#113869=DIRECTION('center_axis',(-0.80747904303877,0.589896257583621,1.84940691754006E-5));
#113870=DIRECTION('ref_axis',(0.511436901809337,0.7000643899933,0.498339387697757));
#113871=DIRECTION('center_axis',(0.867328352817319,-0.497736404190002,1.85257287627715E-5));
#113872=DIRECTION('ref_axis',(0.43065609941129,0.750456526858726,0.501348506864229));
#113873=DIRECTION('center_axis',(-1.4081690688991E-16,0.,-1.));
#113874=DIRECTION('ref_axis',(-1.,0.,1.40816906889911E-16));
#113875=DIRECTION('center_axis',(-1.4081690688991E-16,0.,-1.));
#113876=DIRECTION('ref_axis',(-1.,0.,1.4081690688991E-16));
#113877=DIRECTION('',(0.50000000000001,0.866025403784433,-7.04084534449566E-17));
#113878=DIRECTION('center_axis',(-1.4081690688991E-16,0.,-1.));
#113879=DIRECTION('ref_axis',(-1.,0.,1.4081690688991E-16));
#113880=DIRECTION('center_axis',(-1.4081690688991E-16,0.,-1.));
#113881=DIRECTION('ref_axis',(-1.,0.,1.4081690688991E-16));
#113882=DIRECTION('center_axis',(-1.4081690688991E-16,0.,-1.));
#113883=DIRECTION('ref_axis',(-1.,0.,1.4081690688991E-16));
#113884=DIRECTION('',(-0.40673664307581,-0.913545457642596,5.72753959967212E-17));
#113885=DIRECTION('center_axis',(1.4081690688991E-16,0.,1.));
#113886=DIRECTION('ref_axis',(1.,0.,-1.4081690688991E-16));
#113887=DIRECTION('',(0.250006733496405,0.43301480864773,0.866022406579776));
#113888=DIRECTION('center_axis',(1.4081690688991E-16,0.,1.));
#113889=DIRECTION('ref_axis',(-1.,-3.90798504668055E-14,1.40816906889911E-16));
#113890=DIRECTION('',(-0.203366068089036,-0.456779414654109,-0.866022406579792));
#113891=DIRECTION('center_axis',(-1.4081690688991E-16,0.,-1.));
#113892=DIRECTION('ref_axis',(-1.,0.,1.40816906889911E-16));
#113893=DIRECTION('center_axis',(-1.4081690688991E-16,0.,-1.));
#113894=DIRECTION('ref_axis',(-1.,0.,1.4081690688991E-16));
#113895=DIRECTION('',(0.50000000000001,0.866025403784433,-7.04084534449566E-17));
#113896=DIRECTION('center_axis',(1.4081690688991E-16,0.,1.));
#113897=DIRECTION('ref_axis',(-1.,-4.08562073062058E-14,1.4081690688991E-16));
#113898=DIRECTION('',(-0.40673664307581,-0.913545457642596,5.72753959967212E-17));
#113899=DIRECTION('center_axis',(-1.4081690688991E-16,0.,-1.));
#113900=DIRECTION('ref_axis',(-1.,0.,1.4081690688991E-16));
#113901=DIRECTION('center_axis',(-1.4081690688991E-16,0.,-1.));
#113902=DIRECTION('ref_axis',(1.,1.24344978758018E-14,-1.4081690688991E-16));
#113903=DIRECTION('',(0.249998488182559,0.433019338752883,-0.866022521746664));
#113904=DIRECTION('center_axis',(-1.4081690688991E-16,0.,-1.));
#113905=DIRECTION('ref_axis',(-1.,0.,1.4081690688991E-16));
#113906=DIRECTION('center_axis',(-1.4081690688991E-16,0.,-1.));
#113907=DIRECTION('ref_axis',(-1.,0.,1.4081690688991E-16));
#113908=DIRECTION('center_axis',(-1.4081690688991E-16,0.,-1.));
#113909=DIRECTION('ref_axis',(-1.,0.,1.4081690688991E-16));
#113910=DIRECTION('',(-0.203374579494995,-0.456775406784114,0.866022521746659));
#113911=DIRECTION('center_axis',(-1.4081690688991E-16,0.,-1.));
#113912=DIRECTION('ref_axis',(-1.,0.,1.40816906889911E-16));
#113913=DIRECTION('',(0.50000000000001,0.866025403784433,-7.04084534449566E-17));
#113914=DIRECTION('center_axis',(1.4081690688991E-16,0.,1.));
#113915=DIRECTION('ref_axis',(-1.,3.90798504668055E-14,1.4081690688991E-16));
#113916=DIRECTION('',(-0.40673664307581,-0.913545457642596,5.72753959967212E-17));
#113917=DIRECTION('center_axis',(-1.4081690688991E-16,0.,-1.));
#113918=DIRECTION('ref_axis',(-1.,0.,1.17174841180864E-16));
#113919=DIRECTION('center_axis',(0.866560035746456,-0.499072844768427,7.86457212100347E-6));
#113920=DIRECTION('ref_axis',(7.54612252965279E-6,-2.65573237658704E-6,
-0.999999999968001));
#113921=DIRECTION('center_axis',(-0.913109622086468,0.407714137590612,7.86457225083087E-6));
#113922=DIRECTION('ref_axis',(-0.345763669669355,-0.774356189803036,-0.529924500330477));
#113923=DIRECTION('center_axis',(-1.4081690688991E-16,0.,-1.));
#113924=DIRECTION('ref_axis',(-1.,0.,1.13676889660403E-16));
#113925=DIRECTION('center_axis',(0.866537273151611,-0.499112366249832,-9.77058386824003E-6));
#113926=DIRECTION('ref_axis',(0.436548602171663,0.757907285850706,0.484769908303293));
#113927=DIRECTION('center_axis',(-0.913128216134471,0.407672492086008,-9.77051561494199E-6));
#113928=DIRECTION('ref_axis',(0.356566110901319,0.798668832019173,0.484756336026502));
#113929=DIRECTION('center_axis',(-1.4081690688991E-16,0.,-1.));
#113930=DIRECTION('ref_axis',(-1.,0.,1.15974593313694E-16));
#113931=DIRECTION('center_axis',(-0.864723324094313,0.502248516610458,1.81624798191131E-5));
#113932=DIRECTION('ref_axis',(0.434560065158887,0.748201970510128,-0.501349539836096));
#113933=DIRECTION('center_axis',(0.914599195355562,-0.404361609857071,1.81316452823751E-5));
#113934=DIRECTION('ref_axis',(0.350582289841991,0.792936907581347,-0.498340364253665));
#113935=DIRECTION('center_axis',(-1.4081690688991E-16,0.,-1.));
#113936=DIRECTION('ref_axis',(-1.,0.,1.16261524579732E-16));
#113937=DIRECTION('center_axis',(-0.864716537640355,0.502260200682123,1.84940508031252E-5));
#113938=DIRECTION('ref_axis',(0.435458542075013,0.7496890774218,0.498339387695128));
#113939=DIRECTION('center_axis',(0.914604658800418,-0.404349252203302,1.85256963593625E-5));
#113940=DIRECTION('ref_axis',(0.34985285273782,0.791361267753626,0.501348506859832));
#113941=DIRECTION('center_axis',(-1.4081690688991E-16,0.,-1.));
#113942=DIRECTION('ref_axis',(-1.,0.,1.40816906889911E-16));
#113943=DIRECTION('center_axis',(-1.4081690688991E-16,0.,-1.));
#113944=DIRECTION('ref_axis',(-1.,0.,1.4081690688991E-16));
#113945=DIRECTION('',(0.40673664307581,0.913545457642596,-5.72753959967212E-17));
#113946=DIRECTION('center_axis',(-1.4081690688991E-16,0.,-1.));
#113947=DIRECTION('ref_axis',(-1.,0.,1.4081690688991E-16));
#113948=DIRECTION('center_axis',(-1.4081690688991E-16,0.,-1.));
#113949=DIRECTION('ref_axis',(-1.,0.,1.4081690688991E-16));
#113950=DIRECTION('center_axis',(-1.4081690688991E-16,0.,-1.));
#113951=DIRECTION('ref_axis',(-1.,0.,1.4081690688991E-16));
#113952=DIRECTION('',(-0.309016994374957,-0.95105651629515,4.35148173242984E-17));
#113953=DIRECTION('center_axis',(1.4081690688991E-16,0.,1.));
#113954=DIRECTION('ref_axis',(1.,0.,-1.4081690688991E-16));
#113955=DIRECTION('',(0.203374797931567,0.456775527877826,0.866022406579776));
#113956=DIRECTION('center_axis',(1.4081690688991E-16,0.,1.));
#113957=DIRECTION('ref_axis',(-1.,-9.76996261670138E-15,1.40816906889911E-16));
#113958=DIRECTION('',(-0.154505557223409,-0.475534671805168,-0.866022406579781));
#113959=DIRECTION('center_axis',(-1.4081690688991E-16,0.,-1.));
#113960=DIRECTION('ref_axis',(-1.,0.,1.40816906889911E-16));
#113961=DIRECTION('center_axis',(-1.4081690688991E-16,0.,-1.));
#113962=DIRECTION('ref_axis',(-1.,0.,1.4081690688991E-16));
#113963=DIRECTION('',(0.40673664307581,0.913545457642596,-5.72753959967212E-17));
#113964=DIRECTION('center_axis',(1.4081690688991E-16,0.,1.));
#113965=DIRECTION('ref_axis',(-1.,-9.76996261670138E-15,1.4081690688991E-16));
#113966=DIRECTION('',(-0.309016994374957,-0.95105651629515,4.35148173242984E-17));
#113967=DIRECTION('center_axis',(-1.4081690688991E-16,0.,-1.));
#113968=DIRECTION('ref_axis',(-1.,0.,1.4081690688991E-16));
#113969=DIRECTION('center_axis',(-1.4081690688991E-16,0.,-1.));
#113970=DIRECTION('ref_axis',(1.,1.24344978758018E-14,-1.4081690688991E-16));
#113971=DIRECTION('',(0.203366124261493,0.45677917129659,-0.866022521746669));
#113972=DIRECTION('center_axis',(-1.4081690688991E-16,0.,-1.));
#113973=DIRECTION('ref_axis',(-1.,0.,1.4081690688991E-16));
#113974=DIRECTION('center_axis',(-1.4081690688991E-16,0.,-1.));
#113975=DIRECTION('ref_axis',(-1.,0.,1.4081690688991E-16));
#113976=DIRECTION('center_axis',(-1.4081690688991E-16,0.,-1.));
#113977=DIRECTION('ref_axis',(-1.,0.,1.4081690688991E-16));
#113978=DIRECTION('',(-0.154514440939481,-0.475531575574859,0.866022521746664));
#113979=DIRECTION('center_axis',(-1.4081690688991E-16,0.,-1.));
#113980=DIRECTION('ref_axis',(-1.,0.,1.40816906889911E-16));
#113981=DIRECTION('',(0.40673664307581,0.913545457642596,-5.72753959967212E-17));
#113982=DIRECTION('center_axis',(1.4081690688991E-16,0.,1.));
#113983=DIRECTION('ref_axis',(-1.,0.,1.4081690688991E-16));
#113984=DIRECTION('',(-0.309016994374957,-0.95105651629515,4.35148173242984E-17));
#113985=DIRECTION('center_axis',(-1.4081690688991E-16,0.,-1.));
#113986=DIRECTION('ref_axis',(-1.,0.,1.17174841180864E-16));
#113987=DIRECTION('center_axis',(0.913980246723209,-0.405758682640226,7.86457201705324E-6));
#113988=DIRECTION('ref_axis',(7.78238360297463E-6,-1.85239937195232E-6,
-0.999999999968002));
#113989=DIRECTION('center_axis',(-0.950725244291279,0.310034691293469,7.86457228312283E-6));
#113990=DIRECTION('ref_axis',(-0.262927277567183,-0.806256330617375,-0.529924500330486));
#113991=DIRECTION('center_axis',(-1.4081690688991E-16,0.,-1.));
#113992=DIRECTION('ref_axis',(-1.,0.,1.13676889660403E-16));
#113993=DIRECTION('center_axis',(0.913961739943276,-0.405800366959415,-9.7705808297001E-6));
#113994=DIRECTION('ref_axis',(0.354934259363254,0.799387144965269,0.484769908301385));
#113995=DIRECTION('center_axis',(-0.950739383338138,0.309991330321275,-9.77051799119866E-6));
#113996=DIRECTION('ref_axis',(0.271129178766797,0.831564948216653,0.484756336027367));
#113997=DIRECTION('center_axis',(-1.4081690688991E-16,0.,-1.));
#113998=DIRECTION('ref_axis',(-1.,0.,1.15974593313694E-16));
#113999=DIRECTION('center_axis',(-0.912485544867192,0.409108946466033,1.81624796700739E-5));
#114000=DIRECTION('ref_axis',(0.353971097458838,0.789527137631561,-0.501349539849295));
#114001=DIRECTION('center_axis',(0.951856222950106,-0.30654482625287,1.81316452438961E-5));
#114002=DIRECTION('ref_axis',(0.265777286960435,0.825238944247301,-0.498340364242704));
#114003=DIRECTION('center_axis',(-1.4081690688991E-16,0.,-1.));
#114004=DIRECTION('ref_axis',(-1.,0.,1.16261524579732E-16));
#114005=DIRECTION('center_axis',(-0.91248001690956,0.409121275905689,1.84940567058976E-5));
#114006=DIRECTION('ref_axis',(0.354709207426606,0.791100014432689,0.498339387698172));
#114007=DIRECTION('center_axis',(0.951860364736293,-0.306531965218784,1.85257121801136E-5));
#114008=DIRECTION('ref_axis',(0.265216544996555,0.823595688992732,0.501348506861921));
#114009=DIRECTION('center_axis',(-1.4081690688991E-16,0.,-1.));
#114010=DIRECTION('ref_axis',(-1.,0.,1.40816906889911E-16));
#114011=DIRECTION('center_axis',(-1.4081690688991E-16,0.,-1.));
#114012=DIRECTION('ref_axis',(-1.,0.,1.4081690688991E-16));
#114013=DIRECTION('',(0.309016994374957,0.95105651629515,-4.35148173242984E-17));
#114014=DIRECTION('center_axis',(-1.4081690688991E-16,0.,-1.));
#114015=DIRECTION('ref_axis',(-1.,0.,1.4081690688991E-16));
#114016=DIRECTION('center_axis',(-1.4081690688991E-16,0.,-1.));
#114017=DIRECTION('ref_axis',(-1.,0.,1.4081690688991E-16));
#114018=DIRECTION('center_axis',(-1.4081690688991E-16,0.,-1.));
#114019=DIRECTION('ref_axis',(-1.,0.,1.4081690688991E-16));
#114020=DIRECTION('',(-0.20791169081777,-0.978147600733803,2.92774812072098E-17));
#114021=DIRECTION('center_axis',(1.4081690688991E-16,0.,1.));
#114022=DIRECTION('ref_axis',(1.,0.,-1.4081690688991E-16));
#114023=DIRECTION('',(0.154514645521724,0.475531718838029,0.866022406579787));
#114024=DIRECTION('center_axis',(1.4081690688991E-16,0.,1.));
#114025=DIRECTION('ref_axis',(-1.,3.10862446895044E-14,1.40816906889911E-16));
#114026=DIRECTION('',(-0.103952251140494,-0.489079871579877,-0.86602240657978));
#114027=DIRECTION('center_axis',(-1.4081690688991E-16,0.,-1.));
#114028=DIRECTION('ref_axis',(-1.,0.,1.40816906889911E-16));
#114029=DIRECTION('center_axis',(-1.4081690688991E-16,0.,-1.));
#114030=DIRECTION('ref_axis',(-1.,0.,1.4081690688991E-16));
#114031=DIRECTION('',(0.309016994374957,0.95105651629515,-4.35148173242984E-17));
#114032=DIRECTION('center_axis',(1.4081690688991E-16,0.,1.));
#114033=DIRECTION('ref_axis',(-1.,3.10862446895044E-14,1.4081690688991E-16));
#114034=DIRECTION('',(-0.20791169081777,-0.978147600733803,2.92774812072098E-17));
#114035=DIRECTION('center_axis',(-1.4081690688991E-16,0.,-1.));
#114036=DIRECTION('ref_axis',(-1.,0.,1.4081690688991E-16));
#114037=DIRECTION('center_axis',(-1.4081690688991E-16,0.,-1.));
#114038=DIRECTION('ref_axis',(1.,-3.5527136788005E-14,-1.4081690688991E-16));
#114039=DIRECTION('',(0.154505638525956,0.475534435652422,-0.866022521746646));
#114040=DIRECTION('center_axis',(-1.4081690688991E-16,0.,-1.));
#114041=DIRECTION('ref_axis',(-1.,0.,1.4081690688991E-16));
#114042=DIRECTION('center_axis',(-1.4081690688991E-16,0.,-1.));
#114043=DIRECTION('ref_axis',(-1.,0.,1.4081690688991E-16));
#114044=DIRECTION('center_axis',(-1.4081690688991E-16,0.,-1.));
#114045=DIRECTION('ref_axis',(-1.,0.,1.4081690688991E-16));
#114046=DIRECTION('',(-0.103961409834817,-0.489077720912241,0.866022521746661));
#114047=DIRECTION('center_axis',(-1.4081690688991E-16,0.,-1.));
#114048=DIRECTION('ref_axis',(-1.,0.,1.40816906889911E-16));
#114049=DIRECTION('',(0.309016994374957,0.95105651629515,-4.35148173242984E-17));
#114050=DIRECTION('center_axis',(1.4081690688991E-16,0.,1.));
#114051=DIRECTION('ref_axis',(-1.,0.,1.4081690688991E-16));
#114052=DIRECTION('',(-0.20791169081777,-0.978147600733803,2.92774812072098E-17));
#114053=DIRECTION('center_axis',(-1.4081690688991E-16,0.,-1.));
#114054=DIRECTION('ref_axis',(-1.,0.,1.17174841180864E-16));
#114055=DIRECTION('center_axis',(0.951386698854214,-0.307998943474534,7.86457199139798E-6));
#114056=DIRECTION('ref_axis',(7.93337931586199E-6,-1.02877117099849E-6,
-0.999999999968002));
#114057=DIRECTION('center_axis',(-0.977924521767597,0.208958440039556,7.86457226078363E-6));
#114058=DIRECTION('ref_axis',(-0.177210199190864,-0.829322958353517,-0.529924500330476));
#114059=DIRECTION('center_axis',(-1.4081690688991E-16,0.,-1.));
#114060=DIRECTION('ref_axis',(-1.,0.,1.13676889660403E-16));
#114061=DIRECTION('center_axis',(0.951372650655522,-0.308042333923799,-9.77058865439169E-6));
#114062=DIRECTION('ref_axis',(0.269431182533645,0.832108751235234,0.484769908303168));
#114063=DIRECTION('center_axis',(-0.977934050903654,0.208913838669691,-9.77051656141964E-6));
#114064=DIRECTION('ref_axis',(0.182721698612562,0.855350264826251,0.484756336026464));
#114065=DIRECTION('center_axis',(-1.4081690688991E-16,0.,-1.));
#114066=DIRECTION('ref_axis',(-1.,0.,1.15974593313694E-16));
#114067=DIRECTION('center_axis',(-0.950250383060598,0.311487093092654,1.81624798101011E-5));
#114068=DIRECTION('ref_axis',(0.269503948347349,0.822202080225929,-0.501349539839565));
#114069=DIRECTION('center_axis',(0.978684514577293,-0.205369473383585,1.8131645285516E-5));
#114070=DIRECTION('ref_axis',(0.178060372502838,0.848499490341508,-0.498340364243508));
#114071=DIRECTION('center_axis',(-1.4081690688991E-16,0.,-1.));
#114072=DIRECTION('ref_axis',(-1.,0.,1.16261524579732E-16));
#114073=DIRECTION('center_axis',(-0.950246174164386,0.311499932815269,1.84940638835828E-5));
#114074=DIRECTION('ref_axis',(0.270073604474708,0.82384349413839,0.498339387698673));
#114075=DIRECTION('center_axis',(0.978687289329817,-0.205356249870933,1.85257154385723E-5));
#114076=DIRECTION('ref_axis',(0.17767446928848,0.846806623514623,0.501348506864058));
#114077=DIRECTION('center_axis',(-1.4081690688991E-16,0.,-1.));
#114078=DIRECTION('ref_axis',(-1.,0.,1.40816906889911E-16));
#114079=DIRECTION('center_axis',(-1.4081690688991E-16,0.,-1.));
#114080=DIRECTION('ref_axis',(-1.,0.,1.4081690688991E-16));
#114081=DIRECTION('',(0.20791169081777,0.978147600733803,-2.92774812072098E-17));
#114082=DIRECTION('center_axis',(-1.4081690688991E-16,0.,-1.));
#114083=DIRECTION('ref_axis',(-1.,0.,1.4081690688991E-16));
#114084=DIRECTION('center_axis',(-1.4081690688991E-16,0.,-1.));
#114085=DIRECTION('ref_axis',(-1.,0.,1.4081690688991E-16));
#114086=DIRECTION('center_axis',(-1.4081690688991E-16,0.,-1.));
#114087=DIRECTION('ref_axis',(-1.,0.,1.4081690688991E-16));
#114088=DIRECTION('',(-0.104528463267664,-0.994521895368272,1.4719374879308E-17));
#114089=DIRECTION('center_axis',(1.4081690688991E-16,0.,1.));
#114090=DIRECTION('ref_axis',(1.,0.,-1.4081690688991E-16));
#114091=DIRECTION('',(0.103961598321227,0.489077884775272,0.866022406579785));
#114092=DIRECTION('center_axis',(1.4081690688991E-16,0.,1.));
#114093=DIRECTION('ref_axis',(-1.,3.19744231092045E-14,1.40816906889911E-16));
#114094=DIRECTION('',(-0.0522600224406464,-0.497266609935041,-0.866022406579769));
#114095=DIRECTION('center_axis',(-1.4081690688991E-16,0.,-1.));
#114096=DIRECTION('ref_axis',(-1.,0.,1.40816906889911E-16));
#114097=DIRECTION('center_axis',(-1.4081690688991E-16,0.,-1.));
#114098=DIRECTION('ref_axis',(-1.,0.,1.4081690688991E-16));
#114099=DIRECTION('',(0.20791169081777,0.978147600733803,-2.92774812072098E-17));
#114100=DIRECTION('center_axis',(1.4081690688991E-16,0.,1.));
#114101=DIRECTION('ref_axis',(-1.,3.19744231092045E-14,1.4081690688991E-16));
#114102=DIRECTION('',(-0.104528463267664,-0.994521895368272,1.4719374879308E-17));
#114103=DIRECTION('center_axis',(-1.4081690688991E-16,0.,-1.));
#114104=DIRECTION('ref_axis',(-1.,0.,1.4081690688991E-16));
#114105=DIRECTION('center_axis',(-1.4081690688991E-16,0.,-1.));
#114106=DIRECTION('ref_axis',(1.,-2.30926389122033E-14,-1.4081690688991E-16));
#114107=DIRECTION('',(0.103952356682314,0.489079645219224,-0.866022521746652));
#114108=DIRECTION('center_axis',(-1.4081690688991E-16,0.,-1.));
#114109=DIRECTION('ref_axis',(-1.,0.,1.4081690688991E-16));
#114110=DIRECTION('center_axis',(-1.4081690688991E-16,0.,-1.));
#114111=DIRECTION('ref_axis',(-1.,0.,1.4081690688991E-16));
#114112=DIRECTION('center_axis',(-1.4081690688991E-16,0.,-1.));
#114113=DIRECTION('ref_axis',(-1.,0.,1.4081690688991E-16));
#114114=DIRECTION('',(-0.0522693557686642,-0.497265428393217,0.866022521746657));
#114115=DIRECTION('center_axis',(-1.4081690688991E-16,0.,-1.));
#114116=DIRECTION('ref_axis',(-1.,0.,1.40816906889911E-16));
#114117=DIRECTION('',(0.20791169081777,0.978147600733803,-2.92774812072098E-17));
#114118=DIRECTION('center_axis',(1.4081690688991E-16,0.,1.));
#114119=DIRECTION('ref_axis',(-1.,-1.06581410364015E-14,1.4081690688991E-16));
#114120=DIRECTION('',(-0.104528463267664,-0.994521895368272,1.4719374879308E-17));
#114121=DIRECTION('center_axis',(-1.4081690688991E-16,0.,-1.));
#114122=DIRECTION('ref_axis',(-1.,0.,1.17174841180864E-16));
#114123=DIRECTION('center_axis',(0.978369559222101,-0.206864703431254,7.86457189883735E-6));
#114124=DIRECTION('ref_axis',(7.99745522015369E-6,-1.93871454059186E-7,
-0.999999999968002));
#114125=DIRECTION('center_axis',(-0.994409453539563,0.105592796389223,7.86457226736407E-6));
#114126=DIRECTION('ref_axis',(-0.0895515687886208,-0.843303350210948,-0.52992450033046));
#114127=DIRECTION('center_axis',(-1.4081690688991E-16,0.,-1.));
#114128=DIRECTION('ref_axis',(-1.,0.,1.13676889660403E-16));
#114129=DIRECTION('center_axis',(0.978360123517394,-0.206909324622083,-9.77058422961358E-6));
#114130=DIRECTION('ref_axis',(0.180976161286691,0.855713599898502,0.484769908301536));
#114131=DIRECTION('center_axis',(-0.994414268361316,0.105547443284838,-9.77051740477596E-6));
#114132=DIRECTION('ref_axis',(0.0923122812912943,0.8697641849412,0.484756336024984));
#114133=DIRECTION('center_axis',(-1.4081690688991E-16,0.,-1.));
#114134=DIRECTION('ref_axis',(-1.,0.,1.15974593313694E-16));
#114135=DIRECTION('center_axis',(-0.977604079204545,0.210452521944402,1.81624797242626E-5));
#114136=DIRECTION('ref_axis',(0.182084057577939,0.845868804766277,-0.50134953984144));
#114137=DIRECTION('center_axis',(0.994790133859855,-0.101944049587677,1.81316451691771E-5));
#114138=DIRECTION('ref_axis',(0.0883925913421295,0.862463698454322,-0.498340364253505));
#114139=DIRECTION('center_axis',(-1.4081690688991E-16,0.,-1.));
#114140=DIRECTION('ref_axis',(-1.,0.,1.16261524579732E-16));
#114141=DIRECTION('center_axis',(-0.977601235480913,0.210465731282227,1.84940584797882E-5));
#114142=DIRECTION('ref_axis',(0.18247901859632,0.847560772124576,0.498339387694488));
#114143=DIRECTION('center_axis',(0.99479151117881,-0.101930608471533,1.85257109318316E-5));
#114144=DIRECTION('ref_axis',(0.0881857549144228,0.860739767464254,0.50134850686499));
#114145=DIRECTION('center_axis',(-1.4081690688991E-16,0.,-1.));
#114146=DIRECTION('ref_axis',(-1.,0.,1.40816906889911E-16));
#114147=DIRECTION('center_axis',(-1.4081690688991E-16,0.,-1.));
#114148=DIRECTION('ref_axis',(-1.,0.,1.4081690688991E-16));
#114149=DIRECTION('',(0.104528463267664,0.994521895368272,-1.4719374879308E-17));
#114150=DIRECTION('center_axis',(-1.4081690688991E-16,0.,-1.));
#114151=DIRECTION('ref_axis',(-1.,0.,1.4081690688991E-16));
#114152=DIRECTION('center_axis',(-1.4081690688991E-16,0.,-1.));
#114153=DIRECTION('ref_axis',(-1.,0.,1.4081690688991E-16));
#114154=DIRECTION('center_axis',(-1.4081690688991E-16,0.,-1.));
#114155=DIRECTION('ref_axis',(-1.,0.,1.4081690688991E-16));
#114156=DIRECTION('',(-1.04744440165294E-14,-1.,1.4749788077992E-30));
#114157=DIRECTION('center_axis',(1.4081690688991E-16,0.,1.));
#114158=DIRECTION('ref_axis',(1.,0.,-1.4081690688991E-16));
#114159=DIRECTION('',(0.0522695260941979,0.497265611060806,0.866022406579767));
#114160=DIRECTION('center_axis',(1.4081690688991E-16,0.,1.));
#114161=DIRECTION('ref_axis',(-1.,-1.06581410364015E-14,1.40816906889911E-16));
#114162=DIRECTION('',(4.7780011601864E-6,-0.500005191252011,-0.866022406579767));
#114163=DIRECTION('center_axis',(-1.4081690688991E-16,0.,-1.));
#114164=DIRECTION('ref_axis',(-1.,0.,1.40816906889911E-16));
#114165=DIRECTION('center_axis',(-1.4081690688991E-16,0.,-1.));
#114166=DIRECTION('ref_axis',(-1.,0.,1.4081690688991E-16));
#114167=DIRECTION('',(0.104528463267664,0.994521895368272,-1.4719374879308E-17));
#114168=DIRECTION('center_axis',(1.4081690688991E-16,0.,1.));
#114169=DIRECTION('ref_axis',(-1.,-1.06581410364015E-14,1.4081690688991E-16));
#114170=DIRECTION('',(-1.04744440165294E-14,-1.,1.4749788077992E-30));
#114171=DIRECTION('center_axis',(-1.4081690688991E-16,0.,-1.));
#114172=DIRECTION('ref_axis',(-1.,0.,1.4081690688991E-16));
#114173=DIRECTION('center_axis',(-1.4081690688991E-16,0.,-1.));
#114174=DIRECTION('ref_axis',(1.,2.30926389122033E-14,-1.4081690688991E-16));
#114175=DIRECTION('',(0.0522601510654366,0.497266395846486,-0.866022521746671));
#114176=DIRECTION('center_axis',(-1.4081690688991E-16,0.,-1.));
#114177=DIRECTION('ref_axis',(-1.,0.,1.4081690688991E-16));
#114178=DIRECTION('center_axis',(-1.4081690688991E-16,0.,-1.));
#114179=DIRECTION('ref_axis',(-1.,0.,1.4081690688991E-16));
#114180=DIRECTION('center_axis',(-1.4081690688991E-16,0.,-1.));
#114181=DIRECTION('ref_axis',(-1.,0.,1.4081690688991E-16));
#114182=DIRECTION('',(-4.62770265767274E-6,-0.500004991781207,0.866022521746669));
#114183=DIRECTION('center_axis',(-1.4081690688991E-16,0.,-1.));
#114184=DIRECTION('ref_axis',(-1.,0.,1.40816906889911E-16));
#114185=DIRECTION('',(0.104528463267664,0.994521895368272,-1.4719374879308E-17));
#114186=DIRECTION('center_axis',(1.4081690688991E-16,0.,1.));
#114187=DIRECTION('ref_axis',(-1.,3.28626015289046E-14,1.4081690688991E-16));
#114188=DIRECTION('',(-1.04744440165294E-14,-1.,1.4749788077992E-30));
#114189=DIRECTION('center_axis',(-1.4081690688991E-16,0.,-1.));
#114190=DIRECTION('ref_axis',(-1.,0.,1.17174841180864E-16));
#114191=DIRECTION('center_axis',(0.994633197962181,-0.10346401040784,7.86457202285898E-6));
#114192=DIRECTION('ref_axis',(7.9739095298375E-6,6.43152272453734E-7,-0.999999999968002));
#114193=DIRECTION('center_axis',(-0.999999427244995,0.00107025596491883,
7.86457225228283E-6));
#114194=DIRECTION('ref_axis',(-0.000911792658831313,-0.848044334090885,
-0.529924500330466));
#114195=DIRECTION('center_axis',(-1.4081690688991E-16,0.,-1.));
#114196=DIRECTION('ref_axis',(-1.,0.,1.13676889660403E-16));
#114197=DIRECTION('center_axis',(0.994628478131884,-0.103509373457613,-9.77058644365307E-6));
#114198=DIRECTION('ref_axis',(0.0905383273445195,0.869943071289731,0.484769908303565));
#114199=DIRECTION('center_axis',(-0.999999475000345,0.00102464802306588,
-9.77051628361053E-6));
#114200=DIRECTION('ref_axis',(0.000891471298449509,0.874648786634599,0.484756336026202));
#114201=DIRECTION('center_axis',(-1.4081690688991E-16,0.,-1.));
#114202=DIRECTION('ref_axis',(-1.,0.,1.15974593313694E-16));
#114203=DIRECTION('center_axis',(-0.994246940479911,0.107112188925725,1.81624797550156E-5));
#114204=DIRECTION('ref_axis',(0.0926692157708285,0.860268013676602,-0.501349539835565));
#114205=DIRECTION('center_axis',(0.999996624262643,0.00259829454877897,
1.81316452302667E-5));
#114206=DIRECTION('ref_axis',(0.00224363754547992,-0.866978573809519,0.49834036425497));
#114207=DIRECTION('center_axis',(-1.4081690688991E-16,0.,-1.));
#114208=DIRECTION('ref_axis',(-1.,0.,1.16261524579732E-16));
#114209=DIRECTION('center_axis',(-0.994245493086384,0.107125623150498,1.84940602737029E-5));
#114210=DIRECTION('ref_axis',(0.0928851544029117,0.861991996922407,0.498339387700057));
#114211=DIRECTION('center_axis',(0.999996589057286,0.00261180600211936,
1.85257108473802E-5));
#114212=DIRECTION('ref_axis',(0.00226914104442804,-0.865242466405379,-0.501348506856913));
#114213=DIRECTION('center_axis',(-1.4081690688991E-16,0.,-1.));
#114214=DIRECTION('ref_axis',(-1.,0.,1.40816906889911E-16));
#114215=DIRECTION('center_axis',(-1.4081690688991E-16,0.,-1.));
#114216=DIRECTION('ref_axis',(-1.,0.,1.4081690688991E-16));
#114217=DIRECTION('',(1.04744440165294E-14,1.,-1.4749788077992E-30));
#114218=DIRECTION('center_axis',(-1.4081690688991E-16,0.,-1.));
#114219=DIRECTION('ref_axis',(-1.,0.,1.4081690688991E-16));
#114220=DIRECTION('center_axis',(-1.4081690688991E-16,0.,-1.));
#114221=DIRECTION('ref_axis',(-1.,0.,1.4081690688991E-16));
#114222=DIRECTION('center_axis',(-1.4081690688991E-16,0.,-1.));
#114223=DIRECTION('ref_axis',(-1.,0.,1.4081690688991E-16));
#114224=DIRECTION('',(0.104528463267644,-0.994521895368274,-1.47193748793052E-17));
#114225=DIRECTION('center_axis',(1.4081690688991E-16,0.,1.));
#114226=DIRECTION('ref_axis',(1.,0.,-1.4081690688991E-16));
#114227=DIRECTION('',(4.77800117084857E-6,0.500005191252011,0.866022406579767));
#114228=DIRECTION('center_axis',(1.4081690688991E-16,0.,1.));
#114229=DIRECTION('ref_axis',(-1.,-1.15463194561016E-14,1.40816906889911E-16));
#114230=DIRECTION('',(0.0522695260941891,-0.497265611060765,-0.866022406579791));
#114231=DIRECTION('center_axis',(-1.4081690688991E-16,0.,-1.));
#114232=DIRECTION('ref_axis',(-1.,0.,1.40816906889911E-16));
#114233=DIRECTION('center_axis',(-1.4081690688991E-16,0.,-1.));
#114234=DIRECTION('ref_axis',(-1.,0.,1.4081690688991E-16));
#114235=DIRECTION('',(1.04744440165294E-14,1.,-1.4749788077992E-30));
#114236=DIRECTION('center_axis',(1.4081690688991E-16,0.,1.));
#114237=DIRECTION('ref_axis',(-1.,-1.06581410364015E-14,1.4081690688991E-16));
#114238=DIRECTION('',(0.104528463267644,-0.994521895368274,-1.47193748793052E-17));
#114239=DIRECTION('center_axis',(-1.4081690688991E-16,0.,-1.));
#114240=DIRECTION('ref_axis',(-1.,0.,1.4081690688991E-16));
#114241=DIRECTION('center_axis',(-1.4081690688991E-16,0.,-1.));
#114242=DIRECTION('ref_axis',(1.,2.1316282072803E-14,-1.4081690688991E-16));
#114243=DIRECTION('',(-4.62770264722375E-6,0.500004991781227,-0.866022521746657));
#114244=DIRECTION('center_axis',(-1.4081690688991E-16,0.,-1.));
#114245=DIRECTION('ref_axis',(-1.,0.,1.4081690688991E-16));
#114246=DIRECTION('center_axis',(-1.4081690688991E-16,0.,-1.));
#114247=DIRECTION('ref_axis',(-1.,0.,1.4081690688991E-16));
#114248=DIRECTION('center_axis',(-1.4081690688991E-16,0.,-1.));
#114249=DIRECTION('ref_axis',(-1.,0.,1.4081690688991E-16));
#114250=DIRECTION('',(0.0522601510654256,-0.497266395846507,0.86602252174666));
#114251=DIRECTION('center_axis',(-1.4081690688991E-16,0.,-1.));
#114252=DIRECTION('ref_axis',(-1.,0.,1.40816906889911E-16));
#114253=DIRECTION('',(1.04744440165294E-14,1.,-1.4749788077992E-30));
#114254=DIRECTION('center_axis',(1.4081690688991E-16,0.,1.));
#114255=DIRECTION('ref_axis',(-1.,3.37507799486048E-14,1.4081690688991E-16));
#114256=DIRECTION('',(0.104528463267644,-0.994521895368274,-1.47193748793052E-17));
#114257=DIRECTION('center_axis',(-1.4081690688991E-16,0.,-1.));
#114258=DIRECTION('ref_axis',(-1.,0.,1.17174841180864E-16));
#114259=DIRECTION('center_axis',(0.999999427244995,0.00107025596477238,
7.86457202530897E-6));
#114260=DIRECTION('ref_axis',(7.86299990295297E-6,1.47312952164186E-6,-0.999999999968002));
#114261=DIRECTION('center_axis',(-0.994633197962196,-0.103464010407698,
7.86457224226079E-6));
#114262=DIRECTION('ref_axis',(0.0877379732621283,-0.843493966781848,-0.529924500330449));
#114263=DIRECTION('center_axis',(-1.4081690688991E-16,0.,-1.));
#114264=DIRECTION('ref_axis',(-1.,0.,1.13676889660403E-16));
#114265=DIRECTION('center_axis',(0.999999475000305,0.00102464806172845,
-9.77058609196671E-6));
#114266=DIRECTION('ref_axis',(0.000891463458114906,-0.874641264346845,-0.48476990830151));
#114267=DIRECTION('center_axis',(-0.994628478127934,-0.103509373495574,
-9.77051754500418E-6));
#114268=DIRECTION('ref_axis',(0.0905391058403081,-0.869950553189016,-0.484756336028486));
#114269=DIRECTION('center_axis',(-1.4081690688991E-16,0.,-1.));
#114270=DIRECTION('ref_axis',(-1.,0.,1.15974593313694E-16));
#114271=DIRECTION('center_axis',(-0.999996624215829,0.00259831235054303,
1.81624797937814E-5));
#114272=DIRECTION('ref_axis',(0.0022390706427464,0.86524194619802,-0.501349539844328));
#114273=DIRECTION('center_axis',(0.994246942387258,0.107112171226391,1.81316452305702E-5));
#114274=DIRECTION('ref_axis',(0.0928552846705921,-0.861994650484445,0.498340364254134));
#114275=DIRECTION('center_axis',(-1.4081690688991E-16,0.,-1.));
#114276=DIRECTION('ref_axis',(-1.,0.,1.16261524579732E-16));
#114277=DIRECTION('center_axis',(-0.999996589010146,0.0026118242750869,
1.84940601186701E-5));
#114278=DIRECTION('ref_axis',(0.00227362102102081,0.866979057023919,0.498339387696144));
#114279=DIRECTION('center_axis',(0.994245495043238,0.107125604983238,1.85257097596897E-5));
#114280=DIRECTION('ref_axis',(0.0926991758193815,-0.860265387814003,-0.501348506860876));
#114281=DIRECTION('center_axis',(-1.4081690688991E-16,0.,-1.));
#114282=DIRECTION('ref_axis',(-1.,0.,1.40816906889911E-16));
#114283=DIRECTION('center_axis',(-1.4081690688991E-16,0.,-1.));
#114284=DIRECTION('ref_axis',(-1.,0.,1.4081690688991E-16));
#114285=DIRECTION('',(-0.104528463267644,0.994521895368274,1.47193748793052E-17));
#114286=DIRECTION('center_axis',(-1.4081690688991E-16,0.,-1.));
#114287=DIRECTION('ref_axis',(-1.,0.,1.4081690688991E-16));
#114288=DIRECTION('center_axis',(-1.4081690688991E-16,0.,-1.));
#114289=DIRECTION('ref_axis',(-1.,0.,1.4081690688991E-16));
#114290=DIRECTION('center_axis',(-1.4081690688991E-16,0.,-1.));
#114291=DIRECTION('ref_axis',(-1.,0.,1.4081690688991E-16));
#114292=DIRECTION('',(0.207911690817749,-0.978147600733808,-2.92774812072069E-17));
#114293=DIRECTION('center_axis',(1.4081690688991E-16,0.,1.));
#114294=DIRECTION('ref_axis',(1.,0.,-1.4081690688991E-16));
#114295=DIRECTION('',(-0.0522600224406444,0.497266609935,0.866022406579793));
#114296=DIRECTION('center_axis',(1.4081690688991E-16,0.,1.));
#114297=DIRECTION('ref_axis',(-1.,3.37507799486048E-14,1.40816906889911E-16));
#114298=DIRECTION('',(0.103961598321227,-0.489077884775272,-0.866022406579785));
#114299=DIRECTION('center_axis',(-1.4081690688991E-16,0.,-1.));
#114300=DIRECTION('ref_axis',(-1.,0.,1.40816906889911E-16));
#114301=DIRECTION('center_axis',(-1.4081690688991E-16,0.,-1.));
#114302=DIRECTION('ref_axis',(-1.,0.,1.4081690688991E-16));
#114303=DIRECTION('',(-0.104528463267644,0.994521895368274,1.47193748793052E-17));
#114304=DIRECTION('center_axis',(1.4081690688991E-16,0.,1.));
#114305=DIRECTION('ref_axis',(-1.,3.46389583683049E-14,1.4081690688991E-16));
#114306=DIRECTION('',(0.207911690817749,-0.978147600733808,-2.92774812072069E-17));
#114307=DIRECTION('center_axis',(-1.4081690688991E-16,0.,-1.));
#114308=DIRECTION('ref_axis',(-1.,0.,1.4081690688991E-16));
#114309=DIRECTION('center_axis',(-1.4081690688991E-16,0.,-1.));
#114310=DIRECTION('ref_axis',(1.,-2.1316282072803E-14,-1.4081690688991E-16));
#114311=DIRECTION('',(-0.0522693557686574,0.497265428393217,-0.866022521746658));
#114312=DIRECTION('center_axis',(-1.4081690688991E-16,0.,-1.));
#114313=DIRECTION('ref_axis',(-1.,0.,1.4081690688991E-16));
#114314=DIRECTION('center_axis',(-1.4081690688991E-16,0.,-1.));
#114315=DIRECTION('ref_axis',(-1.,0.,1.4081690688991E-16));
#114316=DIRECTION('center_axis',(-1.4081690688991E-16,0.,-1.));
#114317=DIRECTION('ref_axis',(-1.,0.,1.4081690688991E-16));
#114318=DIRECTION('',(0.103952356682308,-0.489079645219204,0.866022521746664));
#114319=DIRECTION('center_axis',(-1.4081690688991E-16,0.,-1.));
#114320=DIRECTION('ref_axis',(-1.,0.,1.40816906889911E-16));
#114321=DIRECTION('',(-0.104528463267644,0.994521895368274,1.47193748793052E-17));
#114322=DIRECTION('center_axis',(1.4081690688991E-16,0.,1.));
#114323=DIRECTION('ref_axis',(-1.,-1.06581410364015E-14,1.4081690688991E-16));
#114324=DIRECTION('',(0.207911690817749,-0.978147600733808,-2.92774812072069E-17));
#114325=DIRECTION('center_axis',(-1.4081690688991E-16,0.,-1.));
#114326=DIRECTION('ref_axis',(-1.,0.,1.17174841180864E-16));
#114327=DIRECTION('center_axis',(0.994409453539581,0.105592796389056,7.86457200107375E-6));
#114328=DIRECTION('ref_axis',(7.66594157259133E-6,2.28696690243279E-6,-0.999999999968002));
#114329=DIRECTION('center_axis',(-0.978369559222145,-0.206864703431043,
7.86457225237907E-6));
#114330=DIRECTION('ref_axis',(0.175426463587655,-0.82970210306027,-0.529924500330466));
#114331=DIRECTION('center_axis',(-1.4081690688991E-16,0.,-1.));
#114332=DIRECTION('ref_axis',(-1.,0.,1.13676889660403E-16));
#114333=DIRECTION('center_axis',(0.994414268357315,0.105547443322528,-9.77058581902262E-6));
#114334=DIRECTION('ref_axis',(0.0923114872006239,-0.869756704679759,-0.484769908302295));
#114335=DIRECTION('center_axis',(-0.978360123509492,-0.206909324659449,
-9.77051516979182E-6));
#114336=DIRECTION('ref_axis',(0.180977717589048,-0.85572095943558,-0.484756336027606));
#114337=DIRECTION('center_axis',(-1.4081690688991E-16,0.,-1.));
#114338=DIRECTION('ref_axis',(-1.,0.,1.15974593313694E-16));
#114339=DIRECTION('center_axis',(-0.994790135674097,-0.101944031878453,
1.81624797954842E-5));
#114340=DIRECTION('ref_axis',(0.0882156062112984,-0.860736106898752,0.501349539843762));
#114341=DIRECTION('center_axis',(0.97760408295153,0.210452504541384,1.81316452299228E-5));
#114342=DIRECTION('ref_axis',(0.182449589866239,-0.847566533387013,0.498340364249137));
#114343=DIRECTION('center_axis',(-1.4081690688991E-16,0.,-1.));
#114344=DIRECTION('ref_axis',(-1.,0.,1.16261524579732E-16));
#114345=DIRECTION('center_axis',(-0.994791513041914,-0.101930590294321,
1.84940611814327E-5));
#114346=DIRECTION('ref_axis',(0.0883628226288923,-0.862467313148419,-0.498339387694373));
#114347=DIRECTION('center_axis',(0.977601239326121,0.210465713418671,1.85257086791728E-5));
#114348=DIRECTION('ref_axis',(0.182113579025865,-0.84586306161554,-0.501348506858029));
#114349=DIRECTION('center_axis',(-1.4081690688991E-16,0.,-1.));
#114350=DIRECTION('ref_axis',(-1.,0.,1.40816906889911E-16));
#114351=DIRECTION('center_axis',(-1.4081690688991E-16,0.,-1.));
#114352=DIRECTION('ref_axis',(-1.,0.,1.4081690688991E-16));
#114353=DIRECTION('',(-0.207911690817749,0.978147600733808,2.92774812072069E-17));
#114354=DIRECTION('center_axis',(-1.4081690688991E-16,0.,-1.));
#114355=DIRECTION('ref_axis',(-1.,0.,1.4081690688991E-16));
#114356=DIRECTION('center_axis',(-1.4081690688991E-16,0.,-1.));
#114357=DIRECTION('ref_axis',(-1.,0.,1.4081690688991E-16));
#114358=DIRECTION('center_axis',(-1.4081690688991E-16,0.,-1.));
#114359=DIRECTION('ref_axis',(-1.,0.,1.4081690688991E-16));
#114360=DIRECTION('',(0.309016994374938,-0.951056516295157,-4.35148173242957E-17));
#114361=DIRECTION('center_axis',(1.4081690688991E-16,0.,1.));
#114362=DIRECTION('ref_axis',(1.,0.,-1.4081690688991E-16));
#114363=DIRECTION('',(-0.103952251140481,0.489079871579878,0.866022406579781));
#114364=DIRECTION('center_axis',(1.4081690688991E-16,0.,1.));
#114365=DIRECTION('ref_axis',(-1.,3.46389583683049E-14,1.40816906889911E-16));
#114366=DIRECTION('',(0.154514645521709,-0.475531718838051,-0.866022406579778));
#114367=DIRECTION('center_axis',(-1.4081690688991E-16,0.,-1.));
#114368=DIRECTION('ref_axis',(-1.,0.,1.40816906889911E-16));
#114369=DIRECTION('center_axis',(-1.4081690688991E-16,0.,-1.));
#114370=DIRECTION('ref_axis',(-1.,0.,1.4081690688991E-16));
#114371=DIRECTION('',(-0.207911690817749,0.978147600733808,2.92774812072069E-17));
#114372=DIRECTION('center_axis',(1.4081690688991E-16,0.,1.));
#114373=DIRECTION('ref_axis',(-1.,3.5527136788005E-14,1.4081690688991E-16));
#114374=DIRECTION('',(0.309016994374938,-0.951056516295157,-4.35148173242957E-17));
#114375=DIRECTION('center_axis',(-1.4081690688991E-16,0.,-1.));
#114376=DIRECTION('ref_axis',(-1.,0.,1.4081690688991E-16));
#114377=DIRECTION('center_axis',(-1.4081690688991E-16,0.,-1.));
#114378=DIRECTION('ref_axis',(1.,-2.1316282072803E-14,-1.4081690688991E-16));
#114379=DIRECTION('',(-0.103961409834804,0.489077720912242,-0.866022521746662));
#114380=DIRECTION('center_axis',(-1.4081690688991E-16,0.,-1.));
#114381=DIRECTION('ref_axis',(-1.,0.,1.4081690688991E-16));
#114382=DIRECTION('center_axis',(-1.4081690688991E-16,0.,-1.));
#114383=DIRECTION('ref_axis',(-1.,0.,1.4081690688991E-16));
#114384=DIRECTION('center_axis',(-1.4081690688991E-16,0.,-1.));
#114385=DIRECTION('ref_axis',(-1.,0.,1.4081690688991E-16));
#114386=DIRECTION('',(0.154505638525955,-0.475534435652359,0.86602252174668));
#114387=DIRECTION('center_axis',(-1.4081690688991E-16,0.,-1.));
#114388=DIRECTION('ref_axis',(-1.,0.,1.40816906889911E-16));
#114389=DIRECTION('',(-0.207911690817749,0.978147600733808,2.92774812072069E-17));
#114390=DIRECTION('center_axis',(1.4081690688991E-16,0.,1.));
#114391=DIRECTION('ref_axis',(-1.,0.,1.4081690688991E-16));
#114392=DIRECTION('',(0.309016994374938,-0.951056516295157,-4.35148173242957E-17));
#114393=DIRECTION('center_axis',(-1.4081690688991E-16,0.,-1.));
#114394=DIRECTION('ref_axis',(-1.,0.,1.17174841180864E-16));
#114395=DIRECTION('center_axis',(0.977924521767646,0.208958440039328,7.86457187141246E-6));
#114396=DIRECTION('ref_axis',(7.38489348936258E-6,3.07574769236174E-6,-0.999999999968002));
#114397=DIRECTION('center_axis',(-0.951386698854274,-0.307998943474349,
7.86457230114699E-6));
#114398=DIRECTION('ref_axis',(0.261192944867729,-0.80681984947127,-0.529924500330453));
#114399=DIRECTION('center_axis',(-1.4081690688991E-16,0.,-1.));
#114400=DIRECTION('ref_axis',(-1.,0.,1.13676889660403E-16));
#114401=DIRECTION('center_axis',(0.977934050896062,0.208913838705231,-9.77058216020036E-6));
#114402=DIRECTION('ref_axis',(0.182720126971813,-0.855342908547742,-0.484769908303406));
#114403=DIRECTION('center_axis',(-0.951372650642299,-0.308042333964641,
-9.77051105240763E-6));
#114404=DIRECTION('ref_axis',(0.269433499591965,-0.832115907779489,-0.48475633602661));
#114405=DIRECTION('center_axis',(-1.4081690688991E-16,0.,-1.));
#114406=DIRECTION('ref_axis',(-1.,0.,1.15974593313694E-16));
#114407=DIRECTION('center_axis',(-0.978684518232684,-0.205369455961164,
1.81624797100977E-5));
#114408=DIRECTION('ref_axis',(0.177703774423794,-0.846799862692929,0.501349539840991));
#114409=DIRECTION('center_axis',(0.950250388606192,0.311487076176564,1.81316452056593E-5));
#114410=DIRECTION('ref_axis',(0.270044939174703,-0.823852299981494,0.498340364250513));
#114411=DIRECTION('center_axis',(-1.4081690688991E-16,0.,-1.));
#114412=DIRECTION('ref_axis',(-1.,0.,1.16261524579732E-16));
#114413=DIRECTION('center_axis',(-0.978687293084006,-0.205356231982065,
1.84940551457799E-5));
#114414=DIRECTION('ref_axis',(0.178031144703053,-0.848506196906717,-0.498339387693387));
#114415=DIRECTION('center_axis',(0.9502461798562,0.311499915450223,1.85257163965025E-5));
#114416=DIRECTION('ref_axis',(0.269532707749906,-0.822193282701928,-0.501348506862074));
#114417=DIRECTION('center_axis',(-1.4081690688991E-16,0.,-1.));
#114418=DIRECTION('ref_axis',(-1.,0.,1.40816906889911E-16));
#114419=DIRECTION('center_axis',(-1.4081690688991E-16,0.,-1.));
#114420=DIRECTION('ref_axis',(-1.,0.,1.4081690688991E-16));
#114421=DIRECTION('',(-0.309016994374938,0.951056516295157,4.35148173242957E-17));
#114422=DIRECTION('center_axis',(-1.4081690688991E-16,0.,-1.));
#114423=DIRECTION('ref_axis',(-1.,0.,1.4081690688991E-16));
#114424=DIRECTION('center_axis',(-1.4081690688991E-16,0.,-1.));
#114425=DIRECTION('ref_axis',(-1.,0.,1.4081690688991E-16));
#114426=DIRECTION('center_axis',(-1.4081690688991E-16,0.,-1.));
#114427=DIRECTION('ref_axis',(-1.,0.,1.4081690688991E-16));
#114428=DIRECTION('',(0.406736643075792,-0.913545457642605,-5.72753959967185E-17));
#114429=DIRECTION('center_axis',(1.4081690688991E-16,0.,1.));
#114430=DIRECTION('ref_axis',(1.,0.,-1.4081690688991E-16));
#114431=DIRECTION('',(-0.154505557223403,0.475534671805168,0.866022406579782));
#114432=DIRECTION('center_axis',(1.4081690688991E-16,0.,1.));
#114433=DIRECTION('ref_axis',(-1.,0.,1.40816906889911E-16));
#114434=DIRECTION('',(0.203374797931583,-0.456775527877804,-0.866022406579785));
#114435=DIRECTION('center_axis',(-1.4081690688991E-16,0.,-1.));
#114436=DIRECTION('ref_axis',(-1.,0.,1.40816906889911E-16));
#114437=DIRECTION('center_axis',(-1.4081690688991E-16,0.,-1.));
#114438=DIRECTION('ref_axis',(-1.,0.,1.4081690688991E-16));
#114439=DIRECTION('',(-0.309016994374938,0.951056516295157,4.35148173242957E-17));
#114440=DIRECTION('center_axis',(1.4081690688991E-16,0.,1.));
#114441=DIRECTION('ref_axis',(-1.,3.5527136788005E-14,1.4081690688991E-16));
#114442=DIRECTION('',(0.406736643075792,-0.913545457642605,-5.72753959967185E-17));
#114443=DIRECTION('center_axis',(-1.4081690688991E-16,0.,-1.));
#114444=DIRECTION('ref_axis',(-1.,0.,1.4081690688991E-16));
#114445=DIRECTION('center_axis',(-1.4081690688991E-16,0.,-1.));
#114446=DIRECTION('ref_axis',(1.,-1.95399252334028E-14,-1.4081690688991E-16));
#114447=DIRECTION('',(-0.154514440939472,0.475531575574881,-0.866022521746654));
#114448=DIRECTION('center_axis',(-1.4081690688991E-16,0.,-1.));
#114449=DIRECTION('ref_axis',(-1.,0.,1.4081690688991E-16));
#114450=DIRECTION('center_axis',(-1.4081690688991E-16,0.,-1.));
#114451=DIRECTION('ref_axis',(-1.,0.,1.4081690688991E-16));
#114452=DIRECTION('center_axis',(-1.4081690688991E-16,0.,-1.));
#114453=DIRECTION('ref_axis',(-1.,0.,1.4081690688991E-16));
#114454=DIRECTION('',(0.2033661242615,-0.456779171296606,0.866022521746659));
#114455=DIRECTION('center_axis',(-1.4081690688991E-16,0.,-1.));
#114456=DIRECTION('ref_axis',(-1.,0.,1.40816906889911E-16));
#114457=DIRECTION('',(-0.309016994374938,0.951056516295157,4.35148173242957E-17));
#114458=DIRECTION('center_axis',(1.4081690688991E-16,0.,1.));
#114459=DIRECTION('ref_axis',(-1.,0.,1.4081690688991E-16));
#114460=DIRECTION('',(0.406736643075792,-0.913545457642605,-5.72753959967185E-17));
#114461=DIRECTION('center_axis',(-1.4081690688991E-16,0.,-1.));
#114462=DIRECTION('ref_axis',(-1.,0.,1.17174841180864E-16));
#114463=DIRECTION('center_axis',(0.950725244291326,0.310034691293324,7.86457201959739E-6));
#114464=DIRECTION('ref_axis',(7.02293523252021E-6,3.83083002565365E-6,-0.999999999968001));
#114465=DIRECTION('center_axis',(-0.91398024672327,-0.405758682640088,7.86457224839801E-6));
#114466=DIRECTION('ref_axis',(0.3440977415858,-0.775097908773512,-0.529924500330454));
#114467=DIRECTION('center_axis',(-1.4081690688991E-16,0.,-1.));
#114468=DIRECTION('ref_axis',(-1.,0.,1.13676889660403E-16));
#114469=DIRECTION('center_axis',(0.950739383326775,0.309991330356124,-9.77058418244769E-6));
#114470=DIRECTION('ref_axis',(0.271126846795278,-0.831557796518166,-0.484769908303621));
#114471=DIRECTION('center_axis',(-0.913961739929031,-0.4058003669915,-9.77051737432389E-6));
#114472=DIRECTION('ref_axis',(0.354937311790693,-0.799394020105817,-0.48475633602652));
#114473=DIRECTION('center_axis',(-1.4081690688991E-16,0.,-1.));
#114474=DIRECTION('ref_axis',(-1.,0.,1.15974593313694E-16));
#114475=DIRECTION('center_axis',(-0.95185622840661,-0.306544809307982,1.81624796416327E-5));
#114476=DIRECTION('ref_axis',(0.265244982895815,-0.823585901983176,0.501349539845363));
#114477=DIRECTION('center_axis',(0.912485552150587,0.409108930222359,1.81316451411862E-5));
#114478=DIRECTION('ref_axis',(0.354681619616753,-0.791111768370323,0.498340364261231));
#114479=DIRECTION('center_axis',(-1.4081690688991E-16,0.,-1.));
#114480=DIRECTION('ref_axis',(-1.,0.,1.16261524579732E-16));
#114481=DIRECTION('center_axis',(-0.951860370340397,-0.306531947818513,
1.84940485141779E-5));
#114482=DIRECTION('ref_axis',(0.265748920300392,-0.825248669209763,-0.498339387693458));
#114483=DIRECTION('center_axis',(0.91248002438436,0.409121259232902,1.85257051375691E-5));
#114484=DIRECTION('ref_axis',(0.353998779725107,-0.789515382130535,-0.501348506861654));
#114485=DIRECTION('center_axis',(-1.4081690688991E-16,0.,-1.));
#114486=DIRECTION('ref_axis',(-1.,0.,1.40816906889911E-16));
#114487=DIRECTION('center_axis',(-1.4081690688991E-16,0.,-1.));
#114488=DIRECTION('ref_axis',(-1.,0.,1.4081690688991E-16));
#114489=DIRECTION('',(-0.406736643075792,0.913545457642605,5.72753959967185E-17));
#114490=DIRECTION('center_axis',(-1.4081690688991E-16,0.,-1.));
#114491=DIRECTION('ref_axis',(-1.,0.,1.4081690688991E-16));
#114492=DIRECTION('center_axis',(-1.4081690688991E-16,0.,-1.));
#114493=DIRECTION('ref_axis',(-1.,0.,1.4081690688991E-16));
#114494=DIRECTION('center_axis',(-1.4081690688991E-16,0.,-1.));
#114495=DIRECTION('ref_axis',(-1.,0.,1.4081690688991E-16));
#114496=DIRECTION('',(0.499999999999992,-0.866025403784443,-7.04084534449541E-17));
#114497=DIRECTION('center_axis',(1.4081690688991E-16,0.,1.));
#114498=DIRECTION('ref_axis',(1.,0.,-1.4081690688991E-16));
#114499=DIRECTION('',(-0.203366068089009,0.456779414654112,0.866022406579797));
#114500=DIRECTION('center_axis',(1.4081690688991E-16,0.,1.));
#114501=DIRECTION('ref_axis',(-1.,0.,1.40816906889911E-16));
#114502=DIRECTION('',(0.250006733496392,-0.433014808647731,-0.866022406579779));
#114503=DIRECTION('center_axis',(-1.4081690688991E-16,0.,-1.));
#114504=DIRECTION('ref_axis',(-1.,0.,1.40816906889911E-16));
#114505=DIRECTION('center_axis',(-1.4081690688991E-16,0.,-1.));
#114506=DIRECTION('ref_axis',(-1.,0.,1.4081690688991E-16));
#114507=DIRECTION('',(-0.406736643075792,0.913545457642605,5.72753959967185E-17));
#114508=DIRECTION('center_axis',(1.4081690688991E-16,0.,1.));
#114509=DIRECTION('ref_axis',(-1.,-1.15463194561016E-14,1.4081690688991E-16));
#114510=DIRECTION('',(0.499999999999992,-0.866025403784443,-7.04084534449541E-17));
#114511=DIRECTION('center_axis',(-1.4081690688991E-16,0.,-1.));
#114512=DIRECTION('ref_axis',(-1.,0.,1.4081690688991E-16));
#114513=DIRECTION('center_axis',(-1.4081690688991E-16,0.,-1.));
#114514=DIRECTION('ref_axis',(1.,1.06581410364015E-14,-1.4081690688991E-16));
#114515=DIRECTION('',(-0.203374579494982,0.456775406784115,-0.866022521746661));
#114516=DIRECTION('center_axis',(-1.4081690688991E-16,0.,-1.));
#114517=DIRECTION('ref_axis',(-1.,0.,1.4081690688991E-16));
#114518=DIRECTION('center_axis',(-1.4081690688991E-16,0.,-1.));
#114519=DIRECTION('ref_axis',(-1.,0.,1.4081690688991E-16));
#114520=DIRECTION('center_axis',(-1.4081690688991E-16,0.,-1.));
#114521=DIRECTION('ref_axis',(-1.,0.,1.4081690688991E-16));
#114522=DIRECTION('',(0.249998488182543,-0.433019338752907,0.866022521746657));
#114523=DIRECTION('center_axis',(-1.4081690688991E-16,0.,-1.));
#114524=DIRECTION('ref_axis',(-1.,0.,1.40816906889911E-16));
#114525=DIRECTION('',(-0.406736643075792,0.913545457642605,5.72753959967185E-17));
#114526=DIRECTION('center_axis',(1.4081690688991E-16,0.,1.));
#114527=DIRECTION('ref_axis',(-1.,0.,1.4081690688991E-16));
#114528=DIRECTION('',(0.499999999999992,-0.866025403784443,-7.04084534449541E-17));
#114529=DIRECTION('center_axis',(-1.4081690688991E-16,0.,-1.));
#114530=DIRECTION('ref_axis',(-1.,0.,1.17174841180864E-16));
#114531=DIRECTION('center_axis',(0.913109622086558,0.407714137590409,7.86457186754196E-6));
#114532=DIRECTION('ref_axis',(6.58403193953515E-6,4.54394091320277E-6,-0.999999999968002));
#114533=DIRECTION('center_axis',(-0.866560035746524,-0.499072844768309,
7.86457228533342E-6));
#114534=DIRECTION('ref_axis',(0.423232531439884,-0.734883833187603,-0.529924500330456));
#114535=DIRECTION('center_axis',(-1.4081690688991E-16,0.,-1.));
#114536=DIRECTION('ref_axis',(-1.,0.,1.13676889660403E-16));
#114537=DIRECTION('center_axis',(0.913128216116848,0.40767249212548,-9.77059363821822E-6));
#114538=DIRECTION('ref_axis',(0.356563044148667,-0.79866196325611,-0.484769908302208));
#114539=DIRECTION('center_axis',(-0.866537273133093,-0.499112366281983,
-9.77051681670262E-6));
#114540=DIRECTION('ref_axis',(0.436552356525271,-0.75791380426263,-0.484756336029123));
#114541=DIRECTION('center_axis',(-1.4081690688991E-16,0.,-1.));
#114542=DIRECTION('ref_axis',(-1.,0.,1.15974593313694E-16));
#114543=DIRECTION('center_axis',(-0.914599202553385,-0.404361593575401,
1.81624795807573E-5));
#114544=DIRECTION('ref_axis',(0.349880111829649,-0.791348561787279,0.501349539845484));
#114545=DIRECTION('center_axis',(0.86472333303575,0.502248501217064,1.81316452677056E-5));
#114546=DIRECTION('ref_axis',(0.43543233401603,-0.749703650683173,0.49834036425487));
#114547=DIRECTION('center_axis',(-1.4081690688991E-16,0.,-1.));
#114548=DIRECTION('ref_axis',(-1.,0.,1.16261524579732E-16));
#114549=DIRECTION('center_axis',(-0.914604666187431,-0.404349235495936,
1.84940550607155E-5));
#114550=DIRECTION('ref_axis',(0.35055509511501,-0.792949544397653,-0.498339387695234));
#114551=DIRECTION('center_axis',(0.864716546818594,0.502260184879236,1.85257048927828E-5));
#114552=DIRECTION('ref_axis',(0.434586366991679,-0.748187385817474,-0.501348506857843));
#114553=DIRECTION('center_axis',(-1.4081690688991E-16,0.,-1.));
#114554=DIRECTION('ref_axis',(-1.,0.,1.40816906889911E-16));
#114555=DIRECTION('center_axis',(-1.4081690688991E-16,0.,-1.));
#114556=DIRECTION('ref_axis',(-1.,0.,1.4081690688991E-16));
#114557=DIRECTION('',(-0.499999999999992,0.866025403784443,7.04084534449541E-17));
#114558=DIRECTION('center_axis',(-1.4081690688991E-16,0.,-1.));
#114559=DIRECTION('ref_axis',(-1.,0.,1.4081690688991E-16));
#114560=DIRECTION('center_axis',(-1.4081690688991E-16,0.,-1.));
#114561=DIRECTION('ref_axis',(-1.,0.,1.4081690688991E-16));
#114562=DIRECTION('center_axis',(-1.4081690688991E-16,0.,-1.));
#114563=DIRECTION('ref_axis',(-1.,0.,1.4081690688991E-16));
#114564=DIRECTION('',(0.587785252292466,-0.809016994374953,-8.27701011433307E-17));
#114565=DIRECTION('center_axis',(1.4081690688991E-16,0.,1.));
#114566=DIRECTION('ref_axis',(1.,0.,-1.4081690688991E-16));
#114567=DIRECTION('',(-0.249998457755585,0.433019586648859,0.866022406579807));
#114568=DIRECTION('center_axis',(1.4081690688991E-16,0.,1.));
#114569=DIRECTION('ref_axis',(-1.,-1.24344978758018E-14,1.40816906889911E-16));
#114570=DIRECTION('',(0.29389954297172,-0.404509888559932,-0.866022406579787));
#114571=DIRECTION('center_axis',(-1.4081690688991E-16,0.,-1.));
#114572=DIRECTION('ref_axis',(-1.,0.,1.40816906889911E-16));
#114573=DIRECTION('center_axis',(-1.4081690688991E-16,0.,-1.));
#114574=DIRECTION('ref_axis',(-1.,0.,1.4081690688991E-16));
#114575=DIRECTION('',(-0.499999999999992,0.866025403784443,7.04084534449541E-17));
#114576=DIRECTION('center_axis',(1.4081690688991E-16,0.,1.));
#114577=DIRECTION('ref_axis',(-1.,3.01980662698043E-14,1.4081690688991E-16));
#114578=DIRECTION('',(0.587785252292466,-0.809016994374953,-8.27701011433307E-17));
#114579=DIRECTION('center_axis',(-1.4081690688991E-16,0.,-1.));
#114580=DIRECTION('ref_axis',(-1.,0.,1.4081690688991E-16));
#114581=DIRECTION('center_axis',(-1.4081690688991E-16,0.,-1.));
#114582=DIRECTION('ref_axis',(1.,1.95399252334028E-14,-1.4081690688991E-16));
#114583=DIRECTION('',(-0.25000650359866,0.433014711050234,-0.866022521746667));
#114584=DIRECTION('center_axis',(-1.4081690688991E-16,0.,-1.));
#114585=DIRECTION('ref_axis',(-1.,0.,1.4081690688991E-16));
#114586=DIRECTION('center_axis',(-1.4081690688991E-16,0.,-1.));
#114587=DIRECTION('ref_axis',(-1.,0.,1.4081690688991E-16));
#114588=DIRECTION('center_axis',(-1.4081690688991E-16,0.,-1.));
#114589=DIRECTION('ref_axis',(-1.,0.,1.4081690688991E-16));
#114590=DIRECTION('',(0.293891816351498,-0.404515255718706,0.866022521746661));
#114591=DIRECTION('center_axis',(-1.4081690688991E-16,0.,-1.));
#114592=DIRECTION('ref_axis',(-1.,0.,1.40816906889911E-16));
#114593=DIRECTION('',(-0.499999999999992,0.866025403784443,7.04084534449541E-17));
#114594=DIRECTION('center_axis',(1.4081690688991E-16,0.,1.));
#114595=DIRECTION('ref_axis',(-1.,-6.21724893790088E-15,1.4081690688991E-16));
#114596=DIRECTION('',(0.587785252292466,-0.809016994374953,-8.27701011433307E-17));
#114597=DIRECTION('center_axis',(-1.4081690688991E-16,0.,-1.));
#114598=DIRECTION('ref_axis',(-1.,0.,1.17174841180864E-16));
#114599=DIRECTION('center_axis',(0.865489779781645,0.500926582476583,7.86457206261499E-6));
#114600=DIRECTION('ref_axis',(6.07299293807602E-6,5.20726754909509E-6,-0.999999999968002));
#114601=DIRECTION('center_axis',(-0.809645611678775,-0.586919060371574,
7.86457229727665E-6));
#114602=DIRECTION('ref_axis',(0.497730297112456,-0.686618216540951,-0.529924500330443));
#114603=DIRECTION('center_axis',(-1.4081690688991E-16,0.,-1.));
#114604=DIRECTION('ref_axis',(-1.,0.,1.13676889660403E-16));
#114605=DIRECTION('center_axis',(0.865512625088529,0.500887108754956,-9.7705931674539E-6));
#114606=DIRECTION('ref_axis',(0.438092662174321,-0.757015822392775,-0.484769908302905));
#114607=DIRECTION('center_axis',(-0.809618842639843,-0.586955986039037,
-9.77052175743205E-6));
#114608=DIRECTION('ref_axis',(0.513384442289742,-0.7081297261801,-0.484756336023519));
#114609=DIRECTION('center_axis',(-1.4081690688991E-16,0.,-1.));
#114610=DIRECTION('ref_axis',(-1.,0.,1.15974593313694E-16));
#114611=DIRECTION('center_axis',(-0.86732163644481,-0.497748107605465,1.81624796484551E-5));
#114612=DIRECTION('ref_axis',(0.430681881041749,-0.750441041149111,0.50134953984359));
#114613=DIRECTION('center_axis',(0.807487024129162,0.589885332530207,1.81316450787733E-5));
#114614=DIRECTION('ref_axis',(0.511412360643632,-0.700081622911792,0.49834036425128));
#114615=DIRECTION('center_axis',(-1.4081690688991E-16,0.,-1.));
#114616=DIRECTION('ref_axis',(-1.,0.,1.16261524579732E-16));
#114617=DIRECTION('center_axis',(-0.867328361918051,-0.49773638833274,1.84940603276878E-5));
#114618=DIRECTION('ref_axis',(0.431520514948258,-0.751962698440682,-0.498339387699386));
#114619=DIRECTION('center_axis',(0.807479053809579,0.589896242839014,1.85256966566585E-5));
#114620=DIRECTION('ref_axis',(0.510412535074995,-0.698662091931687,-0.501348506865191));
#114621=DIRECTION('center_axis',(-1.4081690688991E-16,0.,-1.));
#114622=DIRECTION('ref_axis',(-1.,0.,1.40816906889911E-16));
#114623=DIRECTION('center_axis',(-1.4081690688991E-16,0.,-1.));
#114624=DIRECTION('ref_axis',(-1.,0.,1.4081690688991E-16));
#114625=DIRECTION('',(-0.587785252292466,0.809016994374953,8.27701011433307E-17));
#114626=DIRECTION('center_axis',(-1.4081690688991E-16,0.,-1.));
#114627=DIRECTION('ref_axis',(-1.,0.,1.4081690688991E-16));
#114628=DIRECTION('center_axis',(-1.4081690688991E-16,0.,-1.));
#114629=DIRECTION('ref_axis',(-1.,0.,1.4081690688991E-16));
#114630=DIRECTION('center_axis',(-1.4081690688991E-16,0.,-1.));
#114631=DIRECTION('ref_axis',(-1.,0.,1.4081690688991E-16));
#114632=DIRECTION('',(0.669130606358852,-0.7431448254774,-9.42249022928238E-17));
#114633=DIRECTION('center_axis',(1.4081690688991E-16,0.,1.));
#114634=DIRECTION('ref_axis',(1.,0.,-1.4081690688991E-16));
#114635=DIRECTION('',(-0.293891812003425,0.404515505437168,0.866022406579793));
#114636=DIRECTION('center_axis',(1.4081690688991E-16,0.,1.));
#114637=DIRECTION('ref_axis',(-1.,1.86517468137026E-14,1.40816906889911E-16));
#114638=DIRECTION('',(0.334572327551833,-0.371573073483921,-0.866022406579796));
#114639=DIRECTION('center_axis',(-1.4081690688991E-16,0.,-1.));
#114640=DIRECTION('ref_axis',(-1.,0.,1.40816906889911E-16));
#114641=DIRECTION('center_axis',(-1.4081690688991E-16,0.,-1.));
#114642=DIRECTION('ref_axis',(-1.,0.,1.4081690688991E-16));
#114643=DIRECTION('',(-0.587785252292466,0.809016994374953,8.27701011433307E-17));
#114644=DIRECTION('center_axis',(1.4081690688991E-16,0.,1.));
#114645=DIRECTION('ref_axis',(-1.,2.48689957516035E-14,1.4081690688991E-16));
#114646=DIRECTION('',(0.669130606358852,-0.7431448254774,-9.42249022928238E-17));
#114647=DIRECTION('center_axis',(-1.4081690688991E-16,0.,-1.));
#114648=DIRECTION('ref_axis',(-1.,0.,1.4081690688991E-16));
#114649=DIRECTION('center_axis',(-1.4081690688991E-16,0.,-1.));
#114650=DIRECTION('ref_axis',(1.,0.,-1.4081690688991E-16));
#114651=DIRECTION('',(-0.293899304131723,0.404509815527924,-0.866022521746666));
#114652=DIRECTION('center_axis',(-1.4081690688991E-16,0.,-1.));
#114653=DIRECTION('ref_axis',(-1.,0.,1.4081690688991E-16));
#114654=DIRECTION('center_axis',(-1.4081690688991E-16,0.,-1.));
#114655=DIRECTION('ref_axis',(-1.,0.,1.4081690688991E-16));
#114656=DIRECTION('center_axis',(-1.4081690688991E-16,0.,-1.));
#114657=DIRECTION('ref_axis',(-1.,0.,1.4081690688991E-16));
#114658=DIRECTION('',(0.334565204279774,-0.371579218892547,0.866022521746656));
#114659=DIRECTION('center_axis',(-1.4081690688991E-16,0.,-1.));
#114660=DIRECTION('ref_axis',(-1.,0.,1.40816906889911E-16));
#114661=DIRECTION('',(-0.587785252292466,0.809016994374953,8.27701011433307E-17));
#114662=DIRECTION('center_axis',(1.4081690688991E-16,0.,1.));
#114663=DIRECTION('ref_axis',(-1.,2.48689957516035E-14,1.4081690688991E-16));
#114664=DIRECTION('',(0.669130606358852,-0.7431448254774,-9.42249022928238E-17));
#114665=DIRECTION('center_axis',(-1.4081690688991E-16,0.,-1.));
#114666=DIRECTION('ref_axis',(-1.,0.,1.17174841180864E-16));
#114667=DIRECTION('center_axis',(0.808387450334136,0.588650770899371,7.86457201793794E-6));
#114668=DIRECTION('ref_axis',(5.49541672851605E-6,5.81354221112889E-6,-0.999999999968002));
#114669=DIRECTION('center_axis',(-0.743860540860193,-0.668334867928743,
7.86457217253649E-6));
#114670=DIRECTION('ref_axis',(0.566774825493203,-0.630829867029694,-0.529924500330422));
#114671=DIRECTION('center_axis',(-1.4081690688991E-16,0.,-1.));
#114672=DIRECTION('ref_axis',(-1.,0.,1.13676889660403E-16));
#114673=DIRECTION('center_axis',(0.808414296622801,0.588613901399208,-9.7705831004133E-6));
#114674=DIRECTION('ref_axis',(0.514822445316052,-0.707075657763321,-0.484769908304308));
#114675=DIRECTION('center_axis',(-0.7438300586801,-0.668368793188683,-9.77051765796924E-6));
#114676=DIRECTION('ref_axis',(0.584591780668461,-0.650587230627073,-0.4847563360286));
#114677=DIRECTION('center_axis',(-1.4081690688991E-16,0.,-1.));
#114678=DIRECTION('ref_axis',(-1.,0.,1.15974593313694E-16));
#114679=DIRECTION('center_axis',(-0.810541512988718,-0.585681189207989,
1.81624798788288E-5));
#114680=DIRECTION('ref_axis',(0.506765009439008,-0.701311531423695,0.501349539842647));
#114681=DIRECTION('center_axis',(0.74140371840874,0.671059256698644,1.81316453410639E-5));
#114682=DIRECTION('ref_axis',(0.581789246428454,-0.642789354378472,0.498340364247086));
#114683=DIRECTION('center_axis',(-1.4081690688991E-16,0.,-1.));
#114684=DIRECTION('ref_axis',(-1.,0.,1.16261524579732E-16));
#114685=DIRECTION('center_axis',(-0.810549426620236,-0.585670237133129,
1.84940495645244E-5));
#114686=DIRECTION('ref_axis',(0.507758105720992,-0.702737191805956,-0.498339387694078));
#114687=DIRECTION('center_axis',(0.74139465132122,0.671069274105948,1.85257164118208E-5));
#114688=DIRECTION('ref_axis',(0.58064651661672,-0.641482109967248,-0.50134850686208));
#114689=DIRECTION('center_axis',(-1.4081690688991E-16,0.,-1.));
#114690=DIRECTION('ref_axis',(-1.,0.,1.40816906889911E-16));
#114691=DIRECTION('center_axis',(-1.4081690688991E-16,0.,-1.));
#114692=DIRECTION('ref_axis',(-1.,0.,1.4081690688991E-16));
#114693=DIRECTION('',(-0.669130606358852,0.7431448254774,9.42249022928238E-17));
#114694=DIRECTION('center_axis',(-1.4081690688991E-16,0.,-1.));
#114695=DIRECTION('ref_axis',(-1.,0.,1.4081690688991E-16));
#114696=DIRECTION('center_axis',(-1.4081690688991E-16,0.,-1.));
#114697=DIRECTION('ref_axis',(-1.,0.,1.4081690688991E-16));
#114698=DIRECTION('center_axis',(-1.4081690688991E-16,0.,-1.));
#114699=DIRECTION('ref_axis',(-1.,0.,1.4081690688991E-16));
#114700=DIRECTION('',(0.743144825477389,-0.669130606358864,-1.04647355694968E-16));
#114701=DIRECTION('center_axis',(1.4081690688991E-16,0.,1.));
#114702=DIRECTION('ref_axis',(1.,0.,-1.4081690688991E-16));
#114703=DIRECTION('',(-0.334565226058171,0.371579467697561,0.866022406579785));
#114704=DIRECTION('center_axis',(1.4081690688991E-16,0.,1.));
#114705=DIRECTION('ref_axis',(-1.,7.105427357601E-15,1.40816906889911E-16));
#114706=DIRECTION('',(0.371579467697514,-0.334565226058178,-0.866022406579802));
#114707=DIRECTION('center_axis',(-1.4081690688991E-16,0.,-1.));
#114708=DIRECTION('ref_axis',(-1.,0.,1.40816906889911E-16));
#114709=DIRECTION('center_axis',(-1.4081690688991E-16,0.,-1.));
#114710=DIRECTION('ref_axis',(-1.,0.,1.4081690688991E-16));
#114711=DIRECTION('',(-0.669130606358852,0.7431448254774,9.42249022928238E-17));
#114712=DIRECTION('center_axis',(1.4081690688991E-16,0.,1.));
#114713=DIRECTION('ref_axis',(-1.,-3.90798504668055E-14,1.4081690688991E-16));
#114714=DIRECTION('',(0.743144825477389,-0.669130606358864,-1.04647355694968E-16));
#114715=DIRECTION('center_axis',(-1.4081690688991E-16,0.,-1.));
#114716=DIRECTION('ref_axis',(-1.,0.,1.4081690688991E-16));
#114717=DIRECTION('center_axis',(-1.4081690688991E-16,0.,-1.));
#114718=DIRECTION('ref_axis',(1.,0.,-1.4081690688991E-16));
#114719=DIRECTION('',(-0.3345720823863,0.371573025817577,-0.866022521746672));
#114720=DIRECTION('center_axis',(-1.4081690688991E-16,0.,-1.));
#114721=DIRECTION('ref_axis',(-1.,0.,1.4081690688991E-16));
#114722=DIRECTION('center_axis',(-1.4081690688991E-16,0.,-1.));
#114723=DIRECTION('ref_axis',(-1.,0.,1.4081690688991E-16));
#114724=DIRECTION('center_axis',(-1.4081690688991E-16,0.,-1.));
#114725=DIRECTION('ref_axis',(-1.,0.,1.4081690688991E-16));
#114726=DIRECTION('',(0.371573025817621,-0.334572082386318,0.866022521746647));
#114727=DIRECTION('center_axis',(-1.4081690688991E-16,0.,-1.));
#114728=DIRECTION('ref_axis',(-1.,0.,1.40816906889911E-16));
#114729=DIRECTION('',(-0.669130606358852,0.7431448254774,9.42249022928238E-17));
#114730=DIRECTION('center_axis',(1.4081690688991E-16,0.,1.));
#114731=DIRECTION('ref_axis',(-1.,-3.19744231092045E-14,1.4081690688991E-16));
#114732=DIRECTION('',(0.743144825477389,-0.669130606358864,-1.04647355694968E-16));
#114733=DIRECTION('center_axis',(-1.4081690688991E-16,0.,-1.));
#114734=DIRECTION('ref_axis',(-1.,0.,1.17174841180864E-16));
#114735=DIRECTION('center_axis',(0.742428258814843,0.669925578293073,7.86457196552063E-6));
#114736=DIRECTION('ref_axis',(4.85763160251991E-6,6.35612243375601E-6,-0.999999999968002));
#114737=DIRECTION('center_axis',(-0.669925578293223,-0.742428258814708,
7.86457226896801E-6));
#114738=DIRECTION('ref_axis',(0.62960965028037,-0.568130013485746,-0.529924500330487));
#114739=DIRECTION('center_axis',(-1.4081690688991E-16,0.,-1.));
#114740=DIRECTION('ref_axis',(-1.,0.,1.13676889660403E-16));
#114741=DIRECTION('center_axis',(0.742458811945264,0.669891716973245,-9.77059280552686E-6));
#114742=DIRECTION('ref_axis',(0.585911726013662,-0.649388624262771,-0.484769908304752));
#114743=DIRECTION('center_axis',(-0.66989171694181,-0.742458811973628,-9.77051631735247E-6));
#114744=DIRECTION('ref_axis',(0.649394209166982,-0.585916765234243,-0.484756336026494));
#114745=DIRECTION('center_axis',(-1.4081690688991E-16,0.,-1.));
#114746=DIRECTION('ref_axis',(-1.,0.,1.15974593313694E-16));
#114747=DIRECTION('center_axis',(-0.744880927099423,-0.667197425140137,
1.81624796016105E-5));
#114748=DIRECTION('ref_axis',(0.577295914344574,-0.644498305799945,0.501349539844272));
#114749=DIRECTION('center_axis',(0.667197438400719,0.744880915222536,1.81316452123543E-5));
#114750=DIRECTION('ref_axis',(0.645791927479624,-0.578454551163014,0.498340364250127));
#114751=DIRECTION('center_axis',(-1.4081690688991E-16,0.,-1.));
#114752=DIRECTION('ref_axis',(-1.,0.,1.16261524579732E-16));
#114753=DIRECTION('center_axis',(-0.744889942181918,-0.667187360262609,
1.84940520599162E-5));
#114754=DIRECTION('ref_axis',(0.578432592428309,-0.645812349435162,-0.498339387700493));
#114755=DIRECTION('center_axis',(0.667187373880019,0.74488992998421,1.85257177449103E-5));
#114756=DIRECTION('ref_axis',(0.644518813413743,-0.577273915766274,-0.50134850686086));
#114757=DIRECTION('center_axis',(-1.4081690688991E-16,0.,-1.));
#114758=DIRECTION('ref_axis',(-1.,0.,1.40816906889911E-16));
#114759=DIRECTION('center_axis',(-1.4081690688991E-16,0.,-1.));
#114760=DIRECTION('ref_axis',(-1.,0.,1.4081690688991E-16));
#114761=DIRECTION('',(-0.743144825477389,0.669130606358864,1.04647355694968E-16));
#114762=DIRECTION('center_axis',(-1.4081690688991E-16,0.,-1.));
#114763=DIRECTION('ref_axis',(-1.,0.,1.4081690688991E-16));
#114764=DIRECTION('center_axis',(-1.4081690688991E-16,0.,-1.));
#114765=DIRECTION('ref_axis',(-1.,0.,1.4081690688991E-16));
#114766=DIRECTION('center_axis',(-1.4081690688991E-16,0.,-1.));
#114767=DIRECTION('ref_axis',(-1.,0.,1.4081690688991E-16));
#114768=DIRECTION('',(0.809016994374943,-0.58778525229248,-1.13923270769252E-16));
#114769=DIRECTION('center_axis',(1.4081690688991E-16,0.,1.));
#114770=DIRECTION('ref_axis',(1.,0.,-1.4081690688991E-16));
#114771=DIRECTION('',(-0.371573073483894,0.334572327551861,0.866022406579797));
#114772=DIRECTION('center_axis',(1.4081690688991E-16,0.,1.));
#114773=DIRECTION('ref_axis',(-1.,2.66453525910038E-14,1.40816906889911E-16));
#114774=DIRECTION('',(0.404515505437159,-0.293891812003487,-0.866022406579776));
#114775=DIRECTION('center_axis',(-1.4081690688991E-16,0.,-1.));
#114776=DIRECTION('ref_axis',(-1.,0.,1.40816906889911E-16));
#114777=DIRECTION('center_axis',(-1.4081690688991E-16,0.,-1.));
#114778=DIRECTION('ref_axis',(-1.,0.,1.4081690688991E-16));
#114779=DIRECTION('',(-0.743144825477389,0.669130606358864,1.04647355694968E-16));
#114780=DIRECTION('center_axis',(1.4081690688991E-16,0.,1.));
#114781=DIRECTION('ref_axis',(-1.,1.33226762955019E-14,1.4081690688991E-16));
#114782=DIRECTION('',(0.809016994374943,-0.58778525229248,-1.13923270769252E-16));
#114783=DIRECTION('center_axis',(-1.4081690688991E-16,0.,-1.));
#114784=DIRECTION('ref_axis',(-1.,0.,1.4081690688991E-16));
#114785=DIRECTION('center_axis',(-1.4081690688991E-16,0.,-1.));
#114786=DIRECTION('ref_axis',(1.,0.,-1.4081690688991E-16));
#114787=DIRECTION('',(-0.371579218892551,0.33456520427975,-0.866022521746664));
#114788=DIRECTION('center_axis',(-1.4081690688991E-16,0.,-1.));
#114789=DIRECTION('ref_axis',(-1.,0.,1.4081690688991E-16));
#114790=DIRECTION('center_axis',(-1.4081690688991E-16,0.,-1.));
#114791=DIRECTION('ref_axis',(-1.,0.,1.4081690688991E-16));
#114792=DIRECTION('center_axis',(-1.4081690688991E-16,0.,-1.));
#114793=DIRECTION('ref_axis',(-1.,0.,1.4081690688991E-16));
#114794=DIRECTION('',(0.404509815527948,-0.293899304131707,0.86602252174666));
#114795=DIRECTION('center_axis',(-1.4081690688991E-16,0.,-1.));
#114796=DIRECTION('ref_axis',(-1.,0.,1.40816906889911E-16));
#114797=DIRECTION('',(-0.743144825477389,0.669130606358864,1.04647355694968E-16));
#114798=DIRECTION('center_axis',(1.4081690688991E-16,0.,1.));
#114799=DIRECTION('ref_axis',(-1.,2.57571741713036E-14,1.4081690688991E-16));
#114800=DIRECTION('',(0.809016994374943,-0.58778525229248,-1.13923270769252E-16));
#114801=DIRECTION('center_axis',(-1.4081690688991E-16,0.,-1.));
#114802=DIRECTION('ref_axis',(-1.,0.,1.17174841180864E-16));
#114803=DIRECTION('center_axis',(0.668334867928844,0.743860540860102,7.86457191841109E-6));
#114804=DIRECTION('ref_axis',(4.16662522946725E-6,6.8290636700625E-6,-0.999999999968001));
#114805=DIRECTION('center_axis',(-0.588650770899511,-0.808387450334034,
7.86457230678758E-6));
#114806=DIRECTION('ref_axis',(0.685546339984867,-0.499205608625207,-0.529924500330462));
#114807=DIRECTION('center_axis',(-1.4081690688991E-16,0.,-1.));
#114808=DIRECTION('ref_axis',(-1.,0.,1.13676889660403E-16));
#114809=DIRECTION('center_axis',(0.668368793161135,0.743830058704852,-9.77058447225306E-6));
#114810=DIRECTION('ref_axis',(0.650581635232363,-0.584586753102607,-0.484769908302213));
#114811=DIRECTION('center_axis',(-0.588613901370769,-0.808414296643509,
-9.77051950914831E-6));
#114812=DIRECTION('ref_axis',(0.707081738814109,-0.514826873149292,-0.484756336027636));
#114813=DIRECTION('center_axis',(-1.4081690688991E-16,0.,-1.));
#114814=DIRECTION('ref_axis',(-1.,0.,1.15974593313694E-16));
#114815=DIRECTION('center_axis',(-0.671059269896554,-0.741403706462295,
1.8162479710228E-5));
#114816=DIRECTION('ref_axis',(0.641501844406933,-0.580623821869249,0.501349539842663));
#114817=DIRECTION('center_axis',(0.585681203637554,0.810541502562891,1.81316450912546E-5));
#114818=DIRECTION('ref_axis',(0.702719177034773,-0.5077820788376,0.498340364248107));
#114819=DIRECTION('center_axis',(-1.4081690688991E-16,0.,-1.));
#114820=DIRECTION('ref_axis',(-1.,0.,1.16261524579732E-16));
#114821=DIRECTION('center_axis',(-0.671069287650237,-0.741394639062472,
1.84940740096905E-5));
#114822=DIRECTION('ref_axis',(0.642769650611826,-0.581811851823278,-0.498339387697099));
#114823=DIRECTION('center_axis',(0.585670251949479,0.810549415913818,1.8525712039311E-5));
#114824=DIRECTION('ref_axis',(0.701329627217096,-0.506740987741917,-0.501348506859126));
#114825=DIRECTION('center_axis',(-1.4081690688991E-16,0.,-1.));
#114826=DIRECTION('ref_axis',(-1.,0.,1.40816906889911E-16));
#114827=DIRECTION('center_axis',(-1.4081690688991E-16,0.,-1.));
#114828=DIRECTION('ref_axis',(-1.,0.,1.4081690688991E-16));
#114829=DIRECTION('',(-0.809016994374943,0.58778525229248,1.13923270769252E-16));
#114830=DIRECTION('center_axis',(-1.4081690688991E-16,0.,-1.));
#114831=DIRECTION('ref_axis',(-1.,0.,1.4081690688991E-16));
#114832=DIRECTION('center_axis',(-1.4081690688991E-16,0.,-1.));
#114833=DIRECTION('ref_axis',(-1.,0.,1.4081690688991E-16));
#114834=DIRECTION('center_axis',(-1.4081690688991E-16,0.,-1.));
#114835=DIRECTION('ref_axis',(-1.,0.,1.4081690688991E-16));
#114836=DIRECTION('',(0.866025403784435,-0.500000000000007,-1.2195101864901E-16));
#114837=DIRECTION('center_axis',(1.4081690688991E-16,0.,1.));
#114838=DIRECTION('ref_axis',(1.,0.,-1.4081690688991E-16));
#114839=DIRECTION('',(-0.404509888559932,0.29389954297172,0.866022406579787));
#114840=DIRECTION('center_axis',(1.4081690688991E-16,0.,1.));
#114841=DIRECTION('ref_axis',(-1.,7.105427357601E-15,1.40816906889911E-16));
#114842=DIRECTION('',(0.433019586648901,-0.249998457755605,-0.86602240657978));
#114843=DIRECTION('center_axis',(-1.4081690688991E-16,0.,-1.));
#114844=DIRECTION('ref_axis',(-1.,0.,1.40816906889911E-16));
#114845=DIRECTION('center_axis',(-1.4081690688991E-16,0.,-1.));
#114846=DIRECTION('ref_axis',(-1.,0.,1.4081690688991E-16));
#114847=DIRECTION('',(-0.809016994374943,0.58778525229248,1.13923270769252E-16));
#114848=DIRECTION('center_axis',(1.4081690688991E-16,0.,1.));
#114849=DIRECTION('ref_axis',(-1.,-3.99680288865056E-14,1.4081690688991E-16));
#114850=DIRECTION('',(0.866025403784435,-0.500000000000007,-1.2195101864901E-16));
#114851=DIRECTION('center_axis',(-1.4081690688991E-16,0.,-1.));
#114852=DIRECTION('ref_axis',(-1.,0.,1.4081690688991E-16));
#114853=DIRECTION('center_axis',(-1.4081690688991E-16,0.,-1.));
#114854=DIRECTION('ref_axis',(1.,0.,-1.4081690688991E-16));
#114855=DIRECTION('',(-0.404515255718706,0.293891816351498,-0.866022521746661));
#114856=DIRECTION('center_axis',(-1.4081690688991E-16,0.,-1.));
#114857=DIRECTION('ref_axis',(-1.,0.,1.4081690688991E-16));
#114858=DIRECTION('center_axis',(-1.4081690688991E-16,0.,-1.));
#114859=DIRECTION('ref_axis',(-1.,0.,1.4081690688991E-16));
#114860=DIRECTION('center_axis',(-1.4081690688991E-16,0.,-1.));
#114861=DIRECTION('ref_axis',(-1.,0.,1.4081690688991E-16));
#114862=DIRECTION('',(0.433014711050233,-0.250006503598672,0.866022521746663));
#114863=DIRECTION('center_axis',(-1.4081690688991E-16,0.,-1.));
#114864=DIRECTION('ref_axis',(-1.,0.,1.40816906889911E-16));
#114865=DIRECTION('',(-0.809016994374943,0.58778525229248,1.13923270769252E-16));
#114866=DIRECTION('center_axis',(1.4081690688991E-16,0.,1.));
#114867=DIRECTION('ref_axis',(-1.,-2.66453525910038E-14,1.4081690688991E-16));
#114868=DIRECTION('',(0.866025403784435,-0.500000000000007,-1.2195101864901E-16));
#114869=DIRECTION('center_axis',(-1.4081690688991E-16,0.,-1.));
#114870=DIRECTION('ref_axis',(-1.,0.,1.17174841180864E-16));
#114871=DIRECTION('center_axis',(0.586919060371726,0.809645611678665,7.86457193544097E-6));
#114872=DIRECTION('ref_axis',(3.42996849075291E-6,7.2271843029038E-6,-0.999999999968002));
#114873=DIRECTION('center_axis',(-0.50092658247667,-0.865489779781594,7.86457223048433E-6));
#114874=DIRECTION('ref_axis',(0.733972040528744,-0.424811802650955,-0.529924500330489));
#114875=DIRECTION('center_axis',(-1.4081690688991E-16,0.,-1.));
#114876=DIRECTION('ref_axis',(-1.,0.,1.13676889660403E-16));
#114877=DIRECTION('center_axis',(0.586955986005752,0.809618842663973,-9.77059599688668E-6));
#114878=DIRECTION('ref_axis',(0.708123635911378,-0.513380027141705,-0.484769908302518));
#114879=DIRECTION('center_axis',(-0.500887108715761,-0.865512625111213,
-9.77051146875296E-6));
#114880=DIRECTION('ref_axis',(0.757022332964799,-0.438096430108037,-0.484756336027831));
#114881=DIRECTION('center_axis',(-1.4081690688991E-16,0.,-1.));
#114882=DIRECTION('ref_axis',(-1.,0.,1.15974593313694E-16));
#114883=DIRECTION('center_axis',(-0.589885346904536,-0.807487013627736,
1.81624796204011E-5));
#114884=DIRECTION('ref_axis',(0.69867934601963,-0.510387901843116,0.501349539839984));
#114885=DIRECTION('center_axis',(0.497748123045631,0.867321627584482,1.8131645060743E-5));
#114886=DIRECTION('ref_axis',(0.751947288228587,-0.43154623979347,0.498340364254986));
#114887=DIRECTION('center_axis',(-1.4081690688991E-16,0.,-1.));
#114888=DIRECTION('ref_axis',(-1.,0.,1.16261524579732E-16));
#114889=DIRECTION('center_axis',(-0.589896257585103,-0.807479043037687,
1.8494065967643E-5));
#114890=DIRECTION('ref_axis',(0.700064389990716,-0.511436901807441,-0.498339387703332));
#114891=DIRECTION('center_axis',(0.497736404185315,0.86732835282001,1.85257193500676E-5));
#114892=DIRECTION('ref_axis',(0.750456526859374,-0.430656099411711,-0.501348506862897));
#114893=DIRECTION('center_axis',(-1.4081690688991E-16,0.,-1.));
#114894=DIRECTION('ref_axis',(-1.,0.,1.40816906889911E-16));
#114895=DIRECTION('center_axis',(-1.4081690688991E-16,0.,-1.));
#114896=DIRECTION('ref_axis',(-1.,0.,1.4081690688991E-16));
#114897=DIRECTION('',(-0.866025403784435,0.500000000000007,1.2195101864901E-16));
#114898=DIRECTION('center_axis',(-1.4081690688991E-16,0.,-1.));
#114899=DIRECTION('ref_axis',(-1.,0.,1.4081690688991E-16));
#114900=DIRECTION('center_axis',(-1.4081690688991E-16,0.,-1.));
#114901=DIRECTION('ref_axis',(-1.,0.,1.4081690688991E-16));
#114902=DIRECTION('center_axis',(-1.4081690688991E-16,0.,-1.));
#114903=DIRECTION('ref_axis',(-1.,0.,1.4081690688991E-16));
#114904=DIRECTION('',(0.913545457642598,-0.406736643075807,-1.28642645648558E-16));
#114905=DIRECTION('center_axis',(1.4081690688991E-16,0.,1.));
#114906=DIRECTION('ref_axis',(1.,0.,-1.4081690688991E-16));
#114907=DIRECTION('',(-0.433014808647733,0.250006733496379,0.866022406579782));
#114908=DIRECTION('center_axis',(1.4081690688991E-16,0.,1.));
#114909=DIRECTION('ref_axis',(-1.,-7.105427357601E-15,1.40816906889911E-16));
#114910=DIRECTION('',(0.456779414654109,-0.203366068089036,-0.866022406579792));
#114911=DIRECTION('center_axis',(-1.4081690688991E-16,0.,-1.));
#114912=DIRECTION('ref_axis',(-1.,0.,1.40816906889911E-16));
#114913=DIRECTION('center_axis',(-1.4081690688991E-16,0.,-1.));
#114914=DIRECTION('ref_axis',(-1.,0.,1.4081690688991E-16));
#114915=DIRECTION('',(-0.866025403784435,0.500000000000007,1.2195101864901E-16));
#114916=DIRECTION('center_axis',(1.4081690688991E-16,0.,1.));
#114917=DIRECTION('ref_axis',(-1.,-7.105427357601E-15,1.4081690688991E-16));
#114918=DIRECTION('',(0.913545457642598,-0.406736643075807,-1.28642645648558E-16));
#114919=DIRECTION('center_axis',(-1.4081690688991E-16,0.,-1.));
#114920=DIRECTION('ref_axis',(-1.,0.,1.4081690688991E-16));
#114921=DIRECTION('center_axis',(-1.4081690688991E-16,0.,-1.));
#114922=DIRECTION('ref_axis',(1.,0.,-1.4081690688991E-16));
#114923=DIRECTION('',(-0.433019338752863,0.249998488182549,-0.866022521746677));
#114924=DIRECTION('center_axis',(-1.4081690688991E-16,0.,-1.));
#114925=DIRECTION('ref_axis',(-1.,0.,1.4081690688991E-16));
#114926=DIRECTION('center_axis',(-1.4081690688991E-16,0.,-1.));
#114927=DIRECTION('ref_axis',(-1.,0.,1.4081690688991E-16));
#114928=DIRECTION('center_axis',(-1.4081690688991E-16,0.,-1.));
#114929=DIRECTION('ref_axis',(-1.,0.,1.4081690688991E-16));
#114930=DIRECTION('',(0.456775406784116,-0.203374579494969,0.866022521746663));
#114931=DIRECTION('center_axis',(-1.4081690688991E-16,0.,-1.));
#114932=DIRECTION('ref_axis',(-1.,0.,1.40816906889911E-16));
#114933=DIRECTION('',(-0.866025403784435,0.500000000000007,1.2195101864901E-16));
#114934=DIRECTION('center_axis',(1.4081690688991E-16,0.,1.));
#114935=DIRECTION('ref_axis',(-1.,0.,1.4081690688991E-16));
#114936=DIRECTION('',(0.913545457642598,-0.406736643075807,-1.28642645648558E-16));
#114937=DIRECTION('center_axis',(-1.4081690688991E-16,0.,-1.));
#114938=DIRECTION('ref_axis',(-1.,0.,1.17174841180864E-16));
#114939=DIRECTION('center_axis',(0.499072844768408,0.866560035746466,7.86457209402E-6));
#114940=DIRECTION('ref_axis',(2.65573233462647E-6,7.54612252265976E-6,-0.999999999968002));
#114941=DIRECTION('center_axis',(-0.407714137590654,-0.913109622086449,
7.86457233598189E-6));
#114942=DIRECTION('ref_axis',(0.774356189803017,-0.345763669669441,-0.529924500330448));
#114943=DIRECTION('center_axis',(-1.4081690688991E-16,0.,-1.));
#114944=DIRECTION('ref_axis',(-1.,0.,1.13676889660403E-16));
#114945=DIRECTION('center_axis',(0.499112366250355,0.866537273151309,-9.77058284535403E-6));
#114946=DIRECTION('ref_axis',(0.757907285851051,-0.436548602171899,-0.484769908302541));
#114947=DIRECTION('center_axis',(-0.40767249208604,-0.913128216134457,-9.77051569036097E-6));
#114948=DIRECTION('ref_axis',(0.798668832019631,-0.356566110901516,-0.484756336025602));
#114949=DIRECTION('center_axis',(-1.4081690688991E-16,0.,-1.));
#114950=DIRECTION('ref_axis',(-1.,0.,1.15974593313694E-16));
#114951=DIRECTION('center_axis',(-0.5022485166105,-0.864723324094289,1.81624798677622E-5));
#114952=DIRECTION('ref_axis',(0.748201970507648,-0.434560065157467,0.501349539841027));
#114953=DIRECTION('center_axis',(0.404361609857045,0.914599195355573,1.81316452956218E-5));
#114954=DIRECTION('ref_axis',(0.79293690758283,-0.350582289842627,0.498340364250858));
#114955=DIRECTION('center_axis',(-1.4081690688991E-16,0.,-1.));
#114956=DIRECTION('ref_axis',(-1.,0.,1.16261524579732E-16));
#114957=DIRECTION('center_axis',(-0.502260200672834,-0.86471653764575,1.84940694697466E-5));
#114958=DIRECTION('ref_axis',(0.749689077418704,-0.435458542073202,-0.498339387701367));
#114959=DIRECTION('center_axis',(0.404349252216125,0.914604658794748,1.85257207050329E-5));
#114960=DIRECTION('ref_axis',(0.791361267750536,-0.349852852736373,-0.50134850686572));
#114961=DIRECTION('center_axis',(-1.4081690688991E-16,0.,-1.));
#114962=DIRECTION('ref_axis',(-1.,0.,1.40816906889911E-16));
#114963=DIRECTION('center_axis',(-1.4081690688991E-16,0.,-1.));
#114964=DIRECTION('ref_axis',(-1.,0.,1.4081690688991E-16));
#114965=DIRECTION('',(-0.913545457642598,0.406736643075807,1.28642645648558E-16));
#114966=DIRECTION('center_axis',(-1.4081690688991E-16,0.,-1.));
#114967=DIRECTION('ref_axis',(-1.,0.,1.4081690688991E-16));
#114968=DIRECTION('center_axis',(-1.4081690688991E-16,0.,-1.));
#114969=DIRECTION('ref_axis',(-1.,0.,1.4081690688991E-16));
#114970=DIRECTION('center_axis',(-1.4081690688991E-16,0.,-1.));
#114971=DIRECTION('ref_axis',(-1.,0.,1.4081690688991E-16));
#114972=DIRECTION('',(0.951056516295151,-0.309016994374955,-1.33924836902177E-16));
#114973=DIRECTION('center_axis',(1.4081690688991E-16,0.,1.));
#114974=DIRECTION('ref_axis',(1.,0.,-1.4081690688991E-16));
#114975=DIRECTION('',(-0.45677552787782,0.203374797931578,0.866022406579777));
#114976=DIRECTION('center_axis',(1.4081690688991E-16,0.,1.));
#114977=DIRECTION('ref_axis',(-1.,2.1316282072803E-14,1.40816906889911E-16));
#114978=DIRECTION('',(0.475534671805163,-0.154505557223394,-0.866022406579786));
#114979=DIRECTION('center_axis',(-1.4081690688991E-16,0.,-1.));
#114980=DIRECTION('ref_axis',(-1.,0.,1.40816906889911E-16));
#114981=DIRECTION('center_axis',(-1.4081690688991E-16,0.,-1.));
#114982=DIRECTION('ref_axis',(-1.,0.,1.4081690688991E-16));
#114983=DIRECTION('',(-0.913545457642598,0.406736643075807,1.28642645648558E-16));
#114984=DIRECTION('center_axis',(1.4081690688991E-16,0.,1.));
#114985=DIRECTION('ref_axis',(-1.,1.77635683940025E-14,1.4081690688991E-16));
#114986=DIRECTION('',(0.951056516295151,-0.309016994374955,-1.33924836902177E-16));
#114987=DIRECTION('center_axis',(-1.4081690688991E-16,0.,-1.));
#114988=DIRECTION('ref_axis',(-1.,0.,1.4081690688991E-16));
#114989=DIRECTION('center_axis',(-1.4081690688991E-16,0.,-1.));
#114990=DIRECTION('ref_axis',(1.,0.,-1.4081690688991E-16));
#114991=DIRECTION('',(-0.456779171296622,0.203366124261496,-0.866022521746652));
#114992=DIRECTION('center_axis',(-1.4081690688991E-16,0.,-1.));
#114993=DIRECTION('ref_axis',(-1.,0.,1.4081690688991E-16));
#114994=DIRECTION('center_axis',(-1.4081690688991E-16,0.,-1.));
#114995=DIRECTION('ref_axis',(-1.,0.,1.4081690688991E-16));
#114996=DIRECTION('center_axis',(-1.4081690688991E-16,0.,-1.));
#114997=DIRECTION('ref_axis',(-1.,0.,1.4081690688991E-16));
#114998=DIRECTION('',(0.475531575574881,-0.154514440939472,0.866022521746654));
#114999=DIRECTION('center_axis',(-1.4081690688991E-16,0.,-1.));
#115000=DIRECTION('ref_axis',(-1.,0.,1.40816906889911E-16));
#115001=DIRECTION('',(-0.913545457642598,0.406736643075807,1.28642645648558E-16));
#115002=DIRECTION('center_axis',(1.4081690688991E-16,0.,1.));
#115003=DIRECTION('ref_axis',(-1.,2.04281036531029E-14,1.4081690688991E-16));
#115004=DIRECTION('',(0.951056516295151,-0.309016994374955,-1.33924836902177E-16));
#115005=DIRECTION('center_axis',(-1.4081690688991E-16,0.,-1.));
#115006=DIRECTION('ref_axis',(-1.,0.,1.17174841180864E-16));
#115007=DIRECTION('center_axis',(0.405758682640175,0.913980246723231,7.86457213173083E-6));
#115008=DIRECTION('ref_axis',(1.85239945587365E-6,7.78238369388909E-6,-0.999999999968002));
#115009=DIRECTION('center_axis',(-0.310034691293475,-0.950725244291277,
7.86457228997841E-6));
#115010=DIRECTION('ref_axis',(0.806256330617388,-0.262927277567195,-0.529924500330461));
#115011=DIRECTION('center_axis',(-1.4081690688991E-16,0.,-1.));
#115012=DIRECTION('ref_axis',(-1.,0.,1.13676889660403E-16));
#115013=DIRECTION('center_axis',(0.405800366956845,0.913961739944417,-9.7705859397404E-6));
#115014=DIRECTION('ref_axis',(0.799387144965416,-0.354934259363339,-0.484769908301082));
#115015=DIRECTION('center_axis',(-0.30999133032007,-0.950739383338531,-9.77051572543388E-6));
#115016=DIRECTION('ref_axis',(0.831564948215717,-0.27112917876648,-0.48475633602915));
#115017=DIRECTION('center_axis',(-1.4081690688991E-16,0.,-1.));
#115018=DIRECTION('ref_axis',(-1.,0.,1.15974593313694E-16));
#115019=DIRECTION('center_axis',(-0.409108946466016,-0.9124855448672,1.81624797290291E-5));
#115020=DIRECTION('ref_axis',(0.789527137637376,-0.353971097461394,0.501349539838333));
#115021=DIRECTION('center_axis',(0.306544826252831,0.951856222950118,1.81316453078655E-5));
#115022=DIRECTION('ref_axis',(0.825238944245296,-0.265777286959786,0.49834036424637));
#115023=DIRECTION('center_axis',(-1.4081690688991E-16,0.,-1.));
#115024=DIRECTION('ref_axis',(-1.,0.,1.16261524579732E-16));
#115025=DIRECTION('center_axis',(-0.409121275899226,-0.912480016912458,
1.84940689712829E-5));
#115026=DIRECTION('ref_axis',(0.791100014430625,-0.354709207425649,-0.49833938770213));
#115027=DIRECTION('center_axis',(0.306531965219087,0.951860364736195,1.85257126434399E-5));
#115028=DIRECTION('ref_axis',(0.823595688995553,-0.265216544997509,-0.501348506856782));
#115029=DIRECTION('center_axis',(-1.4081690688991E-16,0.,-1.));
#115030=DIRECTION('ref_axis',(-1.,0.,1.40816906889911E-16));
#115031=DIRECTION('center_axis',(-1.4081690688991E-16,0.,-1.));
#115032=DIRECTION('ref_axis',(-1.,0.,1.4081690688991E-16));
#115033=DIRECTION('',(-0.951056516295151,0.309016994374955,1.33924836902177E-16));
#115034=DIRECTION('center_axis',(-1.4081690688991E-16,0.,-1.));
#115035=DIRECTION('ref_axis',(-1.,0.,1.4081690688991E-16));
#115036=DIRECTION('center_axis',(-1.4081690688991E-16,0.,-1.));
#115037=DIRECTION('ref_axis',(-1.,0.,1.4081690688991E-16));
#115038=DIRECTION('center_axis',(-1.4081690688991E-16,0.,-1.));
#115039=DIRECTION('ref_axis',(-1.,0.,1.4081690688991E-16));
#115040=DIRECTION('',(0.978147600733804,-0.207911690817766,-1.37739719617121E-16));
#115041=DIRECTION('center_axis',(1.4081690688991E-16,0.,1.));
#115042=DIRECTION('ref_axis',(1.,0.,-1.4081690688991E-16));
#115043=DIRECTION('',(-0.475531718838045,0.154514645521707,0.866022406579781));
#115044=DIRECTION('center_axis',(1.4081690688991E-16,0.,1.));
#115045=DIRECTION('ref_axis',(-1.,-4.08562073062058E-14,1.40816906889911E-16));
#115046=DIRECTION('',(0.489079871579872,-0.103952251140486,-0.866022406579784));
#115047=DIRECTION('center_axis',(-1.4081690688991E-16,0.,-1.));
#115048=DIRECTION('ref_axis',(-1.,0.,1.40816906889911E-16));
#115049=DIRECTION('center_axis',(-1.4081690688991E-16,0.,-1.));
#115050=DIRECTION('ref_axis',(-1.,0.,1.4081690688991E-16));
#115051=DIRECTION('',(-0.951056516295151,0.309016994374955,1.33924836902177E-16));
#115052=DIRECTION('center_axis',(1.4081690688991E-16,0.,1.));
#115053=DIRECTION('ref_axis',(-1.,-3.28626015289046E-14,1.4081690688991E-16));
#115054=DIRECTION('',(0.978147600733804,-0.207911690817766,-1.37739719617121E-16));
#115055=DIRECTION('center_axis',(-1.4081690688991E-16,0.,-1.));
#115056=DIRECTION('ref_axis',(-1.,0.,1.4081690688991E-16));
#115057=DIRECTION('center_axis',(-1.4081690688991E-16,0.,-1.));
#115058=DIRECTION('ref_axis',(1.,0.,-1.4081690688991E-16));
#115059=DIRECTION('',(-0.475534435652379,0.154505638525967,-0.866022521746667));
#115060=DIRECTION('center_axis',(-1.4081690688991E-16,0.,-1.));
#115061=DIRECTION('ref_axis',(-1.,0.,1.4081690688991E-16));
#115062=DIRECTION('center_axis',(-1.4081690688991E-16,0.,-1.));
#115063=DIRECTION('ref_axis',(-1.,0.,1.4081690688991E-16));
#115064=DIRECTION('center_axis',(-1.4081690688991E-16,0.,-1.));
#115065=DIRECTION('ref_axis',(-1.,0.,1.4081690688991E-16));
#115066=DIRECTION('',(0.489077720912262,-0.103961409834809,0.86602252174665));
#115067=DIRECTION('center_axis',(-1.4081690688991E-16,0.,-1.));
#115068=DIRECTION('ref_axis',(-1.,0.,1.40816906889911E-16));
#115069=DIRECTION('',(-0.951056516295151,0.309016994374955,1.33924836902177E-16));
#115070=DIRECTION('center_axis',(1.4081690688991E-16,0.,1.));
#115071=DIRECTION('ref_axis',(-1.,-2.66453525910038E-14,1.4081690688991E-16));
#115072=DIRECTION('',(0.978147600733804,-0.207911690817766,-1.37739719617121E-16));
#115073=DIRECTION('center_axis',(-1.4081690688991E-16,0.,-1.));
#115074=DIRECTION('ref_axis',(-1.,0.,1.17174841180864E-16));
#115075=DIRECTION('center_axis',(0.307998943474507,0.951386698854223,7.86457204724389E-6));
#115076=DIRECTION('ref_axis',(1.02877119897224E-6,7.93337936481566E-6,-0.999999999968002));
#115077=DIRECTION('center_axis',(-0.208958440039582,-0.977924521767592,
7.8645723171832E-6));
#115078=DIRECTION('ref_axis',(0.829322958353485,-0.177210199190913,-0.529924500330509));
#115079=DIRECTION('center_axis',(-1.4081690688991E-16,0.,-1.));
#115080=DIRECTION('ref_axis',(-1.,0.,1.13676889660403E-16));
#115081=DIRECTION('center_axis',(0.308042333922939,0.951372650655801,-9.77059018674394E-6));
#115082=DIRECTION('ref_axis',(0.832108751234766,-0.269431182533443,-0.484769908304082));
#115083=DIRECTION('center_axis',(-0.208913838669525,-0.97793405090369,-9.77051623324827E-6));
#115084=DIRECTION('ref_axis',(0.855350264824845,-0.182721698612272,-0.484756336029055));
#115085=DIRECTION('center_axis',(-1.4081690688991E-16,0.,-1.));
#115086=DIRECTION('ref_axis',(-1.,0.,1.15974593313694E-16));
#115087=DIRECTION('center_axis',(-0.311487093092559,-0.950250383060629,
1.81624797254184E-5));
#115088=DIRECTION('ref_axis',(0.822202080228268,-0.26950394834807,0.501349539835342));
#115089=DIRECTION('center_axis',(0.205369473383598,0.978684514577291,1.81316452366172E-5));
#115090=DIRECTION('ref_axis',(0.848499490337296,-0.178060372501941,0.498340364251));
#115091=DIRECTION('center_axis',(-1.4081690688991E-16,0.,-1.));
#115092=DIRECTION('ref_axis',(-1.,0.,1.16261524579732E-16));
#115093=DIRECTION('center_axis',(-0.311499932817119,-0.95024617416378,1.84940604347653E-5));
#115094=DIRECTION('ref_axis',(0.82384349413835,-0.270073604474662,-0.498339387698762));
#115095=DIRECTION('center_axis',(0.205356249868039,0.978687289330424,1.85257103484312E-5));
#115096=DIRECTION('ref_axis',(0.846806623518866,-0.177674469289364,-0.501348506856578));
#115097=DIRECTION('center_axis',(-1.4081690688991E-16,0.,-1.));
#115098=DIRECTION('ref_axis',(-1.,0.,1.40816906889911E-16));
#115099=DIRECTION('center_axis',(-1.4081690688991E-16,0.,-1.));
#115100=DIRECTION('ref_axis',(-1.,0.,1.4081690688991E-16));
#115101=DIRECTION('',(-0.978147600733804,0.207911690817766,1.37739719617121E-16));
#115102=DIRECTION('center_axis',(-1.4081690688991E-16,0.,-1.));
#115103=DIRECTION('ref_axis',(-1.,0.,1.4081690688991E-16));
#115104=DIRECTION('center_axis',(-1.4081690688991E-16,0.,-1.));
#115105=DIRECTION('ref_axis',(-1.,0.,1.4081690688991E-16));
#115106=DIRECTION('center_axis',(-1.4081690688991E-16,0.,-1.));
#115107=DIRECTION('ref_axis',(-1.,0.,1.4081690688991E-16));
#115108=DIRECTION('',(0.994521895368273,-0.104528463267661,-1.40045497140051E-16));
#115109=DIRECTION('center_axis',(1.4081690688991E-16,0.,1.));
#115110=DIRECTION('ref_axis',(1.,0.,-1.4081690688991E-16));
#115111=DIRECTION('',(-0.489077884775286,0.103961598321231,0.866022406579776));
#115112=DIRECTION('center_axis',(1.4081690688991E-16,0.,1.));
#115113=DIRECTION('ref_axis',(-1.,1.59872115546023E-14,1.40816906889911E-16));
#115114=DIRECTION('',(0.497266609935035,-0.0522600224406424,-0.866022406579773));
#115115=DIRECTION('center_axis',(-1.4081690688991E-16,0.,-1.));
#115116=DIRECTION('ref_axis',(-1.,0.,1.40816906889911E-16));
#115117=DIRECTION('center_axis',(-1.4081690688991E-16,0.,-1.));
#115118=DIRECTION('ref_axis',(-1.,0.,1.4081690688991E-16));
#115119=DIRECTION('',(-0.978147600733804,0.207911690817766,1.37739719617121E-16));
#115120=DIRECTION('center_axis',(1.4081690688991E-16,0.,1.));
#115121=DIRECTION('ref_axis',(-1.,2.1316282072803E-14,1.4081690688991E-16));
#115122=DIRECTION('',(0.994521895368273,-0.104528463267661,-1.40045497140051E-16));
#115123=DIRECTION('center_axis',(-1.4081690688991E-16,0.,-1.));
#115124=DIRECTION('ref_axis',(-1.,0.,1.4081690688991E-16));
#115125=DIRECTION('center_axis',(-1.4081690688991E-16,0.,-1.));
#115126=DIRECTION('ref_axis',(1.,0.,-1.4081690688991E-16));
#115127=DIRECTION('',(-0.489079645219224,0.103952356682314,-0.866022521746652));
#115128=DIRECTION('center_axis',(-1.4081690688991E-16,0.,-1.));
#115129=DIRECTION('ref_axis',(-1.,0.,1.4081690688991E-16));
#115130=DIRECTION('center_axis',(-1.4081690688991E-16,0.,-1.));
#115131=DIRECTION('ref_axis',(-1.,0.,1.4081690688991E-16));
#115132=DIRECTION('center_axis',(-1.4081690688991E-16,0.,-1.));
#115133=DIRECTION('ref_axis',(-1.,0.,1.4081690688991E-16));
#115134=DIRECTION('',(0.497265428393238,-0.0522693557686635,0.866022521746645));
#115135=DIRECTION('center_axis',(-1.4081690688991E-16,0.,-1.));
#115136=DIRECTION('ref_axis',(-1.,0.,1.40816906889911E-16));
#115137=DIRECTION('',(-0.978147600733804,0.207911690817766,1.37739719617121E-16));
#115138=DIRECTION('center_axis',(1.4081690688991E-16,0.,1.));
#115139=DIRECTION('ref_axis',(-1.,2.57571741713036E-14,1.4081690688991E-16));
#115140=DIRECTION('',(0.994521895368273,-0.104528463267661,-1.40045497140051E-16));
#115141=DIRECTION('center_axis',(-1.4081690688991E-16,0.,-1.));
#115142=DIRECTION('ref_axis',(-1.,0.,1.17174841180864E-16));
#115143=DIRECTION('center_axis',(0.20686470343119,0.978369559222114,7.8645720103081E-6));
#115144=DIRECTION('ref_axis',(1.93871496019889E-7,7.99745532505487E-6,-0.999999999968001));
#115145=DIRECTION('center_axis',(-0.105592796389228,-0.994409453539563,
7.86457228715899E-6));
#115146=DIRECTION('ref_axis',(0.843303350210933,-0.0895515687886337,-0.529924500330482));
#115147=DIRECTION('center_axis',(-1.4081690688991E-16,0.,-1.));
#115148=DIRECTION('ref_axis',(-1.,0.,1.13676889660403E-16));
#115149=DIRECTION('center_axis',(0.206909324620437,0.978360123517741,-9.77058714809604E-6));
#115150=DIRECTION('ref_axis',(0.855713599898024,-0.180976161286533,-0.484769908302439));
#115151=DIRECTION('center_axis',(-0.105547443284143,-0.99441426836139,-9.7705161524926E-6));
#115152=DIRECTION('ref_axis',(0.86976418494061,-0.0923122812912277,-0.484756336026055));
#115153=DIRECTION('center_axis',(-1.4081690688991E-16,0.,-1.));
#115154=DIRECTION('ref_axis',(-1.,0.,1.15974593313694E-16));
#115155=DIRECTION('center_axis',(-0.210452521944373,-0.977604079204551,
1.81624797413716E-5));
#115156=DIRECTION('ref_axis',(0.845868804767752,-0.182084057578221,0.501349539838848));
#115157=DIRECTION('center_axis',(0.101944049587634,0.99479013385986,1.81316452525535E-5));
#115158=DIRECTION('ref_axis',(0.862463698455125,-0.0883925913422159,0.4983403642521));
#115159=DIRECTION('center_axis',(-1.4081690688991E-16,0.,-1.));
#115160=DIRECTION('ref_axis',(-1.,0.,1.16261524579732E-16));
#115161=DIRECTION('center_axis',(-0.210465731282001,-0.977601235480962,
1.84940588659675E-5));
#115162=DIRECTION('ref_axis',(0.847560772124303,-0.182479018596253,-0.498339387694976));
#115163=DIRECTION('center_axis',(0.101930608471476,0.994791511178816,1.85257108169065E-5));
#115164=DIRECTION('ref_axis',(0.860739767465406,-0.0881857549145489,-0.501348506862991));
#115165=DIRECTION('center_axis',(-1.4081690688991E-16,0.,-1.));
#115166=DIRECTION('ref_axis',(-1.,0.,1.40816906889911E-16));
#115167=DIRECTION('center_axis',(-1.4081690688991E-16,0.,-1.));
#115168=DIRECTION('ref_axis',(-1.,0.,1.4081690688991E-16));
#115169=DIRECTION('',(-0.994521895368273,0.104528463267661,1.40045497140051E-16));
#115170=DIRECTION('center_axis',(-1.4081690688991E-16,0.,-1.));
#115171=DIRECTION('ref_axis',(-1.,0.,1.4081690688991E-16));
#115172=DIRECTION('center_axis',(-1.4081690688991E-16,0.,-1.));
#115173=DIRECTION('ref_axis',(-1.,0.,1.4081690688991E-16));
#115174=DIRECTION('center_axis',(-1.4081690688991E-16,0.,-1.));
#115175=DIRECTION('ref_axis',(-1.,0.,1.4081690688991E-16));
#115176=DIRECTION('',(1.,0.,-1.40816906889911E-16));
#115177=DIRECTION('center_axis',(1.4081690688991E-16,0.,1.));
#115178=DIRECTION('ref_axis',(1.,0.,-1.4081690688991E-16));
#115179=DIRECTION('',(-0.49726561106078,0.0522695260941912,0.866022406579783));
#115180=DIRECTION('center_axis',(1.4081690688991E-16,0.,1.));
#115181=DIRECTION('ref_axis',(-1.,6.21724893790088E-15,1.40816906889911E-16));
#115182=DIRECTION('',(0.500005191251985,4.77800116551749E-6,-0.866022406579782));
#115183=DIRECTION('center_axis',(-1.4081690688991E-16,0.,-1.));
#115184=DIRECTION('ref_axis',(-1.,0.,1.40816906889911E-16));
#115185=DIRECTION('center_axis',(-1.4081690688991E-16,0.,-1.));
#115186=DIRECTION('ref_axis',(-1.,0.,1.4081690688991E-16));
#115187=DIRECTION('',(-0.994521895368273,0.104528463267661,1.40045497140051E-16));
#115188=DIRECTION('center_axis',(1.4081690688991E-16,0.,1.));
#115189=DIRECTION('ref_axis',(-1.,1.33226762955019E-14,1.4081690688991E-16));
#115190=DIRECTION('',(1.,0.,-1.40816906889911E-16));
#115191=DIRECTION('center_axis',(-1.4081690688991E-16,0.,-1.));
#115192=DIRECTION('ref_axis',(-1.,0.,1.4081690688991E-16));
#115193=DIRECTION('center_axis',(-1.4081690688991E-16,0.,-1.));
#115194=DIRECTION('ref_axis',(1.,0.,-1.4081690688991E-16));
#115195=DIRECTION('',(-0.497266395846527,0.0522601510654385,-0.866022521746648));
#115196=DIRECTION('center_axis',(-1.4081690688991E-16,0.,-1.));
#115197=DIRECTION('ref_axis',(-1.,0.,1.4081690688991E-16));
#115198=DIRECTION('center_axis',(-1.4081690688991E-16,0.,-1.));
#115199=DIRECTION('ref_axis',(-1.,0.,1.4081690688991E-16));
#115200=DIRECTION('center_axis',(-1.4081690688991E-16,0.,-1.));
#115201=DIRECTION('ref_axis',(-1.,0.,1.4081690688991E-16));
#115202=DIRECTION('',(0.500004991781227,-4.62770265276808E-6,0.866022521746657));
#115203=DIRECTION('center_axis',(-1.4081690688991E-16,0.,-1.));
#115204=DIRECTION('ref_axis',(-1.,0.,1.40816906889911E-16));
#115205=DIRECTION('',(-0.994521895368273,0.104528463267661,1.40045497140051E-16));
#115206=DIRECTION('center_axis',(1.4081690688991E-16,0.,1.));
#115207=DIRECTION('ref_axis',(-1.,1.86517468137026E-14,1.4081690688991E-16));
#115208=DIRECTION('',(1.,0.,-1.40816906889911E-16));
#115209=DIRECTION('center_axis',(-1.4081690688991E-16,0.,-1.));
#115210=DIRECTION('ref_axis',(-1.,0.,1.17174841180864E-16));
#115211=DIRECTION('center_axis',(0.103464010407829,0.994633197962182,7.86457202866399E-6));
#115212=DIRECTION('ref_axis',(-6.43152314414483E-7,7.97390954032807E-6,
-0.999999999968002));
#115213=DIRECTION('center_axis',(-0.00107025596492904,-0.999999427244995,
7.86457228903988E-6));
#115214=DIRECTION('ref_axis',(0.848044334090885,-0.000911792658859396,-0.529924500330466));
#115215=DIRECTION('center_axis',(-1.4081690688991E-16,0.,-1.));
#115216=DIRECTION('ref_axis',(-1.,0.,1.13676889660403E-16));
#115217=DIRECTION('center_axis',(0.103509373457831,0.994628478131862,-9.77058613603921E-6));
#115218=DIRECTION('ref_axis',(0.869943071289075,-0.0905383273444945,-0.484769908304747));
#115219=DIRECTION('center_axis',(-0.00102464802304199,-0.999999475000345,
-9.77051628002253E-6));
#115220=DIRECTION('ref_axis',(0.874648786634557,-0.000891471298430306,-0.484756336026278));
#115221=DIRECTION('center_axis',(-1.4081690688991E-16,0.,-1.));
#115222=DIRECTION('ref_axis',(-1.,0.,1.15974593313694E-16));
#115223=DIRECTION('center_axis',(-0.10711218892573,-0.994246940479911,1.8162479773676E-5));
#115224=DIRECTION('ref_axis',(0.860268013676508,-0.0926692157708133,0.50134953983573));
#115225=DIRECTION('center_axis',(-0.0025982945487866,0.999996624262643,
1.81316452254577E-5));
#115226=DIRECTION('ref_axis',(0.866978573812158,0.00224363754549588,0.49834036425038));
#115227=DIRECTION('center_axis',(-1.4081690688991E-16,0.,-1.));
#115228=DIRECTION('ref_axis',(-1.,0.,1.16261524579732E-16));
#115229=DIRECTION('center_axis',(-0.1071256231494,-0.994245493086503,1.84940621084383E-5));
#115230=DIRECTION('ref_axis',(0.861991996926058,-0.0928851544032616,-0.498339387693677));
#115231=DIRECTION('center_axis',(-0.00261180600216756,0.999996589057285,
1.85257107824588E-5));
#115232=DIRECTION('ref_axis',(0.865242466405598,0.00226914104443776,-0.501348506856535));
#115233=DIRECTION('center_axis',(-1.4081690688991E-16,0.,-1.));
#115234=DIRECTION('ref_axis',(-1.,0.,1.40816906889911E-16));
#115235=DIRECTION('center_axis',(-1.4081690688991E-16,0.,-1.));
#115236=DIRECTION('ref_axis',(-1.,0.,1.4081690688991E-16));
#115237=DIRECTION('',(-1.,0.,1.40816906889911E-16));
#115238=DIRECTION('center_axis',(-1.4081690688991E-16,0.,-1.));
#115239=DIRECTION('ref_axis',(-1.,0.,1.4081690688991E-16));
#115240=DIRECTION('center_axis',(-1.4081690688991E-16,0.,-1.));
#115241=DIRECTION('ref_axis',(-1.,0.,1.4081690688991E-16));
#115242=DIRECTION('center_axis',(-1.4081690688991E-16,0.,-1.));
#115243=DIRECTION('ref_axis',(-1.,0.,1.4081690688991E-16));
#115244=DIRECTION('',(0.994521895368274,0.104528463267647,-1.40045497140052E-16));
#115245=DIRECTION('center_axis',(1.4081690688991E-16,0.,1.));
#115246=DIRECTION('ref_axis',(1.,0.,-1.4081690688991E-16));
#115247=DIRECTION('',(-0.500005191251985,4.77800116551749E-6,0.866022406579782));
#115248=DIRECTION('center_axis',(1.4081690688991E-16,0.,1.));
#115249=DIRECTION('ref_axis',(-1.,0.,1.40816906889911E-16));
#115250=DIRECTION('',(0.49726561106078,0.0522695260941878,-0.866022406579783));
#115251=DIRECTION('center_axis',(-1.4081690688991E-16,0.,-1.));
#115252=DIRECTION('ref_axis',(-1.,0.,1.40816906889911E-16));
#115253=DIRECTION('center_axis',(-1.4081690688991E-16,0.,-1.));
#115254=DIRECTION('ref_axis',(-1.,0.,1.4081690688991E-16));
#115255=DIRECTION('',(-1.,0.,1.40816906889911E-16));
#115256=DIRECTION('center_axis',(1.4081690688991E-16,0.,1.));
#115257=DIRECTION('ref_axis',(-1.,0.,1.4081690688991E-16));
#115258=DIRECTION('',(0.994521895368274,0.104528463267647,-1.40045497140052E-16));
#115259=DIRECTION('center_axis',(-1.4081690688991E-16,0.,-1.));
#115260=DIRECTION('ref_axis',(-1.,0.,1.4081690688991E-16));
#115261=DIRECTION('center_axis',(-1.4081690688991E-16,0.,-1.));
#115262=DIRECTION('ref_axis',(1.,0.,-1.4081690688991E-16));
#115263=DIRECTION('',(-0.500004991781227,-4.62770265276808E-6,-0.866022521746657));
#115264=DIRECTION('center_axis',(-1.4081690688991E-16,0.,-1.));
#115265=DIRECTION('ref_axis',(-1.,0.,1.4081690688991E-16));
#115266=DIRECTION('center_axis',(-1.4081690688991E-16,0.,-1.));
#115267=DIRECTION('ref_axis',(-1.,0.,1.4081690688991E-16));
#115268=DIRECTION('center_axis',(-1.4081690688991E-16,0.,-1.));
#115269=DIRECTION('ref_axis',(-1.,0.,1.4081690688991E-16));
#115270=DIRECTION('',(0.497266395846506,0.0522601510654325,0.86602252174666));
#115271=DIRECTION('center_axis',(-1.4081690688991E-16,0.,-1.));
#115272=DIRECTION('ref_axis',(-1.,0.,1.40816906889911E-16));
#115273=DIRECTION('',(-1.,0.,1.40816906889911E-16));
#115274=DIRECTION('center_axis',(1.4081690688991E-16,0.,1.));
#115275=DIRECTION('ref_axis',(-1.,0.,1.4081690688991E-16));
#115276=DIRECTION('',(0.994521895368274,0.104528463267647,-1.40045497140052E-16));
#115277=DIRECTION('center_axis',(-1.4081690688991E-16,0.,-1.));
#115278=DIRECTION('ref_axis',(-1.,0.,1.17174841180864E-16));
#115279=DIRECTION('center_axis',(-0.00107025596477632,0.999999427244995,
7.86457201352231E-6));
#115280=DIRECTION('ref_axis',(-1.47312954961581E-6,7.86299989115223E-6,
-0.999999999968002));
#115281=DIRECTION('center_axis',(0.103464010407674,-0.994633197962198,7.86457229252233E-6));
#115282=DIRECTION('ref_axis',(0.843493966781838,0.0877379732620788,-0.529924500330474));
#115283=DIRECTION('center_axis',(-1.4081690688991E-16,0.,-1.));
#115284=DIRECTION('ref_axis',(-1.,0.,1.13676889660403E-16));
#115285=DIRECTION('center_axis',(-0.00102464806169058,0.999999475000305,
-9.77058600455096E-6));
#115286=DIRECTION('ref_axis',(0.87464126434622,0.000891463458123506,-0.484769908302639));
#115287=DIRECTION('center_axis',(0.103509373496272,-0.994628478127862,-9.77051629371499E-6));
#115288=DIRECTION('ref_axis',(0.869950553189069,0.0905391058403209,-0.484756336028388));
#115289=DIRECTION('center_axis',(-1.4081690688991E-16,0.,-1.));
#115290=DIRECTION('ref_axis',(-1.,0.,1.15974593313694E-16));
#115291=DIRECTION('center_axis',(-0.0025983123505633,-0.999996624215829,
1.81624797797147E-5));
#115292=DIRECTION('ref_axis',(0.865241946200303,-0.00223907064277699,0.501349539840388));
#115293=DIRECTION('center_axis',(-0.107112171226437,0.994246942387253,1.81316453094968E-5));
#115294=DIRECTION('ref_axis',(0.861994650482721,0.0928552846704071,0.49834036425715));
#115295=DIRECTION('center_axis',(-1.4081690688991E-16,0.,-1.));
#115296=DIRECTION('ref_axis',(-1.,0.,1.16261524579732E-16));
#115297=DIRECTION('center_axis',(-0.00261182427503963,-0.999996589010146,
1.84940601579397E-5));
#115298=DIRECTION('ref_axis',(0.866979057020118,-0.00227362102098959,-0.498339387702758));
#115299=DIRECTION('center_axis',(-0.107125604985124,0.994245495043035,1.85257064812721E-5));
#115300=DIRECTION('ref_axis',(0.860265387813178,0.092699175819291,-0.501348506862309));
#115301=DIRECTION('center_axis',(-1.4081690688991E-16,0.,-1.));
#115302=DIRECTION('ref_axis',(-1.,0.,1.40816906889911E-16));
#115303=DIRECTION('center_axis',(-1.4081690688991E-16,0.,-1.));
#115304=DIRECTION('ref_axis',(-1.,0.,1.4081690688991E-16));
#115305=DIRECTION('',(-0.994521895368274,-0.104528463267647,1.40045497140052E-16));
#115306=DIRECTION('center_axis',(-1.4081690688991E-16,0.,-1.));
#115307=DIRECTION('ref_axis',(-1.,0.,1.4081690688991E-16));
#115308=DIRECTION('center_axis',(-1.4081690688991E-16,0.,-1.));
#115309=DIRECTION('ref_axis',(-1.,0.,1.4081690688991E-16));
#115310=DIRECTION('center_axis',(-1.4081690688991E-16,0.,-1.));
#115311=DIRECTION('ref_axis',(-1.,0.,1.4081690688991E-16));
#115312=DIRECTION('',(0.978147600733807,0.207911690817753,-1.37739719617122E-16));
#115313=DIRECTION('center_axis',(1.4081690688991E-16,0.,1.));
#115314=DIRECTION('ref_axis',(1.,0.,-1.4081690688991E-16));
#115315=DIRECTION('',(-0.497266609935035,-0.0522600224406356,0.866022406579773));
#115316=DIRECTION('center_axis',(1.4081690688991E-16,0.,1.));
#115317=DIRECTION('ref_axis',(-1.,0.,1.40816906889911E-16));
#115318=DIRECTION('',(0.489077884775245,0.103961598321228,-0.8660224065798));
#115319=DIRECTION('center_axis',(-1.4081690688991E-16,0.,-1.));
#115320=DIRECTION('ref_axis',(-1.,0.,1.40816906889911E-16));
#115321=DIRECTION('center_axis',(-1.4081690688991E-16,0.,-1.));
#115322=DIRECTION('ref_axis',(-1.,0.,1.4081690688991E-16));
#115323=DIRECTION('',(-0.994521895368274,-0.104528463267647,1.40045497140052E-16));
#115324=DIRECTION('center_axis',(1.4081690688991E-16,0.,1.));
#115325=DIRECTION('ref_axis',(-1.,0.,1.4081690688991E-16));
#115326=DIRECTION('',(0.978147600733807,0.207911690817753,-1.37739719617122E-16));
#115327=DIRECTION('center_axis',(-1.4081690688991E-16,0.,-1.));
#115328=DIRECTION('ref_axis',(-1.,0.,1.4081690688991E-16));
#115329=DIRECTION('center_axis',(-1.4081690688991E-16,0.,-1.));
#115330=DIRECTION('ref_axis',(1.,0.,-1.4081690688991E-16));
#115331=DIRECTION('',(-0.497265428393217,-0.0522693557686642,-0.866022521746657));
#115332=DIRECTION('center_axis',(-1.4081690688991E-16,0.,-1.));
#115333=DIRECTION('ref_axis',(-1.,0.,1.4081690688991E-16));
#115334=DIRECTION('center_axis',(-1.4081690688991E-16,0.,-1.));
#115335=DIRECTION('ref_axis',(-1.,0.,1.4081690688991E-16));
#115336=DIRECTION('center_axis',(-1.4081690688991E-16,0.,-1.));
#115337=DIRECTION('ref_axis',(-1.,0.,1.4081690688991E-16));
#115338=DIRECTION('',(0.489079645219225,0.1039523566823,0.866022521746653));
#115339=DIRECTION('center_axis',(-1.4081690688991E-16,0.,-1.));
#115340=DIRECTION('ref_axis',(-1.,0.,1.40816906889911E-16));
#115341=DIRECTION('',(-0.994521895368274,-0.104528463267647,1.40045497140052E-16));
#115342=DIRECTION('center_axis',(1.4081690688991E-16,0.,1.));
#115343=DIRECTION('ref_axis',(-1.,0.,1.4081690688991E-16));
#115344=DIRECTION('',(0.978147600733807,0.207911690817753,-1.37739719617122E-16));
#115345=DIRECTION('center_axis',(-1.4081690688991E-16,0.,-1.));
#115346=DIRECTION('ref_axis',(-1.,0.,1.17174841180864E-16));
#115347=DIRECTION('center_axis',(-0.105592796389083,0.994409453539578,7.86457203806509E-6));
#115348=DIRECTION('ref_axis',(-2.28696684648491E-6,7.66594161629955E-6,
-0.999999999968002));
#115349=DIRECTION('center_axis',(0.206864703430992,-0.978369559222156,7.86457234781368E-6));
#115350=DIRECTION('ref_axis',(0.829702103060314,0.175426463587569,-0.529924500330426));
#115351=DIRECTION('center_axis',(-1.4081690688991E-16,0.,-1.));
#115352=DIRECTION('ref_axis',(-1.,0.,1.13676889660403E-16));
#115353=DIRECTION('center_axis',(-0.105547443321288,0.994414268357446,-9.77058366484796E-6));
#115354=DIRECTION('ref_axis',(0.869756704679168,0.0923114872005142,-0.484769908303376));
#115355=DIRECTION('center_axis',(0.206909324660093,-0.978360123509355,-9.77051398001622E-6));
#115356=DIRECTION('ref_axis',(0.855720959435109,0.180977717588947,-0.484756336028474));
#115357=DIRECTION('center_axis',(-1.4081690688991E-16,0.,-1.));
#115358=DIRECTION('ref_axis',(-1.,0.,1.15974593313694E-16));
#115359=DIRECTION('center_axis',(0.10194403187845,-0.994790135674098,1.8162479803541E-5));
#115360=DIRECTION('ref_axis',(0.860736106899776,0.088215606211404,0.501349539841987));
#115361=DIRECTION('center_axis',(-0.210452504541383,0.97760408295153,1.81316452253489E-5));
#115362=DIRECTION('ref_axis',(0.847566533385468,0.182449589865907,0.498340364251887));
#115363=DIRECTION('center_axis',(-1.4081690688991E-16,0.,-1.));
#115364=DIRECTION('ref_axis',(-1.,0.,1.16261524579732E-16));
#115365=DIRECTION('center_axis',(0.101930590294196,-0.994791513041927,1.84940609616093E-5));
#115366=DIRECTION('ref_axis',(0.862467313149233,0.088362822628976,-0.498339387692949));
#115367=DIRECTION('center_axis',(-0.210465713418174,0.977601239326228,1.8525709565287E-5));
#115368=DIRECTION('ref_axis',(0.845863061613277,0.182113579025382,-0.501348506862022));
#115369=DIRECTION('center_axis',(-1.4081690688991E-16,0.,-1.));
#115370=DIRECTION('ref_axis',(-1.,0.,1.40816906889911E-16));
#115371=DIRECTION('center_axis',(-1.4081690688991E-16,0.,-1.));
#115372=DIRECTION('ref_axis',(-1.,0.,1.4081690688991E-16));
#115373=DIRECTION('',(-0.978147600733807,-0.207911690817753,1.37739719617122E-16));
#115374=DIRECTION('center_axis',(-1.4081690688991E-16,0.,-1.));
#115375=DIRECTION('ref_axis',(-1.,0.,1.4081690688991E-16));
#115376=DIRECTION('center_axis',(-1.4081690688991E-16,0.,-1.));
#115377=DIRECTION('ref_axis',(-1.,0.,1.4081690688991E-16));
#115378=DIRECTION('center_axis',(-1.4081690688991E-16,0.,-1.));
#115379=DIRECTION('ref_axis',(-1.,0.,1.4081690688991E-16));
#115380=DIRECTION('',(0.951056516295155,0.309016994374942,-1.33924836902178E-16));
#115381=DIRECTION('center_axis',(1.4081690688991E-16,0.,1.));
#115382=DIRECTION('ref_axis',(1.,0.,-1.4081690688991E-16));
#115383=DIRECTION('',(-0.489079871579893,-0.103952251140478,0.866022406579773));
#115384=DIRECTION('center_axis',(1.4081690688991E-16,0.,1.));
#115385=DIRECTION('ref_axis',(-1.,0.,1.40816906889911E-16));
#115386=DIRECTION('',(0.475531718838024,0.154514645521709,-0.866022406579792));
#115387=DIRECTION('center_axis',(-1.4081690688991E-16,0.,-1.));
#115388=DIRECTION('ref_axis',(-1.,0.,1.40816906889911E-16));
#115389=DIRECTION('center_axis',(-1.4081690688991E-16,0.,-1.));
#115390=DIRECTION('ref_axis',(-1.,0.,1.4081690688991E-16));
#115391=DIRECTION('',(-0.978147600733807,-0.207911690817753,1.37739719617122E-16));
#115392=DIRECTION('center_axis',(1.4081690688991E-16,0.,1.));
#115393=DIRECTION('ref_axis',(-1.,0.,1.4081690688991E-16));
#115394=DIRECTION('',(0.951056516295155,0.309016994374942,-1.33924836902177E-16));
#115395=DIRECTION('center_axis',(-1.4081690688991E-16,0.,-1.));
#115396=DIRECTION('ref_axis',(-1.,0.,1.4081690688991E-16));
#115397=DIRECTION('center_axis',(-1.4081690688991E-16,0.,-1.));
#115398=DIRECTION('ref_axis',(1.,0.,-1.4081690688991E-16));
#115399=DIRECTION('',(-0.489077720912262,-0.103961409834802,-0.86602252174665));
#115400=DIRECTION('center_axis',(-1.4081690688991E-16,0.,-1.));
#115401=DIRECTION('ref_axis',(-1.,0.,1.4081690688991E-16));
#115402=DIRECTION('center_axis',(-1.4081690688991E-16,0.,-1.));
#115403=DIRECTION('ref_axis',(-1.,0.,1.4081690688991E-16));
#115404=DIRECTION('center_axis',(-1.4081690688991E-16,0.,-1.));
#115405=DIRECTION('ref_axis',(-1.,0.,1.4081690688991E-16));
#115406=DIRECTION('',(0.475534435652402,0.154505638525938,0.86602252174666));
#115407=DIRECTION('center_axis',(-1.4081690688991E-16,0.,-1.));
#115408=DIRECTION('ref_axis',(-1.,0.,1.40816906889911E-16));
#115409=DIRECTION('',(-0.978147600733807,-0.207911690817753,1.37739719617122E-16));
#115410=DIRECTION('center_axis',(1.4081690688991E-16,0.,1.));
#115411=DIRECTION('ref_axis',(-1.,0.,1.4081690688991E-16));
#115412=DIRECTION('',(0.951056516295155,0.309016994374942,-1.33924836902178E-16));
#115413=DIRECTION('center_axis',(-1.4081690688991E-16,0.,-1.));
#115414=DIRECTION('ref_axis',(-1.,0.,1.17174841180864E-16));
#115415=DIRECTION('center_axis',(-0.208958440039409,0.977924521767629,7.86457200610629E-6));
#115416=DIRECTION('ref_axis',(-3.07574767837473E-6,7.38489362573465E-6,
-0.999999999968002));
#115417=DIRECTION('center_axis',(0.307998943474345,-0.951386698854275,7.86457233122683E-6));
#115418=DIRECTION('ref_axis',(0.806819849471267,0.261192944867712,-0.529924500330468));
#115419=DIRECTION('center_axis',(-1.4081690688991E-16,0.,-1.));
#115420=DIRECTION('ref_axis',(-1.,0.,1.13676889660403E-16));
#115421=DIRECTION('center_axis',(-0.208913838706489,0.977934050895793,-9.77058458900962E-6));
#115422=DIRECTION('ref_axis',(0.855342908549112,0.182720126972052,-0.4847699083009));
#115423=DIRECTION('center_axis',(0.308042333962515,-0.951372650642987,-9.77051510954378E-6));
#115424=DIRECTION('ref_axis',(0.832115907779389,0.269433499591945,-0.484756336026793));
#115425=DIRECTION('center_axis',(-1.4081690688991E-16,0.,-1.));
#115426=DIRECTION('ref_axis',(-1.,0.,1.15974593313694E-16));
#115427=DIRECTION('center_axis',(0.205369455961064,-0.978684518232704,1.81624798317175E-5));
#115428=DIRECTION('ref_axis',(0.846799862697162,0.177703774424654,0.501349539833536));
#115429=DIRECTION('center_axis',(-0.311487076176632,0.95025038860617,1.8131645292547E-5));
#115430=DIRECTION('ref_axis',(0.82385229998436,0.270044939175662,0.498340364245255));
#115431=DIRECTION('center_axis',(-1.4081690688991E-16,0.,-1.));
#115432=DIRECTION('ref_axis',(-1.,0.,1.16261524579732E-16));
#115433=DIRECTION('center_axis',(0.205356231986127,-0.978687293083153,1.84940623151564E-5));
#115434=DIRECTION('ref_axis',(0.848506196903301,0.178031144702363,-0.49833938769945));
#115435=DIRECTION('center_axis',(-0.311499915451504,0.95024617985578,1.85257141175826E-5));
#115436=DIRECTION('ref_axis',(0.822193282701921,0.269532707749929,-0.501348506862074));
#115437=DIRECTION('center_axis',(-1.4081690688991E-16,0.,-1.));
#115438=DIRECTION('ref_axis',(-1.,0.,1.40816906889911E-16));
#115439=DIRECTION('center_axis',(-1.4081690688991E-16,0.,-1.));
#115440=DIRECTION('ref_axis',(-1.,0.,1.4081690688991E-16));
#115441=DIRECTION('',(-0.951056516295155,-0.309016994374942,1.33924836902178E-16));
#115442=DIRECTION('center_axis',(-1.4081690688991E-16,0.,-1.));
#115443=DIRECTION('ref_axis',(-1.,0.,1.4081690688991E-16));
#115444=DIRECTION('center_axis',(-1.4081690688991E-16,0.,-1.));
#115445=DIRECTION('ref_axis',(-1.,0.,1.4081690688991E-16));
#115446=DIRECTION('center_axis',(-1.4081690688991E-16,0.,-1.));
#115447=DIRECTION('ref_axis',(-1.,0.,1.4081690688991E-16));
#115448=DIRECTION('',(0.913545457642603,0.406736643075795,-1.28642645648559E-16));
#115449=DIRECTION('center_axis',(1.4081690688991E-16,0.,1.));
#115450=DIRECTION('ref_axis',(1.,0.,-1.4081690688991E-16));
#115451=DIRECTION('',(-0.475534671805141,-0.154505557223416,0.866022406579794));
#115452=DIRECTION('center_axis',(1.4081690688991E-16,0.,1.));
#115453=DIRECTION('ref_axis',(-1.,0.,1.40816906889911E-16));
#115454=DIRECTION('',(0.456775527877798,0.20337479793158,-0.866022406579788));
#115455=DIRECTION('center_axis',(-1.4081690688991E-16,0.,-1.));
#115456=DIRECTION('ref_axis',(-1.,0.,1.40816906889911E-16));
#115457=DIRECTION('center_axis',(-1.4081690688991E-16,0.,-1.));
#115458=DIRECTION('ref_axis',(-1.,0.,1.4081690688991E-16));
#115459=DIRECTION('',(-0.951056516295155,-0.309016994374942,1.33924836902178E-16));
#115460=DIRECTION('center_axis',(1.4081690688991E-16,0.,1.));
#115461=DIRECTION('ref_axis',(-1.,0.,1.4081690688991E-16));
#115462=DIRECTION('',(0.913545457642603,0.406736643075795,-1.28642645648559E-16));
#115463=DIRECTION('center_axis',(-1.4081690688991E-16,0.,-1.));
#115464=DIRECTION('ref_axis',(-1.,0.,1.4081690688991E-16));
#115465=DIRECTION('center_axis',(-1.4081690688991E-16,0.,-1.));
#115466=DIRECTION('ref_axis',(1.,0.,-1.4081690688991E-16));
#115467=DIRECTION('',(-0.47553157557486,-0.154514440939468,-0.866022521746666));
#115468=DIRECTION('center_axis',(-1.4081690688991E-16,0.,-1.));
#115469=DIRECTION('ref_axis',(-1.,0.,1.4081690688991E-16));
#115470=DIRECTION('center_axis',(-1.4081690688991E-16,0.,-1.));
#115471=DIRECTION('ref_axis',(-1.,0.,1.4081690688991E-16));
#115472=DIRECTION('center_axis',(-1.4081690688991E-16,0.,-1.));
#115473=DIRECTION('ref_axis',(-1.,0.,1.4081690688991E-16));
#115474=DIRECTION('',(0.456779171296622,0.203366124261496,0.866022521746652));
#115475=DIRECTION('center_axis',(-1.4081690688991E-16,0.,-1.));
#115476=DIRECTION('ref_axis',(-1.,0.,1.40816906889911E-16));
#115477=DIRECTION('',(-0.951056516295155,-0.309016994374942,1.33924836902178E-16));
#115478=DIRECTION('center_axis',(1.4081690688991E-16,0.,1.));
#115479=DIRECTION('ref_axis',(-1.,0.,1.4081690688991E-16));
#115480=DIRECTION('',(0.913545457642603,0.406736643075795,-1.28642645648559E-16));
#115481=DIRECTION('center_axis',(-1.4081690688991E-16,0.,-1.));
#115482=DIRECTION('ref_axis',(-1.,0.,1.17174841180864E-16));
#115483=DIRECTION('center_axis',(-0.31003469129331,0.950725244291331,7.86457199748011E-6));
#115484=DIRECTION('ref_axis',(-3.83083002565344E-6,7.02293521153946E-6,
-0.999999999968002));
#115485=DIRECTION('center_axis',(0.405758682640086,-0.91398024672327,7.8645722503889E-6));
#115486=DIRECTION('ref_axis',(0.775097908773512,0.3440977415858,-0.529924500330454));
#115487=DIRECTION('center_axis',(-1.4081690688991E-16,0.,-1.));
#115488=DIRECTION('ref_axis',(-1.,0.,1.13676889660403E-16));
#115489=DIRECTION('center_axis',(-0.309991330354646,0.950739383327257,-9.77058136445211E-6));
#115490=DIRECTION('ref_axis',(0.83155779651886,0.27112684679551,-0.484769908302303));
#115491=DIRECTION('center_axis',(0.405800366992456,-0.913961739928606,-9.77051546410327E-6));
#115492=DIRECTION('ref_axis',(0.79939402010551,0.354937311790544,-0.484756336027137));
#115493=DIRECTION('center_axis',(-1.4081690688991E-16,0.,-1.));
#115494=DIRECTION('ref_axis',(-1.,0.,1.15974593313694E-16));
#115495=DIRECTION('center_axis',(0.306544809308013,-0.951856228406601,1.8162479602898E-5));
#115496=DIRECTION('ref_axis',(0.823585901985266,0.265244982896496,0.501349539841568));
#115497=DIRECTION('center_axis',(-0.409108930222373,0.91248555215058,1.81316452010363E-5));
#115498=DIRECTION('ref_axis',(0.791111768373646,0.354681619618225,0.49834036425491));
#115499=DIRECTION('center_axis',(-1.4081690688991E-16,0.,-1.));
#115500=DIRECTION('ref_axis',(-1.,0.,1.16261524579732E-16));
#115501=DIRECTION('center_axis',(0.306531947823564,-0.951860370338771,1.84940577497957E-5));
#115502=DIRECTION('ref_axis',(0.825248669208761,0.265748920300067,-0.498339387695291));
#115503=DIRECTION('center_axis',(-0.409121259232272,0.912480024384643,1.85257063074674E-5));
#115504=DIRECTION('ref_axis',(0.789515382129243,0.353998779724516,-0.501348506864107));
#115505=DIRECTION('center_axis',(-1.4081690688991E-16,0.,-1.));
#115506=DIRECTION('ref_axis',(-1.,0.,1.40816906889911E-16));
#115507=DIRECTION('center_axis',(-1.4081690688991E-16,0.,-1.));
#115508=DIRECTION('ref_axis',(-1.,0.,1.4081690688991E-16));
#115509=DIRECTION('',(-0.913545457642603,-0.406736643075795,1.28642645648559E-16));
#115510=DIRECTION('center_axis',(-1.4081690688991E-16,0.,-1.));
#115511=DIRECTION('ref_axis',(-1.,0.,1.4081690688991E-16));
#115512=DIRECTION('center_axis',(-1.4081690688991E-16,0.,-1.));
#115513=DIRECTION('ref_axis',(-1.,0.,1.4081690688991E-16));
#115514=DIRECTION('center_axis',(-1.4081690688991E-16,0.,-1.));
#115515=DIRECTION('ref_axis',(-1.,0.,1.4081690688991E-16));
#115516=DIRECTION('',(0.866025403784442,0.499999999999995,-1.21951018649011E-16));
#115517=DIRECTION('center_axis',(1.4081690688991E-16,0.,1.));
#115518=DIRECTION('ref_axis',(1.,0.,-1.4081690688991E-16));
#115519=DIRECTION('',(-0.456779414654131,-0.203366068089033,0.866022406579781));
#115520=DIRECTION('center_axis',(1.4081690688991E-16,0.,1.));
#115521=DIRECTION('ref_axis',(-1.,0.,1.40816906889911E-16));
#115522=DIRECTION('',(0.433014808647734,0.250006733496366,-0.866022406579785));
#115523=DIRECTION('center_axis',(-1.4081690688991E-16,0.,-1.));
#115524=DIRECTION('ref_axis',(-1.,0.,1.40816906889911E-16));
#115525=DIRECTION('center_axis',(-1.4081690688991E-16,0.,-1.));
#115526=DIRECTION('ref_axis',(-1.,0.,1.4081690688991E-16));
#115527=DIRECTION('',(-0.913545457642603,-0.406736643075795,1.28642645648559E-16));
#115528=DIRECTION('center_axis',(1.4081690688991E-16,0.,1.));
#115529=DIRECTION('ref_axis',(-1.,8.88178419700125E-16,1.4081690688991E-16));
#115530=DIRECTION('',(0.866025403784442,0.499999999999995,-1.21951018649011E-16));
#115531=DIRECTION('center_axis',(-1.4081690688991E-16,0.,-1.));
#115532=DIRECTION('ref_axis',(-1.,0.,1.4081690688991E-16));
#115533=DIRECTION('center_axis',(-1.4081690688991E-16,0.,-1.));
#115534=DIRECTION('ref_axis',(1.,0.,-1.4081690688991E-16));
#115535=DIRECTION('',(-0.456775406784116,-0.203374579494969,-0.866022521746663));
#115536=DIRECTION('center_axis',(-1.4081690688991E-16,0.,-1.));
#115537=DIRECTION('ref_axis',(-1.,0.,1.4081690688991E-16));
#115538=DIRECTION('center_axis',(-1.4081690688991E-16,0.,-1.));
#115539=DIRECTION('ref_axis',(-1.,0.,1.4081690688991E-16));
#115540=DIRECTION('center_axis',(-1.4081690688991E-16,0.,-1.));
#115541=DIRECTION('ref_axis',(-1.,0.,1.4081690688991E-16));
#115542=DIRECTION('',(0.433019338752908,0.24999848818253,0.86602252174666));
#115543=DIRECTION('center_axis',(-1.4081690688991E-16,0.,-1.));
#115544=DIRECTION('ref_axis',(-1.,0.,1.40816906889911E-16));
#115545=DIRECTION('',(-0.913545457642603,-0.406736643075795,1.28642645648559E-16));
#115546=DIRECTION('center_axis',(1.4081690688991E-16,0.,1.));
#115547=DIRECTION('ref_axis',(-1.,8.88178419700125E-16,1.4081690688991E-16));
#115548=DIRECTION('',(0.866025403784442,0.499999999999995,-1.21951018649011E-16));
#115549=DIRECTION('center_axis',(-1.4081690688991E-16,0.,-1.));
#115550=DIRECTION('ref_axis',(-1.,0.,1.17174841180864E-16));
#115551=DIRECTION('center_axis',(-0.40771413759047,0.913109622086531,7.86457197304048E-6));
#115552=DIRECTION('ref_axis',(-4.54394095516333E-6,6.58403203744326E-6,
-0.999999999968002));
#115553=DIRECTION('center_axis',(0.499072844768321,-0.866560035746517,7.86457228842995E-6));
#115554=DIRECTION('ref_axis',(0.734883833187592,0.423232531439894,-0.529924500330462));
#115555=DIRECTION('center_axis',(-1.4081690688991E-16,0.,-1.));
#115556=DIRECTION('ref_axis',(-1.,0.,1.13676889660403E-16));
#115557=DIRECTION('center_axis',(-0.407672492120574,0.913128216119038,-9.77058401182242E-6));
#115558=DIRECTION('ref_axis',(0.798661963254375,0.356563044147856,-0.484769908305663));
#115559=DIRECTION('center_axis',(0.499112366279568,-0.866537273134484,-9.77052188210463E-6));
#115560=DIRECTION('ref_axis',(0.757913804263745,0.436552356525934,-0.484756336026784));
#115561=DIRECTION('center_axis',(-1.4081690688991E-16,0.,-1.));
#115562=DIRECTION('ref_axis',(-1.,0.,1.15974593313694E-16));
#115563=DIRECTION('center_axis',(0.404361593575301,-0.914599202553428,1.81624797722619E-5));
#115564=DIRECTION('ref_axis',(0.791348561789598,0.349880111830676,0.501349539841106));
#115565=DIRECTION('center_axis',(-0.502248501217083,0.864723333035739,1.81316452000092E-5));
#115566=DIRECTION('ref_axis',(0.749703650686959,0.43543233401829,0.498340364247198));
#115567=DIRECTION('center_axis',(-1.4081690688991E-16,0.,-1.));
#115568=DIRECTION('ref_axis',(-1.,0.,1.16261524579732E-16));
#115569=DIRECTION('center_axis',(0.404349235495135,-0.914604666187785,1.84940535722811E-5));
#115570=DIRECTION('ref_axis',(0.792949544396578,0.350555095114516,-0.498339387697293));
#115571=DIRECTION('center_axis',(-0.502260184874095,0.86471654682158,1.85257151301963E-5));
#115572=DIRECTION('ref_axis',(0.748187385817233,0.434586366991526,-0.501348506858335));
#115573=DIRECTION('center_axis',(-1.4081690688991E-16,0.,-1.));
#115574=DIRECTION('ref_axis',(-1.,0.,1.40816906889911E-16));
#115575=DIRECTION('center_axis',(-1.4081690688991E-16,0.,-1.));
#115576=DIRECTION('ref_axis',(-1.,0.,1.4081690688991E-16));
#115577=DIRECTION('',(-0.866025403784442,-0.499999999999995,1.21951018649011E-16));
#115578=DIRECTION('center_axis',(-1.4081690688991E-16,0.,-1.));
#115579=DIRECTION('ref_axis',(-1.,0.,1.4081690688991E-16));
#115580=DIRECTION('center_axis',(-1.4081690688991E-16,0.,-1.));
#115581=DIRECTION('ref_axis',(-1.,0.,1.4081690688991E-16));
#115582=DIRECTION('center_axis',(-1.4081690688991E-16,0.,-1.));
#115583=DIRECTION('ref_axis',(-1.,0.,1.4081690688991E-16));
#115584=DIRECTION('',(0.80901699437495,0.587785252292469,-1.13923270769253E-16));
#115585=DIRECTION('center_axis',(1.4081690688991E-16,0.,1.));
#115586=DIRECTION('ref_axis',(1.,0.,-1.4081690688991E-16));
#115587=DIRECTION('',(-0.433019586648882,-0.249998457755582,0.866022406579796));
#115588=DIRECTION('center_axis',(1.4081690688991E-16,0.,1.));
#115589=DIRECTION('ref_axis',(-1.,0.,1.40816906889911E-16));
#115590=DIRECTION('',(0.40450988855993,0.293899542971733,-0.866022406579783));
#115591=DIRECTION('center_axis',(-1.4081690688991E-16,0.,-1.));
#115592=DIRECTION('ref_axis',(-1.,0.,1.40816906889911E-16));
#115593=DIRECTION('center_axis',(-1.4081690688991E-16,0.,-1.));
#115594=DIRECTION('ref_axis',(-1.,0.,1.4081690688991E-16));
#115595=DIRECTION('',(-0.866025403784442,-0.499999999999995,1.21951018649011E-16));
#115596=DIRECTION('center_axis',(1.4081690688991E-16,0.,1.));
#115597=DIRECTION('ref_axis',(-1.,8.88178419700125E-16,1.4081690688991E-16));
#115598=DIRECTION('',(0.80901699437495,0.587785252292469,-1.13923270769253E-16));
#115599=DIRECTION('center_axis',(-1.4081690688991E-16,0.,-1.));
#115600=DIRECTION('ref_axis',(-1.,0.,1.4081690688991E-16));
#115601=DIRECTION('center_axis',(-1.4081690688991E-16,0.,-1.));
#115602=DIRECTION('ref_axis',(1.,0.,-1.4081690688991E-16));
#115603=DIRECTION('',(-0.433014711050233,-0.250006503598672,-0.866022521746663));
#115604=DIRECTION('center_axis',(-1.4081690688991E-16,0.,-1.));
#115605=DIRECTION('ref_axis',(-1.,0.,1.4081690688991E-16));
#115606=DIRECTION('center_axis',(-1.4081690688991E-16,0.,-1.));
#115607=DIRECTION('ref_axis',(-1.,0.,1.4081690688991E-16));
#115608=DIRECTION('center_axis',(-1.4081690688991E-16,0.,-1.));
#115609=DIRECTION('ref_axis',(-1.,0.,1.4081690688991E-16));
#115610=DIRECTION('',(0.4045152557187,0.293891816351548,0.866022521746648));
#115611=DIRECTION('center_axis',(-1.4081690688991E-16,0.,-1.));
#115612=DIRECTION('ref_axis',(-1.,0.,1.40816906889911E-16));
#115613=DIRECTION('',(-0.866025403784442,-0.499999999999995,1.21951018649011E-16));
#115614=DIRECTION('center_axis',(1.4081690688991E-16,0.,1.));
#115615=DIRECTION('ref_axis',(-1.,0.,1.4081690688991E-16));
#115616=DIRECTION('',(0.80901699437495,0.587785252292469,-1.13923270769253E-16));
#115617=DIRECTION('center_axis',(-1.4081690688991E-16,0.,-1.));
#115618=DIRECTION('ref_axis',(-1.,0.,1.17174841180864E-16));
#115619=DIRECTION('center_axis',(-0.500926582476549,0.865489779781664,7.86457205664354E-6));
#115620=DIRECTION('ref_axis',(-5.2072675490952E-6,6.07299293807615E-6,-0.999999999968002));
#115621=DIRECTION('center_axis',(0.586919060371506,-0.809645611678824,7.86457244280782E-6));
#115622=DIRECTION('ref_axis',(0.686618216541034,0.497730297112336,-0.529924500330448));
#115623=DIRECTION('center_axis',(-1.4081690688991E-16,0.,-1.));
#115624=DIRECTION('ref_axis',(-1.,0.,1.13676889660403E-16));
#115625=DIRECTION('center_axis',(-0.500887108752517,0.86551262508994,-9.77058817878717E-6));
#115626=DIRECTION('ref_axis',(0.757015822393057,0.438092662174431,-0.484769908302365));
#115627=DIRECTION('center_axis',(0.586955986039185,-0.809618842639736,-9.7705214324476E-6));
#115628=DIRECTION('ref_axis',(0.708129726178571,0.513384442288636,-0.484756336026925));
#115629=DIRECTION('center_axis',(-1.4081690688991E-16,0.,-1.));
#115630=DIRECTION('ref_axis',(-1.,0.,1.15974593313694E-16));
#115631=DIRECTION('center_axis',(0.497748107605451,-0.867321636444818,1.81624796098486E-5));
#115632=DIRECTION('ref_axis',(0.750441041148855,0.430681881041565,0.501349539844131));
#115633=DIRECTION('center_axis',(-0.589885332530219,0.807487024129154,1.8131645283277E-5));
#115634=DIRECTION('ref_axis',(0.700081622909386,0.511412360641763,0.498340364256578));
#115635=DIRECTION('center_axis',(-1.4081690688991E-16,0.,-1.));
#115636=DIRECTION('ref_axis',(-1.,0.,1.16261524579732E-16));
#115637=DIRECTION('center_axis',(0.497736388330941,-0.867328361919083,1.84940567397459E-5));
#115638=DIRECTION('ref_axis',(0.751962698443092,0.431520514949629,-0.498339387694561));
#115639=DIRECTION('center_axis',(-0.589896242832074,0.807479053814649,1.85257114861555E-5));
#115640=DIRECTION('ref_axis',(0.698662091932204,0.510412535075371,-0.501348506864087));
#115641=DIRECTION('center_axis',(-1.4081690688991E-16,0.,-1.));
#115642=DIRECTION('ref_axis',(-1.,0.,1.40816906889911E-16));
#115643=DIRECTION('center_axis',(-1.4081690688991E-16,0.,-1.));
#115644=DIRECTION('ref_axis',(-1.,0.,1.4081690688991E-16));
#115645=DIRECTION('',(-0.80901699437495,-0.587785252292469,1.13923270769253E-16));
#115646=DIRECTION('center_axis',(-1.4081690688991E-16,0.,-1.));
#115647=DIRECTION('ref_axis',(-1.,0.,1.4081690688991E-16));
#115648=DIRECTION('center_axis',(-1.4081690688991E-16,0.,-1.));
#115649=DIRECTION('ref_axis',(-1.,0.,1.4081690688991E-16));
#115650=DIRECTION('center_axis',(-1.4081690688991E-16,0.,-1.));
#115651=DIRECTION('ref_axis',(-1.,0.,1.4081690688991E-16));
#115652=DIRECTION('',(0.743144825477398,0.669130606358854,-1.04647355694969E-16));
#115653=DIRECTION('center_axis',(1.4081690688991E-16,0.,1.));
#115654=DIRECTION('ref_axis',(1.,0.,-1.4081690688991E-16));
#115655=DIRECTION('',(-0.404515505437168,-0.293891812003425,0.866022406579793));
#115656=DIRECTION('center_axis',(1.4081690688991E-16,0.,1.));
#115657=DIRECTION('ref_axis',(-1.,8.88178419700125E-16,1.40816906889911E-16));
#115658=DIRECTION('',(0.371573073483921,0.334572327551833,-0.866022406579796));
#115659=DIRECTION('center_axis',(-1.4081690688991E-16,0.,-1.));
#115660=DIRECTION('ref_axis',(-1.,0.,1.40816906889911E-16));
#115661=DIRECTION('center_axis',(-1.4081690688991E-16,0.,-1.));
#115662=DIRECTION('ref_axis',(-1.,0.,1.4081690688991E-16));
#115663=DIRECTION('',(-0.80901699437495,-0.587785252292469,1.13923270769253E-16));
#115664=DIRECTION('center_axis',(1.4081690688991E-16,0.,1.));
#115665=DIRECTION('ref_axis',(-1.,0.,1.4081690688991E-16));
#115666=DIRECTION('',(0.743144825477398,0.669130606358854,-1.04647355694969E-16));
#115667=DIRECTION('center_axis',(-1.4081690688991E-16,0.,-1.));
#115668=DIRECTION('ref_axis',(-1.,0.,1.4081690688991E-16));
#115669=DIRECTION('center_axis',(-1.4081690688991E-16,0.,-1.));
#115670=DIRECTION('ref_axis',(1.,0.,-1.4081690688991E-16));
#115671=DIRECTION('',(-0.40450981552795,-0.293899304131695,-0.866022521746663));
#115672=DIRECTION('center_axis',(-1.4081690688991E-16,0.,-1.));
#115673=DIRECTION('ref_axis',(-1.,0.,1.4081690688991E-16));
#115674=DIRECTION('center_axis',(-1.4081690688991E-16,0.,-1.));
#115675=DIRECTION('ref_axis',(-1.,0.,1.4081690688991E-16));
#115676=DIRECTION('center_axis',(-1.4081690688991E-16,0.,-1.));
#115677=DIRECTION('ref_axis',(-1.,0.,1.4081690688991E-16));
#115678=DIRECTION('',(0.371579218892551,0.33456520427975,0.866022521746664));
#115679=DIRECTION('center_axis',(-1.4081690688991E-16,0.,-1.));
#115680=DIRECTION('ref_axis',(-1.,0.,1.40816906889911E-16));
#115681=DIRECTION('',(-0.80901699437495,-0.587785252292469,1.13923270769253E-16));
#115682=DIRECTION('center_axis',(1.4081690688991E-16,0.,1.));
#115683=DIRECTION('ref_axis',(-1.,0.,1.4081690688991E-16));
#115684=DIRECTION('',(0.743144825477398,0.669130606358854,-1.04647355694969E-16));
#115685=DIRECTION('center_axis',(-1.4081690688991E-16,0.,-1.));
#115686=DIRECTION('ref_axis',(-1.,0.,1.17174841180864E-16));
#115687=DIRECTION('center_axis',(-0.588650770899332,0.808387450334164,7.86457198365576E-6));
#115688=DIRECTION('ref_axis',(-5.81354222511576E-6,5.49541667256838E-6,
-0.999999999968002));
#115689=DIRECTION('center_axis',(0.66833486792867,-0.743860540860258,7.86457232182708E-6));
#115690=DIRECTION('ref_axis',(0.630829867029784,0.566774825493066,-0.529924500330461));
#115691=DIRECTION('center_axis',(-1.4081690688991E-16,0.,-1.));
#115692=DIRECTION('ref_axis',(-1.,0.,1.13676889660403E-16));
#115693=DIRECTION('center_axis',(-0.588613901404025,0.808414296619294,-9.77059377784101E-6));
#115694=DIRECTION('ref_axis',(0.707075657763069,0.514822445315911,-0.484769908304826));
#115695=DIRECTION('center_axis',(0.668368793190144,-0.743830058678787,-9.77051413964613E-6));
#115696=DIRECTION('ref_axis',(0.650587230627881,0.584591780669203,-0.484756336026621));
#115697=DIRECTION('center_axis',(-1.4081690688991E-16,0.,-1.));
#115698=DIRECTION('ref_axis',(-1.,0.,1.15974593313694E-16));
#115699=DIRECTION('center_axis',(0.585681189207983,-0.810541512988722,1.81624798474342E-5));
#115700=DIRECTION('ref_axis',(0.701311531424911,0.506765009439859,0.501349539840086));
#115701=DIRECTION('center_axis',(-0.671059256698738,0.741403718408655,1.81316454615391E-5));
#115702=DIRECTION('ref_axis',(0.642789354376861,0.581789246427063,0.498340364250789));
#115703=DIRECTION('center_axis',(-1.4081690688991E-16,0.,-1.));
#115704=DIRECTION('ref_axis',(-1.,0.,1.16261524579732E-16));
#115705=DIRECTION('center_axis',(0.585670237128126,-0.810549426623852,1.84940388037811E-5));
#115706=DIRECTION('ref_axis',(0.702737191804828,0.507758105720191,-0.498339387696485));
#115707=DIRECTION('center_axis',(-0.671069274112383,0.741394651315396,1.85257013794949E-5));
#115708=DIRECTION('ref_axis',(0.641482109968578,0.580646516617888,-0.501348506859026));
#115709=DIRECTION('center_axis',(-1.4081690688991E-16,0.,-1.));
#115710=DIRECTION('ref_axis',(-1.,0.,1.40816906889911E-16));
#115711=DIRECTION('center_axis',(-1.4081690688991E-16,0.,-1.));
#115712=DIRECTION('ref_axis',(-1.,0.,1.4081690688991E-16));
#115713=DIRECTION('',(-0.743144825477398,-0.669130606358854,1.04647355694969E-16));
#115714=DIRECTION('center_axis',(-1.4081690688991E-16,0.,-1.));
#115715=DIRECTION('ref_axis',(-1.,0.,1.4081690688991E-16));
#115716=DIRECTION('center_axis',(-1.4081690688991E-16,0.,-1.));
#115717=DIRECTION('ref_axis',(-1.,0.,1.4081690688991E-16));
#115718=DIRECTION('center_axis',(-1.4081690688991E-16,0.,-1.));
#115719=DIRECTION('ref_axis',(-1.,0.,1.4081690688991E-16));
#115720=DIRECTION('',(0.669130606358862,0.743144825477391,-9.42249022928252E-17));
#115721=DIRECTION('center_axis',(1.4081690688991E-16,0.,1.));
#115722=DIRECTION('ref_axis',(1.,0.,-1.4081690688991E-16));
#115723=DIRECTION('',(-0.371579467697564,-0.334565226058147,0.866022406579793));
#115724=DIRECTION('center_axis',(1.4081690688991E-16,0.,1.));
#115725=DIRECTION('ref_axis',(-1.,-8.88178419700125E-16,1.40816906889911E-16));
#115726=DIRECTION('',(0.334565226058151,0.371579467697541,-0.866022406579802));
#115727=DIRECTION('center_axis',(-1.4081690688991E-16,0.,-1.));
#115728=DIRECTION('ref_axis',(-1.,0.,1.40816906889911E-16));
#115729=DIRECTION('center_axis',(-1.4081690688991E-16,0.,-1.));
#115730=DIRECTION('ref_axis',(-1.,0.,1.4081690688991E-16));
#115731=DIRECTION('',(-0.743144825477398,-0.669130606358854,1.04647355694969E-16));
#115732=DIRECTION('center_axis',(1.4081690688991E-16,0.,1.));
#115733=DIRECTION('ref_axis',(-1.,0.,1.4081690688991E-16));
#115734=DIRECTION('',(0.669130606358862,0.743144825477391,-9.42249022928252E-17));
#115735=DIRECTION('center_axis',(-1.4081690688991E-16,0.,-1.));
#115736=DIRECTION('ref_axis',(-1.,0.,1.4081690688991E-16));
#115737=DIRECTION('center_axis',(-1.4081690688991E-16,0.,-1.));
#115738=DIRECTION('ref_axis',(1.,0.,-1.4081690688991E-16));
#115739=DIRECTION('',(-0.371573025817597,-0.334572082386321,-0.866022521746655));
#115740=DIRECTION('center_axis',(-1.4081690688991E-16,0.,-1.));
#115741=DIRECTION('ref_axis',(-1.,0.,1.4081690688991E-16));
#115742=DIRECTION('center_axis',(-1.4081690688991E-16,0.,-1.));
#115743=DIRECTION('ref_axis',(-1.,0.,1.4081690688991E-16));
#115744=DIRECTION('center_axis',(-1.4081690688991E-16,0.,-1.));
#115745=DIRECTION('ref_axis',(-1.,0.,1.4081690688991E-16));
#115746=DIRECTION('',(0.334572082386318,0.371573025817621,0.866022521746647));
#115747=DIRECTION('center_axis',(-1.4081690688991E-16,0.,-1.));
#115748=DIRECTION('ref_axis',(-1.,0.,1.40816906889911E-16));
#115749=DIRECTION('',(-0.743144825477398,-0.669130606358854,1.04647355694969E-16));
#115750=DIRECTION('center_axis',(1.4081690688991E-16,0.,1.));
#115751=DIRECTION('ref_axis',(-1.,-8.88178419700125E-16,1.4081690688991E-16));
#115752=DIRECTION('',(0.669130606358862,0.743144825477391,-9.42249022928252E-17));
#115753=DIRECTION('center_axis',(-1.4081690688991E-16,0.,-1.));
#115754=DIRECTION('ref_axis',(-1.,0.,1.17174841180864E-16));
#115755=DIRECTION('center_axis',(-0.669925578293108,0.742428258814812,7.86457198741695E-6));
#115756=DIRECTION('ref_axis',(-6.35612244774292E-6,4.85763161650682E-6,
-0.999999999968002));
#115757=DIRECTION('center_axis',(0.742428258814674,-0.669925578293261,7.86457238264939E-6));
#115758=DIRECTION('ref_axis',(0.568130013485845,0.629609650280319,-0.529924500330442));
#115759=DIRECTION('center_axis',(-1.4081690688991E-16,0.,-1.));
#115760=DIRECTION('ref_axis',(-1.,0.,1.13676889660403E-16));
#115761=DIRECTION('center_axis',(-0.669891716969178,0.742458811948934,-9.77058294495678E-6));
#115762=DIRECTION('ref_axis',(0.649388624262771,0.585911726013647,-0.48476990830477));
#115763=DIRECTION('center_axis',(0.742458811969791,-0.669891716946062,-9.77052667155945E-6));
#115764=DIRECTION('ref_axis',(0.58591676523382,0.649394209166528,-0.484756336027614));
#115765=DIRECTION('center_axis',(-1.4081690688991E-16,0.,-1.));
#115766=DIRECTION('ref_axis',(-1.,0.,1.15974593313694E-16));
#115767=DIRECTION('center_axis',(0.667197425140001,-0.744880927099545,1.81624799140914E-5));
#115768=DIRECTION('ref_axis',(0.644498305802315,0.577295914346694,0.501349539838784));
#115769=DIRECTION('center_axis',(-0.744880915222515,0.667197438400742,1.81316451171186E-5));
#115770=DIRECTION('ref_axis',(0.578454551163314,0.645791927479989,0.498340364249305));
#115771=DIRECTION('center_axis',(-1.4081690688991E-16,0.,-1.));
#115772=DIRECTION('ref_axis',(-1.,0.,1.16261524579732E-16));
#115773=DIRECTION('center_axis',(0.667187360268925,-0.744889942176261,1.84940667004621E-5));
#115774=DIRECTION('ref_axis',(0.645812349437408,0.578432592430395,-0.498339387695161));
#115775=DIRECTION('center_axis',(-0.744889929984212,0.667187373880017,1.85257177346086E-5));
#115776=DIRECTION('ref_axis',(0.577273915765294,0.644518813412645,-0.501348506863399));
#115777=DIRECTION('center_axis',(-1.4081690688991E-16,0.,-1.));
#115778=DIRECTION('ref_axis',(-1.,0.,1.40816906889911E-16));
#115779=DIRECTION('center_axis',(-1.4081690688991E-16,0.,-1.));
#115780=DIRECTION('ref_axis',(-1.,0.,1.4081690688991E-16));
#115781=DIRECTION('',(-0.669130606358862,-0.743144825477391,9.42249022928252E-17));
#115782=DIRECTION('center_axis',(-1.4081690688991E-16,0.,-1.));
#115783=DIRECTION('ref_axis',(-1.,0.,1.4081690688991E-16));
#115784=DIRECTION('center_axis',(-1.4081690688991E-16,0.,-1.));
#115785=DIRECTION('ref_axis',(-1.,0.,1.4081690688991E-16));
#115786=DIRECTION('center_axis',(-1.4081690688991E-16,0.,-1.));
#115787=DIRECTION('ref_axis',(-1.,0.,1.4081690688991E-16));
#115788=DIRECTION('',(0.587785252292477,0.809016994374945,-8.27701011433323E-17));
#115789=DIRECTION('center_axis',(1.4081690688991E-16,0.,1.));
#115790=DIRECTION('ref_axis',(1.,0.,-1.4081690688991E-16));
#115791=DIRECTION('',(-0.334572327551837,-0.371573073483898,0.866022406579805));
#115792=DIRECTION('center_axis',(1.4081690688991E-16,0.,1.));
#115793=DIRECTION('ref_axis',(-1.,-8.88178419700125E-16,1.40816906889911E-16));
#115794=DIRECTION('',(0.293891812003446,0.404515505437187,-0.866022406579777));
#115795=DIRECTION('center_axis',(-1.4081690688991E-16,0.,-1.));
#115796=DIRECTION('ref_axis',(-1.,0.,1.40816906889911E-16));
#115797=DIRECTION('center_axis',(-1.4081690688991E-16,0.,-1.));
#115798=DIRECTION('ref_axis',(-1.,0.,1.4081690688991E-16));
#115799=DIRECTION('',(-0.669130606358862,-0.743144825477391,9.42249022928252E-17));
#115800=DIRECTION('center_axis',(1.4081690688991E-16,0.,1.));
#115801=DIRECTION('ref_axis',(-1.,0.,1.4081690688991E-16));
#115802=DIRECTION('',(0.587785252292477,0.809016994374945,-8.27701011433323E-17));
#115803=DIRECTION('center_axis',(-1.4081690688991E-16,0.,-1.));
#115804=DIRECTION('ref_axis',(-1.,0.,1.4081690688991E-16));
#115805=DIRECTION('center_axis',(-1.4081690688991E-16,0.,-1.));
#115806=DIRECTION('ref_axis',(1.,0.,-1.4081690688991E-16));
#115807=DIRECTION('',(-0.334565204279747,-0.371579218892574,-0.866022521746655));
#115808=DIRECTION('center_axis',(-1.4081690688991E-16,0.,-1.));
#115809=DIRECTION('ref_axis',(-1.,0.,1.4081690688991E-16));
#115810=DIRECTION('center_axis',(-1.4081690688991E-16,0.,-1.));
#115811=DIRECTION('ref_axis',(-1.,0.,1.4081690688991E-16));
#115812=DIRECTION('center_axis',(-1.4081690688991E-16,0.,-1.));
#115813=DIRECTION('ref_axis',(-1.,0.,1.4081690688991E-16));
#115814=DIRECTION('',(0.293899304131692,0.404509815527973,0.866022521746654));
#115815=DIRECTION('center_axis',(-1.4081690688991E-16,0.,-1.));
#115816=DIRECTION('ref_axis',(-1.,0.,1.40816906889911E-16));
#115817=DIRECTION('',(-0.669130606358862,-0.743144825477391,9.42249022928252E-17));
#115818=DIRECTION('center_axis',(1.4081690688991E-16,0.,1.));
#115819=DIRECTION('ref_axis',(-1.,0.,1.4081690688991E-16));
#115820=DIRECTION('',(0.587785252292477,0.809016994374945,-8.27701011433323E-17));
#115821=DIRECTION('center_axis',(-1.4081690688991E-16,0.,-1.));
#115822=DIRECTION('ref_axis',(-1.,0.,1.17174841180864E-16));
#115823=DIRECTION('center_axis',(-0.743860540860165,0.668334867928774,7.86457206040205E-6));
#115824=DIRECTION('ref_axis',(-6.82906381692535E-6,4.16662528541507E-6,
-0.999999999968002));
#115825=DIRECTION('center_axis',(0.808387450334043,-0.588650770899498,7.86457228997828E-6));
#115826=DIRECTION('ref_axis',(0.499205608625192,0.685546339984894,-0.529924500330441));
#115827=DIRECTION('center_axis',(-1.4081690688991E-16,0.,-1.));
#115828=DIRECTION('ref_axis',(-1.,0.,1.13676889660403E-16));
#115829=DIRECTION('center_axis',(-0.743830058703291,0.668368793162873,-9.7705803850988E-6));
#115830=DIRECTION('ref_axis',(0.584586753102978,0.650581635232684,-0.484769908301335));
#115831=DIRECTION('center_axis',(0.80841429664589,-0.588613901367499,-9.77051216005777E-6));
#115832=DIRECTION('ref_axis',(0.514826873149602,0.707081738814493,-0.484756336026747));
#115833=DIRECTION('center_axis',(-1.4081690688991E-16,0.,-1.));
#115834=DIRECTION('ref_axis',(-1.,0.,1.15974593313694E-16));
#115835=DIRECTION('center_axis',(0.741403706462381,-0.671059269896459,1.8162479445365E-5));
#115836=DIRECTION('ref_axis',(0.580623821869585,0.641501844407272,0.501349539841839));
#115837=DIRECTION('center_axis',(-0.810541502562996,0.585681203637409,1.8131645405925E-5));
#115838=DIRECTION('ref_axis',(0.507782078838539,0.702719177036071,0.49834036424532));
#115839=DIRECTION('center_axis',(-1.4081690688991E-16,0.,-1.));
#115840=DIRECTION('ref_axis',(-1.,0.,1.16261524579732E-16));
#115841=DIRECTION('center_axis',(0.741394639062402,-0.671069287650314,1.84940740269212E-5));
#115842=DIRECTION('ref_axis',(0.581811851821584,0.642769650609807,-0.498339387701681));
#115843=DIRECTION('center_axis',(-0.810549415915106,0.585670251947697,1.85257082024649E-5));
#115844=DIRECTION('ref_axis',(0.506740987742068,0.701329627217269,-0.501348506858732));
#115845=DIRECTION('center_axis',(-1.4081690688991E-16,0.,-1.));
#115846=DIRECTION('ref_axis',(-1.,0.,1.40816906889911E-16));
#115847=DIRECTION('center_axis',(-1.4081690688991E-16,0.,-1.));
#115848=DIRECTION('ref_axis',(-1.,0.,1.4081690688991E-16));
#115849=DIRECTION('',(-0.587785252292477,-0.809016994374945,8.27701011433323E-17));
#115850=DIRECTION('center_axis',(-1.4081690688991E-16,0.,-1.));
#115851=DIRECTION('ref_axis',(-1.,0.,1.4081690688991E-16));
#115852=DIRECTION('center_axis',(-1.4081690688991E-16,0.,-1.));
#115853=DIRECTION('ref_axis',(-1.,0.,1.4081690688991E-16));
#115854=DIRECTION('center_axis',(-1.4081690688991E-16,0.,-1.));
#115855=DIRECTION('ref_axis',(-1.,0.,1.4081690688991E-16));
#115856=DIRECTION('',(0.500000000000004,0.866025403784436,-7.04084534449558E-17));
#115857=DIRECTION('center_axis',(1.4081690688991E-16,0.,1.));
#115858=DIRECTION('ref_axis',(1.,0.,-1.4081690688991E-16));
#115859=DIRECTION('',(-0.293899542971745,-0.404509888559929,0.86602240657978));
#115860=DIRECTION('center_axis',(1.4081690688991E-16,0.,1.));
#115861=DIRECTION('ref_axis',(-1.,0.,1.40816906889911E-16));
#115862=DIRECTION('',(0.249998457755608,0.433019586648879,-0.866022406579791));
#115863=DIRECTION('center_axis',(-1.4081690688991E-16,0.,-1.));
#115864=DIRECTION('ref_axis',(-1.,0.,1.40816906889911E-16));
#115865=DIRECTION('center_axis',(-1.4081690688991E-16,0.,-1.));
#115866=DIRECTION('ref_axis',(-1.,0.,1.4081690688991E-16));
#115867=DIRECTION('',(-0.587785252292477,-0.809016994374945,8.27701011433323E-17));
#115868=DIRECTION('center_axis',(1.4081690688991E-16,0.,1.));
#115869=DIRECTION('ref_axis',(-1.,1.77635683940025E-15,1.4081690688991E-16));
#115870=DIRECTION('',(0.500000000000004,0.866025403784436,-7.04084534449558E-17));
#115871=DIRECTION('center_axis',(-1.4081690688991E-16,0.,-1.));
#115872=DIRECTION('ref_axis',(-1.,0.,1.4081690688991E-16));
#115873=DIRECTION('center_axis',(-1.4081690688991E-16,0.,-1.));
#115874=DIRECTION('ref_axis',(1.,1.06581410364015E-14,-1.4081690688991E-16));
#115875=DIRECTION('',(-0.293891816351505,-0.404515255718661,-0.866022521746681));
#115876=DIRECTION('center_axis',(-1.4081690688991E-16,0.,-1.));
#115877=DIRECTION('ref_axis',(-1.,0.,1.4081690688991E-16));
#115878=DIRECTION('center_axis',(-1.4081690688991E-16,0.,-1.));
#115879=DIRECTION('ref_axis',(-1.,0.,1.4081690688991E-16));
#115880=DIRECTION('center_axis',(-1.4081690688991E-16,0.,-1.));
#115881=DIRECTION('ref_axis',(-1.,0.,1.4081690688991E-16));
#115882=DIRECTION('',(0.250006503598672,0.433014711050233,0.866022521746663));
#115883=DIRECTION('center_axis',(-1.4081690688991E-16,0.,-1.));
#115884=DIRECTION('ref_axis',(-1.,0.,1.40816906889911E-16));
#115885=DIRECTION('',(-0.587785252292477,-0.809016994374945,8.27701011433323E-17));
#115886=DIRECTION('center_axis',(1.4081690688991E-16,0.,1.));
#115887=DIRECTION('ref_axis',(-1.,0.,1.4081690688991E-16));
#115888=DIRECTION('',(0.500000000000004,0.866025403784436,-7.04084534449558E-17));
#115889=DIRECTION('center_axis',(-1.4081690688991E-16,0.,-1.));
#115890=DIRECTION('ref_axis',(-1.,0.,1.17174841180864E-16));
#115891=DIRECTION('center_axis',(-0.809645611678678,0.586919060371707,7.8645720234677E-6));
#115892=DIRECTION('ref_axis',(-7.22718435185782E-6,3.42996856068737E-6,
-0.999999999968002));
#115893=DIRECTION('center_axis',(0.865489779781566,-0.500926582476719,7.86457236031111E-6));
#115894=DIRECTION('ref_axis',(0.424811802651068,0.7339720405287,-0.529924500330459));
#115895=DIRECTION('center_axis',(-1.4081690688991E-16,0.,-1.));
#115896=DIRECTION('ref_axis',(-1.,0.,1.13676889660403E-16));
#115897=DIRECTION('center_axis',(-0.80961884266152,0.586955986009136,-9.77058844484673E-6));
#115898=DIRECTION('ref_axis',(0.513380027141697,0.708123635911376,-0.48476990830253));
#115899=DIRECTION('center_axis',(0.865512625110006,-0.500887108717845,-9.77051580085054E-6));
#115900=DIRECTION('ref_axis',(0.438096430108505,0.757022332965597,-0.484756336026162));
#115901=DIRECTION('center_axis',(-1.4081690688991E-16,0.,-1.));
#115902=DIRECTION('ref_axis',(-1.,0.,1.15974593313694E-16));
#115903=DIRECTION('center_axis',(0.807487013627689,-0.5898853469046,1.81624798587448E-5));
#115904=DIRECTION('ref_axis',(0.510387901843966,0.698679346020879,0.501349539837378));
#115905=DIRECTION('center_axis',(-0.867321627584491,0.497748123045615,1.81316450671902E-5));
#115906=DIRECTION('ref_axis',(0.43154623979482,0.751947288230966,0.498340364250227));
#115907=DIRECTION('center_axis',(-1.4081690688991E-16,0.,-1.));
#115908=DIRECTION('ref_axis',(-1.,0.,1.16261524579732E-16));
#115909=DIRECTION('center_axis',(0.807479043031469,-0.589896257593616,1.84940475522698E-5));
#115910=DIRECTION('ref_axis',(0.511436901808568,0.700064389992322,-0.498339387699921));
#115911=DIRECTION('center_axis',(-0.867328352820218,0.497736404184951,1.85257186195537E-5));
#115912=DIRECTION('ref_axis',(0.430656099410934,0.750456526858012,-0.501348506865604));
#115913=DIRECTION('center_axis',(-1.4081690688991E-16,0.,-1.));
#115914=DIRECTION('ref_axis',(-1.,0.,1.40816906889911E-16));
#115915=DIRECTION('center_axis',(-1.4081690688991E-16,0.,-1.));
#115916=DIRECTION('ref_axis',(-1.,0.,1.4081690688991E-16));
#115917=DIRECTION('',(-0.500000000000004,-0.866025403784436,7.04084534449558E-17));
#115918=DIRECTION('center_axis',(-1.4081690688991E-16,0.,-1.));
#115919=DIRECTION('ref_axis',(-1.,0.,1.4081690688991E-16));
#115920=DIRECTION('center_axis',(-1.4081690688991E-16,0.,-1.));
#115921=DIRECTION('ref_axis',(-1.,0.,1.4081690688991E-16));
#115922=DIRECTION('center_axis',(-1.4081690688991E-16,0.,-1.));
#115923=DIRECTION('ref_axis',(-1.,0.,1.4081690688991E-16));
#115924=DIRECTION('',(0.406736643075804,0.913545457642599,-5.72753959967203E-17));
#115925=DIRECTION('center_axis',(1.4081690688991E-16,0.,1.));
#115926=DIRECTION('ref_axis',(1.,0.,-1.4081690688991E-16));
#115927=DIRECTION('',(-0.250006733496389,-0.433014808647754,0.866022406579769));
#115928=DIRECTION('center_axis',(1.4081690688991E-16,0.,1.));
#115929=DIRECTION('ref_axis',(-1.,0.,1.40816906889911E-16));
#115930=DIRECTION('',(0.203366068089046,0.45677941465413,-0.866022406579779));
#115931=DIRECTION('center_axis',(-1.4081690688991E-16,0.,-1.));
#115932=DIRECTION('ref_axis',(-1.,0.,1.40816906889911E-16));
#115933=DIRECTION('center_axis',(-1.4081690688991E-16,0.,-1.));
#115934=DIRECTION('ref_axis',(-1.,0.,1.4081690688991E-16));
#115935=DIRECTION('',(-0.500000000000004,-0.866025403784436,7.04084534449558E-17));
#115936=DIRECTION('center_axis',(1.4081690688991E-16,0.,1.));
#115937=DIRECTION('ref_axis',(-1.,0.,1.4081690688991E-16));
#115938=DIRECTION('',(0.406736643075804,0.913545457642599,-5.72753959967203E-17));
#115939=DIRECTION('center_axis',(-1.4081690688991E-16,0.,-1.));
#115940=DIRECTION('ref_axis',(-1.,0.,1.4081690688991E-16));
#115941=DIRECTION('center_axis',(-1.4081690688991E-16,0.,-1.));
#115942=DIRECTION('ref_axis',(1.,-4.44089209850063E-15,-1.4081690688991E-16));
#115943=DIRECTION('',(-0.249998488182553,-0.433019338752928,-0.866022521746643));
#115944=DIRECTION('center_axis',(-1.4081690688991E-16,0.,-1.));
#115945=DIRECTION('ref_axis',(-1.,0.,1.4081690688991E-16));
#115946=DIRECTION('center_axis',(-1.4081690688991E-16,0.,-1.));
#115947=DIRECTION('ref_axis',(-1.,0.,1.4081690688991E-16));
#115948=DIRECTION('center_axis',(-1.4081690688991E-16,0.,-1.));
#115949=DIRECTION('ref_axis',(-1.,0.,1.4081690688991E-16));
#115950=DIRECTION('',(0.203374579494966,0.456775406784138,0.866022521746653));
#115951=DIRECTION('center_axis',(-1.4081690688991E-16,0.,-1.));
#115952=DIRECTION('ref_axis',(-1.,0.,1.40816906889911E-16));
#115953=DIRECTION('',(-0.500000000000004,-0.866025403784436,7.04084534449558E-17));
#115954=DIRECTION('center_axis',(1.4081690688991E-16,0.,1.));
#115955=DIRECTION('ref_axis',(-1.,0.,1.4081690688991E-16));
#115956=DIRECTION('',(0.406736643075804,0.913545457642599,-5.72753959967203E-17));
#115957=DIRECTION('center_axis',(-1.4081690688991E-16,0.,-1.));
#115958=DIRECTION('ref_axis',(-1.,0.,1.17174841180864E-16));
#115959=DIRECTION('center_axis',(-0.866560035746417,0.499072844768494,7.864571930576E-6));
#115960=DIRECTION('ref_axis',(-7.54612234082935E-6,2.65573232063934E-6,
-0.999999999968002));
#115961=DIRECTION('center_axis',(0.913109622086463,-0.407714137590624,7.86457226365977E-6));
#115962=DIRECTION('ref_axis',(0.345763669669371,0.774356189803027,-0.52992450033048));
#115963=DIRECTION('center_axis',(-1.4081690688991E-16,0.,-1.));
#115964=DIRECTION('ref_axis',(-1.,0.,1.13676889660403E-16));
#115965=DIRECTION('center_axis',(-0.866537273152129,0.499112366248933,-9.77058580781023E-6));
#115966=DIRECTION('ref_axis',(0.43654860217199,0.757907285851209,-0.484769908302212));
#115967=DIRECTION('center_axis',(0.913128216134706,-0.407672492085481,-9.77051458842593E-6));
#115968=DIRECTION('ref_axis',(0.35656611090134,0.798668832019239,-0.484756336026378));
#115969=DIRECTION('center_axis',(-1.4081690688991E-16,0.,-1.));
#115970=DIRECTION('ref_axis',(-1.,0.,1.15974593313694E-16));
#115971=DIRECTION('center_axis',(0.864723324094319,-0.502248516610449,1.81624797599045E-5));
#115972=DIRECTION('ref_axis',(0.434560065156467,0.748201970505921,0.501349539844472));
#115973=DIRECTION('center_axis',(-0.914599195355502,0.404361609857206,1.81316449875146E-5));
#115974=DIRECTION('ref_axis',(0.350582289842569,0.792936907582701,0.498340364251104));
#115975=DIRECTION('center_axis',(-1.4081690688991E-16,0.,-1.));
#115976=DIRECTION('ref_axis',(-1.,0.,1.16261524579732E-16));
#115977=DIRECTION('center_axis',(0.864716537645395,-0.502260200673446,1.84940682125922E-5));
#115978=DIRECTION('ref_axis',(0.435458542073553,0.749689077419333,-0.498339387700114));
#115979=DIRECTION('center_axis',(-0.914604658797229,0.404349252210514,1.85257100784132E-5));
#115980=DIRECTION('ref_axis',(0.349852852737583,0.791361267753224,-0.501348506860632));
#115981=DIRECTION('center_axis',(-1.4081690688991E-16,0.,-1.));
#115982=DIRECTION('ref_axis',(-1.,0.,1.40816906889911E-16));
#115983=DIRECTION('center_axis',(-1.4081690688991E-16,0.,-1.));
#115984=DIRECTION('ref_axis',(-1.,0.,1.4081690688991E-16));
#115985=DIRECTION('',(-0.406736643075804,-0.913545457642599,5.72753959967203E-17));
#115986=DIRECTION('center_axis',(-1.4081690688991E-16,0.,-1.));
#115987=DIRECTION('ref_axis',(-1.,0.,1.4081690688991E-16));
#115988=DIRECTION('center_axis',(-1.4081690688991E-16,0.,-1.));
#115989=DIRECTION('ref_axis',(-1.,0.,1.4081690688991E-16));
#115990=DIRECTION('center_axis',(-1.4081690688991E-16,0.,-1.));
#115991=DIRECTION('ref_axis',(-1.,0.,1.4081690688991E-16));
#115992=DIRECTION('',(0.309016994374951,0.951056516295152,-4.35148173242975E-17));
#115993=DIRECTION('center_axis',(1.4081690688991E-16,0.,1.));
#115994=DIRECTION('ref_axis',(1.,0.,-1.4081690688991E-16));
#115995=DIRECTION('',(-0.203374797931583,-0.456775527877804,0.866022406579785));
#115996=DIRECTION('center_axis',(1.4081690688991E-16,0.,1.));
#115997=DIRECTION('ref_axis',(-1.,0.,1.40816906889911E-16));
#115998=DIRECTION('',(0.154505557223423,0.475534671805167,-0.866022406579779));
#115999=DIRECTION('center_axis',(-1.4081690688991E-16,0.,-1.));
#116000=DIRECTION('ref_axis',(-1.,0.,1.40816906889911E-16));
#116001=DIRECTION('center_axis',(-1.4081690688991E-16,0.,-1.));
#116002=DIRECTION('ref_axis',(-1.,0.,1.4081690688991E-16));
#116003=DIRECTION('',(-0.406736643075804,-0.913545457642599,5.72753959967203E-17));
#116004=DIRECTION('center_axis',(1.4081690688991E-16,0.,1.));
#116005=DIRECTION('ref_axis',(-1.,0.,1.4081690688991E-16));
#116006=DIRECTION('',(0.309016994374951,0.951056516295152,-4.35148173242975E-17));
#116007=DIRECTION('center_axis',(-1.4081690688991E-16,0.,-1.));
#116008=DIRECTION('ref_axis',(-1.,0.,1.4081690688991E-16));
#116009=DIRECTION('center_axis',(-1.4081690688991E-16,0.,-1.));
#116010=DIRECTION('ref_axis',(1.,0.,-1.4081690688991E-16));
#116011=DIRECTION('',(-0.203366124261498,-0.456779171296627,-0.866022521746648));
#116012=DIRECTION('center_axis',(-1.4081690688991E-16,0.,-1.));
#116013=DIRECTION('ref_axis',(-1.,0.,1.4081690688991E-16));
#116014=DIRECTION('center_axis',(-1.4081690688991E-16,0.,-1.));
#116015=DIRECTION('ref_axis',(-1.,0.,1.4081690688991E-16));
#116016=DIRECTION('center_axis',(-1.4081690688991E-16,0.,-1.));
#116017=DIRECTION('ref_axis',(-1.,0.,1.4081690688991E-16));
#116018=DIRECTION('',(0.15451444093947,0.475531575574902,0.866022521746643));
#116019=DIRECTION('center_axis',(-1.4081690688991E-16,0.,-1.));
#116020=DIRECTION('ref_axis',(-1.,0.,1.40816906889911E-16));
#116021=DIRECTION('',(-0.406736643075804,-0.913545457642599,5.72753959967203E-17));
#116022=DIRECTION('center_axis',(1.4081690688991E-16,0.,1.));
#116023=DIRECTION('ref_axis',(-1.,0.,1.4081690688991E-16));
#116024=DIRECTION('',(0.309016994374951,0.951056516295152,-4.35148173242975E-17));
#116025=DIRECTION('center_axis',(-1.4081690688991E-16,0.,-1.));
#116026=DIRECTION('ref_axis',(-1.,0.,1.17174841180864E-16));
#116027=DIRECTION('center_axis',(-0.913980246723224,0.405758682640191,7.86457205741761E-6));
#116028=DIRECTION('ref_axis',(-7.78238362395477E-6,1.85239942789989E-6,
-0.999999999968002));
#116029=DIRECTION('center_axis',(0.950725244291261,-0.310034691293524,7.86457240211258E-6));
#116030=DIRECTION('ref_axis',(0.262927277567292,0.806256330617353,-0.529924500330466));
#116031=DIRECTION('center_axis',(-1.4081690688991E-16,0.,-1.));
#116032=DIRECTION('ref_axis',(-1.,0.,1.13676889660403E-16));
#116033=DIRECTION('center_axis',(-0.913961739944989,0.405800366955557,-9.77058836349E-6));
#116034=DIRECTION('ref_axis',(0.354934259362683,0.79938714496408,-0.484769908303766));
#116035=DIRECTION('center_axis',(0.950739383338138,-0.309991330321275,-9.77051800065362E-6));
#116036=DIRECTION('ref_axis',(0.271129178766871,0.831564948216897,-0.484756336026907));
#116037=DIRECTION('center_axis',(-1.4081690688991E-16,0.,-1.));
#116038=DIRECTION('ref_axis',(-1.,0.,1.15974593313694E-16));
#116039=DIRECTION('center_axis',(0.912485544867189,-0.40910894646604,1.81624796870615E-5));
#116040=DIRECTION('ref_axis',(0.353971097459556,0.789527137633167,0.501349539846259));
#116041=DIRECTION('center_axis',(-0.951856222950115,0.306544826252842,1.81316453251061E-5));
#116042=DIRECTION('ref_axis',(0.265777286959374,0.825238944243956,0.498340364248808));
#116043=DIRECTION('center_axis',(-1.4081690688991E-16,0.,-1.));
#116044=DIRECTION('ref_axis',(-1.,0.,1.16261524579732E-16));
#116045=DIRECTION('center_axis',(0.912480016913587,-0.409121275896707,1.84940738513807E-5));
#116046=DIRECTION('ref_axis',(0.354709207426179,0.791100014431713,-0.498339387700025));
#116047=DIRECTION('center_axis',(-0.951860364736054,0.306531965219525,1.85257135621031E-5));
#116048=DIRECTION('ref_axis',(0.265216544996839,0.823595688993674,-0.501348506860223));
#116049=DIRECTION('center_axis',(-1.4081690688991E-16,0.,-1.));
#116050=DIRECTION('ref_axis',(-1.,0.,1.40816906889911E-16));
#116051=DIRECTION('center_axis',(-1.4081690688991E-16,0.,-1.));
#116052=DIRECTION('ref_axis',(-1.,0.,1.4081690688991E-16));
#116053=DIRECTION('',(-0.309016994374951,-0.951056516295152,4.35148173242975E-17));
#116054=DIRECTION('center_axis',(-1.4081690688991E-16,0.,-1.));
#116055=DIRECTION('ref_axis',(-1.,0.,1.4081690688991E-16));
#116056=DIRECTION('center_axis',(-1.4081690688991E-16,0.,-1.));
#116057=DIRECTION('ref_axis',(-1.,0.,1.4081690688991E-16));
#116058=DIRECTION('center_axis',(-1.4081690688991E-16,0.,-1.));
#116059=DIRECTION('ref_axis',(-1.,0.,1.4081690688991E-16));
#116060=DIRECTION('',(0.207911690817763,0.978147600733805,-2.92774812072088E-17));
#116061=DIRECTION('center_axis',(1.4081690688991E-16,0.,1.));
#116062=DIRECTION('ref_axis',(1.,0.,-1.4081690688991E-16));
#116063=DIRECTION('',(-0.154514645521709,-0.475531718838051,0.866022406579778));
#116064=DIRECTION('center_axis',(1.4081690688991E-16,0.,1.));
#116065=DIRECTION('ref_axis',(-1.,0.,1.40816906889911E-16));
#116066=DIRECTION('',(0.103952251140481,0.489079871579878,-0.866022406579781));
#116067=DIRECTION('center_axis',(-1.4081690688991E-16,0.,-1.));
#116068=DIRECTION('ref_axis',(-1.,0.,1.40816906889911E-16));
#116069=DIRECTION('center_axis',(-1.4081690688991E-16,0.,-1.));
#116070=DIRECTION('ref_axis',(-1.,0.,1.4081690688991E-16));
#116071=DIRECTION('',(-0.309016994374951,-0.951056516295152,4.35148173242975E-17));
#116072=DIRECTION('center_axis',(1.4081690688991E-16,0.,1.));
#116073=DIRECTION('ref_axis',(-1.,0.,1.4081690688991E-16));
#116074=DIRECTION('',(0.207911690817763,0.978147600733805,-2.92774812072088E-17));
#116075=DIRECTION('center_axis',(-1.4081690688991E-16,0.,-1.));
#116076=DIRECTION('ref_axis',(-1.,0.,1.4081690688991E-16));
#116077=DIRECTION('center_axis',(-1.4081690688991E-16,0.,-1.));
#116078=DIRECTION('ref_axis',(1.,0.,-1.4081690688991E-16));
#116079=DIRECTION('',(-0.154505638525953,-0.47553443565238,-0.866022521746669));
#116080=DIRECTION('center_axis',(-1.4081690688991E-16,0.,-1.));
#116081=DIRECTION('ref_axis',(-1.,0.,1.4081690688991E-16));
#116082=DIRECTION('center_axis',(-1.4081690688991E-16,0.,-1.));
#116083=DIRECTION('ref_axis',(-1.,0.,1.4081690688991E-16));
#116084=DIRECTION('center_axis',(-1.4081690688991E-16,0.,-1.));
#116085=DIRECTION('ref_axis',(-1.,0.,1.4081690688991E-16));
#116086=DIRECTION('',(0.103961409834823,0.489077720912261,0.866022521746648));
#116087=DIRECTION('center_axis',(-1.4081690688991E-16,0.,-1.));
#116088=DIRECTION('ref_axis',(-1.,0.,1.40816906889911E-16));
#116089=DIRECTION('',(-0.309016994374951,-0.951056516295152,4.35148173242975E-17));
#116090=DIRECTION('center_axis',(1.4081690688991E-16,0.,1.));
#116091=DIRECTION('ref_axis',(-1.,0.,1.4081690688991E-16));
#116092=DIRECTION('',(0.207911690817763,0.978147600733805,-2.92774812072088E-17));
#116093=DIRECTION('center_axis',(-1.4081690688991E-16,0.,-1.));
#116094=DIRECTION('ref_axis',(-1.,0.,1.17174841180864E-16));
#116095=DIRECTION('center_axis',(-0.951386698854225,0.307998943474501,7.864572011635E-6));
#116096=DIRECTION('ref_axis',(-7.93337934383608E-6,1.02877115701162E-6,
-0.999999999968002));
#116097=DIRECTION('center_axis',(0.977924521767603,-0.208958440039532,7.86457222572879E-6));
#116098=DIRECTION('ref_axis',(0.177210199190827,0.829322958353529,-0.529924500330471));
#116099=DIRECTION('center_axis',(-1.4081690688991E-16,0.,-1.));
#116100=DIRECTION('ref_axis',(-1.,0.,1.13676889660403E-16));
#116101=DIRECTION('center_axis',(-0.951372650655541,0.308042333923741,-9.77058865395253E-6));
#116102=DIRECTION('ref_axis',(0.269431182533353,0.832108751234505,-0.48476990830458));
#116103=DIRECTION('center_axis',(0.977934050903516,-0.20891383867034,-9.77051776669988E-6));
#116104=DIRECTION('ref_axis',(0.182721698612496,0.855350264825962,-0.484756336026998));
#116105=DIRECTION('center_axis',(-1.4081690688991E-16,0.,-1.));
#116106=DIRECTION('ref_axis',(-1.,0.,1.15974593313694E-16));
#116107=DIRECTION('center_axis',(0.950250383060633,-0.311487093092547,1.8162479704961E-5));
#116108=DIRECTION('ref_axis',(0.269503948348138,0.822202080228475,0.501349539834967));
#116109=DIRECTION('center_axis',(-0.978684514577286,0.205369473383621,1.81316451935691E-5));
#116110=DIRECTION('ref_axis',(0.178060372501543,0.848499490335405,0.498340364254362));
#116111=DIRECTION('center_axis',(-1.4081690688991E-16,0.,-1.));
#116112=DIRECTION('ref_axis',(-1.,0.,1.16261524579732E-16));
#116113=DIRECTION('center_axis',(0.950246174164968,-0.311499932813493,1.84940671105159E-5));
#116114=DIRECTION('ref_axis',(0.270073604475392,0.823843494140517,-0.498339387694785));
#116115=DIRECTION('center_axis',(-0.978687289329486,0.205356249872508,1.85257182595835E-5));
#116116=DIRECTION('ref_axis',(0.177674469289135,0.846806623517853,-0.50134850685837));
#116117=DIRECTION('center_axis',(-1.4081690688991E-16,0.,-1.));
#116118=DIRECTION('ref_axis',(-1.,0.,1.40816906889911E-16));
#116119=DIRECTION('center_axis',(-1.4081690688991E-16,0.,-1.));
#116120=DIRECTION('ref_axis',(-1.,0.,1.4081690688991E-16));
#116121=DIRECTION('',(-0.207911690817763,-0.978147600733805,2.92774812072088E-17));
#116122=DIRECTION('center_axis',(-1.4081690688991E-16,0.,-1.));
#116123=DIRECTION('ref_axis',(-1.,0.,1.4081690688991E-16));
#116124=DIRECTION('center_axis',(-1.4081690688991E-16,0.,-1.));
#116125=DIRECTION('ref_axis',(-1.,0.,1.4081690688991E-16));
#116126=DIRECTION('center_axis',(-1.4081690688991E-16,0.,-1.));
#116127=DIRECTION('ref_axis',(-1.,0.,1.4081690688991E-16));
#116128=DIRECTION('',(0.104528463267657,0.994521895368273,-1.47193748793071E-17));
#116129=DIRECTION('center_axis',(1.4081690688991E-16,0.,1.));
#116130=DIRECTION('ref_axis',(1.,0.,-1.4081690688991E-16));
#116131=DIRECTION('',(-0.103961598321241,-0.489077884775271,0.866022406579783));
#116132=DIRECTION('center_axis',(1.4081690688991E-16,0.,1.));
#116133=DIRECTION('ref_axis',(-1.,0.,1.40816906889911E-16));
#116134=DIRECTION('',(0.0522600224406464,0.497266609935041,-0.866022406579769));
#116135=DIRECTION('center_axis',(-1.4081690688991E-16,0.,-1.));
#116136=DIRECTION('ref_axis',(-1.,0.,1.40816906889911E-16));
#116137=DIRECTION('center_axis',(-1.4081690688991E-16,0.,-1.));
#116138=DIRECTION('ref_axis',(-1.,0.,1.4081690688991E-16));
#116139=DIRECTION('',(-0.207911690817763,-0.978147600733805,2.92774812072088E-17));
#116140=DIRECTION('center_axis',(1.4081690688991E-16,0.,1.));
#116141=DIRECTION('ref_axis',(-1.,0.,1.4081690688991E-16));
#116142=DIRECTION('',(0.104528463267657,0.994521895368273,-1.47193748793071E-17));
#116143=DIRECTION('center_axis',(-1.4081690688991E-16,0.,-1.));
#116144=DIRECTION('ref_axis',(-1.,0.,1.4081690688991E-16));
#116145=DIRECTION('center_axis',(-1.4081690688991E-16,0.,-1.));
#116146=DIRECTION('ref_axis',(1.,0.,-1.4081690688991E-16));
#116147=DIRECTION('',(-0.103952356682307,-0.489079645219225,-0.866022521746653));
#116148=DIRECTION('center_axis',(-1.4081690688991E-16,0.,-1.));
#116149=DIRECTION('ref_axis',(-1.,0.,1.4081690688991E-16));
#116150=DIRECTION('center_axis',(-1.4081690688991E-16,0.,-1.));
#116151=DIRECTION('ref_axis',(-1.,0.,1.4081690688991E-16));
#116152=DIRECTION('center_axis',(-1.4081690688991E-16,0.,-1.));
#116153=DIRECTION('ref_axis',(-1.,0.,1.4081690688991E-16));
#116154=DIRECTION('',(0.0522693557686676,0.497265428393217,0.866022521746657));
#116155=DIRECTION('center_axis',(-1.4081690688991E-16,0.,-1.));
#116156=DIRECTION('ref_axis',(-1.,0.,1.40816906889911E-16));
#116157=DIRECTION('',(-0.207911690817763,-0.978147600733805,2.92774812072088E-17));
#116158=DIRECTION('center_axis',(1.4081690688991E-16,0.,1.));
#116159=DIRECTION('ref_axis',(-1.,0.,1.4081690688991E-16));
#116160=DIRECTION('',(0.104528463267657,0.994521895368273,-1.47193748793071E-17));
#116161=DIRECTION('center_axis',(-1.4081690688991E-16,0.,-1.));
#116162=DIRECTION('ref_axis',(-1.,0.,1.17174841180864E-16));
#116163=DIRECTION('center_axis',(-0.978369559222116,0.206864703431182,7.86457201672164E-6));
#116164=DIRECTION('ref_axis',(-7.99745533554544E-6,1.93871482032992E-7,
-0.999999999968002));
#116165=DIRECTION('center_axis',(0.994409453539565,-0.105592796389204,7.86457224839845E-6));
#116166=DIRECTION('ref_axis',(0.0895515687885955,0.843303350210959,-0.529924500330448));
#116167=DIRECTION('center_axis',(-1.4081690688991E-16,0.,-1.));
#116168=DIRECTION('ref_axis',(-1.,0.,1.13676889660403E-16));
#116169=DIRECTION('center_axis',(-0.978360123517642,0.206909324620909,-9.77058627110058E-6));
#116170=DIRECTION('ref_axis',(0.180976161286485,0.855713599897814,-0.484769908302827));
#116171=DIRECTION('center_axis',(0.994414268361317,-0.105547443284825,-9.77051739609162E-6));
#116172=DIRECTION('ref_axis',(0.0923122812911824,0.869764184940213,-0.484756336026775));
#116173=DIRECTION('center_axis',(-1.4081690688991E-16,0.,-1.));
#116174=DIRECTION('ref_axis',(-1.,0.,1.15974593313694E-16));
#116175=DIRECTION('center_axis',(0.977604079204551,-0.210452521944373,1.81624797413809E-5));
#116176=DIRECTION('ref_axis',(0.182084057578138,0.845868804767363,0.501349539839535));
#116177=DIRECTION('center_axis',(-0.994790133859856,0.101944049587673,1.81316451772609E-5));
#116178=DIRECTION('ref_axis',(0.0883925913426408,0.862463698459305,0.49834036424479));
#116179=DIRECTION('center_axis',(-1.4081690688991E-16,0.,-1.));
#116180=DIRECTION('ref_axis',(-1.,0.,1.16261524579732E-16));
#116181=DIRECTION('center_axis',(0.977601235481153,-0.210465731281114,1.84940604206757E-5));
#116182=DIRECTION('ref_axis',(0.182479018596279,0.847560772124483,-0.498339387694661));
#116183=DIRECTION('center_axis',(-0.99479151117877,0.101930608471928,1.85257116294611E-5));
#116184=DIRECTION('ref_axis',(0.0881857549144201,0.860739767464283,-0.50134850686494));
#116185=DIRECTION('center_axis',(-1.4081690688991E-16,0.,-1.));
#116186=DIRECTION('ref_axis',(-1.,0.,1.40816906889911E-16));
#116187=DIRECTION('center_axis',(-1.4081690688991E-16,0.,-1.));
#116188=DIRECTION('ref_axis',(-1.,0.,1.4081690688991E-16));
#116189=DIRECTION('',(-0.104528463267657,-0.994521895368273,1.47193748793071E-17));
#116190=DIRECTION('center_axis',(-1.4081690688991E-16,0.,-1.));
#116191=DIRECTION('ref_axis',(-1.,0.,1.4081690688991E-16));
#116192=DIRECTION('center_axis',(-1.4081690688991E-16,0.,-1.));
#116193=DIRECTION('ref_axis',(-1.,0.,1.4081690688991E-16));
#116194=DIRECTION('center_axis',(-1.4081690688991E-16,0.,-1.));
#116195=DIRECTION('ref_axis',(-1.,0.,1.4081690688991E-16));
#116196=DIRECTION('',(3.49148133884313E-15,1.,-4.91659602599733E-31));
#116197=DIRECTION('center_axis',(1.4081690688991E-16,0.,1.));
#116198=DIRECTION('ref_axis',(1.,0.,-1.4081690688991E-16));
#116199=DIRECTION('',(-0.0522695260941986,-0.497265611060785,0.866022406579779));
#116200=DIRECTION('center_axis',(1.4081690688991E-16,0.,1.));
#116201=DIRECTION('ref_axis',(-1.,0.,1.40816906889911E-16));
#116202=DIRECTION('',(-4.77800116381153E-6,0.500005191252011,-0.866022406579767));
#116203=DIRECTION('center_axis',(-1.4081690688991E-16,0.,-1.));
#116204=DIRECTION('ref_axis',(-1.,0.,1.40816906889911E-16));
#116205=DIRECTION('center_axis',(-1.4081690688991E-16,0.,-1.));
#116206=DIRECTION('ref_axis',(-1.,0.,1.4081690688991E-16));
#116207=DIRECTION('',(-0.104528463267657,-0.994521895368273,1.47193748793071E-17));
#116208=DIRECTION('center_axis',(1.4081690688991E-16,0.,1.));
#116209=DIRECTION('ref_axis',(-1.,0.,1.4081690688991E-16));
#116210=DIRECTION('',(3.49148133884313E-15,1.,-4.91659602599733E-31));
#116211=DIRECTION('center_axis',(-1.4081690688991E-16,0.,-1.));
#116212=DIRECTION('ref_axis',(-1.,0.,1.4081690688991E-16));
#116213=DIRECTION('center_axis',(-1.4081690688991E-16,0.,-1.));
#116214=DIRECTION('ref_axis',(1.,0.,-1.4081690688991E-16));
#116215=DIRECTION('',(-0.0522601510654385,-0.497266395846527,-0.866022521746648));
#116216=DIRECTION('center_axis',(-1.4081690688991E-16,0.,-1.));
#116217=DIRECTION('ref_axis',(-1.,0.,1.4081690688991E-16));
#116218=DIRECTION('center_axis',(-1.4081690688991E-16,0.,-1.));
#116219=DIRECTION('ref_axis',(-1.,0.,1.4081690688991E-16));
#116220=DIRECTION('center_axis',(-1.4081690688991E-16,0.,-1.));
#116221=DIRECTION('ref_axis',(-1.,0.,1.4081690688991E-16));
#116222=DIRECTION('',(4.62770265447403E-6,0.500004991781227,0.866022521746657));
#116223=DIRECTION('center_axis',(-1.4081690688991E-16,0.,-1.));
#116224=DIRECTION('ref_axis',(-1.,0.,1.40816906889911E-16));
#116225=DIRECTION('',(-0.104528463267657,-0.994521895368273,1.47193748793071E-17));
#116226=DIRECTION('center_axis',(1.4081690688991E-16,0.,1.));
#116227=DIRECTION('ref_axis',(-1.,0.,1.4081690688991E-16));
#116228=DIRECTION('',(3.49148133884313E-15,1.,-4.91659602599733E-31));
#116229=DIRECTION('center_axis',(-1.4081690688991E-16,0.,-1.));
#116230=DIRECTION('ref_axis',(-1.,0.,1.17174841180864E-16));
#116231=DIRECTION('center_axis',(-0.994633197962182,0.103464010407828,7.86457203065501E-6));
#116232=DIRECTION('ref_axis',(-7.97390954032785E-6,-6.43152300427559E-7,
-0.999999999968002));
#116233=DIRECTION('center_axis',(0.999999427244995,-0.00107025596491175,
7.86457225179323E-6));
#116234=DIRECTION('ref_axis',(0.000911792658825042,0.848044334090874,-0.529924500330484));
#116235=DIRECTION('center_axis',(-1.4081690688991E-16,0.,-1.));
#116236=DIRECTION('ref_axis',(-1.,0.,1.13676889660403E-16));
#116237=DIRECTION('center_axis',(-0.994628478131894,0.103509373457517,-9.77058669981437E-6));
#116238=DIRECTION('ref_axis',(0.090538327344489,0.869943071289052,-0.48476990830479));
#116239=DIRECTION('center_axis',(0.999999475000345,-0.00102464802303281,
-9.77051625719004E-6));
#116240=DIRECTION('ref_axis',(0.000891471298433248,0.87464878663446,-0.484756336026452));
#116241=DIRECTION('center_axis',(-1.4081690688991E-16,0.,-1.));
#116242=DIRECTION('ref_axis',(-1.,0.,1.15974593313694E-16));
#116243=DIRECTION('center_axis',(0.994246940479906,-0.107112188925774,1.81624797806968E-5));
#116244=DIRECTION('ref_axis',(0.0926692157705482,0.860268013673723,0.501349539840557));
#116245=DIRECTION('center_axis',(-0.999996624262643,-0.00259829454878502,
1.81316452283592E-5));
#116246=DIRECTION('ref_axis',(0.00224363754549732,-0.86697857381378,-0.498340364247558));
#116247=DIRECTION('center_axis',(-1.4081690688991E-16,0.,-1.));
#116248=DIRECTION('ref_axis',(-1.,0.,1.16261524579732E-16));
#116249=DIRECTION('center_axis',(0.994245493086383,-0.107125623150506,1.84940601461275E-5));
#116250=DIRECTION('ref_axis',(0.0928851544031254,0.861991996924917,-0.498339387695677));
#116251=DIRECTION('center_axis',(-0.999996589057285,-0.00261180600212912,
1.85257108423049E-5));
#116252=DIRECTION('ref_axis',(0.0022691410444307,-0.865242466404122,0.501348506859083));
#116253=DIRECTION('center_axis',(-1.4081690688991E-16,0.,-1.));
#116254=DIRECTION('ref_axis',(-1.,0.,1.40816906889911E-16));
#116255=DIRECTION('center_axis',(-1.4081690688991E-16,0.,-1.));
#116256=DIRECTION('ref_axis',(-1.,0.,1.4081690688991E-16));
#116257=DIRECTION('',(-3.49148133884313E-15,-1.,4.91659602599733E-31));
#116258=DIRECTION('center_axis',(-1.4081690688991E-16,0.,-1.));
#116259=DIRECTION('ref_axis',(-1.,0.,1.4081690688991E-16));
#116260=DIRECTION('center_axis',(-1.4081690688991E-16,0.,-1.));
#116261=DIRECTION('ref_axis',(-1.,0.,1.4081690688991E-16));
#116262=DIRECTION('center_axis',(-1.4081690688991E-16,0.,-1.));
#116263=DIRECTION('ref_axis',(-1.,0.,1.4081690688991E-16));
#116264=DIRECTION('',(-0.10452846326765,0.994521895368274,1.47193748793061E-17));
#116265=DIRECTION('center_axis',(1.4081690688991E-16,0.,1.));
#116266=DIRECTION('ref_axis',(1.,0.,-1.4081690688991E-16));
#116267=DIRECTION('',(-4.77800116722343E-6,-0.500005191252011,0.866022406579767));
#116268=DIRECTION('center_axis',(1.4081690688991E-16,0.,1.));
#116269=DIRECTION('ref_axis',(-1.,0.,1.40816906889911E-16));
#116270=DIRECTION('',(-0.0522695260941986,0.497265611060785,-0.866022406579779));
#116271=DIRECTION('center_axis',(-1.4081690688991E-16,0.,-1.));
#116272=DIRECTION('ref_axis',(-1.,0.,1.40816906889911E-16));
#116273=DIRECTION('center_axis',(-1.4081690688991E-16,0.,-1.));
#116274=DIRECTION('ref_axis',(-1.,0.,1.4081690688991E-16));
#116275=DIRECTION('',(-3.49148133884313E-15,-1.,4.91659602599733E-31));
#116276=DIRECTION('center_axis',(1.4081690688991E-16,0.,1.));
#116277=DIRECTION('ref_axis',(-1.,0.,1.4081690688991E-16));
#116278=DIRECTION('',(-0.10452846326765,0.994521895368274,1.47193748793061E-17));
#116279=DIRECTION('center_axis',(-1.4081690688991E-16,0.,-1.));
#116280=DIRECTION('ref_axis',(-1.,0.,1.4081690688991E-16));
#116281=DIRECTION('center_axis',(-1.4081690688991E-16,0.,-1.));
#116282=DIRECTION('ref_axis',(1.,0.,-1.4081690688991E-16));
#116283=DIRECTION('',(4.62770265084889E-6,-0.500004991781227,-0.866022521746657));
#116284=DIRECTION('center_axis',(-1.4081690688991E-16,0.,-1.));
#116285=DIRECTION('ref_axis',(-1.,0.,1.4081690688991E-16));
#116286=DIRECTION('center_axis',(-1.4081690688991E-16,0.,-1.));
#116287=DIRECTION('ref_axis',(-1.,0.,1.4081690688991E-16));
#116288=DIRECTION('center_axis',(-1.4081690688991E-16,0.,-1.));
#116289=DIRECTION('ref_axis',(-1.,0.,1.4081690688991E-16));
#116290=DIRECTION('',(-0.0522601510654331,0.497266395846486,0.866022521746671));
#116291=DIRECTION('center_axis',(-1.4081690688991E-16,0.,-1.));
#116292=DIRECTION('ref_axis',(-1.,0.,1.40816906889911E-16));
#116293=DIRECTION('',(-3.49148133884313E-15,-1.,4.91659602599733E-31));
#116294=DIRECTION('center_axis',(1.4081690688991E-16,0.,1.));
#116295=DIRECTION('ref_axis',(-1.,0.,1.4081690688991E-16));
#116296=DIRECTION('',(-0.10452846326765,0.994521895368274,1.47193748793061E-17));
#116297=DIRECTION('center_axis',(-1.4081690688991E-16,0.,-1.));
#116298=DIRECTION('ref_axis',(-1.,0.,1.17174841180864E-16));
#116299=DIRECTION('center_axis',(-0.999999427244995,-0.0010702559647792,
7.86457202574355E-6));
#116300=DIRECTION('ref_axis',(-7.86299990339083E-6,-1.47312957758963E-6,
-0.999999999968002));
#116301=DIRECTION('center_axis',(0.994633197962196,0.103464010407699,7.86457225586277E-6));
#116302=DIRECTION('ref_axis',(-0.0877379732621213,0.843493966781849,-0.52992450033045));
#116303=DIRECTION('center_axis',(-1.4081690688991E-16,0.,-1.));
#116304=DIRECTION('ref_axis',(-1.,0.,1.13676889660403E-16));
#116305=DIRECTION('center_axis',(-0.999999475000305,-0.00102464806168893,
-9.77058600784865E-6));
#116306=DIRECTION('ref_axis',(0.00089146345812007,-0.874641264345843,0.484769908303318));
#116307=DIRECTION('center_axis',(0.994628478127861,0.103509373496281,-9.77051628788904E-6));
#116308=DIRECTION('ref_axis',(0.0905391058403898,-0.869950553189685,0.484756336027271));
#116309=DIRECTION('center_axis',(-1.4081690688991E-16,0.,-1.));
#116310=DIRECTION('ref_axis',(-1.,0.,1.15974593313694E-16));
#116311=DIRECTION('center_axis',(0.999996624215829,-0.00259831235053714,
1.81624797955926E-5));
#116312=DIRECTION('ref_axis',(0.00223907064273736,0.865241946196868,0.501349539846316));
#116313=DIRECTION('center_axis',(-0.994246942387256,-0.107112171226408,
1.81316452589115E-5));
#116314=DIRECTION('ref_axis',(0.0928552846706877,-0.861994650485332,-0.498340364252582));
#116315=DIRECTION('center_axis',(-1.4081690688991E-16,0.,-1.));
#116316=DIRECTION('ref_axis',(-1.,0.,1.16261524579732E-16));
#116317=DIRECTION('center_axis',(0.999996589010145,-0.00261182427511404,
1.84940600372377E-5));
#116318=DIRECTION('ref_axis',(0.00227362102100041,0.866979057022621,-0.498339387698403));
#116319=DIRECTION('center_axis',(-0.994245495043456,-0.107125604981216,
1.85257132984629E-5));
#116320=DIRECTION('ref_axis',(0.0926991758193393,-0.86026538781347,0.501348506861799));
#116321=DIRECTION('center_axis',(-1.4081690688991E-16,0.,-1.));
#116322=DIRECTION('ref_axis',(-1.,0.,1.40816906889911E-16));
#116323=DIRECTION('center_axis',(-1.4081690688991E-16,0.,-1.));
#116324=DIRECTION('ref_axis',(-1.,0.,1.4081690688991E-16));
#116325=DIRECTION('',(0.10452846326765,-0.994521895368274,-1.47193748793061E-17));
#116326=DIRECTION('center_axis',(-1.4081690688991E-16,0.,-1.));
#116327=DIRECTION('ref_axis',(-1.,0.,1.4081690688991E-16));
#116328=DIRECTION('center_axis',(-1.4081690688991E-16,0.,-1.));
#116329=DIRECTION('ref_axis',(-1.,0.,1.4081690688991E-16));
#116330=DIRECTION('center_axis',(-1.4081690688991E-16,0.,-1.));
#116331=DIRECTION('ref_axis',(-1.,0.,1.4081690688991E-16));
#116332=DIRECTION('',(-0.207911690817756,0.978147600733806,2.92774812072079E-17));
#116333=DIRECTION('center_axis',(1.4081690688991E-16,0.,1.));
#116334=DIRECTION('ref_axis',(1.,0.,-1.4081690688991E-16));
#116335=DIRECTION('',(0.0522600224406464,-0.497266609935041,0.866022406579769));
#116336=DIRECTION('center_axis',(1.4081690688991E-16,0.,1.));
#116337=DIRECTION('ref_axis',(-1.,0.,1.40816906889911E-16));
#116338=DIRECTION('',(-0.103961598321248,0.489077884775271,-0.866022406579783));
#116339=DIRECTION('center_axis',(-1.4081690688991E-16,0.,-1.));
#116340=DIRECTION('ref_axis',(-1.,0.,1.40816906889911E-16));
#116341=DIRECTION('center_axis',(-1.4081690688991E-16,0.,-1.));
#116342=DIRECTION('ref_axis',(-1.,0.,1.4081690688991E-16));
#116343=DIRECTION('',(0.10452846326765,-0.994521895368274,-1.47193748793061E-17));
#116344=DIRECTION('center_axis',(1.4081690688991E-16,0.,1.));
#116345=DIRECTION('ref_axis',(-1.,0.,1.4081690688991E-16));
#116346=DIRECTION('',(-0.207911690817756,0.978147600733806,2.92774812072079E-17));
#116347=DIRECTION('center_axis',(-1.4081690688991E-16,0.,-1.));
#116348=DIRECTION('ref_axis',(-1.,0.,1.4081690688991E-16));
#116349=DIRECTION('center_axis',(-1.4081690688991E-16,0.,-1.));
#116350=DIRECTION('ref_axis',(1.,0.,-1.4081690688991E-16));
#116351=DIRECTION('',(0.0522693557686642,-0.497265428393217,-0.866022521746657));
#116352=DIRECTION('center_axis',(-1.4081690688991E-16,0.,-1.));
#116353=DIRECTION('ref_axis',(-1.,0.,1.4081690688991E-16));
#116354=DIRECTION('center_axis',(-1.4081690688991E-16,0.,-1.));
#116355=DIRECTION('ref_axis',(-1.,0.,1.4081690688991E-16));
#116356=DIRECTION('center_axis',(-1.4081690688991E-16,0.,-1.));
#116357=DIRECTION('ref_axis',(-1.,0.,1.4081690688991E-16));
#116358=DIRECTION('',(-0.103952356682315,0.489079645219204,0.866022521746664));
#116359=DIRECTION('center_axis',(-1.4081690688991E-16,0.,-1.));
#116360=DIRECTION('ref_axis',(-1.,0.,1.40816906889911E-16));
#116361=DIRECTION('',(0.10452846326765,-0.994521895368274,-1.47193748793061E-17));
#116362=DIRECTION('center_axis',(1.4081690688991E-16,0.,1.));
#116363=DIRECTION('ref_axis',(-1.,0.,1.4081690688991E-16));
#116364=DIRECTION('',(-0.207911690817756,0.978147600733806,2.92774812072079E-17));
#116365=DIRECTION('center_axis',(-1.4081690688991E-16,0.,-1.));
#116366=DIRECTION('ref_axis',(-1.,0.,1.17174841180864E-16));
#116367=DIRECTION('center_axis',(-0.99440945353958,-0.105592796389066,7.86457201556077E-6));
#116368=DIRECTION('ref_axis',(-7.66594159182268E-6,-2.28696686047188E-6,
-0.999999999968001));
#116369=DIRECTION('center_axis',(0.978369559222142,0.20686470343106,7.86457223501791E-6));
#116370=DIRECTION('ref_axis',(-0.175426463587678,0.829702103060261,-0.529924500330472));
#116371=DIRECTION('center_axis',(-1.4081690688991E-16,0.,-1.));
#116372=DIRECTION('ref_axis',(-1.,0.,1.13676889660403E-16));
#116373=DIRECTION('center_axis',(-0.994414268357372,-0.105547443321989,
-9.77058482928466E-6));
#116374=DIRECTION('ref_axis',(0.0923114872004343,-0.869756704677923,0.484769908305625));
#116375=DIRECTION('center_axis',(0.978360123509597,0.206909324658953,-9.7705160822993E-6));
#116376=DIRECTION('ref_axis',(0.180977717589175,-0.855720959436191,0.484756336026481));
#116377=DIRECTION('center_axis',(-1.4081690688991E-16,0.,-1.));
#116378=DIRECTION('ref_axis',(-1.,0.,1.15974593313694E-16));
#116379=DIRECTION('center_axis',(0.99479013567409,0.101944031878529,1.81624797615794E-5));
#116380=DIRECTION('ref_axis',(0.0882156062113998,-0.860736106899266,-0.501349539842862));
#116381=DIRECTION('center_axis',(-0.977604082951519,-0.210452504541434,
1.81316453016117E-5));
#116382=DIRECTION('ref_axis',(0.182449589865665,-0.847566533384306,-0.498340364253952));
#116383=DIRECTION('center_axis',(-1.4081690688991E-16,0.,-1.));
#116384=DIRECTION('ref_axis',(-1.,0.,1.16261524579732E-16));
#116385=DIRECTION('center_axis',(0.994791513041743,0.101930590295988,1.8494064067236E-5));
#116386=DIRECTION('ref_axis',(0.0883628226286463,-0.862467313145872,0.498339387698825));
#116387=DIRECTION('center_axis',(-0.977601239327261,-0.210465713413377,
1.85257180944615E-5));
#116388=DIRECTION('ref_axis',(0.182113579025377,-0.845863061613112,0.501348506862303));
#116389=DIRECTION('center_axis',(-1.4081690688991E-16,0.,-1.));
#116390=DIRECTION('ref_axis',(-1.,0.,1.40816906889911E-16));
#116391=DIRECTION('center_axis',(-1.4081690688991E-16,0.,-1.));
#116392=DIRECTION('ref_axis',(-1.,0.,1.4081690688991E-16));
#116393=DIRECTION('',(0.207911690817756,-0.978147600733806,-2.92774812072079E-17));
#116394=DIRECTION('center_axis',(-1.4081690688991E-16,0.,-1.));
#116395=DIRECTION('ref_axis',(-1.,0.,1.4081690688991E-16));
#116396=DIRECTION('center_axis',(-1.4081690688991E-16,0.,-1.));
#116397=DIRECTION('ref_axis',(-1.,0.,1.4081690688991E-16));
#116398=DIRECTION('center_axis',(-1.4081690688991E-16,0.,-1.));
#116399=DIRECTION('ref_axis',(-1.,0.,1.4081690688991E-16));
#116400=DIRECTION('',(-0.309016994374945,0.951056516295154,4.35148173242966E-17));
#116401=DIRECTION('center_axis',(1.4081690688991E-16,0.,1.));
#116402=DIRECTION('ref_axis',(1.,0.,-1.4081690688991E-16));
#116403=DIRECTION('',(0.103952251140481,-0.489079871579878,0.866022406579781));
#116404=DIRECTION('center_axis',(1.4081690688991E-16,0.,1.));
#116405=DIRECTION('ref_axis',(-1.,0.,1.40816906889911E-16));
#116406=DIRECTION('',(-0.154514645521691,0.475531718838031,-0.866022406579792));
#116407=DIRECTION('center_axis',(-1.4081690688991E-16,0.,-1.));
#116408=DIRECTION('ref_axis',(-1.,0.,1.40816906889911E-16));
#116409=DIRECTION('center_axis',(-1.4081690688991E-16,0.,-1.));
#116410=DIRECTION('ref_axis',(-1.,0.,1.4081690688991E-16));
#116411=DIRECTION('',(0.207911690817756,-0.978147600733806,-2.92774812072079E-17));
#116412=DIRECTION('center_axis',(1.4081690688991E-16,0.,1.));
#116413=DIRECTION('ref_axis',(-1.,0.,1.4081690688991E-16));
#116414=DIRECTION('',(-0.309016994374945,0.951056516295154,4.35148173242966E-17));
#116415=DIRECTION('center_axis',(-1.4081690688991E-16,0.,-1.));
#116416=DIRECTION('ref_axis',(-1.,0.,1.4081690688991E-16));
#116417=DIRECTION('center_axis',(-1.4081690688991E-16,0.,-1.));
#116418=DIRECTION('ref_axis',(1.,0.,-1.4081690688991E-16));
#116419=DIRECTION('',(0.103961409834804,-0.489077720912242,-0.866022521746662));
#116420=DIRECTION('center_axis',(-1.4081690688991E-16,0.,-1.));
#116421=DIRECTION('ref_axis',(-1.,0.,1.4081690688991E-16));
#116422=DIRECTION('center_axis',(-1.4081690688991E-16,0.,-1.));
#116423=DIRECTION('ref_axis',(-1.,0.,1.4081690688991E-16));
#116424=DIRECTION('center_axis',(-1.4081690688991E-16,0.,-1.));
#116425=DIRECTION('ref_axis',(-1.,0.,1.4081690688991E-16));
#116426=DIRECTION('',(-0.154505638525963,0.475534435652421,0.866022521746645));
#116427=DIRECTION('center_axis',(-1.4081690688991E-16,0.,-1.));
#116428=DIRECTION('ref_axis',(-1.,0.,1.40816906889911E-16));
#116429=DIRECTION('',(0.207911690817756,-0.978147600733806,-2.92774812072079E-17));
#116430=DIRECTION('center_axis',(1.4081690688991E-16,0.,1.));
#116431=DIRECTION('ref_axis',(-1.,0.,1.4081690688991E-16));
#116432=DIRECTION('',(-0.309016994374945,0.951056516295154,4.35148173242966E-17));
#116433=DIRECTION('center_axis',(-1.4081690688991E-16,0.,-1.));
#116434=DIRECTION('ref_axis',(-1.,0.,1.17174841180864E-16));
#116435=DIRECTION('center_axis',(-0.977924521767625,-0.208958440039425,
7.86457203496813E-6));
#116436=DIRECTION('ref_axis',(-7.38489364321875E-6,-3.07574773432254E-6,
-0.999999999968002));
#116437=DIRECTION('center_axis',(0.95138669885428,0.307998943474332,7.86457235843123E-6));
#116438=DIRECTION('ref_axis',(-0.261192944867685,0.806819849471268,-0.529924500330478));
#116439=DIRECTION('center_axis',(-1.4081690688991E-16,0.,-1.));
#116440=DIRECTION('ref_axis',(-1.,0.,1.13676889660403E-16));
#116441=DIRECTION('center_axis',(-0.977934050895729,-0.208913838706787,
-9.77058511661614E-6));
#116442=DIRECTION('ref_axis',(0.182720126971744,-0.855342908547616,0.484769908303655));
#116443=DIRECTION('center_axis',(0.951372650643379,0.308042333961304,-9.77051741258055E-6));
#116444=DIRECTION('ref_axis',(0.269433499591897,-0.832115907779229,0.484756336027093));
#116445=DIRECTION('center_axis',(-1.4081690688991E-16,0.,-1.));
#116446=DIRECTION('ref_axis',(-1.,0.,1.15974593313694E-16));
#116447=DIRECTION('center_axis',(0.9786845182327,0.205369455961084,1.8162479768661E-5));
#116448=DIRECTION('ref_axis',(0.177703774422995,-0.846799862689322,-0.501349539847368));
#116449=DIRECTION('center_axis',(-0.95025038860616,-0.311487076176663,1.81316453262635E-5));
#116450=DIRECTION('ref_axis',(0.270044939174518,-0.823852299980834,-0.498340364251704));
#116451=DIRECTION('center_axis',(-1.4081690688991E-16,0.,-1.));
#116452=DIRECTION('ref_axis',(-1.,0.,1.16261524579732E-16));
#116453=DIRECTION('center_axis',(0.978687293082516,0.205356231989163,1.84940676879274E-5));
#116454=DIRECTION('ref_axis',(0.178031144703038,-0.848506196906464,0.498339387693823));
#116455=DIRECTION('center_axis',(-0.950246179854085,-0.311499915456677,
1.85257046986954E-5));
#116456=DIRECTION('ref_axis',(0.269532707750914,-0.822193282704966,0.501348506856551));
#116457=DIRECTION('center_axis',(-1.4081690688991E-16,0.,-1.));
#116458=DIRECTION('ref_axis',(-1.,0.,1.40816906889911E-16));
#116459=DIRECTION('center_axis',(-1.4081690688991E-16,0.,-1.));
#116460=DIRECTION('ref_axis',(-1.,0.,1.4081690688991E-16));
#116461=DIRECTION('',(0.309016994374945,-0.951056516295154,-4.35148173242966E-17));
#116462=DIRECTION('center_axis',(-1.4081690688991E-16,0.,-1.));
#116463=DIRECTION('ref_axis',(-1.,0.,1.4081690688991E-16));
#116464=DIRECTION('center_axis',(-1.4081690688991E-16,0.,-1.));
#116465=DIRECTION('ref_axis',(-1.,0.,1.4081690688991E-16));
#116466=DIRECTION('center_axis',(-1.4081690688991E-16,0.,-1.));
#116467=DIRECTION('ref_axis',(-1.,0.,1.4081690688991E-16));
#116468=DIRECTION('',(-0.406736643075798,0.913545457642602,5.72753959967194E-17));
#116469=DIRECTION('center_axis',(1.4081690688991E-16,0.,1.));
#116470=DIRECTION('ref_axis',(1.,0.,-1.4081690688991E-16));
#116471=DIRECTION('',(0.154505557223429,-0.475534671805166,0.866022406579778));
#116472=DIRECTION('center_axis',(1.4081690688991E-16,0.,1.));
#116473=DIRECTION('ref_axis',(-1.,0.,1.40816906889911E-16));
#116474=DIRECTION('',(-0.20337479793158,0.456775527877825,-0.866022406579774));
#116475=DIRECTION('center_axis',(-1.4081690688991E-16,0.,-1.));
#116476=DIRECTION('ref_axis',(-1.,0.,1.40816906889911E-16));
#116477=DIRECTION('center_axis',(-1.4081690688991E-16,0.,-1.));
#116478=DIRECTION('ref_axis',(-1.,0.,1.4081690688991E-16));
#116479=DIRECTION('',(0.309016994374945,-0.951056516295154,-4.35148173242966E-17));
#116480=DIRECTION('center_axis',(1.4081690688991E-16,0.,1.));
#116481=DIRECTION('ref_axis',(-1.,0.,1.4081690688991E-16));
#116482=DIRECTION('',(-0.406736643075798,0.913545457642602,5.72753959967194E-17));
#116483=DIRECTION('center_axis',(-1.4081690688991E-16,0.,-1.));
#116484=DIRECTION('ref_axis',(-1.,0.,1.4081690688991E-16));
#116485=DIRECTION('center_axis',(-1.4081690688991E-16,0.,-1.));
#116486=DIRECTION('ref_axis',(1.,0.,-1.4081690688991E-16));
#116487=DIRECTION('',(0.154514440939481,-0.475531575574859,-0.866022521746664));
#116488=DIRECTION('center_axis',(-1.4081690688991E-16,0.,-1.));
#116489=DIRECTION('ref_axis',(-1.,0.,1.4081690688991E-16));
#116490=DIRECTION('center_axis',(-1.4081690688991E-16,0.,-1.));
#116491=DIRECTION('ref_axis',(-1.,0.,1.4081690688991E-16));
#116492=DIRECTION('center_axis',(-1.4081690688991E-16,0.,-1.));
#116493=DIRECTION('ref_axis',(-1.,0.,1.4081690688991E-16));
#116494=DIRECTION('',(-0.203366124261491,0.456779171296611,0.866022521746658));
#116495=DIRECTION('center_axis',(-1.4081690688991E-16,0.,-1.));
#116496=DIRECTION('ref_axis',(-1.,0.,1.40816906889911E-16));
#116497=DIRECTION('',(0.309016994374945,-0.951056516295154,-4.35148173242966E-17));
#116498=DIRECTION('center_axis',(1.4081690688991E-16,0.,1.));
#116499=DIRECTION('ref_axis',(-1.,0.,1.4081690688991E-16));
#116500=DIRECTION('',(-0.406736643075798,0.913545457642602,5.72753959967194E-17));
#116501=DIRECTION('center_axis',(-1.4081690688991E-16,0.,-1.));
#116502=DIRECTION('ref_axis',(-1.,0.,1.17174841180864E-16));
#116503=DIRECTION('center_axis',(-0.950725244291327,-0.310034691293322,
7.86457203087576E-6));
#116504=DIRECTION('ref_axis',(-7.02293522902363E-6,-3.83083008160136E-6,
-0.999999999968002));
#116505=DIRECTION('center_axis',(0.913980246723271,0.405758682640085,7.86457225348564E-6));
#116506=DIRECTION('ref_axis',(-0.344097741585782,0.775097908773498,-0.529924500330485));
#116507=DIRECTION('center_axis',(-1.4081690688991E-16,0.,-1.));
#116508=DIRECTION('ref_axis',(-1.,0.,1.13676889660403E-16));
#116509=DIRECTION('center_axis',(-0.950739383327519,-0.309991330353843,
-9.77057985364929E-6));
#116510=DIRECTION('ref_axis',(0.271126846795285,-0.83155779651819,0.484769908303578));
#116511=DIRECTION('center_axis',(0.913961739929036,0.405800366991488,-9.77051738652309E-6));
#116512=DIRECTION('ref_axis',(0.354937311790829,-0.799394020106138,0.484756336025892));
#116513=DIRECTION('center_axis',(-1.4081690688991E-16,0.,-1.));
#116514=DIRECTION('ref_axis',(-1.,0.,1.15974593313694E-16));
#116515=DIRECTION('center_axis',(0.951856228406623,0.306544809307943,1.81624797519335E-5));
#116516=DIRECTION('ref_axis',(0.265244982896516,-0.823585901985291,-0.501349539841518));
#116517=DIRECTION('center_axis',(-0.912485552150575,-0.409108930222384,
1.81316452567651E-5));
#116518=DIRECTION('ref_axis',(0.354681619619182,-0.791111768375823,-0.498340364250771));
#116519=DIRECTION('center_axis',(-1.4081690688991E-16,0.,-1.));
#116520=DIRECTION('ref_axis',(-1.,0.,1.16261524579732E-16));
#116521=DIRECTION('center_axis',(0.951860370338612,0.306531947824057,1.84940585634574E-5));
#116522=DIRECTION('ref_axis',(0.265748920299228,-0.825248669206012,0.498339387700291));
#116523=DIRECTION('center_axis',(-0.912480024382915,-0.409121259236127,
1.85256990113859E-5));
#116524=DIRECTION('ref_axis',(0.353998779725528,-0.789515382131506,0.501348506859828));
#116525=DIRECTION('center_axis',(-1.4081690688991E-16,0.,-1.));
#116526=DIRECTION('ref_axis',(-1.,0.,1.40816906889911E-16));
#116527=DIRECTION('center_axis',(-1.4081690688991E-16,0.,-1.));
#116528=DIRECTION('ref_axis',(-1.,0.,1.4081690688991E-16));
#116529=DIRECTION('',(0.406736643075798,-0.913545457642602,-5.72753959967194E-17));
#116530=DIRECTION('center_axis',(-1.4081690688991E-16,0.,-1.));
#116531=DIRECTION('ref_axis',(-1.,0.,1.4081690688991E-16));
#116532=DIRECTION('center_axis',(-1.4081690688991E-16,0.,-1.));
#116533=DIRECTION('ref_axis',(-1.,0.,1.4081690688991E-16));
#116534=DIRECTION('center_axis',(-1.4081690688991E-16,0.,-1.));
#116535=DIRECTION('ref_axis',(-1.,0.,1.4081690688991E-16));
#116536=DIRECTION('',(-0.499999999999998,0.86602540378444,7.04084534449549E-17));
#116537=DIRECTION('center_axis',(1.4081690688991E-16,0.,1.));
#116538=DIRECTION('ref_axis',(1.,0.,-1.4081690688991E-16));
#116539=DIRECTION('',(0.203366068089046,-0.45677941465413,0.866022406579779));
#116540=DIRECTION('center_axis',(1.4081690688991E-16,0.,1.));
#116541=DIRECTION('ref_axis',(-1.,5.32907051820075E-15,1.40816906889911E-16));
#116542=DIRECTION('',(-0.250006733496382,0.433014808647711,-0.866022406579792));
#116543=DIRECTION('center_axis',(-1.4081690688991E-16,0.,-1.));
#116544=DIRECTION('ref_axis',(-1.,0.,1.40816906889911E-16));
#116545=DIRECTION('center_axis',(-1.4081690688991E-16,0.,-1.));
#116546=DIRECTION('ref_axis',(-1.,0.,1.4081690688991E-16));
#116547=DIRECTION('',(0.406736643075798,-0.913545457642602,-5.72753959967194E-17));
#116548=DIRECTION('center_axis',(1.4081690688991E-16,0.,1.));
#116549=DIRECTION('ref_axis',(-1.,-4.44089209850063E-15,1.4081690688991E-16));
#116550=DIRECTION('',(-0.499999999999998,0.86602540378444,7.04084534449549E-17));
#116551=DIRECTION('center_axis',(-1.4081690688991E-16,0.,-1.));
#116552=DIRECTION('ref_axis',(-1.,0.,1.4081690688991E-16));
#116553=DIRECTION('center_axis',(-1.4081690688991E-16,0.,-1.));
#116554=DIRECTION('ref_axis',(1.,0.,-1.4081690688991E-16));
#116555=DIRECTION('',(0.203374579494982,-0.456775406784115,-0.866022521746661));
#116556=DIRECTION('center_axis',(-1.4081690688991E-16,0.,-1.));
#116557=DIRECTION('ref_axis',(-1.,0.,1.4081690688991E-16));
#116558=DIRECTION('center_axis',(-1.4081690688991E-16,0.,-1.));
#116559=DIRECTION('ref_axis',(-1.,0.,1.4081690688991E-16));
#116560=DIRECTION('center_axis',(-1.4081690688991E-16,0.,-1.));
#116561=DIRECTION('ref_axis',(-1.,0.,1.4081690688991E-16));
#116562=DIRECTION('',(-0.249998488182569,0.433019338752904,0.866022521746651));
#116563=DIRECTION('center_axis',(-1.4081690688991E-16,0.,-1.));
#116564=DIRECTION('ref_axis',(-1.,0.,1.40816906889911E-16));
#116565=DIRECTION('',(0.406736643075798,-0.913545457642602,-5.72753959967194E-17));
#116566=DIRECTION('center_axis',(1.4081690688991E-16,0.,1.));
#116567=DIRECTION('ref_axis',(-1.,-4.44089209850063E-15,1.4081690688991E-16));
#116568=DIRECTION('',(-0.499999999999998,0.86602540378444,7.04084534449549E-17));
#116569=DIRECTION('center_axis',(-1.4081690688991E-16,0.,-1.));
#116570=DIRECTION('ref_axis',(-1.,0.,1.17174841180864E-16));
#116571=DIRECTION('center_axis',(-0.913109622086492,-0.407714137590558,
7.86457210773485E-6));
#116572=DIRECTION('ref_axis',(-6.58403218430508E-6,-4.54394095516285E-6,
-0.999999999968001));
#116573=DIRECTION('center_axis',(0.866560035746485,0.499072844768375,7.86457220438574E-6));
#116574=DIRECTION('ref_axis',(-0.423232531439969,0.734883833187538,-0.529924500330478));
#116575=DIRECTION('center_axis',(-1.4081690688991E-16,0.,-1.));
#116576=DIRECTION('ref_axis',(-1.,0.,1.13676889660403E-16));
#116577=DIRECTION('center_axis',(-0.913128216116625,-0.407672492125978,
-9.77059469166599E-6));
#116578=DIRECTION('ref_axis',(0.356563044148412,-0.79866196325562,0.484769908303204));
#116579=DIRECTION('center_axis',(0.866537273132503,0.499112366283007,-9.77051476609031E-6));
#116580=DIRECTION('ref_axis',(0.436552356526076,-0.757913804263947,0.484756336026339));
#116581=DIRECTION('center_axis',(-1.4081690688991E-16,0.,-1.));
#116582=DIRECTION('ref_axis',(-1.,0.,1.15974593313694E-16));
#116583=DIRECTION('center_axis',(0.914599202553438,0.40436159357528,1.8162479713582E-5));
#116584=DIRECTION('ref_axis',(0.349880111830792,-0.791348561789984,-0.501349539840416));
#116585=DIRECTION('center_axis',(-0.864723333035746,-0.502248501217071,
1.8131645220716E-5));
#116586=DIRECTION('ref_axis',(0.435432334017781,-0.749703650686127,-0.498340364248894));
#116587=DIRECTION('center_axis',(-1.4081690688991E-16,0.,-1.));
#116588=DIRECTION('ref_axis',(-1.,0.,1.16261524579732E-16));
#116589=DIRECTION('center_axis',(0.914604666184872,0.404349235501724,1.84940660467886E-5));
#116590=DIRECTION('ref_axis',(0.350555095113837,-0.79294954439497,0.498339387700328));
#116591=DIRECTION('center_axis',(-0.864716546823262,-0.502260184871199,
1.85257209310319E-5));
#116592=DIRECTION('ref_axis',(0.434586366990742,-0.748187385815862,0.50134850686106));
#116593=DIRECTION('center_axis',(-1.4081690688991E-16,0.,-1.));
#116594=DIRECTION('ref_axis',(-1.,0.,1.40816906889911E-16));
#116595=DIRECTION('center_axis',(-1.4081690688991E-16,0.,-1.));
#116596=DIRECTION('ref_axis',(-1.,0.,1.4081690688991E-16));
#116597=DIRECTION('',(0.499999999999998,-0.86602540378444,-7.04084534449549E-17));
#116598=DIRECTION('center_axis',(-1.4081690688991E-16,0.,-1.));
#116599=DIRECTION('ref_axis',(-1.,0.,1.4081690688991E-16));
#116600=DIRECTION('center_axis',(-1.4081690688991E-16,0.,-1.));
#116601=DIRECTION('ref_axis',(-1.,0.,1.4081690688991E-16));
#116602=DIRECTION('center_axis',(-1.4081690688991E-16,0.,-1.));
#116603=DIRECTION('ref_axis',(-1.,0.,1.4081690688991E-16));
#116604=DIRECTION('',(-0.587785252292471,0.809016994374949,8.27701011433315E-17));
#116605=DIRECTION('center_axis',(1.4081690688991E-16,0.,1.));
#116606=DIRECTION('ref_axis',(1.,0.,-1.4081690688991E-16));
#116607=DIRECTION('',(0.249998457755605,-0.433019586648901,0.86602240657978));
#116608=DIRECTION('center_axis',(1.4081690688991E-16,0.,1.));
#116609=DIRECTION('ref_axis',(-1.,1.06581410364015E-14,1.40816906889911E-16));
#116610=DIRECTION('',(-0.293899542971745,0.404509888559929,-0.86602240657978));
#116611=DIRECTION('center_axis',(-1.4081690688991E-16,0.,-1.));
#116612=DIRECTION('ref_axis',(-1.,0.,1.40816906889911E-16));
#116613=DIRECTION('center_axis',(-1.4081690688991E-16,0.,-1.));
#116614=DIRECTION('ref_axis',(-1.,0.,1.4081690688991E-16));
#116615=DIRECTION('',(0.499999999999998,-0.86602540378444,-7.04084534449549E-17));
#116616=DIRECTION('center_axis',(1.4081690688991E-16,0.,1.));
#116617=DIRECTION('ref_axis',(-1.,0.,1.4081690688991E-16));
#116618=DIRECTION('',(-0.587785252292471,0.809016994374949,8.27701011433315E-17));
#116619=DIRECTION('center_axis',(-1.4081690688991E-16,0.,-1.));
#116620=DIRECTION('ref_axis',(-1.,0.,1.4081690688991E-16));
#116621=DIRECTION('center_axis',(-1.4081690688991E-16,0.,-1.));
#116622=DIRECTION('ref_axis',(1.,0.,-1.4081690688991E-16));
#116623=DIRECTION('',(0.250006503598675,-0.433014711050211,-0.866022521746674));
#116624=DIRECTION('center_axis',(-1.4081690688991E-16,0.,-1.));
#116625=DIRECTION('ref_axis',(-1.,0.,1.4081690688991E-16));
#116626=DIRECTION('center_axis',(-1.4081690688991E-16,0.,-1.));
#116627=DIRECTION('ref_axis',(-1.,0.,1.4081690688991E-16));
#116628=DIRECTION('center_axis',(-1.4081690688991E-16,0.,-1.));
#116629=DIRECTION('ref_axis',(-1.,0.,1.4081690688991E-16));
#116630=DIRECTION('',(-0.293891816351551,0.404515255718677,0.866022521746657));
#116631=DIRECTION('center_axis',(-1.4081690688991E-16,0.,-1.));
#116632=DIRECTION('ref_axis',(-1.,0.,1.40816906889911E-16));
#116633=DIRECTION('',(0.499999999999998,-0.86602540378444,-7.04084534449549E-17));
#116634=DIRECTION('center_axis',(1.4081690688991E-16,0.,1.));
#116635=DIRECTION('ref_axis',(-1.,0.,1.4081690688991E-16));
#116636=DIRECTION('',(-0.587785252292471,0.809016994374949,8.27701011433315E-17));
#116637=DIRECTION('center_axis',(-1.4081690688991E-16,0.,-1.));
#116638=DIRECTION('ref_axis',(-1.,0.,1.17174841180864E-16));
#116639=DIRECTION('center_axis',(-0.865489779781641,-0.50092658247659,7.86457214489057E-6));
#116640=DIRECTION('ref_axis',(-6.07299300101722E-6,-5.20726760504282E-6,
-0.999999999968002));
#116641=DIRECTION('center_axis',(0.809645611678816,0.586919060371517,7.86457245342431E-6));
#116642=DIRECTION('ref_axis',(-0.497730297112331,0.686618216541011,-0.529924500330483));
#116643=DIRECTION('center_axis',(-1.4081690688991E-16,0.,-1.));
#116644=DIRECTION('ref_axis',(-1.,0.,1.13676889660403E-16));
#116645=DIRECTION('center_axis',(-0.86551262508884,-0.500887108754418,-9.77059212653647E-6));
#116646=DIRECTION('ref_axis',(0.43809266217451,-0.75701582239318,0.484769908302101));
#116647=DIRECTION('center_axis',(0.809618842638511,0.586955986040874,-9.77051773404624E-6));
#116648=DIRECTION('ref_axis',(0.513384442288508,-0.708129726178339,0.484756336027398));
#116649=DIRECTION('center_axis',(-1.4081690688991E-16,0.,-1.));
#116650=DIRECTION('ref_axis',(-1.,0.,1.15974593313694E-16));
#116651=DIRECTION('center_axis',(0.867321636444858,0.497748107605381,1.81624797810239E-5));
#116652=DIRECTION('ref_axis',(0.430681881042823,-0.750441041151016,-0.501349539839815));
#116653=DIRECTION('center_axis',(-0.80748702412921,-0.589885332530142,1.81316451347442E-5));
#116654=DIRECTION('ref_axis',(0.511412360641924,-0.700081622909619,-0.498340364256086));
#116655=DIRECTION('center_axis',(-1.4081690688991E-16,0.,-1.));
#116656=DIRECTION('ref_axis',(-1.,0.,1.16261524579732E-16));
#116657=DIRECTION('center_axis',(0.867328361919153,0.49773638833082,1.84940564337033E-5));
#116658=DIRECTION('ref_axis',(0.431520514948347,-0.751962698440794,0.49833938769914));
#116659=DIRECTION('center_axis',(-0.807479053810967,-0.589896242837114,
1.85257006906714E-5));
#116660=DIRECTION('ref_axis',(0.510412535076058,-0.698662091933164,0.50134850686205));
#116661=DIRECTION('center_axis',(-1.4081690688991E-16,0.,-1.));
#116662=DIRECTION('ref_axis',(-1.,0.,1.40816906889911E-16));
#116663=DIRECTION('center_axis',(-1.4081690688991E-16,0.,-1.));
#116664=DIRECTION('ref_axis',(-1.,0.,1.4081690688991E-16));
#116665=DIRECTION('',(0.587785252292471,-0.809016994374949,-8.27701011433315E-17));
#116666=DIRECTION('center_axis',(-1.4081690688991E-16,0.,-1.));
#116667=DIRECTION('ref_axis',(-1.,0.,1.4081690688991E-16));
#116668=DIRECTION('center_axis',(-1.4081690688991E-16,0.,-1.));
#116669=DIRECTION('ref_axis',(-1.,0.,1.4081690688991E-16));
#116670=DIRECTION('center_axis',(-1.4081690688991E-16,0.,-1.));
#116671=DIRECTION('ref_axis',(-1.,0.,1.4081690688991E-16));
#116672=DIRECTION('',(-0.669130606358857,0.743144825477395,9.42249022928245E-17));
#116673=DIRECTION('center_axis',(1.4081690688991E-16,0.,1.));
#116674=DIRECTION('ref_axis',(1.,0.,-1.4081690688991E-16));
#116675=DIRECTION('',(0.293891812003446,-0.404515505437187,0.866022406579777));
#116676=DIRECTION('center_axis',(1.4081690688991E-16,0.,1.));
#116677=DIRECTION('ref_axis',(-1.,0.,1.40816906889911E-16));
#116678=DIRECTION('',(-0.334572327551833,0.371573073483921,-0.866022406579796));
#116679=DIRECTION('center_axis',(-1.4081690688991E-16,0.,-1.));
#116680=DIRECTION('ref_axis',(-1.,0.,1.40816906889911E-16));
#116681=DIRECTION('center_axis',(-1.4081690688991E-16,0.,-1.));
#116682=DIRECTION('ref_axis',(-1.,0.,1.4081690688991E-16));
#116683=DIRECTION('',(0.587785252292471,-0.809016994374949,-8.27701011433315E-17));
#116684=DIRECTION('center_axis',(1.4081690688991E-16,0.,1.));
#116685=DIRECTION('ref_axis',(-1.,0.,1.4081690688991E-16));
#116686=DIRECTION('',(-0.669130606358857,0.743144825477395,9.42249022928245E-17));
#116687=DIRECTION('center_axis',(-1.4081690688991E-16,0.,-1.));
#116688=DIRECTION('ref_axis',(-1.,0.,1.4081690688991E-16));
#116689=DIRECTION('center_axis',(-1.4081690688991E-16,0.,-1.));
#116690=DIRECTION('ref_axis',(1.,0.,-1.4081690688991E-16));
#116691=DIRECTION('',(0.293899304131716,-0.404509815527969,-0.866022521746647));
#116692=DIRECTION('center_axis',(-1.4081690688991E-16,0.,-1.));
#116693=DIRECTION('ref_axis',(-1.,0.,1.4081690688991E-16));
#116694=DIRECTION('center_axis',(-1.4081690688991E-16,0.,-1.));
#116695=DIRECTION('ref_axis',(-1.,0.,1.4081690688991E-16));
#116696=DIRECTION('center_axis',(-1.4081690688991E-16,0.,-1.));
#116697=DIRECTION('ref_axis',(-1.,0.,1.4081690688991E-16));
#116698=DIRECTION('',(-0.334565204279747,0.371579218892574,0.866022521746655));
#116699=DIRECTION('center_axis',(-1.4081690688991E-16,0.,-1.));
#116700=DIRECTION('ref_axis',(-1.,0.,1.40816906889911E-16));
#116701=DIRECTION('',(0.587785252292471,-0.809016994374949,-8.27701011433315E-17));
#116702=DIRECTION('center_axis',(1.4081690688991E-16,0.,1.));
#116703=DIRECTION('ref_axis',(-1.,0.,1.4081690688991E-16));
#116704=DIRECTION('',(-0.669130606358857,0.743144825477395,9.42249022928245E-17));
#116705=DIRECTION('center_axis',(-1.4081690688991E-16,0.,-1.));
#116706=DIRECTION('ref_axis',(-1.,0.,1.17174841180864E-16));
#116707=DIRECTION('center_axis',(-0.808387450334234,-0.588650770899236,
7.86457176845602E-6));
#116708=DIRECTION('ref_axis',(-5.49541649073876E-6,-5.81354209923377E-6,
-0.999999999968002));
#116709=DIRECTION('center_axis',(0.743860540860191,0.668334867928745,7.86457216966126E-6));
#116710=DIRECTION('ref_axis',(-0.566774825493195,0.630829867029678,-0.52992450033045));
#116711=DIRECTION('center_axis',(-1.4081690688991E-16,0.,-1.));
#116712=DIRECTION('ref_axis',(-1.,0.,1.13676889660403E-16));
#116713=DIRECTION('center_axis',(-0.808414296619818,-0.588613901403305,
-9.77059222526084E-6));
#116714=DIRECTION('ref_axis',(0.514822445316686,-0.707075657764177,0.484769908302387));
#116715=DIRECTION('center_axis',(0.743830058675508,0.668368793193793,-9.77050528701263E-6));
#116716=DIRECTION('ref_axis',(0.584591780669454,-0.650587230628161,0.484756336025942));
#116717=DIRECTION('center_axis',(-1.4081690688991E-16,0.,-1.));
#116718=DIRECTION('ref_axis',(-1.,0.,1.15974593313694E-16));
#116719=DIRECTION('center_axis',(0.810541512988656,0.585681189208076,1.81624796940111E-5));
#116720=DIRECTION('ref_axis',(0.506765009440592,-0.701311531425889,-0.501349539837977));
#116721=DIRECTION('center_axis',(-0.741403718408774,-0.671059256698607,
1.81316451549553E-5));
#116722=DIRECTION('ref_axis',(0.58178924642817,-0.642789354378085,-0.498340364247917));
#116723=DIRECTION('center_axis',(-1.4081690688991E-16,0.,-1.));
#116724=DIRECTION('ref_axis',(-1.,0.,1.16261524579732E-16));
#116725=DIRECTION('center_axis',(0.810549426621222,0.585670237131766,1.84940465536676E-5));
#116726=DIRECTION('ref_axis',(0.507758105721217,-0.702737191806194,0.498339387693513));
#116727=DIRECTION('center_axis',(-0.741394651320048,-0.671069274107243,
1.85257134388176E-5));
#116728=DIRECTION('ref_axis',(0.580646516618426,-0.641482109969101,0.501348506857733));
#116729=DIRECTION('center_axis',(-1.4081690688991E-16,0.,-1.));
#116730=DIRECTION('ref_axis',(-1.,0.,1.40816906889911E-16));
#116731=DIRECTION('center_axis',(-1.4081690688991E-16,0.,-1.));
#116732=DIRECTION('ref_axis',(-1.,0.,1.4081690688991E-16));
#116733=DIRECTION('',(0.669130606358857,-0.743144825477395,-9.42249022928245E-17));
#116734=DIRECTION('center_axis',(-1.4081690688991E-16,0.,-1.));
#116735=DIRECTION('ref_axis',(-1.,0.,1.4081690688991E-16));
#116736=DIRECTION('center_axis',(-1.4081690688991E-16,0.,-1.));
#116737=DIRECTION('ref_axis',(-1.,0.,1.4081690688991E-16));
#116738=DIRECTION('center_axis',(-1.4081690688991E-16,0.,-1.));
#116739=DIRECTION('ref_axis',(-1.,0.,1.4081690688991E-16));
#116740=DIRECTION('',(-0.743144825477393,0.669130606358859,1.04647355694969E-16));
#116741=DIRECTION('center_axis',(1.4081690688991E-16,0.,1.));
#116742=DIRECTION('ref_axis',(1.,0.,-1.4081690688991E-16));
#116743=DIRECTION('',(0.334565226058178,-0.371579467697514,0.866022406579802));
#116744=DIRECTION('center_axis',(1.4081690688991E-16,0.,1.));
#116745=DIRECTION('ref_axis',(-1.,0.,1.40816906889911E-16));
#116746=DIRECTION('',(-0.371579467697534,0.334565226058199,-0.866022406579786));
#116747=DIRECTION('center_axis',(-1.4081690688991E-16,0.,-1.));
#116748=DIRECTION('ref_axis',(-1.,0.,1.40816906889911E-16));
#116749=DIRECTION('center_axis',(-1.4081690688991E-16,0.,-1.));
#116750=DIRECTION('ref_axis',(-1.,0.,1.4081690688991E-16));
#116751=DIRECTION('',(0.669130606358857,-0.743144825477395,-9.42249022928245E-17));
#116752=DIRECTION('center_axis',(1.4081690688991E-16,0.,1.));
#116753=DIRECTION('ref_axis',(-1.,0.,1.4081690688991E-16));
#116754=DIRECTION('',(-0.743144825477393,0.669130606358859,1.04647355694969E-16));
#116755=DIRECTION('center_axis',(-1.4081690688991E-16,0.,-1.));
#116756=DIRECTION('ref_axis',(-1.,0.,1.4081690688991E-16));
#116757=DIRECTION('center_axis',(-1.4081690688991E-16,0.,-1.));
#116758=DIRECTION('ref_axis',(1.,-8.88178419700125E-16,-1.4081690688991E-16));
#116759=DIRECTION('',(0.334572082386297,-0.3715730258176,-0.866022521746663));
#116760=DIRECTION('center_axis',(-1.4081690688991E-16,0.,-1.));
#116761=DIRECTION('ref_axis',(-1.,0.,1.4081690688991E-16));
#116762=DIRECTION('center_axis',(-1.4081690688991E-16,0.,-1.));
#116763=DIRECTION('ref_axis',(-1.,0.,1.4081690688991E-16));
#116764=DIRECTION('center_axis',(-1.4081690688991E-16,0.,-1.));
#116765=DIRECTION('ref_axis',(-1.,0.,1.4081690688991E-16));
#116766=DIRECTION('',(-0.371573025817621,0.334572082386318,0.866022521746647));
#116767=DIRECTION('center_axis',(-1.4081690688991E-16,0.,-1.));
#116768=DIRECTION('ref_axis',(-1.,0.,1.40816906889911E-16));
#116769=DIRECTION('',(0.669130606358857,-0.743144825477395,-9.42249022928245E-17));
#116770=DIRECTION('center_axis',(1.4081690688991E-16,0.,1.));
#116771=DIRECTION('ref_axis',(-1.,-1.06581410364015E-14,1.4081690688991E-16));
#116772=DIRECTION('',(-0.743144825477393,0.669130606358859,1.04647355694969E-16));
#116773=DIRECTION('center_axis',(-1.4081690688991E-16,0.,-1.));
#116774=DIRECTION('ref_axis',(-1.,0.,1.17174841180864E-16));
#116775=DIRECTION('center_axis',(-0.742428258814693,-0.66992557829324,7.86457228688268E-6));
#116776=DIRECTION('ref_axis',(-4.85763185428401E-6,-6.35612262957243E-6,
-0.999999999968002));
#116777=DIRECTION('center_axis',(0.669925578293269,0.742428258814666,7.86457233399125E-6));
#116778=DIRECTION('ref_axis',(-0.629609650280318,0.56813001348582,-0.529924500330469));
#116779=DIRECTION('center_axis',(-1.4081690688991E-16,0.,-1.));
#116780=DIRECTION('ref_axis',(-1.,0.,1.13676889660403E-16));
#116781=DIRECTION('center_axis',(-0.742458811945211,-0.669891716973304,
-9.77059288644529E-6));
#116782=DIRECTION('ref_axis',(0.585911726014151,-0.649388624263268,0.484769908303495));
#116783=DIRECTION('center_axis',(0.669891716943917,0.742458811971727,-9.77052145993168E-6));
#116784=DIRECTION('ref_axis',(0.64939420916695,-0.5859167652342,0.484756336026589));
#116785=DIRECTION('center_axis',(-1.4081690688991E-16,0.,-1.));
#116786=DIRECTION('ref_axis',(-1.,0.,1.15974593313694E-16));
#116787=DIRECTION('center_axis',(0.744880927099454,0.667197425140102,1.81624797774034E-5));
#116788=DIRECTION('ref_axis',(0.577295914342274,-0.644498305797306,-0.501349539850312));
#116789=DIRECTION('center_axis',(-0.667197438400562,-0.744880915222676,
1.81316454311543E-5));
#116790=DIRECTION('ref_axis',(0.645791927483423,-0.578454551166319,-0.498340364241366));
#116791=DIRECTION('center_axis',(-1.4081690688991E-16,0.,-1.));
#116792=DIRECTION('ref_axis',(-1.,0.,1.16261524579732E-16));
#116793=DIRECTION('center_axis',(0.744889942178357,0.667187360266584,1.84940612986181E-5));
#116794=DIRECTION('ref_axis',(0.578432592429571,-0.645812349436537,0.498339387697245));
#116795=DIRECTION('center_axis',(-0.667187373874865,-0.744889929988827,
1.85257057548291E-5));
#116796=DIRECTION('ref_axis',(0.644518813413962,-0.577273915766504,0.501348506860314));
#116797=DIRECTION('center_axis',(-1.4081690688991E-16,0.,-1.));
#116798=DIRECTION('ref_axis',(-1.,0.,1.40816906889911E-16));
#116799=DIRECTION('center_axis',(-1.4081690688991E-16,0.,-1.));
#116800=DIRECTION('ref_axis',(-1.,0.,1.4081690688991E-16));
#116801=DIRECTION('',(0.743144825477393,-0.669130606358859,-1.04647355694969E-16));
#116802=DIRECTION('center_axis',(-1.4081690688991E-16,0.,-1.));
#116803=DIRECTION('ref_axis',(-1.,0.,1.4081690688991E-16));
#116804=DIRECTION('center_axis',(-1.4081690688991E-16,0.,-1.));
#116805=DIRECTION('ref_axis',(-1.,0.,1.4081690688991E-16));
#116806=DIRECTION('center_axis',(-1.4081690688991E-16,0.,-1.));
#116807=DIRECTION('ref_axis',(-1.,0.,1.4081690688991E-16));
#116808=DIRECTION('',(-0.809016994374947,0.587785252292474,1.13923270769252E-16));
#116809=DIRECTION('center_axis',(1.4081690688991E-16,0.,1.));
#116810=DIRECTION('ref_axis',(1.,0.,-1.4081690688991E-16));
#116811=DIRECTION('',(0.371573073483898,-0.334572327551837,0.866022406579805));
#116812=DIRECTION('center_axis',(1.4081690688991E-16,0.,1.));
#116813=DIRECTION('ref_axis',(-1.,0.,1.40816906889911E-16));
#116814=DIRECTION('',(-0.404515505437166,0.293891812003437,-0.86602240657979));
#116815=DIRECTION('center_axis',(-1.4081690688991E-16,0.,-1.));
#116816=DIRECTION('ref_axis',(-1.,0.,1.40816906889911E-16));
#116817=DIRECTION('center_axis',(-1.4081690688991E-16,0.,-1.));
#116818=DIRECTION('ref_axis',(-1.,0.,1.4081690688991E-16));
#116819=DIRECTION('',(0.743144825477393,-0.669130606358859,-1.04647355694969E-16));
#116820=DIRECTION('center_axis',(1.4081690688991E-16,0.,1.));
#116821=DIRECTION('ref_axis',(-1.,0.,1.4081690688991E-16));
#116822=DIRECTION('',(-0.809016994374947,0.587785252292474,1.13923270769252E-16));
#116823=DIRECTION('center_axis',(-1.4081690688991E-16,0.,-1.));
#116824=DIRECTION('ref_axis',(-1.,0.,1.4081690688991E-16));
#116825=DIRECTION('center_axis',(-1.4081690688991E-16,0.,-1.));
#116826=DIRECTION('ref_axis',(1.,0.,-1.4081690688991E-16));
#116827=DIRECTION('',(0.371579218892551,-0.33456520427975,-0.866022521746664));
#116828=DIRECTION('center_axis',(-1.4081690688991E-16,0.,-1.));
#116829=DIRECTION('ref_axis',(-1.,0.,1.4081690688991E-16));
#116830=DIRECTION('center_axis',(-1.4081690688991E-16,0.,-1.));
#116831=DIRECTION('ref_axis',(-1.,0.,1.4081690688991E-16));
#116832=DIRECTION('center_axis',(-1.4081690688991E-16,0.,-1.));
#116833=DIRECTION('ref_axis',(-1.,0.,1.4081690688991E-16));
#116834=DIRECTION('',(-0.404509815527947,0.29389930413172,0.866022521746656));
#116835=DIRECTION('center_axis',(-1.4081690688991E-16,0.,-1.));
#116836=DIRECTION('ref_axis',(-1.,0.,1.40816906889911E-16));
#116837=DIRECTION('',(0.743144825477393,-0.669130606358859,-1.04647355694969E-16));
#116838=DIRECTION('center_axis',(1.4081690688991E-16,0.,1.));
#116839=DIRECTION('ref_axis',(-1.,-1.06581410364015E-14,1.4081690688991E-16));
#116840=DIRECTION('',(-0.809016994374947,0.587785252292474,1.13923270769252E-16));
#116841=DIRECTION('center_axis',(-1.4081690688991E-16,0.,-1.));
#116842=DIRECTION('ref_axis',(-1.,0.,1.17174841180864E-16));
#116843=DIRECTION('center_axis',(-0.668334867928773,-0.743860540860166,
7.86457209247282E-6));
#116844=DIRECTION('ref_axis',(-4.16662536933619E-6,-6.82906378195756E-6,
-0.999999999968002));
#116845=DIRECTION('center_axis',(0.58865077089958,0.808387450333983,7.86457252685304E-6));
#116846=DIRECTION('ref_axis',(-0.685546339984752,0.499205608625359,-0.529924500330467));
#116847=DIRECTION('center_axis',(-1.4081690688991E-16,0.,-1.));
#116848=DIRECTION('ref_axis',(-1.,0.,1.13676889660403E-16));
#116849=DIRECTION('center_axis',(-0.668368793160425,-0.74383005870549,-9.77058632101317E-6));
#116850=DIRECTION('ref_axis',(0.650581635232264,-0.5845867531026,0.484769908302354));
#116851=DIRECTION('center_axis',(0.588613901374041,0.808414296641126,-9.77052680656433E-6));
#116852=DIRECTION('ref_axis',(0.707081738813996,-0.514826873149213,0.484756336027885));
#116853=DIRECTION('center_axis',(-1.4081690688991E-16,0.,-1.));
#116854=DIRECTION('ref_axis',(-1.,0.,1.15974593313694E-16));
#116855=DIRECTION('center_axis',(0.671059269896534,0.741403706462312,1.81624796124116E-5));
#116856=DIRECTION('ref_axis',(0.641501844408008,-0.580623821870257,-0.50134953984012));
#116857=DIRECTION('center_axis',(-0.585681203637444,-0.81054150256297,1.8131645301284E-5));
#116858=DIRECTION('ref_axis',(0.702719177032194,-0.50778207883572,-0.49834036425366));
#116859=DIRECTION('center_axis',(-1.4081690688991E-16,0.,-1.));
#116860=DIRECTION('ref_axis',(-1.,0.,1.16261524579732E-16));
#116861=DIRECTION('center_axis',(0.671069287652099,0.741394639060787,1.84940697053889E-5));
#116862=DIRECTION('ref_axis',(0.642769650611578,-0.581811851823098,0.498339387697629));
#116863=DIRECTION('center_axis',(-0.585670251953324,-0.81054941591104,1.85257201982103E-5));
#116864=DIRECTION('ref_axis',(0.701329627214891,-0.50674098774034,0.501348506863805));
#116865=DIRECTION('center_axis',(-1.4081690688991E-16,0.,-1.));
#116866=DIRECTION('ref_axis',(-1.,0.,1.40816906889911E-16));
#116867=DIRECTION('center_axis',(-1.4081690688991E-16,0.,-1.));
#116868=DIRECTION('ref_axis',(-1.,0.,1.4081690688991E-16));
#116869=DIRECTION('',(0.809016994374947,-0.587785252292474,-1.13923270769252E-16));
#116870=DIRECTION('center_axis',(-1.4081690688991E-16,0.,-1.));
#116871=DIRECTION('ref_axis',(-1.,0.,1.4081690688991E-16));
#116872=DIRECTION('center_axis',(-1.4081690688991E-16,0.,-1.));
#116873=DIRECTION('ref_axis',(-1.,0.,1.4081690688991E-16));
#116874=DIRECTION('center_axis',(-1.4081690688991E-16,0.,-1.));
#116875=DIRECTION('ref_axis',(-1.,0.,1.4081690688991E-16));
#116876=DIRECTION('',(-0.866025403784438,0.500000000000001,1.2195101864901E-16));
#116877=DIRECTION('center_axis',(1.4081690688991E-16,0.,1.));
#116878=DIRECTION('ref_axis',(1.,0.,-1.4081690688991E-16));
#116879=DIRECTION('',(0.404509888559909,-0.293899542971724,0.866022406579796));
#116880=DIRECTION('center_axis',(1.4081690688991E-16,0.,1.));
#116881=DIRECTION('ref_axis',(-1.,0.,1.40816906889911E-16));
#116882=DIRECTION('',(-0.433019586648901,0.249998457755605,-0.86602240657978));
#116883=DIRECTION('center_axis',(-1.4081690688991E-16,0.,-1.));
#116884=DIRECTION('ref_axis',(-1.,0.,1.40816906889911E-16));
#116885=DIRECTION('center_axis',(-1.4081690688991E-16,0.,-1.));
#116886=DIRECTION('ref_axis',(-1.,0.,1.4081690688991E-16));
#116887=DIRECTION('',(0.809016994374947,-0.587785252292474,-1.13923270769252E-16));
#116888=DIRECTION('center_axis',(1.4081690688991E-16,0.,1.));
#116889=DIRECTION('ref_axis',(-1.,0.,1.4081690688991E-16));
#116890=DIRECTION('',(-0.866025403784438,0.500000000000001,1.2195101864901E-16));
#116891=DIRECTION('center_axis',(-1.4081690688991E-16,0.,-1.));
#116892=DIRECTION('ref_axis',(-1.,0.,1.4081690688991E-16));
#116893=DIRECTION('center_axis',(-1.4081690688991E-16,0.,-1.));
#116894=DIRECTION('ref_axis',(1.,0.,-1.4081690688991E-16));
#116895=DIRECTION('',(0.40451525571868,-0.293891816351526,-0.866022521746664));
#116896=DIRECTION('center_axis',(-1.4081690688991E-16,0.,-1.));
#116897=DIRECTION('ref_axis',(-1.,0.,1.4081690688991E-16));
#116898=DIRECTION('center_axis',(-1.4081690688991E-16,0.,-1.));
#116899=DIRECTION('ref_axis',(-1.,0.,1.4081690688991E-16));
#116900=DIRECTION('center_axis',(-1.4081690688991E-16,0.,-1.));
#116901=DIRECTION('ref_axis',(-1.,0.,1.4081690688991E-16));
#116902=DIRECTION('',(-0.433014711050233,0.250006503598672,0.866022521746663));
#116903=DIRECTION('center_axis',(-1.4081690688991E-16,0.,-1.));
#116904=DIRECTION('ref_axis',(-1.,0.,1.40816906889911E-16));
#116905=DIRECTION('',(0.809016994374947,-0.587785252292474,-1.13923270769252E-16));
#116906=DIRECTION('center_axis',(1.4081690688991E-16,0.,1.));
#116907=DIRECTION('ref_axis',(-1.,-1.24344978758018E-14,1.4081690688991E-16));
#116908=DIRECTION('',(-0.866025403784438,0.500000000000001,1.2195101864901E-16));
#116909=DIRECTION('center_axis',(-1.4081690688991E-16,0.,-1.));
#116910=DIRECTION('ref_axis',(-1.,0.,1.17174841180864E-16));
#116911=DIRECTION('center_axis',(-0.586919060371807,-0.809645611678606,
7.86457181291275E-6));
#116912=DIRECTION('ref_axis',(-3.4299684348052E-6,-7.2271841840149E-6,-0.999999999968002));
#116913=DIRECTION('center_axis',(0.500926582476729,0.86548977978156,7.86457235433928E-6));
#116914=DIRECTION('ref_axis',(-0.733972040528699,0.424811802651075,-0.529924500330455));
#116915=DIRECTION('center_axis',(-1.4081690688991E-16,0.,-1.));
#116916=DIRECTION('ref_axis',(-1.,0.,1.13676889660403E-16));
#116917=DIRECTION('center_axis',(-0.586955986008474,-0.809618842662,-9.77058993673793E-6));
#116918=DIRECTION('ref_axis',(0.708123635911361,-0.513380027141697,0.484769908302552));
#116919=DIRECTION('center_axis',(0.500887108719152,0.86551262510925,-9.77051851264757E-6));
#116920=DIRECTION('ref_axis',(0.757022332965959,-0.438096430108722,0.484756336025401));
#116921=DIRECTION('center_axis',(-1.4081690688991E-16,0.,-1.));
#116922=DIRECTION('ref_axis',(-1.,0.,1.15974593313694E-16));
#116923=DIRECTION('center_axis',(0.589885346904599,0.80748701362769,1.81624796986456E-5));
#116924=DIRECTION('ref_axis',(0.698679346015346,-0.510387901840021,-0.501349539849106));
#116925=DIRECTION('center_axis',(-0.497748123045557,-0.867321627584524,
1.81316453122383E-5));
#116926=DIRECTION('ref_axis',(0.751947288228285,-0.431546239793356,-0.498340364255539));
#116927=DIRECTION('center_axis',(-1.4081690688991E-16,0.,-1.));
#116928=DIRECTION('ref_axis',(-1.,0.,1.16261524579732E-16));
#116929=DIRECTION('center_axis',(0.589896257578203,0.807479043042728,1.84940806699832E-5));
#116930=DIRECTION('ref_axis',(0.700064389992645,-0.511436901808749,0.498339387699282));
#116931=DIRECTION('center_axis',(-0.497736404182369,-0.8673283528217,1.85257135242689E-5));
#116932=DIRECTION('ref_axis',(0.750456526858729,-0.430656099411321,0.501348506864197));
#116933=DIRECTION('center_axis',(-1.4081690688991E-16,0.,-1.));
#116934=DIRECTION('ref_axis',(-1.,0.,1.40816906889911E-16));
#116935=DIRECTION('center_axis',(-1.4081690688991E-16,0.,-1.));
#116936=DIRECTION('ref_axis',(-1.,0.,1.4081690688991E-16));
#116937=DIRECTION('',(0.866025403784438,-0.500000000000001,-1.2195101864901E-16));
#116938=DIRECTION('center_axis',(-1.4081690688991E-16,0.,-1.));
#116939=DIRECTION('ref_axis',(-1.,0.,1.4081690688991E-16));
#116940=DIRECTION('center_axis',(-1.4081690688991E-16,0.,-1.));
#116941=DIRECTION('ref_axis',(-1.,0.,1.4081690688991E-16));
#116942=DIRECTION('center_axis',(-1.4081690688991E-16,0.,-1.));
#116943=DIRECTION('ref_axis',(-1.,0.,1.4081690688991E-16));
#116944=DIRECTION('',(-0.913545457642601,0.406736643075801,1.28642645648559E-16));
#116945=DIRECTION('center_axis',(1.4081690688991E-16,0.,1.));
#116946=DIRECTION('ref_axis',(1.,0.,-1.4081690688991E-16));
#116947=DIRECTION('',(0.433014808647712,-0.250006733496369,0.866022406579795));
#116948=DIRECTION('center_axis',(1.4081690688991E-16,0.,1.));
#116949=DIRECTION('ref_axis',(-1.,0.,1.40816906889911E-16));
#116950=DIRECTION('',(-0.456779414654131,0.203366068089033,-0.866022406579781));
#116951=DIRECTION('center_axis',(-1.4081690688991E-16,0.,-1.));
#116952=DIRECTION('ref_axis',(-1.,0.,1.40816906889911E-16));
#116953=DIRECTION('center_axis',(-1.4081690688991E-16,0.,-1.));
#116954=DIRECTION('ref_axis',(-1.,0.,1.4081690688991E-16));
#116955=DIRECTION('',(0.866025403784438,-0.500000000000001,-1.2195101864901E-16));
#116956=DIRECTION('center_axis',(1.4081690688991E-16,0.,1.));
#116957=DIRECTION('ref_axis',(-1.,1.24344978758018E-14,1.4081690688991E-16));
#116958=DIRECTION('',(-0.913545457642601,0.406736643075801,1.28642645648559E-16));
#116959=DIRECTION('center_axis',(-1.4081690688991E-16,0.,-1.));
#116960=DIRECTION('ref_axis',(-1.,0.,1.4081690688991E-16));
#116961=DIRECTION('center_axis',(-1.4081690688991E-16,0.,-1.));
#116962=DIRECTION('ref_axis',(1.,0.,-1.4081690688991E-16));
#116963=DIRECTION('',(0.433019338752905,-0.249998488182556,-0.866022521746654));
#116964=DIRECTION('center_axis',(-1.4081690688991E-16,0.,-1.));
#116965=DIRECTION('ref_axis',(-1.,0.,1.4081690688991E-16));
#116966=DIRECTION('center_axis',(-1.4081690688991E-16,0.,-1.));
#116967=DIRECTION('ref_axis',(-1.,0.,1.4081690688991E-16));
#116968=DIRECTION('center_axis',(-1.4081690688991E-16,0.,-1.));
#116969=DIRECTION('ref_axis',(-1.,0.,1.4081690688991E-16));
#116970=DIRECTION('',(-0.456775406784136,0.203374579494979,0.86602252174665));
#116971=DIRECTION('center_axis',(-1.4081690688991E-16,0.,-1.));
#116972=DIRECTION('ref_axis',(-1.,0.,1.40816906889911E-16));
#116973=DIRECTION('',(0.866025403784438,-0.500000000000001,-1.2195101864901E-16));
#116974=DIRECTION('center_axis',(1.4081690688991E-16,0.,1.));
#116975=DIRECTION('ref_axis',(-1.,0.,1.4081690688991E-16));
#116976=DIRECTION('',(-0.913545457642601,0.406736643075801,1.28642645648559E-16));
#116977=DIRECTION('center_axis',(-1.4081690688991E-16,0.,-1.));
#116978=DIRECTION('ref_axis',(-1.,0.,1.17174841180864E-16));
#116979=DIRECTION('center_axis',(-0.499072844768411,-0.866560035746465,
7.86457214289953E-6));
#116980=DIRECTION('ref_axis',(-2.655732390574E-6,-7.54612254363985E-6,-0.999999999968002));
#116981=DIRECTION('center_axis',(0.407714137590715,0.913109622086422,7.86457249655275E-6));
#116982=DIRECTION('ref_axis',(-0.774356189802951,0.345763669669564,-0.529924500330464));
#116983=DIRECTION('center_axis',(-1.4081690688991E-16,0.,-1.));
#116984=DIRECTION('ref_axis',(-1.,0.,1.13676889660403E-16));
#116985=DIRECTION('center_axis',(-0.499112366248818,-0.866537273152195,
-9.77058602131441E-6));
#116986=DIRECTION('ref_axis',(0.757907285848944,-0.43654860217067,0.484769908306942));
#116987=DIRECTION('center_axis',(0.407672492086804,0.913128216134116,-9.77051719973362E-6));
#116988=DIRECTION('ref_axis',(0.798668832020144,-0.356566110901745,0.484756336024588));
#116989=DIRECTION('center_axis',(-1.4081690688991E-16,0.,-1.));
#116990=DIRECTION('ref_axis',(-1.,0.,1.15974593313694E-16));
#116991=DIRECTION('center_axis',(0.502248516610394,0.864723324094351,1.81624796546292E-5));
#116992=DIRECTION('ref_axis',(0.748201970509818,-0.434560065158728,-0.501349539836697));
#116993=DIRECTION('center_axis',(-0.404361609857007,-0.91459919535559,1.81316453037353E-5));
#116994=DIRECTION('ref_axis',(0.792936907584003,-0.350582289843111,-0.498340364248652));
#116995=DIRECTION('center_axis',(-1.4081690688991E-16,0.,-1.));
#116996=DIRECTION('ref_axis',(-1.,0.,1.16261524579732E-16));
#116997=DIRECTION('center_axis',(0.502260200679148,0.864716537642083,1.84940567917327E-5));
#116998=DIRECTION('ref_axis',(0.74968907742121,-0.435458542074672,0.498339387696313));
#116999=DIRECTION('center_axis',(-0.404349252215734,-0.914604658794921,
1.85257199402894E-5));
#117000=DIRECTION('ref_axis',(0.791361267754418,-0.349852852738104,0.501348506858384));
#117001=DIRECTION('center_axis',(-1.4081690688991E-16,0.,-1.));
#117002=DIRECTION('ref_axis',(-1.,0.,1.40816906889911E-16));
#117003=DIRECTION('center_axis',(-1.4081690688991E-16,0.,-1.));
#117004=DIRECTION('ref_axis',(-1.,0.,1.4081690688991E-16));
#117005=DIRECTION('',(0.913545457642601,-0.406736643075801,-1.28642645648559E-16));
#117006=DIRECTION('center_axis',(-1.4081690688991E-16,0.,-1.));
#117007=DIRECTION('ref_axis',(-1.,0.,1.4081690688991E-16));
#117008=DIRECTION('center_axis',(-1.4081690688991E-16,0.,-1.));
#117009=DIRECTION('ref_axis',(-1.,0.,1.4081690688991E-16));
#117010=DIRECTION('center_axis',(-1.4081690688991E-16,0.,-1.));
#117011=DIRECTION('ref_axis',(-1.,0.,1.4081690688991E-16));
#117012=DIRECTION('',(-0.951056516295153,0.309016994374948,1.33924836902177E-16));
#117013=DIRECTION('center_axis',(1.4081690688991E-16,0.,1.));
#117014=DIRECTION('ref_axis',(1.,0.,-1.4081690688991E-16));
#117015=DIRECTION('',(0.456775527877821,-0.203374797931565,0.86602240657978));
#117016=DIRECTION('center_axis',(1.4081690688991E-16,0.,1.));
#117017=DIRECTION('ref_axis',(-1.,0.,1.40816906889911E-16));
#117018=DIRECTION('',(-0.475534671805141,0.15450555722341,-0.866022406579795));
#117019=DIRECTION('center_axis',(-1.4081690688991E-16,0.,-1.));
#117020=DIRECTION('ref_axis',(-1.,0.,1.40816906889911E-16));
#117021=DIRECTION('center_axis',(-1.4081690688991E-16,0.,-1.));
#117022=DIRECTION('ref_axis',(-1.,0.,1.4081690688991E-16));
#117023=DIRECTION('',(0.9135454576426,-0.406736643075801,-1.28642645648559E-16));
#117024=DIRECTION('center_axis',(1.4081690688991E-16,0.,1.));
#117025=DIRECTION('ref_axis',(-1.,-1.24344978758018E-14,1.4081690688991E-16));
#117026=DIRECTION('',(-0.951056516295153,0.309016994374948,1.33924836902177E-16));
#117027=DIRECTION('center_axis',(-1.4081690688991E-16,0.,-1.));
#117028=DIRECTION('ref_axis',(-1.,0.,1.4081690688991E-16));
#117029=DIRECTION('center_axis',(-1.4081690688991E-16,0.,-1.));
#117030=DIRECTION('ref_axis',(1.,0.,-1.4081690688991E-16));
#117031=DIRECTION('',(0.456779171296642,-0.203366124261506,-0.866022521746638));
#117032=DIRECTION('center_axis',(-1.4081690688991E-16,0.,-1.));
#117033=DIRECTION('ref_axis',(-1.,0.,1.4081690688991E-16));
#117034=DIRECTION('center_axis',(-1.4081690688991E-16,0.,-1.));
#117035=DIRECTION('ref_axis',(-1.,0.,1.4081690688991E-16));
#117036=DIRECTION('center_axis',(-1.4081690688991E-16,0.,-1.));
#117037=DIRECTION('ref_axis',(-1.,0.,1.4081690688991E-16));
#117038=DIRECTION('',(-0.47553157557488,0.154514440939486,0.866022521746652));
#117039=DIRECTION('center_axis',(-1.4081690688991E-16,0.,-1.));
#117040=DIRECTION('ref_axis',(-1.,0.,1.40816906889911E-16));
#117041=DIRECTION('',(0.913545457642601,-0.406736643075801,-1.28642645648559E-16));
#117042=DIRECTION('center_axis',(1.4081690688991E-16,0.,1.));
#117043=DIRECTION('ref_axis',(-1.,-1.24344978758018E-14,1.4081690688991E-16));
#117044=DIRECTION('',(-0.951056516295153,0.309016994374948,1.33924836902177E-16));
#117045=DIRECTION('center_axis',(-1.4081690688991E-16,0.,-1.));
#117046=DIRECTION('ref_axis',(-1.,0.,1.17174841180864E-16));
#117047=DIRECTION('center_axis',(-0.405758682640351,-0.913980246723153,
7.86457178216999E-6));
#117048=DIRECTION('ref_axis',(-1.85239931600463E-6,-7.78238337918387E-6,
-0.999999999968002));
#117049=DIRECTION('center_axis',(0.310034691293422,0.950725244291294,7.86457224375456E-6));
#117050=DIRECTION('ref_axis',(-0.806256330617395,0.262927277567121,-0.529924500330488));
#117051=DIRECTION('center_axis',(-1.4081690688991E-16,0.,-1.));
#117052=DIRECTION('ref_axis',(-1.,0.,1.13676889660403E-16));
#117053=DIRECTION('center_axis',(-0.405800366957686,-0.913961739944043,
-9.77058414968768E-6));
#117054=DIRECTION('ref_axis',(0.799387144964551,-0.354934259362886,0.48476990830284));
#117055=DIRECTION('center_axis',(0.309991330319367,0.95073938333876,-9.77051439570099E-6));
#117056=DIRECTION('ref_axis',(0.831564948216299,-0.271129178766668,0.484756336028046));
#117057=DIRECTION('center_axis',(-1.4081690688991E-16,0.,-1.));
#117058=DIRECTION('ref_axis',(-1.,0.,1.15974593313694E-16));
#117059=DIRECTION('center_axis',(0.409108946466091,0.912485544867166,1.81624799040554E-5));
#117060=DIRECTION('ref_axis',(0.789527137636282,-0.353971097460886,-0.501349539840415));
#117061=DIRECTION('center_axis',(-0.306544826252881,-0.951856222950102,
1.81316451570291E-5));
#117062=DIRECTION('ref_axis',(0.825238944244478,-0.265777286959491,-0.498340364247882));
#117063=DIRECTION('center_axis',(-1.4081690688991E-16,0.,-1.));
#117064=DIRECTION('ref_axis',(-1.,0.,1.16261524579732E-16));
#117065=DIRECTION('center_axis',(0.40912127591188,0.912480016906785,1.84940449550723E-5));
#117066=DIRECTION('ref_axis',(0.791100014435804,-0.354709207428031,0.498339387692211));
#117067=DIRECTION('center_axis',(-0.306531965214468,-0.951860364737683,
1.85257042376944E-5));
#117068=DIRECTION('ref_axis',(0.823595688991461,-0.265216544996207,0.501348506864193));
#117069=DIRECTION('center_axis',(-1.4081690688991E-16,0.,-1.));
#117070=DIRECTION('ref_axis',(-1.,0.,1.40816906889911E-16));
#117071=DIRECTION('center_axis',(-1.4081690688991E-16,0.,-1.));
#117072=DIRECTION('ref_axis',(-1.,0.,1.4081690688991E-16));
#117073=DIRECTION('',(0.951056516295153,-0.309016994374948,-1.33924836902177E-16));
#117074=DIRECTION('center_axis',(-1.4081690688991E-16,0.,-1.));
#117075=DIRECTION('ref_axis',(-1.,0.,1.4081690688991E-16));
#117076=DIRECTION('center_axis',(-1.4081690688991E-16,0.,-1.));
#117077=DIRECTION('ref_axis',(-1.,0.,1.4081690688991E-16));
#117078=DIRECTION('center_axis',(-1.4081690688991E-16,0.,-1.));
#117079=DIRECTION('ref_axis',(-1.,0.,1.4081690688991E-16));
#117080=DIRECTION('',(-0.978147600733806,0.20791169081776,1.37739719617122E-16));
#117081=DIRECTION('center_axis',(1.4081690688991E-16,0.,1.));
#117082=DIRECTION('ref_axis',(1.,0.,-1.4081690688991E-16));
#117083=DIRECTION('',(0.475531718838045,-0.154514645521707,0.866022406579781));
#117084=DIRECTION('center_axis',(1.4081690688991E-16,0.,1.));
#117085=DIRECTION('ref_axis',(-1.,0.,1.40816906889911E-16));
#117086=DIRECTION('',(-0.489079871579872,0.103952251140493,-0.866022406579784));
#117087=DIRECTION('center_axis',(-1.4081690688991E-16,0.,-1.));
#117088=DIRECTION('ref_axis',(-1.,0.,1.40816906889911E-16));
#117089=DIRECTION('center_axis',(-1.4081690688991E-16,0.,-1.));
#117090=DIRECTION('ref_axis',(-1.,0.,1.4081690688991E-16));
#117091=DIRECTION('',(0.951056516295153,-0.309016994374948,-1.33924836902177E-16));
#117092=DIRECTION('center_axis',(1.4081690688991E-16,0.,1.));
#117093=DIRECTION('ref_axis',(-1.,0.,1.4081690688991E-16));
#117094=DIRECTION('',(-0.978147600733806,0.20791169081776,1.37739719617122E-16));
#117095=DIRECTION('center_axis',(-1.4081690688991E-16,0.,-1.));
#117096=DIRECTION('ref_axis',(-1.,0.,1.4081690688991E-16));
#117097=DIRECTION('center_axis',(-1.4081690688991E-16,0.,-1.));
#117098=DIRECTION('ref_axis',(1.,0.,-1.4081690688991E-16));
#117099=DIRECTION('',(0.475534435652401,-0.154505638525951,-0.866022521746658));
#117100=DIRECTION('center_axis',(-1.4081690688991E-16,0.,-1.));
#117101=DIRECTION('ref_axis',(-1.,0.,1.4081690688991E-16));
#117102=DIRECTION('center_axis',(-1.4081690688991E-16,0.,-1.));
#117103=DIRECTION('ref_axis',(-1.,0.,1.4081690688991E-16));
#117104=DIRECTION('center_axis',(-1.4081690688991E-16,0.,-1.));
#117105=DIRECTION('ref_axis',(-1.,0.,1.4081690688991E-16));
#117106=DIRECTION('',(-0.489077720912242,0.103961409834797,0.866022521746662));
#117107=DIRECTION('center_axis',(-1.4081690688991E-16,0.,-1.));
#117108=DIRECTION('ref_axis',(-1.,0.,1.40816906889911E-16));
#117109=DIRECTION('',(0.951056516295153,-0.309016994374948,-1.33924836902177E-16));
#117110=DIRECTION('center_axis',(1.4081690688991E-16,0.,1.));
#117111=DIRECTION('ref_axis',(-1.,-1.33226762955019E-14,1.4081690688991E-16));
#117112=DIRECTION('',(-0.978147600733806,0.20791169081776,1.37739719617122E-16));
#117113=DIRECTION('center_axis',(-1.4081690688991E-16,0.,-1.));
#117114=DIRECTION('ref_axis',(-1.,0.,1.17174841180864E-16));
#117115=DIRECTION('center_axis',(-0.307998943474356,-0.951386698854272,
7.86457226542829E-6));
#117116=DIRECTION('ref_axis',(-1.0287712269461E-6,-7.93337958510981E-6,
-0.999999999968001));
#117117=DIRECTION('center_axis',(0.208958440039612,0.977924521767585,7.86457233133809E-6));
#117118=DIRECTION('ref_axis',(-0.829322958353501,0.177210199190947,-0.529924500330474));
#117119=DIRECTION('center_axis',(-1.4081690688991E-16,0.,-1.));
#117120=DIRECTION('ref_axis',(-1.,0.,1.13676889660403E-16));
#117121=DIRECTION('center_axis',(-0.308042333923157,-0.95137265065573,-9.77058986043835E-6));
#117122=DIRECTION('ref_axis',(0.83210875123643,-0.269431182534026,0.484769908300902));
#117123=DIRECTION('center_axis',(0.208913838670723,0.977934050903434,-9.77051847801327E-6));
#117124=DIRECTION('ref_axis',(0.855350264825764,-0.182721698612452,0.484756336027365));
#117125=DIRECTION('center_axis',(-1.4081690688991E-16,0.,-1.));
#117126=DIRECTION('ref_axis',(-1.,0.,1.15974593313694E-16));
#117127=DIRECTION('center_axis',(0.311487093092649,0.950250383060599,1.81624798352045E-5));
#117128=DIRECTION('ref_axis',(0.822202080223852,-0.269503948346651,-0.501349539843347));
#117129=DIRECTION('center_axis',(-0.20536947338361,-0.978684514577288,1.81316452437622E-5));
#117130=DIRECTION('ref_axis',(0.848499490336976,-0.178060372501888,-0.498340364251564));
#117131=DIRECTION('center_axis',(-1.4081690688991E-16,0.,-1.));
#117132=DIRECTION('ref_axis',(-1.,0.,1.16261524579732E-16));
#117133=DIRECTION('center_axis',(0.311499932820754,0.950246174162588,1.84940539067784E-5));
#117134=DIRECTION('ref_axis',(0.8238434941389,-0.270073604474909,0.49833938769772));
#117135=DIRECTION('center_axis',(-0.205356249870299,-0.97868728932995,1.85257143532325E-5));
#117136=DIRECTION('ref_axis',(0.846806623515352,-0.177674469288616,0.501348506862778));
#117137=DIRECTION('center_axis',(-1.4081690688991E-16,0.,-1.));
#117138=DIRECTION('ref_axis',(-1.,0.,1.40816906889911E-16));
#117139=DIRECTION('center_axis',(-1.4081690688991E-16,0.,-1.));
#117140=DIRECTION('ref_axis',(-1.,0.,1.4081690688991E-16));
#117141=DIRECTION('',(0.978147600733806,-0.20791169081776,-1.37739719617122E-16));
#117142=DIRECTION('center_axis',(-1.4081690688991E-16,0.,-1.));
#117143=DIRECTION('ref_axis',(-1.,0.,1.4081690688991E-16));
#117144=DIRECTION('center_axis',(-1.4081690688991E-16,0.,-1.));
#117145=DIRECTION('ref_axis',(-1.,0.,1.4081690688991E-16));
#117146=DIRECTION('center_axis',(-1.4081690688991E-16,0.,-1.));
#117147=DIRECTION('ref_axis',(-1.,0.,1.4081690688991E-16));
#117148=DIRECTION('',(-0.994521895368273,0.104528463267654,1.40045497140051E-16));
#117149=DIRECTION('center_axis',(1.4081690688991E-16,0.,1.));
#117150=DIRECTION('ref_axis',(1.,0.,-1.4081690688991E-16));
#117151=DIRECTION('',(0.489077884775266,-0.103961598321233,0.866022406579787));
#117152=DIRECTION('center_axis',(1.4081690688991E-16,0.,1.));
#117153=DIRECTION('ref_axis',(-1.,0.,1.40816906889911E-16));
#117154=DIRECTION('',(-0.497266609935056,0.0522600224406417,-0.866022406579761));
#117155=DIRECTION('center_axis',(-1.4081690688991E-16,0.,-1.));
#117156=DIRECTION('ref_axis',(-1.,0.,1.40816906889911E-16));
#117157=DIRECTION('center_axis',(-1.4081690688991E-16,0.,-1.));
#117158=DIRECTION('ref_axis',(-1.,0.,1.4081690688991E-16));
#117159=DIRECTION('',(0.978147600733806,-0.20791169081776,-1.37739719617122E-16));
#117160=DIRECTION('center_axis',(1.4081690688991E-16,0.,1.));
#117161=DIRECTION('ref_axis',(-1.,0.,1.4081690688991E-16));
#117162=DIRECTION('',(-0.994521895368273,0.104528463267654,1.40045497140051E-16));
#117163=DIRECTION('center_axis',(-1.4081690688991E-16,0.,-1.));
#117164=DIRECTION('ref_axis',(-1.,0.,1.4081690688991E-16));
#117165=DIRECTION('center_axis',(-1.4081690688991E-16,0.,-1.));
#117166=DIRECTION('ref_axis',(1.,0.,-1.4081690688991E-16));
#117167=DIRECTION('',(0.489079645219224,-0.103952356682314,-0.866022521746652));
#117168=DIRECTION('center_axis',(-1.4081690688991E-16,0.,-1.));
#117169=DIRECTION('ref_axis',(-1.,0.,1.4081690688991E-16));
#117170=DIRECTION('center_axis',(-1.4081690688991E-16,0.,-1.));
#117171=DIRECTION('ref_axis',(-1.,0.,1.4081690688991E-16));
#117172=DIRECTION('center_axis',(-1.4081690688991E-16,0.,-1.));
#117173=DIRECTION('ref_axis',(-1.,0.,1.4081690688991E-16));
#117174=DIRECTION('',(-0.497265428393217,0.0522693557686608,0.866022521746657));
#117175=DIRECTION('center_axis',(-1.4081690688991E-16,0.,-1.));
#117176=DIRECTION('ref_axis',(-1.,0.,1.40816906889911E-16));
#117177=DIRECTION('',(0.978147600733806,-0.20791169081776,-1.37739719617122E-16));
#117178=DIRECTION('center_axis',(1.4081690688991E-16,0.,1.));
#117179=DIRECTION('ref_axis',(-1.,0.,1.4081690688991E-16));
#117180=DIRECTION('',(-0.994521895368273,0.104528463267654,1.40045497140051E-16));
#117181=DIRECTION('center_axis',(-1.4081690688991E-16,0.,-1.));
#117182=DIRECTION('ref_axis',(-1.,0.,1.17174841180864E-16));
#117183=DIRECTION('center_axis',(-0.206864703431192,-0.978369559222114,
7.86457194672106E-6));
#117184=DIRECTION('ref_axis',(-1.93871468046092E-7,-7.99745526561114E-6,
-0.999999999968002));
#117185=DIRECTION('center_axis',(0.105592796389255,0.99440945353956,7.86457230629007E-6));
#117186=DIRECTION('ref_axis',(-0.843303350210935,0.0895515687886684,-0.529924500330473));
#117187=DIRECTION('center_axis',(-1.4081690688991E-16,0.,-1.));
#117188=DIRECTION('ref_axis',(-1.,0.,1.13676889660403E-16));
#117189=DIRECTION('center_axis',(-0.206909324622115,-0.978360123517387,
-9.77058412670988E-6));
#117190=DIRECTION('ref_axis',(0.855713599896876,-0.180976161286326,0.484769908304544));
#117191=DIRECTION('center_axis',(0.105547443284639,0.994414268361337,-9.77051707379648E-6));
#117192=DIRECTION('ref_axis',(0.869764184940883,-0.092312281291246,0.484756336025561));
#117193=DIRECTION('center_axis',(-1.4081690688991E-16,0.,-1.));
#117194=DIRECTION('ref_axis',(-1.,0.,1.15974593313694E-16));
#117195=DIRECTION('center_axis',(0.210452521944388,0.977604079204548,1.81624797328856E-5));
#117196=DIRECTION('ref_axis',(0.845868804765148,-0.182084057577678,-0.50134953984344));
#117197=DIRECTION('center_axis',(-0.101944049587622,-0.994790133859861,
1.81316452425136E-5));
#117198=DIRECTION('ref_axis',(0.862463698451802,-0.0883925913418604,-0.498340364257914));
#117199=DIRECTION('center_axis',(-1.4081690688991E-16,0.,-1.));
#117200=DIRECTION('ref_axis',(-1.,0.,1.16261524579732E-16));
#117201=DIRECTION('center_axis',(0.210465731284082,0.977601235480513,1.84940551537643E-5));
#117202=DIRECTION('ref_axis',(0.847560772122061,-0.182479018595766,0.498339387698967));
#117203=DIRECTION('center_axis',(-0.101930608472471,-0.994791511178714,
1.8525712556693E-5));
#117204=DIRECTION('ref_axis',(0.860739767465021,-0.0881857549145027,0.50134850686366));
#117205=DIRECTION('center_axis',(-1.4081690688991E-16,0.,-1.));
#117206=DIRECTION('ref_axis',(-1.,0.,1.40816906889911E-16));
#117207=DIRECTION('center_axis',(-1.4081690688991E-16,0.,-1.));
#117208=DIRECTION('ref_axis',(-1.,0.,1.40816906889911E-16));
#117209=DIRECTION('center_axis',(-1.4081690688991E-16,0.,-1.));
#117210=DIRECTION('ref_axis',(-1.,0.,1.4081690688991E-16));
#117211=DIRECTION('',(0.994521895368273,-0.104528463267654,-1.40045497140051E-16));
#117212=DIRECTION('center_axis',(-1.4081690688991E-16,0.,-1.));
#117213=DIRECTION('ref_axis',(-1.,0.,1.4081690688991E-16));
#117214=DIRECTION('center_axis',(-1.4081690688991E-16,0.,-1.));
#117215=DIRECTION('ref_axis',(-1.,0.,1.4081690688991E-16));
#117216=DIRECTION('center_axis',(-1.4081690688991E-16,0.,-1.));
#117217=DIRECTION('ref_axis',(-1.,0.,1.4081690688991E-16));
#117218=DIRECTION('',(-1.,0.,1.40816906889911E-16));
#117219=DIRECTION('center_axis',(1.4081690688991E-16,0.,1.));
#117220=DIRECTION('ref_axis',(1.,0.,-1.4081690688991E-16));
#117221=DIRECTION('',(0.497265611060779,-0.052269526094198,0.866022406579782));
#117222=DIRECTION('center_axis',(1.4081690688991E-16,0.,1.));
#117223=DIRECTION('ref_axis',(-1.,0.,1.40816906889911E-16));
#117224=DIRECTION('',(-0.500005191251964,-4.77800116594404E-6,-0.866022406579794));
#117225=DIRECTION('center_axis',(-1.4081690688991E-16,0.,-1.));
#117226=DIRECTION('ref_axis',(-1.,0.,1.40816906889911E-16));
#117227=DIRECTION('center_axis',(-1.4081690688991E-16,0.,-1.));
#117228=DIRECTION('ref_axis',(-1.,0.,1.4081690688991E-16));
#117229=DIRECTION('',(0.994521895368273,-0.104528463267654,-1.40045497140051E-16));
#117230=DIRECTION('center_axis',(1.4081690688991E-16,0.,1.));
#117231=DIRECTION('ref_axis',(-1.,0.,1.4081690688991E-16));
#117232=DIRECTION('',(-1.,0.,1.40816906889911E-16));
#117233=DIRECTION('center_axis',(-1.4081690688991E-16,0.,-1.));
#117234=DIRECTION('ref_axis',(-1.,0.,1.4081690688991E-16));
#117235=DIRECTION('center_axis',(-1.4081690688991E-16,0.,-1.));
#117236=DIRECTION('ref_axis',(1.,0.,-1.4081690688991E-16));
#117237=DIRECTION('',(0.497266395846506,-0.0522601510654393,-0.86602252174666));
#117238=DIRECTION('center_axis',(-1.4081690688991E-16,0.,-1.));
#117239=DIRECTION('ref_axis',(-1.,0.,1.4081690688991E-16));
#117240=DIRECTION('center_axis',(-1.4081690688991E-16,0.,-1.));
#117241=DIRECTION('ref_axis',(-1.,0.,1.4081690688991E-16));
#117242=DIRECTION('center_axis',(-1.4081690688991E-16,0.,-1.));
#117243=DIRECTION('ref_axis',(-1.,0.,1.4081690688991E-16));
#117244=DIRECTION('',(-0.500004991781248,4.62770265298126E-6,0.866022521746645));
#117245=DIRECTION('center_axis',(-1.4081690688991E-16,0.,-1.));
#117246=DIRECTION('ref_axis',(-1.,0.,1.40816906889911E-16));
#117247=DIRECTION('',(0.994521895368273,-0.104528463267654,-1.40045497140051E-16));
#117248=DIRECTION('center_axis',(1.4081690688991E-16,0.,1.));
#117249=DIRECTION('ref_axis',(-1.,8.88178419700125E-16,1.4081690688991E-16));
#117250=DIRECTION('',(-1.,0.,1.40816906889911E-16));
#117251=DIRECTION('center_axis',(-1.4081690688991E-16,0.,-1.));
#117252=DIRECTION('ref_axis',(-1.,0.,1.40816906889911E-16));
#117253=DIRECTION('center_axis',(1.4081690688991E-16,0.,1.));
#117254=DIRECTION('ref_axis',(1.,0.,-1.40816906889911E-16));
#117255=DIRECTION('center_axis',(-1.4081690688991E-16,0.,-1.));
#117256=DIRECTION('ref_axis',(-1.,0.,1.17174841180864E-16));
#117257=DIRECTION('center_axis',(-0.10346401040769,-0.994633197962197,7.86457223164439E-6));
#117258=DIRECTION('ref_axis',(6.43152272453738E-7,-7.97390974138951E-6,
-0.999999999968001));
#117259=DIRECTION('center_axis',(0.00107025596496794,0.999999427244995,
7.86457231481231E-6));
#117260=DIRECTION('ref_axis',(-0.848044334090874,0.000911792658906122,-0.529924500330484));
#117261=DIRECTION('center_axis',(-1.4081690688991E-16,0.,-1.));
#117262=DIRECTION('ref_axis',(-1.,0.,1.13676889660403E-16));
#117263=DIRECTION('center_axis',(-0.103509373457973,-0.994628478131847,
-9.77058577218967E-6));
#117264=DIRECTION('ref_axis',(0.86994307128939,-0.090538327344475,0.484769908304186));
#117265=DIRECTION('center_axis',(0.00102464802306578,0.999999475000345,
-9.77051630226669E-6));
#117266=DIRECTION('ref_axis',(0.874648786634608,-0.000891471298440391,0.484756336026185));
#117267=DIRECTION('center_axis',(-1.4081690688991E-16,0.,-1.));
#117268=DIRECTION('ref_axis',(-1.,0.,1.15974593313694E-16));
#117269=DIRECTION('center_axis',(0.107112188925724,0.994246940479911,1.81624797797238E-5));
#117270=DIRECTION('ref_axis',(0.8602680136723,-0.0926692157703517,-0.501349539843035));
#117271=DIRECTION('center_axis',(0.0025982945487801,-0.999996624262643,
1.81316452304032E-5));
#117272=DIRECTION('ref_axis',(0.86697857380863,0.0022436375454785,-0.498340364256518));
#117273=DIRECTION('center_axis',(-1.4081690688991E-16,0.,-1.));
#117274=DIRECTION('ref_axis',(-1.,0.,1.16261524579732E-16));
#117275=DIRECTION('center_axis',(0.107125623152071,0.994245493086215,1.84940574365093E-5));
#117276=DIRECTION('ref_axis',(0.861991996922946,-0.0928851544029273,0.498339387699122));
#117277=DIRECTION('center_axis',(0.00261180600209789,-0.999996589057286,
1.85257109031372E-5));
#117278=DIRECTION('ref_axis',(0.865242466402697,0.0022691410444305,0.501348506861542));
#117279=DIRECTION('center_axis',(0.,0.,-1.));
#117280=DIRECTION('ref_axis',(-1.,0.,0.));
#117281=DIRECTION('',(1.,0.,0.));
#117282=DIRECTION('center_axis',(0.,0.,1.));
#117283=DIRECTION('ref_axis',(-1.,2.87680990140871E-12,0.));
#117284=DIRECTION('',(-1.,0.,0.));
#117285=DIRECTION('center_axis',(0.,0.,-1.));
#117286=DIRECTION('ref_axis',(-1.,0.,0.));
#117287=DIRECTION('center_axis',(0.,1.,0.));
#117288=DIRECTION('ref_axis',(0.,0.,1.));
#117289=DIRECTION('center_axis',(0.,1.,0.));
#117290=DIRECTION('ref_axis',(0.874651456243763,0.,-0.484752338922326));
#117291=DIRECTION('',(-0.529924709392054,0.,0.848044693619238));
#117292=DIRECTION('',(1.,0.,0.));
#117293=DIRECTION('',(-0.529924185123399,0.,-0.848045021223108));
#117294=DIRECTION('center_axis',(0.,1.,0.));
#117295=DIRECTION('ref_axis',(0.87464958095347,0.,0.484755722542725));
#117296=DIRECTION('',(-1.,0.,1.40816906889911E-16));
#117297=DIRECTION('',(-0.500005012714982,0.,0.866022509672752));
#117298=DIRECTION('center_axis',(9.46835263434497E-7,-0.999999999998207,
1.6399888684466E-6));
#117299=DIRECTION('ref_axis',(0.866072335964589,1.6672152936214E-10,-0.499918702267519));
#117300=DIRECTION('',(-1.,0.,1.40816906889911E-16));
#117301=DIRECTION('center_axis',(-9.46924650952009E-7,-0.999999999998207,
1.64014404584511E-6));
#117302=DIRECTION('ref_axis',(0.866043284546592,-5.6510002087391E-11,0.499969028332507));
#117303=DIRECTION('',(-0.500005169296824,0.,-0.866022419268955));
#117304=DIRECTION('',(-1.,0.,1.40816906889911E-16));
#117305=DIRECTION('center_axis',(0.,1.,0.));
#117306=DIRECTION('ref_axis',(0.,0.,1.));
#117307=DIRECTION('center_axis',(0.,-1.,0.));
#117308=DIRECTION('ref_axis',(0.874649580936389,0.,0.484755722573544));
#117309=DIRECTION('',(0.529924185123402,0.,0.848045021223106));
#117310=DIRECTION('',(-1.,0.,0.));
#117311=DIRECTION('',(0.529924709392048,0.,-0.848044693619242));
#117312=DIRECTION('center_axis',(0.,-1.,0.));
#117313=DIRECTION('ref_axis',(0.874651456263025,0.,-0.48475233888757));
#117314=DIRECTION('',(1.,0.,-1.40816906889911E-16));
#117315=DIRECTION('',(0.500005169296809,0.,0.866022419268964));
#117316=DIRECTION('center_axis',(-9.47055353975915E-7,0.999999999998206,
1.64037043322054E-6));
#117317=DIRECTION('ref_axis',(0.866072438648806,1.66973549937258E-10,0.499918524374633));
#117318=DIRECTION('',(1.,0.,-1.40816906889911E-16));
#117319=DIRECTION('center_axis',(9.46713288386241E-7,0.999999999998207,
1.63977759862047E-6));
#117320=DIRECTION('ref_axis',(0.866043178342335,-5.6270925409859E-11,-0.499969212298824));
#117321=DIRECTION('',(0.500005012714974,0.,-0.866022509672756));
#117322=DIRECTION('',(1.,0.,-1.40816906889911E-16));
#117323=DIRECTION('center_axis',(1.,0.,0.));
#117324=DIRECTION('ref_axis',(0.,0.,-1.));
#117325=DIRECTION('center_axis',(-1.,0.,0.));
#117326=DIRECTION('ref_axis',(0.,0.,1.));
#117327=DIRECTION('center_axis',(-0.50000501436341,0.,0.866022508721018));
#117328=DIRECTION('ref_axis',(0.,1.,0.));
#117329=DIRECTION('center_axis',(-0.866018223014682,-3.00422159123528E-5,
0.500012436349295));
#117330=DIRECTION('ref_axis',(0.500012217440787,-0.000989701289107013,0.866017784402437));
#117331=DIRECTION('center_axis',(0.500005023014372,-1.99980824065794E-14,
-0.866022503726316));
#117332=DIRECTION('ref_axis',(-0.866022503726316,2.47318747560494E-28,-0.500005023014372));
#117333=DIRECTION('center_axis',(1.,0.,0.));
#117334=DIRECTION('ref_axis',(0.,0.,-1.));
#117335=DIRECTION('center_axis',(-1.,0.,1.4081690688991E-16));
#117336=DIRECTION('ref_axis',(1.40816906889911E-16,0.,1.));
#117337=DIRECTION('center_axis',(-1.,0.,0.));
#117338=DIRECTION('ref_axis',(0.,0.,1.));
#117339=DIRECTION('center_axis',(-1.,0.,1.4081690688991E-16));
#117340=DIRECTION('ref_axis',(1.40816906889911E-16,0.,1.));
#117341=DIRECTION('center_axis',(1.,0.,0.));
#117342=DIRECTION('ref_axis',(0.,0.,-1.));
#117343=DIRECTION('center_axis',(-0.529924213265765,0.,-0.848045003637578));
#117344=DIRECTION('ref_axis',(-0.848045003637578,0.,0.529924213265765));
#117345=DIRECTION('center_axis',(0.500005158533463,0.,0.866022425483271));
#117346=DIRECTION('ref_axis',(0.866022425483271,0.,-0.500005158533463));
#117347=DIRECTION('center_axis',(0.529924185004324,-2.16262675490169E-8,
0.848045021297515));
#117348=DIRECTION('ref_axis',(0.848037146343382,-0.004309503024554,-0.529919264233199));
#117349=DIRECTION('center_axis',(-0.529924157141051,0.,-0.848045038708645));
#117350=DIRECTION('ref_axis',(-0.848045038708645,0.,0.529924157141051));
#117351=DIRECTION('center_axis',(0.500005172385364,-1.05122400740158E-8,
0.866022417485762));
#117352=DIRECTION('ref_axis',(0.866013458679462,-0.00454855867535886,-0.500000000000012));
#117353=DIRECTION('center_axis',(0.866037336481604,3.44576745566438E-5,
0.499979330205277));
#117354=DIRECTION('ref_axis',(0.499979069431793,0.000963977570940208,-0.866036951219381));
#117355=DIRECTION('center_axis',(-0.00024249581833115,-0.999999970597889,
-1.33391011393658E-17));
#117356=DIRECTION('ref_axis',(0.999999970597889,-0.00024249581833115,2.11314776580936E-36));
#117357=DIRECTION('center_axis',(-1.,0.,1.4081690688991E-16));
#117358=DIRECTION('ref_axis',(1.40816906889911E-16,0.,1.));
#117359=DIRECTION('center_axis',(1.,0.,0.));
#117360=DIRECTION('ref_axis',(0.,0.,-1.));
#117361=DIRECTION('center_axis',(0.,0.,-1.));
#117362=DIRECTION('ref_axis',(1.,-1.22464679914735E-16,0.));
#117363=DIRECTION('center_axis',(0.000242495818331158,-0.999999970597889,
0.));
#117364=DIRECTION('ref_axis',(0.999999970597889,0.000242495818331158,0.));
#117365=DIRECTION('center_axis',(0.529924676825566,-1.73811117043118E-14,
-0.848044713969328));
#117366=DIRECTION('ref_axis',(-0.848044713969328,2.32169098057144E-28,-0.529924676825566));
#117367=DIRECTION('center_axis',(0.529924157141051,0.,0.848045038708645));
#117368=DIRECTION('ref_axis',(0.848045038708645,0.,-0.529924157141051));
#117369=DIRECTION('center_axis',(0.529924709439987,2.52123003281154E-8,
-0.848044693589285));
#117370=DIRECTION('ref_axis',(-0.848035979777038,0.00453325469494587,-0.529919264233213));
#117371=DIRECTION('center_axis',(0.529924742154432,2.89534768729527E-14,
-0.848044673146739));
#117372=DIRECTION('ref_axis',(-0.848044673146739,-6.50756462101157E-28,
-0.529924742154432));
#117373=DIRECTION('center_axis',(-0.529924185162637,2.16871498834536E-8,
-0.848045021198589));
#117374=DIRECTION('ref_axis',(0.84803714634339,0.00430950302080326,-0.529919264233217));
#117375=DIRECTION('center_axis',(0.52992421326579,0.,0.848045003637563));
#117376=DIRECTION('ref_axis',(0.848045003637563,0.,-0.52992421326579));
#117377=DIRECTION('center_axis',(-0.000258180127964207,-0.99999996667151,
2.74452783786513E-17));
#117378=DIRECTION('ref_axis',(0.99999996667151,-0.000258180127964207,3.13697794718818E-34));
#117379=DIRECTION('center_axis',(1.,0.,0.));
#117380=DIRECTION('ref_axis',(0.,0.,-1.));
#117381=DIRECTION('center_axis',(0.,0.,-1.));
#117382=DIRECTION('ref_axis',(1.,-1.22464679914735E-16,0.));
#117383=DIRECTION('center_axis',(0.000258180127964191,-0.99999996667151,
-7.67076204667453E-19));
#117384=DIRECTION('ref_axis',(0.99999996667151,0.000258180127964191,6.2059328036136E-36));
#117385=DIRECTION('center_axis',(1.,0.,-1.4081690688991E-16));
#117386=DIRECTION('ref_axis',(-1.40816906889911E-16,0.,-1.));
#117387=DIRECTION('center_axis',(0.866018223015031,-3.00422149566322E-5,
-0.500012436348692));
#117388=DIRECTION('ref_axis',(0.500012217440177,0.000989701300755193,0.866017784402776));
#117389=DIRECTION('center_axis',(-0.529924742154432,2.89534768729527E-14,
0.848044673146739));
#117390=DIRECTION('ref_axis',(0.848044673146739,-6.50756462101157E-28,0.529924742154432));
#117391=DIRECTION('center_axis',(-0.500005009599423,-1.01154993436287E-8,
0.866022511471544));
#117392=DIRECTION('ref_axis',(-0.866013834616154,-0.00447641077897882,-0.499999999999963));
#117393=DIRECTION('center_axis',(0.50000502301429,0.,-0.866022503726363));
#117394=DIRECTION('ref_axis',(-0.866022503726363,0.,-0.50000502301429));
#117395=DIRECTION('center_axis',(-0.529924709245855,-2.52865664166506E-8,
0.848044693710594));
#117396=DIRECTION('ref_axis',(-0.848035979777064,-0.00453325468699187,-0.529919264233239));
#117397=DIRECTION('center_axis',(-0.529924676825566,0.,0.848044713969328));
#117398=DIRECTION('ref_axis',(0.848044713969328,0.,0.529924676825566));
#117399=DIRECTION('center_axis',(1.,0.,0.));
#117400=DIRECTION('ref_axis',(0.,0.,-1.));
#117401=DIRECTION('center_axis',(-1.,0.,0.));
#117402=DIRECTION('ref_axis',(0.,0.,1.));
#117403=DIRECTION('center_axis',(1.,0.,-1.4081690688991E-16));
#117404=DIRECTION('ref_axis',(-1.40816906889911E-16,0.,-1.));
#117405=DIRECTION('center_axis',(1.,0.,-5.46369598732844E-14));
#117406=DIRECTION('ref_axis',(-5.46369598732844E-14,0.,-1.));
#117407=DIRECTION('center_axis',(1.,0.,-1.4081690688991E-16));
#117408=DIRECTION('ref_axis',(-1.40816906889911E-16,0.,-1.));
#117409=DIRECTION('center_axis',(-0.866037336481684,3.44576748030691E-5,
-0.499979330205138));
#117410=DIRECTION('ref_axis',(0.499979069431657,-0.000963977564006246,-0.866036951219467));
#117411=DIRECTION('center_axis',(0.500005158533422,0.,0.866022425483294));
#117412=DIRECTION('ref_axis',(0.866022425483294,0.,-0.500005158533422));
#117413=DIRECTION('center_axis',(0.500005167510848,3.81405054986521E-20,
0.866022420300104));
#117414=DIRECTION('ref_axis',(-5.80463060321091E-12,-1.,3.35689480667619E-12));
#117415=DIRECTION('center_axis',(-7.71409749859041E-19,-1.47193748793066E-17,
-1.));
#117416=DIRECTION('ref_axis',(0.,1.,-1.47193748793066E-17));
#117417=DIRECTION('',(0.994521895368273,-0.104528463267654,7.71409749859047E-19));
#117418=DIRECTION('center_axis',(7.71409749859041E-19,1.47193748793066E-17,
1.));
#117419=DIRECTION('ref_axis',(-1.13546692937274E-35,1.,-1.47193748793066E-17));
#117420=DIRECTION('',(-0.994521895368273,0.104528463267654,-7.71409749859047E-19));
#117421=DIRECTION('center_axis',(-7.71409749859041E-19,-1.47193748793066E-17,
-1.));
#117422=DIRECTION('ref_axis',(-1.13546692937274E-35,1.,-1.47193748793066E-17));
#117423=DIRECTION('center_axis',(0.104528463267654,0.994521895368273,-1.47193748793066E-17));
#117424=DIRECTION('ref_axis',(7.71409749859047E-19,1.47193748793066E-17,
1.));
#117425=DIRECTION('center_axis',(0.104528463267658,0.994521895368273,9.44192068578644E-15));
#117426=DIRECTION('ref_axis',(0.869860024050839,-0.0914259726160459,-0.484752338921106));
#117427=DIRECTION('',(-0.527021726387054,0.0553922155203088,0.848044693619246));
#117428=DIRECTION('',(0.994521895368273,-0.104528463267654,7.71409749859047E-19));
#117429=DIRECTION('',(-0.527021204990396,0.0553921607193119,-0.848045021223117));
#117430=DIRECTION('center_axis',(0.104528463267649,0.994521895368274,9.30408455334034E-16));
#117431=DIRECTION('ref_axis',(0.869858159032171,-0.0914257765946819,0.484755722544067));
#117432=DIRECTION('',(-0.994521895368273,0.104528463267654,1.40045497140051E-16));
#117433=DIRECTION('',(-0.497265932938937,0.0522647556052235,0.866022509672754));
#117434=DIRECTION('center_axis',(-0.104527521619077,-0.994521994337724,
1.63998885004745E-6));
#117435=DIRECTION('ref_axis',(0.861327901104895,-0.090529210190981,-0.499918702271112));
#117436=DIRECTION('',(-0.994521895368273,0.104528463267654,1.40045497140051E-16));
#117437=DIRECTION('center_axis',(-0.10452940500478,-0.99452179638591,1.64014407352427E-6));
#117438=DIRECTION('ref_axis',(0.861299008811912,-0.0905261737130823,0.499969028333243));
#117439=DIRECTION('',(-0.497266088663009,0.0522647719724877,-0.866022419268957));
#117440=DIRECTION('',(-0.994521895368273,0.104528463267654,1.40045497140051E-16));
#117441=DIRECTION('center_axis',(0.104528463267654,0.994521895368273,-1.47193748793066E-17));
#117442=DIRECTION('ref_axis',(7.71409749859047E-19,1.47193748793066E-17,
1.));
#117443=DIRECTION('center_axis',(-0.10452846326766,-0.994521895368273,1.53689692974248E-14));
#117444=DIRECTION('ref_axis',(0.869858159016364,-0.0914257765930224,0.484755722572745));
#117445=DIRECTION('',(0.527021204990418,-0.0553921607193131,0.848045021223103));
#117446=DIRECTION('',(-0.994521895368273,0.104528463267654,-7.71409749859047E-19));
#117447=DIRECTION('',(0.527021726387064,-0.0553922155203084,-0.84804469361924));
#117448=DIRECTION('center_axis',(-0.104528463267655,-0.994521895368273,
-5.16893468263946E-15));
#117449=DIRECTION('ref_axis',(0.86986002406852,-0.0914259726179035,-0.484752338889029));
#117450=DIRECTION('',(0.994521895368273,-0.104528463267654,-1.40045497140051E-16));
#117451=DIRECTION('',(0.497266088663021,-0.0522647719724764,0.866022419268951));
#117452=DIRECTION('center_axis',(0.104527521400183,0.99452199436073,1.64037041736128E-6));
#117453=DIRECTION('ref_axis',(0.861328003227763,-0.0905292209242674,0.499918524376243));
#117454=DIRECTION('',(0.994521895368273,-0.104528463267654,-1.40045497140051E-16));
#117455=DIRECTION('center_axis',(0.104529404794558,0.994521796408006,1.6397775895808E-6));
#117456=DIRECTION('ref_axis',(0.861298903189669,-0.0905261626115,-0.499969212299227));
#117457=DIRECTION('',(0.497265932938941,-0.0522647556052202,-0.866022509672752));
#117458=DIRECTION('',(0.994521895368273,-0.104528463267654,-1.40045497140051E-16));
#117459=DIRECTION('center_axis',(-3.07718727278886E-18,-2.92774812072083E-17,
-1.));
#117460=DIRECTION('ref_axis',(0.,1.,-2.92774812072083E-17));
#117461=DIRECTION('',(0.978147600733805,-0.20791169081776,3.07718727278885E-18));
#117462=DIRECTION('center_axis',(3.07718727278886E-18,2.92774812072083E-17,
1.));
#117463=DIRECTION('ref_axis',(2.06146211212399E-12,1.,-2.92774812072147E-17));
#117464=DIRECTION('',(-0.978147600733805,0.20791169081776,-3.07718727278885E-18));
#117465=DIRECTION('center_axis',(-3.07718727278886E-18,-2.92774812072083E-17,
-1.));
#117466=DIRECTION('ref_axis',(-9.00922925501365E-35,1.,-2.92774812072083E-17));
#117467=DIRECTION('center_axis',(0.20791169081776,0.978147600733806,-2.92774812072083E-17));
#117468=DIRECTION('ref_axis',(3.07718727278885E-18,2.92774812072083E-17,
1.));
#117469=DIRECTION('center_axis',(0.20791169081775,0.978147600733808,-1.98487091788775E-14));
#117470=DIRECTION('ref_axis',(0.855538223403966,-0.181850263144028,-0.484752338920849));
#117471=DIRECTION('',(-0.518344583061404,0.110177542335813,0.848044693619234));
#117472=DIRECTION('',(0.978147600733806,-0.20791169081776,3.07718727278885E-18));
#117473=DIRECTION('',(-0.51834407024927,0.110177433334225,-0.848045021223109));
#117474=DIRECTION('center_axis',(0.207911690817753,0.978147600733807,2.06757434518666E-14));
#117475=DIRECTION('ref_axis',(0.855536389092489,-0.18184987324909,0.48475572254268));
#117476=DIRECTION('',(-0.978147600733806,0.20791169081776,1.37739719617122E-16));
#117477=DIRECTION('',(-0.489078703542049,0.103956887610924,0.866022509672744));
#117478=DIRECTION('center_axis',(-0.207910764672752,-0.978147797590171,
1.63998885404889E-6));
#117479=DIRECTION('ref_axis',(0.847146577520636,-0.180066563577866,-0.49991870226701));
#117480=DIRECTION('',(-0.978147600733806,0.20791169081776,1.37739719617122E-16));
#117481=DIRECTION('center_axis',(-0.207912617049446,-0.978147403855349,
1.64014403655927E-6));
#117482=DIRECTION('ref_axis',(0.847118160899391,-0.18006052366677,0.499969028332038));
#117483=DIRECTION('',(-0.489078856702209,0.10395692016612,-0.866022419268944));
#117484=DIRECTION('',(-0.978147600733806,0.20791169081776,1.37739719617122E-16));
#117485=DIRECTION('center_axis',(0.20791169081776,0.978147600733806,-2.92774812072083E-17));
#117486=DIRECTION('ref_axis',(3.07718727278885E-18,2.92774812072083E-17,
1.));
#117487=DIRECTION('center_axis',(-0.207911690817745,-0.978147600733809,
-2.96352322775435E-14));
#117488=DIRECTION('ref_axis',(0.855536389075761,-0.181849873245532,0.484755722573536));
#117489=DIRECTION('',(0.51834407024926,-0.110177433334229,0.848045021223114));
#117490=DIRECTION('',(-0.978147600733806,0.20791169081776,-3.07718727278885E-18));
#117491=DIRECTION('',(0.518344583061397,-0.110177542335811,-0.848044693619238));
#117492=DIRECTION('center_axis',(-0.207911690817741,-0.978147600733809,
3.58379471329602E-14));
#117493=DIRECTION('ref_axis',(0.855538223421254,-0.181850263147702,-0.48475233888896));
#117494=DIRECTION('',(0.978147600733806,-0.20791169081776,-1.37739719617122E-16));
#117495=DIRECTION('',(0.489078856702182,-0.103956920166122,0.866022419268959));
#117496=DIRECTION('center_axis',(0.207910764457463,0.978147797635931,1.64037042063162E-6));
#117497=DIRECTION('ref_axis',(0.847146677961002,-0.180066584926861,0.499918524374138));
#117498=DIRECTION('',(0.978147600733806,-0.20791169081776,-1.37739719617122E-16));
#117499=DIRECTION('center_axis',(0.207912616842747,0.978147403899286,1.63977763102226E-6));
#117500=DIRECTION('ref_axis',(0.847118057016918,-0.180060501585644,-0.499969212296724));
#117501=DIRECTION('',(0.489078703542038,-0.103956887610914,-0.866022509672751));
#117502=DIRECTION('',(0.978147600733806,-0.20791169081776,-1.37739719617122E-16));
#117503=DIRECTION('center_axis',(-6.89206998773325E-18,-4.35148173242971E-17,
-1.));
#117504=DIRECTION('ref_axis',(0.,1.,-4.35148173242971E-17));
#117505=DIRECTION('',(0.951056516295153,-0.309016994374948,6.89206998773323E-18));
#117506=DIRECTION('center_axis',(6.89206998773325E-18,4.35148173242971E-17,
1.));
#117507=DIRECTION('ref_axis',(-6.04138961080025E-12,1.,-4.35148173242554E-17));
#117508=DIRECTION('',(-0.951056516295153,0.309016994374948,-6.89206998773323E-18));
#117509=DIRECTION('center_axis',(-6.89206998773325E-18,-4.35148173242971E-17,
-1.));
#117510=DIRECTION('ref_axis',(-2.99907166502483E-34,1.,-4.3514817324297E-17));
#117511=DIRECTION('center_axis',(0.309016994374948,0.951056516295153,-4.35148173242971E-17));
#117512=DIRECTION('ref_axis',(6.89206998773323E-18,4.35148173242971E-17,
1.));
#117513=DIRECTION('center_axis',(0.309016994374967,0.951056516295147,1.64027527242141E-14));
#117514=DIRECTION('ref_axis',(0.831842966947326,-0.270282164134015,-0.484752338922984));
#117515=DIRECTION('',(-0.503988348013121,0.163755740941345,0.848044693619243));
#117516=DIRECTION('',(0.951056516295153,-0.309016994374948,6.89206998773323E-18));
#117517=DIRECTION('',(-0.503987849404001,0.163755578933424,-0.848045021223113));
#117518=DIRECTION('center_axis',(0.309016994374924,0.951056516295161,2.70163047771038E-14));
#117519=DIRECTION('ref_axis',(0.831841183440083,-0.270281584637364,0.484755722543754));
#117520=DIRECTION('',(-0.951056516295153,0.309016994374948,1.33924836902177E-16));
#117521=DIRECTION('',(-0.475533025522855,0.154510046201616,0.86602250967273));
#117522=DIRECTION('center_axis',(-0.309016093880578,-0.951056808881625,
1.63998878674474E-6));
#117523=DIRECTION('ref_axis',(0.823683738752414,-0.267631070012105,-0.4999187022697));
#117524=DIRECTION('',(-0.951056516295153,0.309016994374948,1.33924836902177E-16));
#117525=DIRECTION('center_axis',(-0.309017894953236,-0.951056223677644,
1.64014402270259E-6));
#117526=DIRECTION('ref_axis',(0.823656109144367,-0.267622092842979,0.499969028332263));
#117527=DIRECTION('',(-0.475533174441006,0.154510094588038,-0.866022419268956));
#117528=DIRECTION('',(-0.951056516295153,0.309016994374948,1.33924836902177E-16));
#117529=DIRECTION('center_axis',(0.309016994374948,0.951056516295153,-4.35148173242971E-17));
#117530=DIRECTION('ref_axis',(6.89206998773323E-18,4.35148173242971E-17,
1.));
#117531=DIRECTION('center_axis',(-0.309016994374939,-0.951056516295156,
-2.55000835876533E-14));
#117532=DIRECTION('ref_axis',(0.831841183424993,-0.270281584632475,0.484755722572375));
#117533=DIRECTION('',(0.50398784940402,-0.163755578933425,0.848045021223101));
#117534=DIRECTION('',(-0.951056516295153,0.309016994374948,-6.89206998773323E-18));
#117535=DIRECTION('',(0.503988348013121,-0.163755740941342,-0.848044693619244));
#117536=DIRECTION('center_axis',(-0.309016994374968,-0.951056516295147,
-3.11514463540405E-14));
#117537=DIRECTION('ref_axis',(0.831842966966041,-0.270282164140089,-0.484752338887482));
#117538=DIRECTION('',(0.951056516295153,-0.309016994374948,-1.33924836902177E-16));
#117539=DIRECTION('',(0.475533174441017,-0.154510094588048,0.866022419268948));
#117540=DIRECTION('center_axis',(0.309016093671225,0.951056808949647,1.64037048079197E-6));
#117541=DIRECTION('ref_axis',(0.823683836411307,-0.267631101743173,0.49991852437621));
#117542=DIRECTION('',(0.951056516295153,-0.309016994374948,-1.33924836902177E-16));
#117543=DIRECTION('center_axis',(0.309017894752217,0.95105622374296,1.63977757430429E-6));
#117544=DIRECTION('ref_axis',(0.823656008137434,-0.267622060023585,-0.499969212299957));
#117545=DIRECTION('',(0.475533025522778,-0.154510046201593,-0.866022509672777));
#117546=DIRECTION('',(0.951056516295153,-0.309016994374948,-1.33924836902177E-16));
#117547=DIRECTION('center_axis',(-1.21742612413517E-17,-5.72753959967198E-17,
-1.));
#117548=DIRECTION('ref_axis',(0.,1.,-5.72753959967198E-17));
#117549=DIRECTION('',(0.913545457642601,-0.406736643075801,1.21742612413517E-17));
#117550=DIRECTION('center_axis',(1.21742612413517E-17,5.72753959967198E-17,
1.));
#117551=DIRECTION('ref_axis',(6.46878029454758E-34,1.,-5.72753959967198E-17));
#117552=DIRECTION('',(-0.913545457642601,0.406736643075801,-1.21742612413517E-17));
#117553=DIRECTION('center_axis',(-1.21742612413517E-17,-5.72753959967198E-17,
-1.));
#117554=DIRECTION('ref_axis',(-6.97285633565939E-34,1.,-5.72753959967198E-17));
#117555=DIRECTION('center_axis',(0.406736643075801,0.913545457642601,-5.72753959967198E-17));
#117556=DIRECTION('ref_axis',(1.21742612413517E-17,5.72753959967198E-17,
1.));
#117557=DIRECTION('center_axis',(0.406736643075802,0.9135454576426,-1.92973561461323E-15));
#117558=DIRECTION('ref_axis',(0.799033864872045,-0.355752797173982,-0.484752338922186));
#117559=DIRECTION('',(-0.484110311157685,0.21553979738105,0.848044693619237));
#117560=DIRECTION('',(0.913545457642601,-0.406736643075801,1.21742612413517E-17));
#117561=DIRECTION('',(-0.48410983221443,0.215539584141768,-0.848045021223113));
#117562=DIRECTION('center_axis',(0.406736643075762,0.913545457642618,8.22894589384297E-14));
#117563=DIRECTION('ref_axis',(0.799032151707043,-0.355752034423781,0.48475572254668));
#117564=DIRECTION('',(-0.913545457642601,0.406736643075801,1.28642645648559E-16));
#117565=DIRECTION('',(-0.456777308164345,0.203370360392779,0.866022509672725));
#117566=DIRECTION('center_axis',(-0.406735778098035,-0.913545842753551,
1.63998882315082E-6));
#117567=DIRECTION('ref_axis',(0.791196448574938,-0.352263354437297,-0.499918702273668));
#117568=DIRECTION('',(-0.913545457642601,0.406736643075801,1.28642645648559E-16));
#117569=DIRECTION('center_axis',(-0.406737508133811,-0.913545072491997,
1.64014409189978E-6));
#117570=DIRECTION('ref_axis',(0.791169908697132,-0.352251538366759,0.49996902833118));
#117571=DIRECTION('',(-0.456777451208935,0.203370424080343,-0.866022419268953));
#117572=DIRECTION('',(-0.913545457642601,0.406736643075801,1.28642645648559E-16));
#117573=DIRECTION('center_axis',(0.406736643075801,0.913545457642601,-5.72753959967198E-17));
#117574=DIRECTION('ref_axis',(1.21742612413517E-17,5.72753959967198E-17,
1.));
#117575=DIRECTION('center_axis',(-0.406736643075822,-0.913545457642591,
5.01731374373309E-14));
#117576=DIRECTION('ref_axis',(0.799032151693804,-0.355752034417879,0.484755722572834));
#117577=DIRECTION('',(0.484109832214452,-0.215539584141766,0.848045021223101));
#117578=DIRECTION('',(-0.913545457642601,0.406736643075801,-1.21742612413517E-17));
#117579=DIRECTION('',(0.484110311157686,-0.215539797381044,-0.848044693619238));
#117580=DIRECTION('center_axis',(-0.406736643075838,-0.913545457642584,
-6.80920995526314E-14));
#117581=DIRECTION('ref_axis',(0.799033864889633,-0.355752797181813,-0.484752338887448));
#117582=DIRECTION('',(0.913545457642601,-0.406736643075801,-1.28642645648559E-16));
#117583=DIRECTION('',(0.456777451208942,-0.203370424080346,0.866022419268949));
#117584=DIRECTION('center_axis',(0.406735777896996,0.913545842843059,1.64037035504947E-6));
#117585=DIRECTION('ref_axis',(0.791196542384502,-0.352263396203737,0.499918524375541));
#117586=DIRECTION('',(0.913545457642601,-0.406736643075801,-1.28642645648559E-16));
#117587=DIRECTION('center_axis',(0.406737507940663,0.913545072577993,1.63977754573074E-6));
#117588=DIRECTION('ref_axis',(0.791169811676266,-0.352251495170018,-0.499969212294745));
#117589=DIRECTION('',(0.45677730816427,-0.203370360392744,-0.866022509672773));
#117590=DIRECTION('',(0.913545457642601,-0.406736643075801,-1.28642645648559E-16));
#117591=DIRECTION('center_axis',(-1.88658882409001E-17,-7.04084534449554E-17,
-1.));
#117592=DIRECTION('ref_axis',(0.,1.,-7.04084534449554E-17));
#117593=DIRECTION('',(0.866025403784438,-0.500000000000001,1.88658882409001E-17));
#117594=DIRECTION('center_axis',(1.88658882409001E-17,7.04084534449554E-17,
1.));
#117595=DIRECTION('ref_axis',(3.83604259468484E-12,1.,-7.04084534450278E-17));
#117596=DIRECTION('',(-0.866025403784438,0.500000000000001,-1.88658882409001E-17));
#117597=DIRECTION('center_axis',(-1.88658882409001E-17,-7.04084534449554E-17,
-1.));
#117598=DIRECTION('ref_axis',(8.89395021849247E-34,1.,-7.04084534449554E-17));
#117599=DIRECTION('center_axis',(0.500000000000001,0.866025403784438,-7.04084534449554E-17));
#117600=DIRECTION('ref_axis',(1.88658882409001E-17,7.04084534449554E-17,
1.));
#117601=DIRECTION('center_axis',(0.500000000000022,0.866025403784426,2.2605474342613E-14));
#117602=DIRECTION('ref_axis',(0.757470380563718,-0.437325728121644,-0.484752338923218));
#117603=DIRECTION('',(-0.458928260426596,0.264962354696016,0.848044693619246));
#117604=DIRECTION('',(0.866025403784438,-0.500000000000001,1.88658882409001E-17));
#117605=DIRECTION('',(-0.458927806396615,0.264962092561696,-0.848045021223118));
#117606=DIRECTION('center_axis',(0.500000000000048,0.866025403784411,-7.41569998473607E-14));
#117607=DIRECTION('ref_axis',(0.757468756513884,-0.437324790476036,0.484755722545285));
#117608=DIRECTION('',(-0.866025403784438,0.500000000000001,1.2195101864901E-16));
#117609=DIRECTION('',(-0.433017043030787,0.250002506357517,0.866022509672719));
#117610=DIRECTION('center_axis',(-0.499999180015722,-0.866025877200512,
1.63998882624894E-6));
#117611=DIRECTION('ref_axis',(0.750040644539098,-0.433036167835282,-0.499918702276589));
#117612=DIRECTION('',(-0.866025403784438,0.500000000000001,1.2195101864901E-16));
#117613=DIRECTION('center_axis',(-0.500000820059934,-0.866024930320544,
1.64014408122753E-6));
#117614=DIRECTION('ref_axis',(0.750015485167091,-0.433021642322871,0.499969028330332));
#117615=DIRECTION('',(-0.4330171786346,0.25000258464842,-0.866022419268947));
#117616=DIRECTION('',(-0.866025403784438,0.500000000000001,1.2195101864901E-16));
#117617=DIRECTION('center_axis',(0.500000000000001,0.866025403784438,-7.04084534449554E-17));
#117618=DIRECTION('ref_axis',(1.88658882409001E-17,7.04084534449554E-17,
1.));
#117619=DIRECTION('center_axis',(-0.499999999999992,-0.866025403784443,
-4.38325761128318E-14));
#117620=DIRECTION('ref_axis',(0.757468756499917,-0.437324790467973,0.484755722574385));
#117621=DIRECTION('',(0.458927806396625,-0.264962092561694,0.848045021223113));
#117622=DIRECTION('',(-0.866025403784438,0.500000000000001,-1.88658882409001E-17));
#117623=DIRECTION('',(0.458928260426603,-0.264962354696039,-0.848044693619235));
#117624=DIRECTION('center_axis',(-0.50000000000002,-0.866025403784427,-6.68515552287977E-14));
#117625=DIRECTION('ref_axis',(0.757470380581235,-0.437325728131731,-0.484752338886745));
#117626=DIRECTION('',(0.866025403784438,-0.500000000000001,-1.2195101864901E-16));
#117627=DIRECTION('',(0.433017178634607,-0.250002584648424,0.866022419268943));
#117628=DIRECTION('center_axis',(0.499999179825101,0.866025877310566,1.64037044197607E-6));
#117629=DIRECTION('ref_axis',(0.750040733470373,-0.433036219179497,0.499918524375674));
#117630=DIRECTION('',(0.866025403784438,-0.500000000000001,-1.2195101864901E-16));
#117631=DIRECTION('center_axis',(0.500000819876834,0.866024930426258,1.63977752249215E-6));
#117632=DIRECTION('ref_axis',(0.750015393194705,-0.433021589222314,-0.49996921229049));
#117633=DIRECTION('',(0.433017043030727,-0.250002506357485,-0.866022509672758));
#117634=DIRECTION('',(0.866025403784438,-0.500000000000001,-1.2195101864901E-16));
#117635=DIRECTION('center_axis',(-2.68936361206584E-17,-8.27701011433319E-17,
-1.));
#117636=DIRECTION('ref_axis',(0.,1.,-8.27701011433319E-17));
#117637=DIRECTION('',(0.809016994374947,-0.587785252292474,2.68936361206584E-17));
#117638=DIRECTION('center_axis',(2.68936361206584E-17,8.27701011433319E-17,
1.));
#117639=DIRECTION('ref_axis',(7.43345068374082E-34,1.,-8.27701011433319E-17));
#117640=DIRECTION('',(-0.809016994374947,0.587785252292474,-2.68936361206584E-17));
#117641=DIRECTION('center_axis',(-2.68936361206584E-17,-8.27701011433319E-17,
-1.));
#117642=DIRECTION('ref_axis',(9.35397677642635E-34,1.,-8.27701011433319E-17));
#117643=DIRECTION('center_axis',(0.587785252292474,0.809016994374947,-8.27701011433319E-17));
#117644=DIRECTION('ref_axis',(2.68936361206584E-17,8.27701011433319E-17,
1.));
#117645=DIRECTION('center_axis',(0.587785252292476,0.809016994374946,-3.44595645466632E-14));
#117646=DIRECTION('ref_axis',(0.707607892255973,-0.514107226876224,-0.48475233892236));
#117647=DIRECTION('',(-0.428718095637389,0.311481929006018,0.848044693619234));
#117648=DIRECTION('',(0.809016994374947,-0.587785252292474,2.68936361206584E-17));
#117649=DIRECTION('',(-0.42871767149514,0.311481620848648,-0.848045021223098));
#117650=DIRECTION('center_axis',(0.587785252292473,0.809016994374947,-1.4335182126627E-14));
#117651=DIRECTION('ref_axis',(0.707606375113141,-0.514106124607403,0.484755722545282));
#117652=DIRECTION('',(-0.809016994374947,0.587785252292474,1.13923270769252E-16));
#117653=DIRECTION('',(-0.404512552559106,0.293895572546189,0.866022509672736));
#117654=DIRECTION('center_axis',(-0.587784486285654,-0.809017550909262,
1.63998874706822E-6));
#117655=DIRECTION('ref_axis',(0.700667238248267,-0.509064546361347,-0.499918702274142));
#117656=DIRECTION('',(-0.809016994374947,0.587785252292474,1.13923270769252E-16));
#117657=DIRECTION('center_axis',(-0.587786018369519,-0.809016437785177,
1.64014399705464E-6));
#117658=DIRECTION('ref_axis',(0.70064373503004,-0.509047470549678,0.499969028330886));
#117659=DIRECTION('',(-0.404512679236429,0.29389566458273,-0.866022419268948));
#117660=DIRECTION('',(-0.809016994374947,0.587785252292474,1.13923270769252E-16));
#117661=DIRECTION('center_axis',(0.587785252292474,0.809016994374947,-8.27701011433319E-17));
#117662=DIRECTION('ref_axis',(2.68936361206584E-17,8.27701011433319E-17,
1.));
#117663=DIRECTION('center_axis',(-0.587785252292488,-0.809016994374937,
3.80433679469878E-14));
#117664=DIRECTION('ref_axis',(0.707606375100347,-0.514106124598112,0.484755722573811));
#117665=DIRECTION('',(0.428717671495134,-0.311481620848637,0.848045021223105));
#117666=DIRECTION('',(-0.809016994374947,0.587785252292474,-2.68936361206584E-17));
#117667=DIRECTION('',(0.428718095637378,-0.311481929006026,-0.848044693619237));
#117668=DIRECTION('center_axis',(-0.587785252292439,-0.809016994374972,
4.05244479118913E-14));
#117669=DIRECTION('ref_axis',(0.707607892271159,-0.514107226887212,-0.484752338888539));
#117670=DIRECTION('',(0.809016994374947,-0.587785252292474,-1.13923270769252E-16));
#117671=DIRECTION('',(0.404512679236463,-0.293895664582694,0.866022419268944));
#117672=DIRECTION('center_axis',(0.587784486107514,0.809017551038687,1.64037051564877E-6));
#117673=DIRECTION('ref_axis',(0.700667321323678,-0.509064606718872,0.499918524376984));
#117674=DIRECTION('',(0.809016994374947,-0.587785252292474,-1.13923270769252E-16));
#117675=DIRECTION('center_axis',(0.587786018198527,0.809016437909411,1.63977755536976E-6));
#117676=DIRECTION('ref_axis',(0.700643649105069,-0.509047408121237,-0.499969212305901));
#117677=DIRECTION('',(0.404512552559087,-0.293895572546175,-0.86602250967275));
#117678=DIRECTION('',(0.809016994374947,-0.587785252292474,-1.13923270769252E-16));
#117679=DIRECTION('center_axis',(-3.61695511949416E-17,-9.42249022928248E-17,
-1.));
#117680=DIRECTION('ref_axis',(0.,1.,-9.42249022928248E-17));
#117681=DIRECTION('',(0.743144825477393,-0.669130606358859,3.61695511949416E-17));
#117682=DIRECTION('center_axis',(3.61695511949416E-17,9.42249022928248E-17,
1.));
#117683=DIRECTION('ref_axis',(5.85418057251285E-34,1.,-9.42249022928248E-17));
#117684=DIRECTION('',(-0.743144825477393,0.669130606358859,-3.61695511949416E-17));
#117685=DIRECTION('center_axis',(-3.61695511949416E-17,-9.42249022928248E-17,
-1.));
#117686=DIRECTION('ref_axis',(8.43711753644579E-34,1.,-9.42249022928248E-17));
#117687=DIRECTION('center_axis',(0.669130606358859,0.743144825477393,-9.42249022928248E-17));
#117688=DIRECTION('ref_axis',(3.61695511949416E-17,9.42249022928248E-17,
1.));
#117689=DIRECTION('center_axis',(0.669130606358863,0.74314482547739,-2.5362239506344E-14));
#117690=DIRECTION('ref_axis',(0.649992703803064,-0.585256059268391,-0.484752338924131));
#117691=DIRECTION('',(-0.393810805677316,0.354588842120037,0.848044693619242));
#117692=DIRECTION('',(0.743144825477393,-0.669130606358859,3.61695511949416E-17));
#117693=DIRECTION('',(-0.393810416069769,0.354588491315839,-0.848045021223114));
#117694=DIRECTION('center_axis',(0.669130606358859,0.743144825477393,-4.13514869037259E-15));
#117695=DIRECTION('ref_axis',(0.649991310191181,-0.58525480445459,0.484755722543604));
#117696=DIRECTION('',(-0.743144825477393,0.669130606358859,1.04647355694969E-16));
#117697=DIRECTION('',(-0.371576137911905,0.334568657340474,0.866022509672737));
#117698=DIRECTION('center_axis',(-0.669129902721926,-0.743145459032521,
1.63998881471712E-6));
#117699=DIRECTION('ref_axis',(0.643617175073679,-0.579515507191499,-0.499918702265435));
#117700=DIRECTION('',(-0.743144825477393,0.669130606358859,1.04647355694969E-16));
#117701=DIRECTION('center_axis',(-0.669131310059734,-0.743144191859866,
1.64014392166056E-6));
#117702=DIRECTION('ref_axis',(0.643595585510885,-0.57949606816224,0.499969028336162));
#117703=DIRECTION('',(-0.371576254274916,0.334568762114208,-0.866022419268918));
#117704=DIRECTION('',(-0.743144825477393,0.669130606358859,1.04647355694969E-16));
#117705=DIRECTION('center_axis',(0.669130606358859,0.743144825477393,-9.42249022928248E-17));
#117706=DIRECTION('ref_axis',(3.61695511949416E-17,9.42249022928248E-17,
1.));
#117707=DIRECTION('center_axis',(-0.669130606358832,-0.743144825477418,
-7.1675910624755E-15));
#117708=DIRECTION('ref_axis',(0.649991310178681,-0.585254804443299,0.484755722573996));
#117709=DIRECTION('',(0.393810416069767,-0.35458849131585,0.848045021223111));
#117710=DIRECTION('',(-0.743144825477393,0.669130606358859,-3.61695511949416E-17));
#117711=DIRECTION('',(0.39381080567732,-0.354588842120049,-0.848044693619236));
#117712=DIRECTION('center_axis',(-0.669130606358823,-0.743144825477425,
4.43839191415929E-14));
#117713=DIRECTION('ref_axis',(0.649992703817898,-0.585256059281697,-0.484752338888176));
#117714=DIRECTION('',(0.743144825477393,-0.669130606358859,-1.04647355694969E-16));
#117715=DIRECTION('',(0.371576254274913,-0.334568762114135,0.866022419268947));
#117716=DIRECTION('center_axis',(0.669129902558282,0.743145459179866,1.64037065800196E-6));
#117717=DIRECTION('ref_axis',(0.6436172513831,-0.579515575900527,0.499918524372467));
#117718=DIRECTION('',(0.743144825477393,-0.669130606358859,-1.04647355694969E-16));
#117719=DIRECTION('center_axis',(0.669131309902781,0.743144192001188,1.63977770340336E-6));
#117720=DIRECTION('ref_axis',(0.643595506584037,-0.579495997095898,-0.499969212306785));
#117721=DIRECTION('',(0.3715761379119,-0.334568657340403,-0.866022509672767));
#117722=DIRECTION('',(0.743144825477393,-0.669130606358859,-1.04647355694969E-16));
#117723=DIRECTION('center_axis',(-4.6592004597086E-17,-1.04647355694969E-16,
-1.));
#117724=DIRECTION('ref_axis',(0.,1.,-1.04647355694969E-16));
#117725=DIRECTION('',(0.669130606358857,-0.743144825477395,4.6592004597086E-17));
#117726=DIRECTION('center_axis',(4.6592004597086E-17,1.04647355694969E-16,
1.));
#117727=DIRECTION('ref_axis',(3.5473846082823E-12,1.,-1.04647355695134E-16));
#117728=DIRECTION('',(-0.669130606358857,0.743144825477395,-4.6592004597086E-17));
#117729=DIRECTION('center_axis',(-4.6592004597086E-17,-1.04647355694969E-16,
-1.));
#117730=DIRECTION('ref_axis',(6.01228899222931E-34,1.,-1.04647355694969E-16));
#117731=DIRECTION('center_axis',(0.743144825477395,0.669130606358857,-1.04647355694969E-16));
#117732=DIRECTION('ref_axis',(4.6592004597086E-17,1.04647355694969E-16,
1.));
#117733=DIRECTION('center_axis',(0.74314482547737,0.669130606358885,-7.77407776172683E-14));
#117734=DIRECTION('ref_axis',(0.585256059269616,-0.64999270380446,-0.484752338920781));
#117735=DIRECTION('',(-0.354588842120056,0.393810805677302,0.848044693619241));
#117736=DIRECTION('',(0.669130606358857,-0.743144825477395,4.6592004597086E-17));
#117737=DIRECTION('',(-0.354588491315837,0.393810416069767,-0.848045021223116));
#117738=DIRECTION('center_axis',(0.743144825477371,0.669130606358884,3.94217508482209E-14));
#117739=DIRECTION('ref_axis',(0.585254804454593,-0.649991310191166,0.48475572254362));
#117740=DIRECTION('',(-0.669130606358857,0.743144825477395,9.42249022928245E-17));
#117741=DIRECTION('',(-0.33456865734047,0.371576137911935,0.866022509672725));
#117742=DIRECTION('center_axis',(-0.743144191919671,-0.669131309993315,
1.63998871109189E-6));
#117743=DIRECTION('ref_axis',(0.579515507438012,-0.643617174849089,-0.49991870226882));
#117744=DIRECTION('',(-0.669130606358857,0.743144825477395,9.42249022928245E-17));
#117745=DIRECTION('center_axis',(-0.743145459092338,-0.669129902655492,
1.64014408828484E-6));
#117746=DIRECTION('ref_axis',(0.579496068078453,-0.643595585586683,0.499969028335704));
#117747=DIRECTION('',(-0.334568762114167,0.371576254274909,-0.866022419268937));
#117748=DIRECTION('',(-0.669130606358857,0.743144825477395,9.42249022928245E-17));
#117749=DIRECTION('center_axis',(0.743144825477395,0.669130606358857,-1.04647355694969E-16));
#117750=DIRECTION('ref_axis',(4.6592004597086E-17,1.04647355694969E-16,
1.));
#117751=DIRECTION('center_axis',(-0.743144825477388,-0.669130606358865,
3.17028066224897E-14));
#117752=DIRECTION('ref_axis',(0.585254804443526,-0.649991310178857,0.484755722573486));
#117753=DIRECTION('',(0.354588491315847,-0.39381041606979,0.848045021223102));
#117754=DIRECTION('',(-0.669130606358857,0.743144825477395,-4.6592004597086E-17));
#117755=DIRECTION('',(0.354588842120031,-0.393810805677317,-0.848044693619244));
#117756=DIRECTION('center_axis',(-0.743144825477382,-0.669130606358872,
2.12270917633713E-14));
#117757=DIRECTION('ref_axis',(0.585256059282123,-0.649992703818332,-0.48475233888708));
#117758=DIRECTION('',(0.669130606358857,-0.743144825477395,-9.42249022928245E-17));
#117759=DIRECTION('',(0.334568762114171,-0.371576254274878,0.866022419268948));
#117760=DIRECTION('center_axis',(0.743144191772357,0.669131310156922,1.64037043440206E-6));
#117761=DIRECTION('ref_axis',(0.579515576147011,-0.643617251157822,0.49991852437677));
#117762=DIRECTION('',(0.669130606358857,-0.743144825477395,-9.42249022928245E-17));
#117763=DIRECTION('center_axis',(0.743145458950911,0.669129902812563,1.63977758704219E-6));
#117764=DIRECTION('ref_axis',(0.579495997015134,-0.643595506662556,-0.499969212299321));
#117765=DIRECTION('',(0.334568657340475,-0.371576137911903,-0.866022509672737));
#117766=DIRECTION('',(0.669130606358857,-0.743144825477395,-9.42249022928245E-17));
#117767=DIRECTION('center_axis',(-5.8046805746579E-17,-1.13923270769252E-16,
-1.));
#117768=DIRECTION('ref_axis',(0.,1.,-1.13923270769252E-16));
#117769=DIRECTION('',(0.587785252292471,-0.809016994374949,5.8046805746579E-17));
#117770=DIRECTION('center_axis',(5.8046805746579E-17,1.13923270769252E-16,
1.));
#117771=DIRECTION('ref_axis',(-2.03917556295434E-34,1.,-1.13923270769252E-16));
#117772=DIRECTION('',(-0.587785252292471,0.809016994374949,-5.8046805746579E-17));
#117773=DIRECTION('center_axis',(-5.8046805746579E-17,-1.13923270769252E-16,
-1.));
#117774=DIRECTION('ref_axis',(2.10605807273539E-34,1.,-1.13923270769252E-16));
#117775=DIRECTION('center_axis',(0.809016994374949,0.587785252292471,-1.13923270769252E-16));
#117776=DIRECTION('ref_axis',(5.8046805746579E-17,1.13923270769252E-16,
1.));
#117777=DIRECTION('center_axis',(0.809016994374928,0.5877852522925,-5.84434214711463E-14));
#117778=DIRECTION('ref_axis',(0.51410722687612,-0.707607892255862,-0.484752338922631));
#117779=DIRECTION('',(-0.311481929006011,0.428718095637375,0.848044693619244));
#117780=DIRECTION('',(0.587785252292471,-0.809016994374949,5.8046805746579E-17));
#117781=DIRECTION('',(-0.311481620848643,0.42871767149512,-0.84804502122311));
#117782=DIRECTION('center_axis',(0.809016994374939,0.587785252292485,3.91460742688633E-14));
#117783=DIRECTION('ref_axis',(0.514106124608326,-0.707606375114411,0.484755722542449));
#117784=DIRECTION('',(-0.587785252292471,0.809016994374949,8.27701011433315E-17));
#117785=DIRECTION('',(-0.293895572546222,0.404512552559057,0.866022509672748));
#117786=DIRECTION('center_axis',(-0.809016437837695,-0.587786018297235,
1.63998885723267E-6));
#117787=DIRECTION('ref_axis',(0.509064546631475,-0.70066723805277,-0.499918702273074));
#117788=DIRECTION('',(-0.587785252292471,0.809016994374949,8.27701011433315E-17));
#117789=DIRECTION('center_axis',(-0.809017550961851,-0.587784486213271,
1.64014409551461E-6));
#117790=DIRECTION('ref_axis',(0.509047470457721,-0.700643735095713,0.49996902833248));
#117791=DIRECTION('',(-0.293895664582671,0.404512679236479,-0.866022419268945));
#117792=DIRECTION('',(-0.587785252292471,0.809016994374949,8.27701011433315E-17));
#117793=DIRECTION('center_axis',(0.809016994374949,0.587785252292471,-1.13923270769252E-16));
#117794=DIRECTION('ref_axis',(5.8046805746579E-17,1.13923270769252E-16,
1.));
#117795=DIRECTION('center_axis',(-0.809016994374936,-0.587785252292489,
-1.90216839734942E-14));
#117796=DIRECTION('ref_axis',(0.514106124597937,-0.707606375100088,0.484755722574375));
#117797=DIRECTION('',(0.311481620848639,-0.428717671495141,0.8480450212231));
#117798=DIRECTION('',(-0.587785252292471,0.809016994374949,-5.8046805746579E-17));
#117799=DIRECTION('',(0.311481929006024,-0.428718095637357,-0.848044693619248));
#117800=DIRECTION('center_axis',(-0.809016994374946,-0.587785252292474,
-1.47486936277963E-14));
#117801=DIRECTION('ref_axis',(0.514107226887618,-0.707607892271675,-0.484752338887354));
#117802=DIRECTION('',(0.587785252292471,-0.809016994374949,-8.27701011433315E-17));
#117803=DIRECTION('',(0.29389566458269,-0.404512679236492,0.866022419268932));
#117804=DIRECTION('center_axis',(0.809016437708314,0.587786018475311,1.64037048466487E-6));
#117805=DIRECTION('ref_axis',(0.509064606988954,-0.700667321127302,0.499918524377196));
#117806=DIRECTION('',(0.587785252292471,-0.809016994374949,-8.27701011433315E-17));
#117807=DIRECTION('center_axis',(0.809017550837583,0.587784486384312,1.63977753368073E-6));
#117808=DIRECTION('ref_axis',(0.509047408033278,-0.700643649175448,-0.499969212296831));
#117809=DIRECTION('',(0.293895572546198,-0.404512552559071,-0.866022509672749));
#117810=DIRECTION('',(0.587785252292471,-0.809016994374949,-8.27701011433315E-17));
#117811=DIRECTION('center_axis',(-7.04084534449555E-17,-1.21951018649011E-16,
-1.));
#117812=DIRECTION('ref_axis',(0.,1.,-1.21951018649011E-16));
#117813=DIRECTION('',(0.499999999999998,-0.86602540378444,7.04084534449555E-17));
#117814=DIRECTION('center_axis',(7.04084534449556E-17,1.21951018649011E-16,
1.));
#117815=DIRECTION('ref_axis',(-8.12565151756264E-34,1.,-1.21951018649011E-16));
#117816=DIRECTION('',(-0.499999999999998,0.86602540378444,-7.04084534449555E-17));
#117817=DIRECTION('center_axis',(-7.04084534449556E-17,-1.21951018649011E-16,
-1.));
#117818=DIRECTION('ref_axis',(-3.09764893063087E-34,1.,-1.21951018649011E-16));
#117819=DIRECTION('center_axis',(0.86602540378444,0.499999999999998,-1.21951018649011E-16));
#117820=DIRECTION('ref_axis',(7.04084534449555E-17,1.21951018649011E-16,
1.));
#117821=DIRECTION('center_axis',(0.866025403784438,0.500000000000001,3.85947122922661E-15));
#117822=DIRECTION('ref_axis',(0.437325728121527,-0.757470380563533,-0.484752338923613));
#117823=DIRECTION('',(-0.264962354696013,0.458928260426604,0.848044693619243));
#117824=DIRECTION('',(0.499999999999998,-0.86602540378444,7.04084534449555E-17));
#117825=DIRECTION('',(-0.264962092561699,0.458927806396622,-0.848045021223113));
#117826=DIRECTION('center_axis',(0.866025403784433,0.50000000000001,2.81190110945387E-14));
#117827=DIRECTION('ref_axis',(0.437324790476745,-0.757468756515143,0.484755722542679));
#117828=DIRECTION('',(-0.499999999999998,0.86602540378444,7.04084534449549E-17));
#117829=DIRECTION('',(-0.250002506357482,0.433017043030748,0.866022509672748));
#117830=DIRECTION('center_axis',(-0.86602493036527,-0.500000819982468,1.63998884690466E-6));
#117831=DIRECTION('ref_axis',(0.433036168127082,-0.750040644377634,-0.499918702266075));
#117832=DIRECTION('',(-0.499999999999998,0.86602540378444,7.04084534449549E-17));
#117833=DIRECTION('center_axis',(-0.866025877245222,-0.499999179938281,
1.64014409947301E-6));
#117834=DIRECTION('ref_axis',(0.433021642224044,-0.750015485221962,0.499969028333613));
#117835=DIRECTION('',(-0.25000258464842,0.4330171786346,-0.866022419268947));
#117836=DIRECTION('',(-0.499999999999998,0.86602540378444,7.04084534449549E-17));
#117837=DIRECTION('center_axis',(0.86602540378444,0.499999999999998,-1.21951018649011E-16));
#117838=DIRECTION('ref_axis',(7.04084534449555E-17,1.21951018649011E-16,
1.));
#117839=DIRECTION('center_axis',(-0.866025403784437,-0.500000000000003,
4.96217842786824E-15));
#117840=DIRECTION('ref_axis',(0.437324790468618,-0.757468756501049,0.484755722572034));
#117841=DIRECTION('',(0.264962092561697,-0.458927806396632,0.848045021223108));
#117842=DIRECTION('',(-0.499999999999998,0.86602540378444,-7.04084534449555E-17));
#117843=DIRECTION('',(0.264962354696018,-0.4589282604266,-0.848044693619243));
#117844=DIRECTION('center_axis',(-0.866025403784433,-0.500000000000011,
3.28055054524852E-14));
#117845=DIRECTION('ref_axis',(0.437325728131414,-0.757470380580673,-0.484752338887911));
#117846=DIRECTION('',(0.499999999999998,-0.86602540378444,-7.04084534449549E-17));
#117847=DIRECTION('',(0.250002584648412,-0.433017178634587,0.866022419268956));
#117848=DIRECTION('center_axis',(0.866024930255237,0.500000820173048,1.64037033731929E-6));
#117849=DIRECTION('ref_axis',(0.433036219468869,-0.750040733303686,0.4999185243751));
#117850=DIRECTION('',(0.499999999999998,-0.86602540378444,-7.04084534449549E-17));
#117851=DIRECTION('center_axis',(0.866025877139543,0.499999180121325,1.63977763420594E-6));
#117852=DIRECTION('ref_axis',(0.433021589122406,-0.75001539324677,-0.499969212298916));
#117853=DIRECTION('',(0.250002506357476,-0.433017043030742,-0.866022509672753));
#117854=DIRECTION('',(0.499999999999998,-0.86602540378444,-7.04084534449549E-17));
#117855=DIRECTION('center_axis',(-8.35415108931911E-17,-1.28642645648559E-16,
-1.));
#117856=DIRECTION('ref_axis',(0.,1.,-1.28642645648559E-16));
#117857=DIRECTION('',(0.406736643075798,-0.913545457642602,8.35415108931911E-17));
#117858=DIRECTION('center_axis',(8.35415108931911E-17,1.28642645648559E-16,
1.));
#117859=DIRECTION('ref_axis',(-1.52315888917702E-33,1.,-1.28642645648559E-16));
#117860=DIRECTION('',(-0.406736643075798,0.913545457642602,-8.35415108931911E-17));
#117861=DIRECTION('center_axis',(-8.35415108931911E-17,-1.28642645648559E-16,
-1.));
#117862=DIRECTION('ref_axis',(-9.26572950507683E-34,1.,-1.28642645648559E-16));
#117863=DIRECTION('center_axis',(0.913545457642602,0.406736643075798,-1.28642645648559E-16));
#117864=DIRECTION('ref_axis',(8.35415108931911E-17,1.28642645648559E-16,
1.));
#117865=DIRECTION('center_axis',(0.913545457642591,0.406736643075822,-2.2329797826238E-14));
#117866=DIRECTION('ref_axis',(0.35575279717394,-0.799033864871932,-0.484752338922403));
#117867=DIRECTION('',(-0.215539797381028,0.48411031115768,0.848044693619245));
#117868=DIRECTION('',(0.406736643075798,-0.913545457642602,8.35415108931911E-17));
#117869=DIRECTION('',(-0.215539584141775,0.484109832214432,-0.84804502122311));
#117870=DIRECTION('center_axis',(0.913545457642603,0.406736643075797,-9.64868027753777E-16));
#117871=DIRECTION('ref_axis',(0.355752034424016,-0.799032151707585,0.484755722545614));
#117872=DIRECTION('',(-0.406736643075798,0.913545457642602,5.72753959967194E-17));
#117873=DIRECTION('',(-0.203370360392779,0.456777308164345,0.866022509672725));
#117874=DIRECTION('center_axis',(-0.913545072528371,-0.406737508052115,
1.63998885654379E-6));
#117875=DIRECTION('ref_axis',(0.352263354743201,-0.791196448442204,-0.499918702268187));
#117876=DIRECTION('',(-0.406736643075798,0.913545457642602,5.72753959967194E-17));
#117877=DIRECTION('center_axis',(-0.913545842789927,-0.406735778016334,
1.64014409086703E-6));
#117878=DIRECTION('ref_axis',(0.352251538262375,-0.791169908740555,0.499969028336008));
#117879=DIRECTION('',(-0.203370424080352,0.456777451208921,-0.866022419268959));
#117880=DIRECTION('',(-0.406736643075798,0.913545457642602,5.72753959967194E-17));
#117881=DIRECTION('center_axis',(0.913545457642602,0.406736643075798,-1.28642645648559E-16));
#117882=DIRECTION('ref_axis',(8.35415108931911E-17,1.28642645648559E-16,
1.));
#117883=DIRECTION('center_axis',(-0.913545457642604,-0.406736643075794,
2.75676579326004E-15));
#117884=DIRECTION('ref_axis',(0.355752034417364,-0.79903215169265,0.484755722575115));
#117885=DIRECTION('',(0.215539584141774,-0.484109832214442,0.848045021223105));
#117886=DIRECTION('',(-0.406736643075798,0.913545457642602,-8.35415108931911E-17));
#117887=DIRECTION('',(0.215539797381044,-0.484110311157686,-0.848044693619238));
#117888=DIRECTION('center_axis',(-0.913545457642585,-0.406736643075836,
6.54731726467594E-14));
#117889=DIRECTION('ref_axis',(0.355752797181805,-0.799033864889616,-0.484752338887483));
#117890=DIRECTION('',(0.406736643075798,-0.913545457642602,-5.72753959967194E-17));
#117891=DIRECTION('',(0.203370424080343,-0.456777451208935,0.866022419268953));
#117892=DIRECTION('center_axis',(0.91354507243885,0.40673750825318,1.64037042149229E-6));
#117893=DIRECTION('ref_axis',(0.352263396508779,-0.791196542248603,0.499918524375676));
#117894=DIRECTION('',(0.406736643075798,-0.913545457642602,-5.72753959967194E-17));
#117895=DIRECTION('center_axis',(0.913545842703946,0.406735778209453,1.63977757396033E-6));
#117896=DIRECTION('ref_axis',(0.352251495066729,-0.791169811720976,-0.499969212296767));
#117897=DIRECTION('',(0.203370360392771,-0.456777308164288,-0.866022509672757));
#117898=DIRECTION('',(0.406736643075798,-0.913545457642602,-5.72753959967194E-17));
#117899=DIRECTION('center_axis',(-9.73020895656139E-17,-1.33924836902177E-16,
-1.));
#117900=DIRECTION('ref_axis',(0.,1.,-1.33924836902177E-16));
#117901=DIRECTION('',(0.309016994374945,-0.951056516295154,9.73020895656138E-17));
#117902=DIRECTION('center_axis',(9.73020895656139E-17,1.33924836902177E-16,
1.));
#117903=DIRECTION('ref_axis',(-2.28801495776546E-33,1.,-1.33924836902177E-16));
#117904=DIRECTION('',(-0.309016994374945,0.951056516295154,-9.73020895656139E-17));
#117905=DIRECTION('center_axis',(-9.73020895656139E-17,-1.33924836902177E-16,
-1.));
#117906=DIRECTION('ref_axis',(-1.59316208980373E-33,1.,-1.33924836902177E-16));
#117907=DIRECTION('center_axis',(0.951056516295154,0.309016994374945,-1.33924836902177E-16));
#117908=DIRECTION('ref_axis',(9.73020895656139E-17,1.33924836902177E-16,
1.));
#117909=DIRECTION('center_axis',(0.95105651629516,0.309016994374929,2.49487247317848E-14));
#117910=DIRECTION('ref_axis',(0.270282164134087,-0.831842966947593,-0.484752338922485));
#117911=DIRECTION('',(-0.163755740941348,0.503988348013118,0.848044693619245));
#117912=DIRECTION('',(0.309016994374945,-0.951056516295154,9.73020895656139E-17));
#117913=DIRECTION('',(-0.163755578933429,0.503987849403997,-0.848045021223114));
#117914=DIRECTION('center_axis',(0.951056516295162,0.309016994374921,-3.08757768881175E-14));
#117915=DIRECTION('ref_axis',(0.270281584637474,-0.831841183440424,0.484755722543109));
#117916=DIRECTION('',(-0.309016994374945,0.951056516295154,4.35148173242966E-17));
#117917=DIRECTION('',(-0.15451004620159,0.475533025522823,0.866022509672753));
#117918=DIRECTION('center_axis',(-0.951056223705264,-0.309017894868233,
1.63998886704514E-6));
#117919=DIRECTION('ref_axis',(0.267631070329452,-0.823683738650044,-0.499918702268478));
#117920=DIRECTION('',(-0.309016994374945,0.951056516295154,4.35148173242966E-17));
#117921=DIRECTION('center_axis',(-0.951056808909262,-0.309016093795519,
1.64014407072764E-6));
#117922=DIRECTION('ref_axis',(0.267622092735341,-0.823656109178821,0.499969028333118));
#117923=DIRECTION('',(-0.154510094588055,0.475533174441005,-0.866022419268954));
#117924=DIRECTION('',(-0.309016994374945,0.951056516295154,4.35148173242966E-17));
#117925=DIRECTION('center_axis',(0.951056516295154,0.309016994374945,-1.33924836902177E-16));
#117926=DIRECTION('ref_axis',(9.73020895656139E-17,1.33924836902177E-16,
1.));
#117927=DIRECTION('center_axis',(-0.951056516295147,-0.309016994374967,
-3.33568660984481E-14));
#117928=DIRECTION('ref_axis',(0.270281584632006,-0.83184118342356,0.484755722575096));
#117929=DIRECTION('',(0.16375557893343,-0.503987849404013,0.848045021223104));
#117930=DIRECTION('',(-0.309016994374945,0.951056516295154,-9.73020895656139E-17));
#117931=DIRECTION('',(0.16375574094134,-0.503988348013128,-0.84804469361924));
#117932=DIRECTION('center_axis',(-0.951056516295154,-0.309016994374946,
-5.78920684455565E-15));
#117933=DIRECTION('ref_axis',(0.270282164139835,-0.831842966965265,-0.484752338888954));
#117934=DIRECTION('',(0.309016994374945,-0.951056516295154,-4.35148173242966E-17));
#117935=DIRECTION('',(0.154510094588053,-0.475533174441032,0.866022419268939));
#117936=DIRECTION('center_axis',(0.95105622363726,0.309017895077522,1.64037036907791E-6));
#117937=DIRECTION('ref_axis',(0.267631102060799,-0.823683836308256,0.499918524375959));
#117938=DIRECTION('',(0.309016994374945,-0.951056516295154,-4.35148173242966E-17));
#117939=DIRECTION('center_axis',(0.951056808843939,0.309016093996566,1.6397775629441E-6));
#117940=DIRECTION('ref_axis',(0.26762205991693,-0.823656008173377,-0.499969212297834));
#117941=DIRECTION('',(0.154510046201592,-0.475533025522835,-0.866022509672746));
#117942=DIRECTION('',(0.309016994374945,-0.951056516295154,-4.35148173242966E-17));
#117943=DIRECTION('center_axis',(-1.11539425682703E-16,-1.37739719617122E-16,
-1.));
#117944=DIRECTION('ref_axis',(0.,1.,-1.37739719617122E-16));
#117945=DIRECTION('',(0.207911690817756,-0.978147600733806,1.11539425682703E-16));
#117946=DIRECTION('center_axis',(1.11539425682703E-16,1.37739719617122E-16,
1.));
#117947=DIRECTION('ref_axis',(-3.0483093525691E-33,1.,-1.37739719617122E-16));
#117948=DIRECTION('',(-0.207911690817756,0.978147600733806,-1.11539425682703E-16));
#117949=DIRECTION('center_axis',(-1.11539425682703E-16,-1.37739719617122E-16,
-1.));
#117950=DIRECTION('ref_axis',(-2.25178493903976E-33,1.,-1.37739719617122E-16));
#117951=DIRECTION('center_axis',(0.978147600733806,0.207911690817756,-1.37739719617122E-16));
#117952=DIRECTION('ref_axis',(1.11539425682703E-16,1.37739719617122E-16,
1.));
#117953=DIRECTION('center_axis',(0.978147600733805,0.20791169081776,-2.48108864735987E-14));
#117954=DIRECTION('ref_axis',(0.181850263143634,-0.855538223402174,-0.484752338924158));
#117955=DIRECTION('',(-0.110177542335811,0.518344583061382,0.848044693619247));
#117956=DIRECTION('',(0.207911690817756,-0.978147600733806,1.11539425682703E-16));
#117957=DIRECTION('',(-0.110177433334228,0.518344070249267,-0.84804502122311));
#117958=DIRECTION('center_axis',(0.97814760073381,0.207911690817738,-2.55000835906321E-14));
#117959=DIRECTION('ref_axis',(0.181849873249065,-0.855536389092426,0.4847557225428));
#117960=DIRECTION('',(-0.207911690817756,0.978147600733806,2.92774812072079E-17));
#117961=DIRECTION('',(-0.103956887610938,0.489078703542067,0.866022509672732));
#117962=DIRECTION('center_axis',(-0.978147403873932,-0.207912616962023,
1.6399888759094E-6));
#117963=DIRECTION('ref_axis',(0.180066563904203,-0.84714657745219,-0.499918702265453));
#117964=DIRECTION('',(-0.207911690817756,0.978147600733806,2.92774812072079E-17));
#117965=DIRECTION('center_axis',(-0.978147797608757,-0.20791076458531,1.64014403328849E-6));
#117966=DIRECTION('ref_axis',(0.18006052355641,-0.847118160923773,0.499969028330471));
#117967=DIRECTION('',(-0.10395692016614,0.489078856702181,-0.866022419268957));
#117968=DIRECTION('',(-0.207911690817756,0.978147600733806,2.92774812072079E-17));
#117969=DIRECTION('center_axis',(0.978147600733806,0.207911690817756,-1.37739719617122E-16));
#117970=DIRECTION('ref_axis',(1.11539425682703E-16,1.37739719617122E-16,
1.));
#117971=DIRECTION('center_axis',(-0.978147600733803,-0.20791169081777,-9.51084198674744E-15));
#117972=DIRECTION('ref_axis',(0.181849873245419,-0.855536389075214,0.484755722574546));
#117973=DIRECTION('',(0.110177433334224,-0.518344070249276,0.848045021223105));
#117974=DIRECTION('',(-0.207911690817756,0.978147600733806,-1.11539425682703E-16));
#117975=DIRECTION('',(0.11017754233581,-0.518344583061379,-0.848044693619249));
#117976=DIRECTION('center_axis',(-0.978147600733808,-0.20791169081775,-3.85947122970341E-15));
#117977=DIRECTION('ref_axis',(0.18185026314786,-0.855538223422036,-0.484752338887519));
#117978=DIRECTION('',(0.207911690817756,-0.978147600733806,-2.92774812072079E-17));
#117979=DIRECTION('',(0.103956920166119,-0.489078856702202,0.866022419268949));
#117980=DIRECTION('center_axis',(0.978147403828174,0.207912617177293,1.64037041228311E-6));
#117981=DIRECTION('ref_axis',(0.180066585253765,-0.847146677892752,0.499918524372045));
#117982=DIRECTION('',(0.207911690817756,-0.978147600733806,-2.92774812072079E-17));
#117983=DIRECTION('center_axis',(0.978147797564809,0.207910764792073,1.63977756750503E-6));
#117984=DIRECTION('ref_axis',(0.180060501475011,-0.84711805703777,-0.499969212301239));
#117985=DIRECTION('',(0.103956887610919,-0.489078703542027,-0.866022509672757));
#117986=DIRECTION('',(0.207911690817756,-0.978147600733806,-2.92774812072079E-17));
#117987=DIRECTION('center_axis',(-1.26097532010604E-16,-1.40045497140051E-16,
-1.));
#117988=DIRECTION('ref_axis',(0.,1.,-1.40045497140051E-16));
#117989=DIRECTION('',(0.10452846326765,-0.994521895368274,1.26097532010604E-16));
#117990=DIRECTION('center_axis',(1.26097532010604E-16,1.40045497140051E-16,
1.));
#117991=DIRECTION('ref_axis',(-3.73692701101589E-33,1.,-1.40045497140052E-16));
#117992=DIRECTION('',(-0.10452846326765,0.994521895368274,-1.26097532010604E-16));
#117993=DIRECTION('center_axis',(-1.26097532010604E-16,-1.40045497140051E-16,
-1.));
#117994=DIRECTION('ref_axis',(-2.83644037037309E-33,1.,-1.40045497140051E-16));
#117995=DIRECTION('center_axis',(0.994521895368274,0.10452846326765,-1.40045497140051E-16));
#117996=DIRECTION('ref_axis',(1.26097532010604E-16,1.40045497140051E-16,
1.));
#117997=DIRECTION('center_axis',(0.994521895368275,0.10452846326764,2.23297978262382E-14));
#117998=DIRECTION('ref_axis',(0.091425972615977,-0.869860024050187,-0.48475233892229));
#117999=DIRECTION('',(-0.0553922155203048,0.527021726387063,0.848044693619241));
#118000=DIRECTION('',(0.10452846326765,-0.994521895368274,1.26097532010604E-16));
#118001=DIRECTION('',(-0.0553921607193106,0.5270212049904,-0.848045021223115));
#118002=DIRECTION('center_axis',(0.994521895368273,0.104528463267655,7.06421234605402E-15));
#118003=DIRECTION('ref_axis',(0.0914257765946829,-0.869858159032163,0.484755722544083));
#118004=DIRECTION('',(-0.10452846326765,0.994521895368274,1.47193748793061E-17));
#118005=DIRECTION('',(-0.0522647556052155,0.497265932938945,0.86602250967275));
#118006=DIRECTION('center_axis',(-0.994521796395255,-0.104529404915866,
1.63998885607056E-6));
#118007=DIRECTION('ref_axis',(0.0905292105227215,-0.86132790107118,-0.499918702269128));
#118008=DIRECTION('',(-0.10452846326765,0.994521895368274,1.47193748793061E-17));
#118009=DIRECTION('center_axis',(-0.994521994347068,-0.10452752153017,1.64014403010456E-6));
#118010=DIRECTION('ref_axis',(0.0905261736005623,-0.861299008822643,0.499969028335129));
#118011=DIRECTION('',(-0.0522647719724833,0.497266088663009,-0.866022419268957));
#118012=DIRECTION('',(-0.10452846326765,0.994521895368274,1.47193748793061E-17));
#118013=DIRECTION('center_axis',(0.994521895368274,0.10452846326765,-1.40045497140051E-16));
#118014=DIRECTION('ref_axis',(1.26097532010604E-16,1.40045497140051E-16,
1.));
#118015=DIRECTION('center_axis',(-0.994521895368273,-0.104528463267658,
-6.61623790382415E-15));
#118016=DIRECTION('ref_axis',(0.0914257765929248,-0.869858159015414,0.484755722574468));
#118017=DIRECTION('',(0.0553921607193095,-0.527021204990405,0.848045021223111));
#118018=DIRECTION('',(-0.10452846326765,0.994521895368274,-1.26097532010604E-16));
#118019=DIRECTION('',(0.0553922155203074,-0.52702172638707,-0.848044693619236));
#118020=DIRECTION('center_axis',(-0.994521895368274,-0.104528463267647,
-9.13178460599495E-15));
#118021=DIRECTION('ref_axis',(0.0914259726178967,-0.869860024068452,-0.484752338889152));
#118022=DIRECTION('',(0.10452846326765,-0.994521895368274,-1.47193748793061E-17));
#118023=DIRECTION('',(0.0522647719724736,-0.497266088663036,0.866022419268942));
#118024=DIRECTION('center_axis',(0.994521796372249,0.104529405134743,1.64037042463382E-6));
#118025=DIRECTION('ref_axis',(0.0905292212562927,-0.861328003191953,0.499918524377815));
#118026=DIRECTION('',(0.10452846326765,-0.994521895368274,-1.47193748793061E-17));
#118027=DIRECTION('center_axis',(0.994521994324975,0.104527521740383,1.63977756772086E-6));
#118028=DIRECTION('ref_axis',(0.0905261624998373,-0.861298903204019,-0.499969212294724));
#118029=DIRECTION('',(0.052264755605215,-0.497265932938933,-0.866022509672757));
#118030=DIRECTION('',(0.10452846326765,-0.994521895368274,-1.47193748793061E-17));
#118031=DIRECTION('center_axis',(-1.40816906889911E-16,-1.40816906889911E-16,
-1.));
#118032=DIRECTION('ref_axis',(-1.,-1.24216341050767E-48,1.40816906889911E-16));
#118033=DIRECTION('',(-3.49148133884313E-15,-1.,1.40816906889911E-16));
#118034=DIRECTION('center_axis',(1.40816906889911E-16,1.40816906889911E-16,
1.));
#118035=DIRECTION('ref_axis',(-1.,4.28176633132684E-33,1.40816906889911E-16));
#118036=DIRECTION('',(3.49148133884313E-15,1.,-1.40816906889911E-16));
#118037=DIRECTION('center_axis',(-1.40816906889911E-16,-1.40816906889911E-16,
-1.));
#118038=DIRECTION('ref_axis',(-1.,3.27616581394049E-33,1.40816906889911E-16));
#118039=DIRECTION('center_axis',(1.,-3.49148133884313E-15,-1.4081690688991E-16));
#118040=DIRECTION('ref_axis',(1.40816906889911E-16,1.40816906889911E-16,
1.));
#118041=DIRECTION('center_axis',(1.,-3.44043747061122E-15,-3.31073780200115E-16));
#118042=DIRECTION('ref_axis',(3.16967243309126E-15,0.87465145624295,0.484752338923792));
#118043=DIRECTION('',(1.96084725663077E-15,0.529924709392051,0.84804469361924));
#118044=DIRECTION('',(-3.49148133884313E-15,-1.,1.40816906889911E-16));
#118045=DIRECTION('',(1.75444295999834E-15,0.529924185123396,-0.84804502122311));
#118046=DIRECTION('center_axis',(1.,-3.58452992681196E-15,-2.19445148712539E-16));
#118047=DIRECTION('ref_axis',(3.02883030677949E-15,0.874649580953691,-0.484755722542326));
#118048=DIRECTION('',(3.49148133884313E-15,1.,-4.91659602599733E-31));
#118049=DIRECTION('',(1.92690513386533E-15,0.500005012715,0.866022509672741));
#118050=DIRECTION('center_axis',(-0.999999999998207,-9.468352603161E-7,
1.63998886905525E-6));
#118051=DIRECTION('ref_axis',(1.66718511939339E-10,-0.866072335961319,-0.499918702273184));
#118052=DIRECTION('',(3.49148133884313E-15,1.,-4.91659602599733E-31));
#118053=DIRECTION('center_axis',(-0.999999999998207,9.46924651316897E-7,
1.64014404046701E-6));
#118054=DIRECTION('ref_axis',(-5.65130098543586E-11,-0.866043284547351,
0.499969028331192));
#118055=DIRECTION('',(1.51399673284832E-15,0.50000516929684,-0.866022419268946));
#118056=DIRECTION('',(3.49148133884313E-15,1.,-4.91659602599733E-31));
#118057=DIRECTION('center_axis',(1.,-3.49148133884313E-15,-1.4081690688991E-16));
#118058=DIRECTION('ref_axis',(1.40816906889911E-16,1.40816906889911E-16,
1.));
#118059=DIRECTION('center_axis',(-1.,3.31723128487429E-15,-2.62780671920002E-16));
#118060=DIRECTION('ref_axis',(3.02879938767921E-15,0.87464958093635,-0.484755722573615));
#118061=DIRECTION('',(-1.70284169646898E-15,-0.529924185123411,0.8480450212231));
#118062=DIRECTION('',(3.49148133884313E-15,1.,-1.40816906889911E-16));
#118063=DIRECTION('',(-1.90924601303524E-15,-0.529924709392042,-0.848044693619246));
#118064=DIRECTION('center_axis',(-1.,3.24518402866523E-15,5.38039174125153E-16));
#118065=DIRECTION('ref_axis',(3.09922068458289E-15,0.874651456262602,0.484752338888334));
#118066=DIRECTION('',(-3.49148133884313E-15,-1.,4.91659602599733E-31));
#118067=DIRECTION('',(-1.65163279947087E-15,-0.500005169296866,0.866022419268931));
#118068=DIRECTION('center_axis',(0.999999999998206,9.47055346977043E-7,
1.64037042692596E-6));
#118069=DIRECTION('ref_axis',(1.66970631684952E-10,-0.866072438647882,0.499918524376234));
#118070=DIRECTION('',(-3.49148133884313E-15,-1.,4.91659602599733E-31));
#118071=DIRECTION('center_axis',(0.999999999998207,-9.46713286247913E-7,
1.63977758872445E-6));
#118072=DIRECTION('ref_axis',(-5.62740306604305E-11,-0.866043178344825,
-0.49996921229451));
#118073=DIRECTION('',(-1.92690513386536E-15,-0.500005012714974,-0.866022509672756));
#118074=DIRECTION('',(-3.49148133884313E-15,-1.,4.91659602599733E-31));
#118075=DIRECTION('center_axis',(-1.55536281769218E-16,-1.40045497140051E-16,
-1.));
#118076=DIRECTION('ref_axis',(-1.,3.43882990390064E-49,1.55536281769218E-16));
#118077=DIRECTION('',(-0.104528463267657,-0.994521895368273,1.55536281769218E-16));
#118078=DIRECTION('center_axis',(1.55536281769218E-16,1.40045497140051E-16,
1.));
#118079=DIRECTION('ref_axis',(-1.,6.31969253991851E-33,1.55536281769218E-16));
#118080=DIRECTION('',(0.104528463267657,0.994521895368273,-1.55536281769218E-16));
#118081=DIRECTION('center_axis',(-1.55536281769218E-16,-1.40045497140051E-16,
-1.));
#118082=DIRECTION('ref_axis',(-1.,5.31960080738412E-33,1.55536281769218E-16));
#118083=DIRECTION('center_axis',(0.994521895368273,-0.104528463267657,-1.40045497140051E-16));
#118084=DIRECTION('ref_axis',(1.55536281769218E-16,1.40045497140051E-16,
1.));
#118085=DIRECTION('center_axis',(0.994521895368273,-0.10452846326766,6.54731726386673E-15));
#118086=DIRECTION('ref_axis',(0.0914259726160302,0.869860024050657,0.484752338921436));
#118087=DIRECTION('',(0.055392215520309,0.52702172638707,0.848044693619236));
#118088=DIRECTION('',(-0.104528463267657,-0.994521895368273,1.55536281769218E-16));
#118089=DIRECTION('',(0.0553921607193155,0.527021204990399,-0.848045021223115));
#118090=DIRECTION('center_axis',(0.994521895368271,-0.104528463267675,-3.31156490954067E-14));
#118091=DIRECTION('ref_axis',(0.0914257765945625,0.869858159030975,-0.484755722546238));
#118092=DIRECTION('',(0.104528463267657,0.994521895368273,-1.47193748793071E-17));
#118093=DIRECTION('',(0.0522647556052243,0.497265932938944,0.866022509672749));
#118094=DIRECTION('center_axis',(-0.994521994337724,0.104527521619072,1.63998887332766E-6));
#118095=DIRECTION('ref_axis',(0.0905292101909773,0.861327901104786,0.499918702271301));
#118096=DIRECTION('',(0.104528463267657,0.994521895368273,-1.47193748793071E-17));
#118097=DIRECTION('center_axis',(-0.994521796385912,0.10452940500476,1.6401440452089E-6));
#118098=DIRECTION('ref_axis',(0.0905261737131933,0.861299008813,-0.499969028331347));
#118099=DIRECTION('',(0.0522647719724817,0.497266088662994,-0.866022419268966));
#118100=DIRECTION('',(0.104528463267657,0.994521895368273,-1.47193748793071E-17));
#118101=DIRECTION('center_axis',(0.994521895368273,-0.104528463267657,-1.40045497140051E-16));
#118102=DIRECTION('ref_axis',(1.55536281769218E-16,1.40045497140051E-16,
1.));
#118103=DIRECTION('center_axis',(-0.994521895368273,0.104528463267655,-3.51487638640649E-15));
#118104=DIRECTION('ref_axis',(0.0914257765928257,0.869858159014446,-0.484755722576225));
#118105=DIRECTION('',(-0.0553921607193145,-0.527021204990405,0.848045021223111));
#118106=DIRECTION('',(0.104528463267657,0.994521895368273,-1.55536281769218E-16));
#118107=DIRECTION('',(-0.0553922155203081,-0.527021726387063,-0.84804469361924));
#118108=DIRECTION('center_axis',(-0.994521895368272,0.104528463267671,-1.61615357743855E-14));
#118109=DIRECTION('ref_axis',(0.0914259726178233,0.869860024067671,0.484752338890568));
#118110=DIRECTION('',(-0.104528463267657,-0.994521895368273,1.47193748793071E-17));
#118111=DIRECTION('',(-0.0522647719724884,-0.497266088663051,0.866022419268933));
#118112=DIRECTION('center_axis',(0.99452199436073,-0.104527521400184,1.64037042497792E-6));
#118113=DIRECTION('ref_axis',(0.0905292209242248,0.861328003227316,-0.499918524377021));
#118114=DIRECTION('',(-0.104528463267657,-0.994521895368273,1.47193748793071E-17));
#118115=DIRECTION('center_axis',(0.994521796408007,-0.104529404794542,1.63977756733249E-6));
#118116=DIRECTION('ref_axis',(0.0905261626114006,0.861298903188755,0.49996921230082));
#118117=DIRECTION('',(-0.052264755605229,-0.49726593293894,-0.866022509672752));
#118118=DIRECTION('',(-0.104528463267657,-0.994521895368273,1.47193748793071E-17));
#118119=DIRECTION('center_axis',(-1.70094388097119E-16,-1.37739719617122E-16,
-1.));
#118120=DIRECTION('ref_axis',(-1.,6.23562738597969E-50,1.70094388097119E-16));
#118121=DIRECTION('',(-0.207911690817763,-0.978147600733805,1.70094388097119E-16));
#118122=DIRECTION('center_axis',(1.70094388097119E-16,1.37739719617122E-16,
1.));
#118123=DIRECTION('ref_axis',(-1.,-6.98701029200995E-33,1.70094388097119E-16));
#118124=DIRECTION('',(0.207911690817763,0.978147600733805,-1.70094388097119E-16));
#118125=DIRECTION('center_axis',(-1.70094388097119E-16,-1.37739719617122E-16,
-1.));
#118126=DIRECTION('ref_axis',(-1.,7.23724578308843E-33,1.70094388097119E-16));
#118127=DIRECTION('center_axis',(0.978147600733805,-0.207911690817763,-1.37739719617122E-16));
#118128=DIRECTION('ref_axis',(1.70094388097119E-16,1.37739719617122E-16,
1.));
#118129=DIRECTION('center_axis',(0.978147600733804,-0.207911690817767,2.10892535025602E-14));
#118130=DIRECTION('ref_axis',(0.181850263143708,0.855538223402485,0.484752338923582));
#118131=DIRECTION('',(0.110177542335813,0.518344583061401,0.848044693619235));
#118132=DIRECTION('',(-0.207911690817763,-0.978147600733805,1.70094388097119E-16));
#118133=DIRECTION('',(0.11017743333423,0.518344070249263,-0.848045021223112));
#118134=DIRECTION('center_axis',(0.9781476007338,-0.207911690817786,-3.70784999236818E-14));
#118135=DIRECTION('ref_axis',(0.181849873248753,0.855536389090898,-0.484755722545614));
#118136=DIRECTION('',(0.207911690817763,0.978147600733805,-2.92774812072088E-17));
#118137=DIRECTION('',(0.10395688761095,0.489078703542082,0.866022509672723));
#118138=DIRECTION('center_axis',(-0.978147797590169,0.207910764672762,1.63998886609772E-6));
#118139=DIRECTION('ref_axis',(0.18006656357774,0.847146577519975,0.499918702268176));
#118140=DIRECTION('',(0.207911690817763,0.978147600733805,-2.92774812072088E-17));
#118141=DIRECTION('center_axis',(-0.978147403855348,0.207912617049453,1.64014401168597E-6));
#118142=DIRECTION('ref_axis',(0.180060523666507,0.847118160898064,-0.499969028334382));
#118143=DIRECTION('',(0.10395692016612,0.489078856702209,-0.866022419268944));
#118144=DIRECTION('',(0.207911690817763,0.978147600733805,-2.92774812072088E-17));
#118145=DIRECTION('center_axis',(0.978147600733805,-0.207911690817763,-1.37739719617122E-16));
#118146=DIRECTION('ref_axis',(1.70094388097119E-16,1.37739719617122E-16,
1.));
#118147=DIRECTION('center_axis',(-0.978147600733803,0.207911690817772,1.15784163316921E-14));
#118148=DIRECTION('ref_axis',(0.181849873245457,0.855536389075389,-0.484755722574222));
#118149=DIRECTION('',(-0.110177433334229,-0.518344070249272,0.848045021223106));
#118150=DIRECTION('',(0.207911690817763,0.978147600733805,-1.70094388097119E-16));
#118151=DIRECTION('',(-0.110177542335815,-0.518344583061397,-0.848044693619238));
#118152=DIRECTION('center_axis',(-0.978147600733803,0.207911690817772,-2.01243856977405E-14));
#118153=DIRECTION('ref_axis',(0.181850263148122,0.855538223423227,0.48475233888532));
#118154=DIRECTION('',(-0.207911690817763,-0.978147600733805,2.92774812072088E-17));
#118155=DIRECTION('',(-0.103956920166122,-0.489078856702182,0.866022419268959));
#118156=DIRECTION('center_axis',(0.978147797635933,-0.207910764457452,1.6403704604808E-6));
#118157=DIRECTION('ref_axis',(0.180066584926772,0.847146677960533,-0.499918524374965));
#118158=DIRECTION('',(-0.207911690817763,-0.978147600733805,2.92774812072088E-17));
#118159=DIRECTION('center_axis',(0.978147403899289,-0.207912616842733,1.63977762473961E-6));
#118160=DIRECTION('ref_axis',(0.180060501584972,0.847118057013803,0.499969212302246));
#118161=DIRECTION('',(-0.103956887610927,-0.489078703542019,-0.866022509672761));
#118162=DIRECTION('',(-0.207911690817763,-0.978147600733805,2.92774812072088E-17));
#118163=DIRECTION('center_axis',(-1.84331724214208E-16,-1.33924836902177E-16,
-1.));
#118164=DIRECTION('ref_axis',(-1.,3.96466909511285E-49,1.84331724214208E-16));
#118165=DIRECTION('',(-0.309016994374951,-0.951056516295152,1.84331724214208E-16));
#118166=DIRECTION('center_axis',(1.84331724214208E-16,1.33924836902177E-16,
1.));
#118167=DIRECTION('ref_axis',(-1.,-4.8867629339927E-33,1.84331724214208E-16));
#118168=DIRECTION('',(0.309016994374951,0.951056516295152,-1.84331724214208E-16));
#118169=DIRECTION('center_axis',(-1.84331724214208E-16,-1.33924836902177E-16,
-1.));
#118170=DIRECTION('ref_axis',(-1.,-6.79952878369283E-33,1.84331724214208E-16));
#118171=DIRECTION('center_axis',(0.951056516295152,-0.309016994374951,-1.33924836902177E-16));
#118172=DIRECTION('ref_axis',(1.84331724214208E-16,1.33924836902177E-16,
1.));
#118173=DIRECTION('center_axis',(0.951056516295147,-0.309016994374967,1.64027527242136E-14));
#118174=DIRECTION('ref_axis',(0.270282164134392,0.831842966948485,0.484752338920785));
#118175=DIRECTION('',(0.163755740941359,0.503988348013124,0.848044693619239));
#118176=DIRECTION('',(-0.309016994374951,-0.951056516295152,1.84331724214208E-16));
#118177=DIRECTION('',(0.163755578933429,0.50398784940401,-0.848045021223106));
#118178=DIRECTION('center_axis',(0.951056516295152,-0.309016994374951,-1.48865352853428E-14));
#118179=DIRECTION('ref_axis',(0.270281584637258,0.831841183439741,-0.4847557225444));
#118180=DIRECTION('',(0.309016994374951,0.951056516295152,-4.35148173242975E-17));
#118181=DIRECTION('',(0.154510046201612,0.475533025522836,0.866022509672741));
#118182=DIRECTION('center_axis',(-0.951056808881645,0.309016093880519,1.63998890568801E-6));
#118183=DIRECTION('ref_axis',(0.267631070012908,0.823683738754867,0.499918702265228));
#118184=DIRECTION('',(0.309016994374951,0.951056516295152,-4.35148173242975E-17));
#118185=DIRECTION('center_axis',(-0.951056223677645,0.309017894953234,1.64014401443984E-6));
#118186=DIRECTION('ref_axis',(0.267622092842512,0.823656109142922,-0.499969028334893));
#118187=DIRECTION('',(0.154510094588035,0.475533174441033,-0.866022419268941));
#118188=DIRECTION('',(0.309016994374951,0.951056516295152,-4.35148173242975E-17));
#118189=DIRECTION('center_axis',(0.951056516295152,-0.309016994374951,-1.33924836902177E-16));
#118190=DIRECTION('ref_axis',(1.84331724214208E-16,1.33924836902177E-16,
1.));
#118191=DIRECTION('center_axis',(-0.951056516295152,0.309016994374953,-1.41973438352885E-14));
#118192=DIRECTION('ref_axis',(0.270281584632026,0.831841183423588,-0.484755722575036));
#118193=DIRECTION('',(-0.163755578933429,-0.50398784940401,0.848045021223106));
#118194=DIRECTION('',(0.309016994374951,0.951056516295152,-1.84331724214208E-16));
#118195=DIRECTION('',(-0.163755740941351,-0.50398834801313,-0.848044693619237));
#118196=DIRECTION('center_axis',(-0.951056516295161,0.309016994374925,4.4108242625183E-14));
#118197=DIRECTION('ref_axis',(0.270282164140163,0.831842966966275,0.484752338887038));
#118198=DIRECTION('',(-0.309016994374951,-0.951056516295152,4.35148173242975E-17));
#118199=DIRECTION('',(-0.15451009458806,-0.475533174441019,0.866022419268945));
#118200=DIRECTION('center_axis',(0.951056808949636,-0.30901609367126,1.64037036907829E-6));
#118201=DIRECTION('ref_axis',(0.267631101743422,0.823683836412152,-0.499918524374684));
#118202=DIRECTION('',(-0.309016994374951,-0.951056516295152,4.35148173242975E-17));
#118203=DIRECTION('center_axis',(0.951056223742969,-0.309017894752189,1.63977748978694E-6));
#118204=DIRECTION('ref_axis',(0.267622060023532,0.823656008137218,0.499969212300342));
#118205=DIRECTION('',(-0.154510046201597,-0.475533025522832,-0.866022509672746));
#118206=DIRECTION('',(-0.309016994374951,-0.951056516295152,4.35148173242975E-17));
#118207=DIRECTION('center_axis',(-1.98092302886631E-16,-1.28642645648559E-16,
-1.));
#118208=DIRECTION('ref_axis',(-1.,-1.14441315467514E-48,1.98092302886631E-16));
#118209=DIRECTION('',(-0.406736643075804,-0.913545457642599,1.98092302886631E-16));
#118210=DIRECTION('center_axis',(1.98092302886631E-16,1.28642645648559E-16,
1.));
#118211=DIRECTION('ref_axis',(-1.,-2.92382461743668E-33,1.98092302886631E-16));
#118212=DIRECTION('',(0.406736643075804,0.913545457642599,-1.98092302886631E-16));
#118213=DIRECTION('center_axis',(-1.98092302886631E-16,-1.28642645648559E-16,
-1.));
#118214=DIRECTION('ref_axis',(-1.,-4.76114818715937E-33,1.98092302886631E-16));
#118215=DIRECTION('center_axis',(0.913545457642599,-0.406736643075804,-1.28642645648559E-16));
#118216=DIRECTION('ref_axis',(1.98092302886631E-16,1.28642645648559E-16,
1.));
#118217=DIRECTION('center_axis',(0.913545457642599,-0.406736643075804,8.27029549119849E-16));
#118218=DIRECTION('ref_axis',(0.355752797173883,0.79903386487182,0.48475233892263));
#118219=DIRECTION('',(0.21553979738105,0.484110311157685,0.848044693619237));
#118220=DIRECTION('',(-0.406736643075804,-0.913545457642599,1.98092302886631E-16));
#118221=DIRECTION('',(0.215539584141768,0.48410983221443,-0.848045021223113));
#118222=DIRECTION('center_axis',(0.913545457642593,-0.406736643075818,-2.34325092454487E-14));
#118223=DIRECTION('ref_axis',(0.355752034424554,0.799032151708775,-0.484755722543257));
#118224=DIRECTION('',(0.406736643075804,0.913545457642599,-5.72753959967203E-17));
#118225=DIRECTION('',(0.203370360392782,0.456777308164353,0.866022509672721));
#118226=DIRECTION('center_axis',(-0.913545842753543,0.406735778098055,1.63998883055243E-6));
#118227=DIRECTION('ref_axis',(0.352263354438993,0.791196448578691,0.499918702266534));
#118228=DIRECTION('',(0.406736643075804,0.913545457642599,-5.72753959967203E-17));
#118229=DIRECTION('center_axis',(-0.913545072491979,0.406737508133851,1.64014412908005E-6));
#118230=DIRECTION('ref_axis',(0.352251538366349,0.791169908696165,-0.499969028332998));
#118231=DIRECTION('',(0.203370424080349,0.456777451208949,-0.866022419268945));
#118232=DIRECTION('',(0.406736643075804,0.913545457642599,-5.72753959967203E-17));
#118233=DIRECTION('center_axis',(0.913545457642599,-0.406736643075804,-1.28642645648559E-16));
#118234=DIRECTION('ref_axis',(1.98092302886631E-16,1.28642645648559E-16,
1.));
#118235=DIRECTION('center_axis',(-0.913545457642582,0.406736643075842,7.41569998386918E-14));
#118236=DIRECTION('ref_axis',(0.355752034417934,0.799032151693907,-0.484755722572623));
#118237=DIRECTION('',(-0.215539584141773,-0.484109832214439,0.848045021223107));
#118238=DIRECTION('',(0.406736643075804,0.913545457642599,-1.98092302886631E-16));
#118239=DIRECTION('',(-0.215539797381042,-0.48411031115768,-0.848044693619242));
#118240=DIRECTION('center_axis',(-0.913545457642587,0.406736643075831,-3.9559580104464E-14));
#118241=DIRECTION('ref_axis',(0.355752797181886,0.799033864889778,0.484752338887155));
#118242=DIRECTION('',(-0.406736643075804,-0.913545457642599,5.72753959967203E-17));
#118243=DIRECTION('',(-0.203370424080353,-0.456777451208954,0.866022419268941));
#118244=DIRECTION('center_axis',(0.913545842843099,-0.406735777896905,1.64037054559977E-6));
#118245=DIRECTION('ref_axis',(0.352263396203069,0.791196542382979,-0.499918524378422));
#118246=DIRECTION('',(-0.406736643075804,-0.913545457642599,5.72753959967203E-17));
#118247=DIRECTION('center_axis',(0.913545072577997,-0.406737507940653,1.63977751543501E-6));
#118248=DIRECTION('ref_axis',(0.352251495169236,0.791169811674494,0.4999692122981));
#118249=DIRECTION('',(-0.203370360392794,-0.4567773081643,-0.866022509672746));
#118250=DIRECTION('',(-0.406736643075804,-0.913545457642599,5.72753959967203E-17));
#118251=DIRECTION('center_axis',(-2.11225360334866E-16,-1.2195101864901E-16,
-1.));
#118252=DIRECTION('ref_axis',(-1.,-1.3208785554854E-48,2.11225360334866E-16));
#118253=DIRECTION('',(-0.500000000000004,-0.866025403784436,2.11225360334866E-16));
#118254=DIRECTION('center_axis',(2.11225360334866E-16,1.2195101864901E-16,
1.));
#118255=DIRECTION('ref_axis',(-1.,-1.17014578711787E-33,2.11225360334866E-16));
#118256=DIRECTION('',(0.500000000000004,0.866025403784436,-2.11225360334866E-16));
#118257=DIRECTION('center_axis',(-2.11225360334866E-16,-1.2195101864901E-16,
-1.));
#118258=DIRECTION('ref_axis',(-1.,-2.91189697534857E-33,2.11225360334866E-16));
#118259=DIRECTION('center_axis',(0.866025403784436,-0.500000000000004,-1.2195101864901E-16));
#118260=DIRECTION('ref_axis',(2.11225360334866E-16,1.2195101864901E-16,
1.));
#118261=DIRECTION('center_axis',(0.866025403784421,-0.500000000000031,1.15784136876797E-14));
#118262=DIRECTION('ref_axis',(0.437325728122469,0.757470380565119,0.484752338920285));
#118263=DIRECTION('',(0.264962354696018,0.4589282604266,0.848044693619243));
#118264=DIRECTION('',(-0.500000000000004,-0.866025403784436,2.11225360334866E-16));
#118265=DIRECTION('',(0.264962092561706,0.458927806396624,-0.84804502122311));
#118266=DIRECTION('center_axis',(0.866025403784434,-0.500000000000007,-2.48108921422391E-14));
#118267=DIRECTION('ref_axis',(0.437324790476918,0.757468756515445,-0.48475572254205));
#118268=DIRECTION('',(0.500000000000004,0.866025403784436,-7.04084534449558E-17));
#118269=DIRECTION('',(0.250002506357508,0.433017043030766,0.866022509672731));
#118270=DIRECTION('center_axis',(-0.866025877200519,0.49999918001571,1.63998888615131E-6));
#118271=DIRECTION('ref_axis',(0.433036167837011,0.750040644542055,0.499918702270653));
#118272=DIRECTION('',(0.500000000000004,0.866025403784436,-7.04084534449558E-17));
#118273=DIRECTION('center_axis',(-0.866024930320553,0.500000820059919,1.64014405730139E-6));
#118274=DIRECTION('ref_axis',(0.433021642321843,0.750015485165317,-0.499969028333883));
#118275=DIRECTION('',(0.250002584648429,0.433017178634621,-0.866022419268935));
#118276=DIRECTION('',(0.500000000000004,0.866025403784436,-7.04084534449558E-17));
#118277=DIRECTION('center_axis',(0.866025403784436,-0.500000000000004,-1.2195101864901E-16));
#118278=DIRECTION('ref_axis',(2.11225360334866E-16,1.2195101864901E-16,
1.));
#118279=DIRECTION('center_axis',(-0.866025403784422,0.50000000000003,5.29299032305956E-14));
#118280=DIRECTION('ref_axis',(0.437324790468609,0.757468756501035,-0.484755722572063));
#118281=DIRECTION('',(-0.264962092561705,-0.458927806396619,0.848045021223113));
#118282=DIRECTION('',(0.500000000000004,0.866025403784436,-2.11225360334866E-16));
#118283=DIRECTION('',(-0.264962354696036,-0.458928260426624,-0.848044693619225));
#118284=DIRECTION('center_axis',(-0.866025403784439,0.5,2.46730482184633E-14));
#118285=DIRECTION('ref_axis',(0.437325728131445,0.757470380580693,0.484752338887851));
#118286=DIRECTION('',(-0.500000000000004,-0.866025403784436,7.04084534449558E-17));
#118287=DIRECTION('',(-0.25000258464842,-0.4330171786346,0.866022419268947));
#118288=DIRECTION('center_axis',(0.866025877310547,-0.499999179825134,1.64037039928712E-6));
#118289=DIRECTION('ref_axis',(0.43303621917957,0.750040733470476,-0.499918524375456));
#118290=DIRECTION('',(-0.500000000000004,-0.866025403784436,7.04084534449558E-17));
#118291=DIRECTION('center_axis',(0.866024930426266,-0.50000081987682,1.63977751491898E-6));
#118292=DIRECTION('ref_axis',(0.433021589219966,0.750015393190659,0.499969212298594));
#118293=DIRECTION('',(-0.250002506357472,-0.433017043030735,-0.866022509672757));
#118294=DIRECTION('',(-0.500000000000004,-0.866025403784436,7.04084534449558E-17));
#118295=DIRECTION('center_axis',(-2.23587008033243E-16,-1.13923270769252E-16,
-1.));
#118296=DIRECTION('ref_axis',(-1.,-1.7597119642318E-48,2.23587008033243E-16));
#118297=DIRECTION('',(-0.587785252292477,-0.809016994374945,2.23587008033243E-16));
#118298=DIRECTION('center_axis',(2.23587008033243E-16,1.13923270769252E-16,
1.));
#118299=DIRECTION('ref_axis',(-1.,-2.1582735598713E-13,2.23587008033267E-16));
#118300=DIRECTION('',(0.587785252292477,0.809016994374945,-2.23587008033243E-16));
#118301=DIRECTION('center_axis',(-2.23587008033243E-16,-1.13923270769252E-16,
-1.));
#118302=DIRECTION('ref_axis',(-1.,-1.31193432862153E-33,2.23587008033243E-16));
#118303=DIRECTION('center_axis',(0.809016994374945,-0.587785252292477,-1.13923270769252E-16));
#118304=DIRECTION('ref_axis',(2.23587008033243E-16,1.13923270769252E-16,
1.));
#118305=DIRECTION('center_axis',(0.809016994374929,-0.587785252292498,1.59892379496519E-14));
#118306=DIRECTION('ref_axis',(0.514107226876986,0.707607892257023,0.484752338920019));
#118307=DIRECTION('',(0.311481929006017,0.428718095637374,0.848044693619242));
#118308=DIRECTION('',(-0.587785252292477,-0.809016994374945,2.23587008033243E-16));
#118309=DIRECTION('',(0.31148162084865,0.428717671495116,-0.848045021223109));
#118310=DIRECTION('center_axis',(0.809016994374931,-0.587785252292496,-3.45974107094534E-14));
#118311=DIRECTION('ref_axis',(0.514106124608479,0.707606375114597,-0.484755722542015));
#118312=DIRECTION('',(0.587785252292477,0.809016994374945,-8.27701011433323E-17));
#118313=DIRECTION('',(0.293895572546184,0.4045125525591,0.866022509672741));
#118314=DIRECTION('center_axis',(-0.809017550909309,0.58778448628559,1.63998887651158E-6));
#118315=DIRECTION('ref_axis',(0.50906454636235,0.700667238249654,0.499918702271177));
#118316=DIRECTION('',(0.587785252292477,0.809016994374945,-8.27701011433323E-17));
#118317=DIRECTION('center_axis',(-0.809016437785106,0.587786018369617,1.64014417022043E-6));
#118318=DIRECTION('ref_axis',(0.509047470549715,0.70064373503006,-0.49996902833082));
#118319=DIRECTION('',(0.293895664582666,0.404512679236473,-0.866022419268949));
#118320=DIRECTION('',(0.587785252292477,0.809016994374945,-8.27701011433323E-17));
#118321=DIRECTION('center_axis',(0.809016994374945,-0.587785252292477,-1.13923270769252E-16));
#118322=DIRECTION('ref_axis',(2.23587008033243E-16,1.13923270769252E-16,
1.));
#118323=DIRECTION('center_axis',(-0.809016994374939,0.587785252292484,2.23298029254063E-14));
#118324=DIRECTION('ref_axis',(0.514106124597969,0.707606375100143,-0.484755722574261));
#118325=DIRECTION('',(-0.311481620848633,-0.428717671495124,0.848045021223112));
#118326=DIRECTION('',(0.587785252292477,0.809016994374945,-2.23587008033243E-16));
#118327=DIRECTION('',(-0.311481929006026,-0.428718095637378,-0.848044693619237));
#118328=DIRECTION('center_axis',(-0.80901699437497,0.587785252292442,5.77542301873549E-14));
#118329=DIRECTION('ref_axis',(0.514107226887194,0.707607892271115,0.484752338888621));
#118330=DIRECTION('',(-0.587785252292477,-0.809016994374945,8.27701011433323E-17));
#118331=DIRECTION('',(-0.293895664582688,-0.404512679236433,0.86602241926896));
#118332=DIRECTION('center_axis',(0.809017551038662,-0.587784486107549,1.64037043199266E-6));
#118333=DIRECTION('ref_axis',(0.50906460671898,0.700667321323834,-0.499918524376656));
#118334=DIRECTION('',(-0.587785252292477,-0.809016994374945,8.27701011433323E-17));
#118335=DIRECTION('center_axis',(0.809016437909387,-0.58778601819856,1.6397775619102E-6));
#118336=DIRECTION('ref_axis',(0.509047408123843,0.700643649108601,0.499969212298298));
#118337=DIRECTION('',(-0.293895572546212,-0.404512552559089,-0.866022509672736));
#118338=DIRECTION('',(-0.587785252292477,-0.809016994374945,8.27701011433323E-17));
#118339=DIRECTION('center_axis',(-2.35041809182736E-16,-1.04647355694969E-16,
-1.));
#118340=DIRECTION('ref_axis',(-1.,1.47166508017397E-49,2.35041809182736E-16));
#118341=DIRECTION('',(-0.669130606358862,-0.743144825477391,2.35041809182736E-16));
#118342=DIRECTION('center_axis',(2.35041809182736E-16,1.04647355694969E-16,
1.));
#118343=DIRECTION('ref_axis',(-1.,1.48821490844481E-33,2.35041809182736E-16));
#118344=DIRECTION('',(0.669130606358862,0.743144825477391,-2.35041809182736E-16));
#118345=DIRECTION('center_axis',(-2.35041809182736E-16,-1.04647355694969E-16,
-1.));
#118346=DIRECTION('ref_axis',(-1.,-6.39873354129293E-36,2.35041809182736E-16));
#118347=DIRECTION('center_axis',(0.743144825477391,-0.669130606358862,-1.04647355694969E-16));
#118348=DIRECTION('ref_axis',(2.35041809182736E-16,1.04647355694969E-16,
1.));
#118349=DIRECTION('center_axis',(0.743144825477429,-0.669130606358819,-1.06962488352839E-13));
#118350=DIRECTION('ref_axis',(0.585256059269864,0.649992703804717,0.484752338920137));
#118351=DIRECTION('',(0.354588842120037,0.393810805677316,0.848044693619242));
#118352=DIRECTION('',(-0.669130606358862,-0.743144825477391,2.35041809182736E-16));
#118353=DIRECTION('',(0.354588491315835,0.393810416069778,-0.848045021223112));
#118354=DIRECTION('center_axis',(0.743144825477371,-0.669130606358884,-3.94217508482234E-14));
#118355=DIRECTION('ref_axis',(0.585254804454904,0.649991310191511,-0.484755722542782));
#118356=DIRECTION('',(0.669130606358862,0.743144825477391,-9.42249022928252E-17));
#118357=DIRECTION('',(0.334568657340454,0.371576137911918,0.866022509672739));
#118358=DIRECTION('center_axis',(-0.743145459032553,0.66912990272189,1.63998899132442E-6));
#118359=DIRECTION('ref_axis',(0.579515507192058,0.64361717507423,0.499918702264078));
#118360=DIRECTION('',(0.669130606358862,0.743144825477391,-9.42249022928252E-17));
#118361=DIRECTION('center_axis',(-0.743144191859738,0.669131310059876,1.64014411444931E-6));
#118362=DIRECTION('ref_axis',(0.579496068164192,0.64359558551295,-0.499969028331242));
#118363=DIRECTION('',(0.33456876211414,0.371576254274883,-0.866022419268959));
#118364=DIRECTION('',(0.669130606358862,0.743144825477391,-9.42249022928252E-17));
#118365=DIRECTION('center_axis',(0.743144825477391,-0.669130606358862,-1.04647355694969E-16));
#118366=DIRECTION('ref_axis',(2.35041809182736E-16,1.04647355694969E-16,
1.));
#118367=DIRECTION('center_axis',(-0.743144825477379,0.669130606358875,2.06757434494493E-14));
#118368=DIRECTION('ref_axis',(0.585254804443977,0.649991310179378,-0.484755722572244));
#118369=DIRECTION('',(-0.354588491315839,-0.393810416069783,0.848045021223108));
#118370=DIRECTION('',(0.669130606358862,0.743144825477391,-2.35041809182736E-16));
#118371=DIRECTION('',(-0.354588842120062,-0.393810805677307,-0.848044693619236));
#118372=DIRECTION('center_axis',(-0.743144825477412,0.669130606358838,6.12001866424422E-14));
#118373=DIRECTION('ref_axis',(0.585256059281444,0.649992703817579,0.484752338888909));
#118374=DIRECTION('',(-0.669130606358862,-0.743144825477391,9.42249022928252E-17));
#118375=DIRECTION('',(-0.334568762114167,-0.371576254274909,0.866022419268937));
#118376=DIRECTION('center_axis',(0.743145459179755,-0.669129902558405,1.64037040565622E-6));
#118377=DIRECTION('ref_axis',(0.579515575899146,0.643617251381539,-0.499918524376076));
#118378=DIRECTION('',(-0.669130606358862,-0.743144825477391,9.42249022928252E-17));
#118379=DIRECTION('center_axis',(0.743144192001206,-0.669131309902762,1.63977762043609E-6));
#118380=DIRECTION('ref_axis',(0.579495997097348,0.643595506585619,0.499969212303069));
#118381=DIRECTION('',(-0.334568657340481,-0.371576137911908,-0.866022509672733));
#118382=DIRECTION('',(-0.669130606358862,-0.743144825477391,9.42249022928252E-17));
#118383=DIRECTION('center_axis',(-2.4546426258488E-16,-9.42249022928242E-17,
-1.));
#118384=DIRECTION('ref_axis',(-1.,-5.4163468893589E-49,2.4546426258488E-16));
#118385=DIRECTION('',(-0.743144825477398,-0.669130606358854,2.4546426258488E-16));
#118386=DIRECTION('center_axis',(2.4546426258488E-16,9.42249022928242E-17,
1.));
#118387=DIRECTION('ref_axis',(-1.,2.32204937581661E-33,2.4546426258488E-16));
#118388=DIRECTION('',(0.743144825477398,0.669130606358854,-2.4546426258488E-16));
#118389=DIRECTION('center_axis',(-2.4546426258488E-16,-9.42249022928242E-17,
-1.));
#118390=DIRECTION('ref_axis',(-1.,9.76293207909597E-34,2.4546426258488E-16));
#118391=DIRECTION('center_axis',(0.669130606358854,-0.743144825477398,-9.42249022928242E-17));
#118392=DIRECTION('ref_axis',(2.4546426258488E-16,9.42249022928242E-17,
1.));
#118393=DIRECTION('center_axis',(0.669130606358848,-0.743144825477403,8.54597200757256E-15));
#118394=DIRECTION('ref_axis',(0.649992703802778,0.5852560592681,0.484752338924866));
#118395=DIRECTION('',(0.393810805677326,0.354588842120041,0.848044693619236));
#118396=DIRECTION('',(-0.743144825477398,-0.669130606358854,2.4546426258488E-16));
#118397=DIRECTION('',(0.393810416069787,0.354588491315845,-0.848045021223104));
#118398=DIRECTION('center_axis',(0.669130606358885,-0.74314482547737,4.49352824353853E-14));
#118399=DIRECTION('ref_axis',(0.649991310191743,0.58525480445511,-0.484755722542222));
#118400=DIRECTION('',(0.743144825477398,0.669130606358854,-1.04647355694969E-16));
#118401=DIRECTION('',(0.37157613791195,0.334568657340486,0.866022509672713));
#118402=DIRECTION('center_axis',(-0.66913130999335,0.743144191919639,1.63998879715907E-6));
#118403=DIRECTION('ref_axis',(0.643617174849723,0.57951550743858,0.499918702267346));
#118404=DIRECTION('',(0.743144825477398,0.669130606358854,-1.04647355694969E-16));
#118405=DIRECTION('center_axis',(-0.669129902655549,0.743145459092287,1.64014392062814E-6));
#118406=DIRECTION('ref_axis',(0.643595585588892,0.579496068080419,-0.499969028330582));
#118407=DIRECTION('',(0.371576254274919,0.33456876211414,-0.866022419268943));
#118408=DIRECTION('',(0.743144825477398,0.669130606358854,-1.04647355694969E-16));
#118409=DIRECTION('center_axis',(0.669130606358854,-0.743144825477398,-9.42249022928242E-17));
#118410=DIRECTION('ref_axis',(2.4546426258488E-16,9.42249022928242E-17,
1.));
#118411=DIRECTION('center_axis',(-0.669130606358856,0.743144825477396,-2.31568326633855E-14));
#118412=DIRECTION('ref_axis',(0.64999131017826,0.585254804442939,-0.484755722574996));
#118413=DIRECTION('',(-0.393810416069767,-0.354588491315837,0.848045021223116));
#118414=DIRECTION('',(0.743144825477398,0.669130606358854,-2.4546426258488E-16));
#118415=DIRECTION('',(-0.393810805677306,-0.354588842120033,-0.848044693619249));
#118416=DIRECTION('center_axis',(-0.669130606358852,0.7431448254774,1.18540902055183E-14));
#118417=DIRECTION('ref_axis',(0.649992703818894,0.585256059282603,0.484752338885747));
#118418=DIRECTION('',(-0.743144825477398,-0.669130606358854,1.04647355694969E-16));
#118419=DIRECTION('',(-0.371576254274903,-0.334568762114161,0.866022419268941));
#118420=DIRECTION('center_axis',(0.669131310156939,-0.743144191772342,1.64037041409087E-6));
#118421=DIRECTION('ref_axis',(0.643617251158495,0.579515576147658,-0.499918524375154));
#118422=DIRECTION('',(-0.743144825477398,-0.669130606358854,1.04647355694969E-16));
#118423=DIRECTION('center_axis',(0.66912990281256,-0.743145458950915,1.63977762973069E-6));
#118424=DIRECTION('ref_axis',(0.643595506661403,0.579495997014118,0.499969212301983));
#118425=DIRECTION('',(-0.371576137911901,-0.334568657340439,-0.866022509672752));
#118426=DIRECTION('',(-0.743144825477398,-0.669130606358854,1.04647355694969E-16));
#118427=DIRECTION('center_axis',(-2.54740177659163E-16,-8.27701011433311E-17,
-1.));
#118428=DIRECTION('ref_axis',(-1.,8.43631949586388E-49,2.54740177659163E-16));
#118429=DIRECTION('',(-0.80901699437495,-0.587785252292469,2.54740177659163E-16));
#118430=DIRECTION('center_axis',(2.54740177659163E-16,8.27701011433311E-17,
1.));
#118431=DIRECTION('ref_axis',(-1.,1.4388490399142E-13,2.54740177659151E-16));
#118432=DIRECTION('',(0.80901699437495,0.587785252292469,-2.54740177659163E-16));
#118433=DIRECTION('center_axis',(-2.54740177659163E-16,-8.27701011433311E-17,
-1.));
#118434=DIRECTION('ref_axis',(-1.,1.62537491717908E-33,2.54740177659163E-16));
#118435=DIRECTION('center_axis',(0.587785252292469,-0.80901699437495,-8.27701011433311E-17));
#118436=DIRECTION('ref_axis',(2.54740177659163E-16,8.27701011433311E-17,
1.));
#118437=DIRECTION('center_axis',(0.587785252292449,-0.809016994374965,4.85190668817008E-14));
#118438=DIRECTION('ref_axis',(0.707607892255849,0.514107226876106,0.484752338922666));
#118439=DIRECTION('',(0.428718095637378,0.31148192900602,0.848044693619239));
#118440=DIRECTION('',(-0.80901699437495,-0.587785252292469,2.54740177659163E-16));
#118441=DIRECTION('',(0.428717671495124,0.311481620848633,-0.848045021223112));
#118442=DIRECTION('center_axis',(0.587785252292468,-0.809016994374951,1.7505462789247E-14));
#118443=DIRECTION('ref_axis',(0.707606375113376,0.514106124607565,-0.484755722544767));
#118444=DIRECTION('',(0.80901699437495,0.587785252292469,-1.13923270769253E-16));
#118445=DIRECTION('',(0.40451255255907,0.293895572546188,0.866022509672753));
#118446=DIRECTION('center_axis',(-0.587786018297218,0.809016437837708,1.63998882108571E-6));
#118447=DIRECTION('ref_axis',(0.700667238053761,0.509064546632194,0.499918702270952));
#118448=DIRECTION('',(0.80901699437495,0.587785252292469,-1.13923270769253E-16));
#118449=DIRECTION('center_axis',(-0.587784486213293,0.809017550961835,1.64014400187427E-6));
#118450=DIRECTION('ref_axis',(0.700643735095865,0.509047470457802,-0.499969028332185));
#118451=DIRECTION('',(0.404512679236439,0.293895664582703,-0.866022419268952));
#118452=DIRECTION('',(0.80901699437495,0.587785252292469,-1.13923270769253E-16));
#118453=DIRECTION('center_axis',(0.587785252292469,-0.80901699437495,-8.27701011433311E-17));
#118454=DIRECTION('ref_axis',(2.54740177659163E-16,8.27701011433311E-17,
1.));
#118455=DIRECTION('center_axis',(-0.587785252292455,0.809016994374961,5.2378550071936E-15));
#118456=DIRECTION('ref_axis',(0.707606375100509,0.514106124598213,-0.484755722573467));
#118457=DIRECTION('',(-0.428717671495138,-0.311481620848646,0.8480450212231));
#118458=DIRECTION('',(0.80901699437495,0.587785252292469,-2.54740177659163E-16));
#118459=DIRECTION('',(-0.428718095637388,-0.311481929006024,-0.848044693619232));
#118460=DIRECTION('center_axis',(-0.587785252292488,0.809016994374937,2.35703421528348E-14));
#118461=DIRECTION('ref_axis',(0.707607892272611,0.514107226888294,0.484752338885272));
#118462=DIRECTION('',(-0.80901699437495,-0.587785252292469,1.13923270769253E-16));
#118463=DIRECTION('',(-0.404512679236475,-0.293895664582703,0.866022419268936));
#118464=DIRECTION('center_axis',(0.587786018475335,-0.809016437708297,1.64037056436227E-6));
#118465=DIRECTION('ref_axis',(0.700667321128012,0.509064606989453,-0.499918524375691));
#118466=DIRECTION('',(-0.80901699437495,-0.587785252292469,1.13923270769253E-16));
#118467=DIRECTION('center_axis',(0.58778448638428,-0.809017550837606,1.63977760081284E-6));
#118468=DIRECTION('ref_axis',(0.70064364917268,0.509047408031267,0.499969212302758));
#118469=DIRECTION('',(-0.404512552559119,-0.293895572546208,-0.866022509672724));
#118470=DIRECTION('',(-0.80901699437495,-0.587785252292469,1.13923270769253E-16));
#118471=DIRECTION('center_axis',(-2.62767925538921E-16,-7.04084534449545E-17,
-1.));
#118472=DIRECTION('ref_axis',(-1.,-5.53924399605649E-49,2.62767925538921E-16));
#118473=DIRECTION('',(-0.866025403784441,-0.499999999999995,2.62767925538921E-16));
#118474=DIRECTION('center_axis',(2.62767925538921E-16,7.04084534449545E-17,
1.));
#118475=DIRECTION('ref_axis',(-1.,1.19904086659517E-13,2.62767925538913E-16));
#118476=DIRECTION('',(0.866025403784441,0.499999999999995,-2.62767925538921E-16));
#118477=DIRECTION('center_axis',(-2.62767925538921E-16,-7.04084534449545E-17,
-1.));
#118478=DIRECTION('ref_axis',(-1.,1.9478478000333E-33,2.62767925538921E-16));
#118479=DIRECTION('center_axis',(0.499999999999995,-0.866025403784442,-7.04084534449545E-17));
#118480=DIRECTION('ref_axis',(2.62767925538921E-16,7.04084534449546E-17,
1.));
#118481=DIRECTION('center_axis',(0.500000000000008,-0.866025403784434,-2.67406220882127E-14));
#118482=DIRECTION('ref_axis',(0.757470380562976,0.437325728121196,0.484752338924782));
#118483=DIRECTION('',(0.458928260426606,0.264962354696021,0.848044693619239));
#118484=DIRECTION('',(-0.866025403784442,-0.499999999999995,2.62767925538921E-16));
#118485=DIRECTION('',(0.458927806396636,0.264962092561693,-0.848045021223108));
#118486=DIRECTION('center_axis',(0.500000000000001,-0.866025403784438,-1.18540929124028E-14));
#118487=DIRECTION('ref_axis',(0.757468756514725,0.437324790476515,-0.484755722543538));
#118488=DIRECTION('',(0.866025403784442,0.499999999999995,-1.21951018649011E-16));
#118489=DIRECTION('',(0.433017043030755,0.250002506357484,0.866022509672744));
#118490=DIRECTION('center_axis',(-0.50000081998247,0.866024930365269,1.63998882177424E-6));
#118491=DIRECTION('ref_axis',(0.750040644378195,0.433036168127423,0.499918702264939));
#118492=DIRECTION('',(0.866025403784442,0.499999999999995,-1.21951018649011E-16));
#118493=DIRECTION('center_axis',(-0.499999179938243,0.866025877245244,1.64014413493299E-6));
#118494=DIRECTION('ref_axis',(0.750015485221644,0.433021642223838,-0.499969028334268));
#118495=DIRECTION('',(0.433017178634609,0.250002584648407,-0.866022419268947));
#118496=DIRECTION('',(0.866025403784442,0.499999999999995,-1.21951018649011E-16));
#118497=DIRECTION('center_axis',(0.499999999999995,-0.866025403784442,-7.04084534449545E-17));
#118498=DIRECTION('ref_axis',(2.62767925538921E-16,7.04084534449546E-17,
1.));
#118499=DIRECTION('center_axis',(-0.500000000000014,0.866025403784431,-5.23785500719396E-14));
#118500=DIRECTION('ref_axis',(0.757468756499955,0.437324790467967,-0.48475572257433));
#118501=DIRECTION('',(-0.458927806396646,-0.264962092561691,0.848045021223103));
#118502=DIRECTION('',(0.866025403784442,0.499999999999995,-2.62767925538921E-16));
#118503=DIRECTION('',(-0.458928260426595,-0.264962354696022,-0.848044693619245));
#118504=DIRECTION('center_axis',(-0.499999999999967,0.866025403784458,-3.87325505552417E-14));
#118505=DIRECTION('ref_axis',(0.757470380580733,0.437325728131438,0.484752338887795));
#118506=DIRECTION('',(-0.866025403784442,-0.499999999999995,1.21951018649011E-16));
#118507=DIRECTION('',(-0.433017178634596,-0.2500025846484,0.866022419268955));
#118508=DIRECTION('center_axis',(0.500000820173097,-0.866024930255209,1.64037045746811E-6));
#118509=DIRECTION('ref_axis',(0.750040733301865,0.433036219467805,-0.499918524378755));
#118510=DIRECTION('',(-0.866025403784442,-0.499999999999995,1.21951018649011E-16));
#118511=DIRECTION('center_axis',(0.499999180121334,-0.866025877139537,1.63977761957551E-6));
#118512=DIRECTION('ref_axis',(0.75001539324847,0.433021589123389,0.499969212295514));
#118513=DIRECTION('',(-0.433017043030764,-0.250002506357468,-0.866022509672744));
#118514=DIRECTION('',(-0.866025403784442,-0.499999999999995,1.21951018649011E-16));
#118515=DIRECTION('center_axis',(-2.6945955253847E-16,-5.7275395996719E-17,
-1.));
#118516=DIRECTION('ref_axis',(-1.,-2.59568075678046E-49,2.6945955253847E-16));
#118517=DIRECTION('',(-0.913545457642603,-0.406736643075795,2.6945955253847E-16));
#118518=DIRECTION('center_axis',(2.6945955253847E-16,5.7275395996719E-17,
1.));
#118519=DIRECTION('ref_axis',(-1.,-4.79616346638067E-14,2.69459552538472E-16));
#118520=DIRECTION('',(0.913545457642603,0.406736643075795,-2.6945955253847E-16));
#118521=DIRECTION('center_axis',(-2.6945955253847E-16,-5.7275395996719E-17,
-1.));
#118522=DIRECTION('ref_axis',(-1.,1.96778773707771E-33,2.6945955253847E-16));
#118523=DIRECTION('center_axis',(0.406736643075795,-0.913545457642603,-5.7275395996719E-17));
#118524=DIRECTION('ref_axis',(2.6945955253847E-16,5.72753959967189E-17,
1.));
#118525=DIRECTION('center_axis',(0.406736643075756,-0.913545457642621,7.60867185190295E-14));
#118526=DIRECTION('ref_axis',(0.799033864871858,0.355752797173889,0.484752338922563));
#118527=DIRECTION('',(0.484110311157687,0.215539797381032,0.84804469361924));
#118528=DIRECTION('',(-0.913545457642603,-0.406736643075795,2.6945955253847E-16));
#118529=DIRECTION('',(0.484109832214429,0.215539584141774,-0.848045021223112));
#118530=DIRECTION('center_axis',(0.406736643075805,-0.913545457642599,3.50109255784926E-14));
#118531=DIRECTION('ref_axis',(0.799032151708166,0.355752034424264,-0.484755722544475));
#118532=DIRECTION('',(0.913545457642603,0.406736643075795,-1.28642645648559E-16));
#118533=DIRECTION('',(0.45677730816434,0.203370360392759,0.866022509672733));
#118534=DIRECTION('center_axis',(-0.406737508052106,0.913545072528375,1.63998884122466E-6));
#118535=DIRECTION('ref_axis',(0.791196448438914,0.352263354741736,0.499918702274427));
#118536=DIRECTION('',(0.913545457642603,0.406736643075795,-1.28642645648559E-16));
#118537=DIRECTION('center_axis',(-0.406735778016346,0.913545842789921,1.64014402562863E-6));
#118538=DIRECTION('ref_axis',(0.791169908742041,0.352251538263013,-0.499969028333208));
#118539=DIRECTION('',(0.456777451208943,0.203370424080329,-0.866022419268952));
#118540=DIRECTION('',(0.913545457642603,0.406736643075795,-1.28642645648559E-16));
#118541=DIRECTION('center_axis',(0.406736643075795,-0.913545457642603,-5.7275395996719E-17));
#118542=DIRECTION('ref_axis',(2.6945955253847E-16,5.72753959967189E-17,
1.));
#118543=DIRECTION('center_axis',(-0.406736643075747,0.913545457642625,8.04975611631868E-14));
#118544=DIRECTION('ref_axis',(0.799032151693964,0.355752034417941,-0.484755722572524));
#118545=DIRECTION('',(-0.484109832214455,-0.215539584141767,0.848045021223099));
#118546=DIRECTION('',(0.913545457642603,0.406736643075795,-2.6945955253847E-16));
#118547=DIRECTION('',(-0.484110311157686,-0.215539797381038,-0.848044693619239));
#118548=DIRECTION('center_axis',(-0.406736643075831,0.913545457642587,3.95595801044615E-14));
#118549=DIRECTION('ref_axis',(0.799033864889901,0.355752797181941,0.484752338886912));
#118550=DIRECTION('',(-0.913545457642603,-0.406736643075795,1.28642645648559E-16));
#118551=DIRECTION('',(-0.45677745120895,-0.203370424080332,0.866022419268948));
#118552=DIRECTION('center_axis',(0.406737508253185,-0.913545072438848,1.6403704280331E-6));
#118553=DIRECTION('ref_axis',(0.791196542247288,0.352263396508196,-0.499918524378168));
#118554=DIRECTION('',(-0.913545457642603,-0.406736643075795,1.28642645648559E-16));
#118555=DIRECTION('center_axis',(0.406735778209537,-0.913545842703908,1.63977743556656E-6));
#118556=DIRECTION('ref_axis',(0.791169811719127,0.352251495065917,0.499969212300265));
#118557=DIRECTION('',(-0.456777308164345,-0.203370360392764,-0.866022509672729));
#118558=DIRECTION('',(-0.913545457642603,-0.406736643075795,1.28642645648559E-16));
#118559=DIRECTION('center_axis',(-2.74741743792088E-16,-4.35148173242961E-17,
-1.));
#118560=DIRECTION('ref_axis',(-1.,-6.81793207750932E-49,2.74741743792088E-16));
#118561=DIRECTION('',(-0.951056516295155,-0.309016994374942,2.74741743792088E-16));
#118562=DIRECTION('center_axis',(2.74741743792088E-16,4.35148173242961E-17,
1.));
#118563=DIRECTION('ref_axis',(-1.,-3.5527136788005E-14,2.7474174379209E-16));
#118564=DIRECTION('',(0.951056516295155,0.309016994374942,-2.74741743792088E-16));
#118565=DIRECTION('center_axis',(-2.74741743792088E-16,-4.35148173242961E-17,
-1.));
#118566=DIRECTION('ref_axis',(-1.,1.72487465929315E-33,2.74741743792088E-16));
#118567=DIRECTION('center_axis',(0.309016994374942,-0.951056516295155,-4.35148173242961E-17));
#118568=DIRECTION('ref_axis',(2.74741743792088E-16,4.35148173242962E-17,
1.));
#118569=DIRECTION('center_axis',(0.309016994374943,-0.951056516295155,-1.10270606549342E-14));
#118570=DIRECTION('ref_axis',(0.831842966946887,0.270282164133852,0.484752338923827));
#118571=DIRECTION('',(0.50398834801313,0.163755740941354,0.848044693619236));
#118572=DIRECTION('',(-0.951056516295155,-0.309016994374942,2.74741743792088E-16));
#118573=DIRECTION('',(0.503987849404007,0.163755578933419,-0.84804502122311));
#118574=DIRECTION('center_axis',(0.309016994374941,-0.951056516295156,7.16759106331303E-15));
#118575=DIRECTION('ref_axis',(0.831841183439701,0.270281584637239,-0.48475572254448));
#118576=DIRECTION('',(0.951056516295155,0.309016994374942,-1.33924836902178E-16));
#118577=DIRECTION('',(0.475533025522861,0.154510046201606,0.866022509672729));
#118578=DIRECTION('center_axis',(-0.309017894868253,0.951056223705257,1.63998893959849E-6));
#118579=DIRECTION('ref_axis',(0.823683738646395,0.267631070328247,0.499918702275135));
#118580=DIRECTION('',(0.951056516295155,0.309016994374942,-1.33924836902178E-16));
#118581=DIRECTION('center_axis',(-0.309016093795537,0.951056808909256,1.64014401168567E-6));
#118582=DIRECTION('ref_axis',(0.823656109179299,0.267622092735483,-0.499969028332256));
#118583=DIRECTION('',(0.475533174441019,0.15451009458806,-0.866022419268945));
#118584=DIRECTION('',(0.951056516295155,0.309016994374942,-1.33924836902178E-16));
#118585=DIRECTION('center_axis',(0.309016994374942,-0.951056516295155,-4.35148173242961E-17));
#118586=DIRECTION('ref_axis',(2.74741743792088E-16,4.35148173242962E-17,
1.));
#118587=DIRECTION('center_axis',(-0.30901699437496,0.95105651629515,-3.73541764986754E-14));
#118588=DIRECTION('ref_axis',(0.831841183424385,0.270281584632265,-0.484755722573536));
#118589=DIRECTION('',(-0.50398784940401,-0.163755578933429,0.848045021223106));
#118590=DIRECTION('',(0.951056516295155,0.309016994374942,-2.74741743792088E-16));
#118591=DIRECTION('',(-0.503988348013116,-0.16375574094134,-0.848044693619247));
#118592=DIRECTION('center_axis',(-0.30901699437493,0.951056516295159,-3.51487558419452E-14));
#118593=DIRECTION('ref_axis',(0.831842966965654,0.270282164139961,0.484752338888217));
#118594=DIRECTION('',(-0.951056516295155,-0.309016994374942,1.33924836902178E-16));
#118595=DIRECTION('',(-0.475533174441039,-0.154510094588055,0.866022419268935));
#118596=DIRECTION('center_axis',(0.309017895077549,-0.951056223637252,1.64037043259453E-6));
#118597=DIRECTION('ref_axis',(0.82368383630952,0.267631102061202,-0.49991852437366));
#118598=DIRECTION('',(-0.951056516295155,-0.309016994374942,1.33924836902178E-16));
#118599=DIRECTION('center_axis',(0.309016093996535,-0.951056808843949,1.63977760201822E-6));
#118600=DIRECTION('ref_axis',(0.823656008170397,0.267622059915953,0.499969212303267));
#118601=DIRECTION('',(-0.475533025522838,-0.154510046201608,-0.866022509672741));
#118602=DIRECTION('',(-0.951056516295155,-0.309016994374942,1.33924836902178E-16));
#118603=DIRECTION('center_axis',(-2.78556626507032E-16,-2.92774812072074E-17,
-1.));
#118604=DIRECTION('ref_axis',(-1.,-3.4710284701162E-49,2.78556626507032E-16));
#118605=DIRECTION('',(-0.978147600733807,-0.207911690817753,2.78556626507032E-16));
#118606=DIRECTION('center_axis',(2.78556626507032E-16,2.92774812072074E-17,
1.));
#118607=DIRECTION('ref_axis',(-1.,-1.15463194561016E-14,2.78556626507033E-16));
#118608=DIRECTION('',(0.978147600733807,0.207911690817753,-2.78556626507032E-16));
#118609=DIRECTION('center_axis',(-2.78556626507032E-16,-2.92774812072074E-17,
-1.));
#118610=DIRECTION('ref_axis',(-1.,1.27221405500122E-33,2.78556626507032E-16));
#118611=DIRECTION('center_axis',(0.207911690817753,-0.978147600733807,-2.92774812072074E-17));
#118612=DIRECTION('ref_axis',(2.78556626507032E-16,2.92774812072074E-17,
1.));
#118613=DIRECTION('center_axis',(0.207911690817736,-0.978147600733811,3.70784914522103E-14));
#118614=DIRECTION('ref_axis',(0.855538223403387,0.1818502631439,0.484752338921918));
#118615=DIRECTION('',(0.518344583061388,0.11017754233581,0.848044693619243));
#118616=DIRECTION('',(-0.978147600733807,-0.207911690817753,2.78556626507032E-16));
#118617=DIRECTION('',(0.51834407024927,0.110177433334225,-0.848045021223109));
#118618=DIRECTION('center_axis',(0.207911690817736,-0.978147600733811,-2.73609005013009E-14));
#118619=DIRECTION('ref_axis',(0.855536389091131,0.181849873248789,-0.484755722545189));
#118620=DIRECTION('',(0.978147600733807,0.207911690817753,-1.37739719617122E-16));
#118621=DIRECTION('',(0.489078703542109,0.103956887610931,0.866022509672709));
#118622=DIRECTION('center_axis',(-0.207912616962004,0.978147403873936,1.63998883769561E-6));
#118623=DIRECTION('ref_axis',(0.847146577450102,0.180066563903761,0.499918702269151));
#118624=DIRECTION('',(0.978147600733807,0.207911690817753,-1.37739719617122E-16));
#118625=DIRECTION('center_axis',(-0.207910764585298,0.97814779760876,1.64014406599374E-6));
#118626=DIRECTION('ref_axis',(0.847118160922528,0.180060523556151,-0.499969028332675));
#118627=DIRECTION('',(0.48907885670219,0.103956920166115,-0.866022419268956));
#118628=DIRECTION('',(0.978147600733807,0.207911690817753,-1.37739719617122E-16));
#118629=DIRECTION('center_axis',(0.207911690817753,-0.978147600733807,-2.92774812072074E-17));
#118630=DIRECTION('ref_axis',(2.78556626507032E-16,2.92774812072074E-17,
1.));
#118631=DIRECTION('center_axis',(-0.207911690817752,0.978147600733807,-2.75676579326004E-15));
#118632=DIRECTION('ref_axis',(0.855536389076247,0.181849873245626,-0.484755722572644));
#118633=DIRECTION('',(-0.51834407024927,-0.110177433334225,0.848045021223109));
#118634=DIRECTION('',(0.978147600733807,0.207911690817753,-2.78556626507032E-16));
#118635=DIRECTION('',(-0.518344583061404,-0.110177542335807,-0.848044693619234));
#118636=DIRECTION('center_axis',(-0.20791169081776,0.978147600733806,7.09867029749066E-15));
#118637=DIRECTION('ref_axis',(0.855538223422756,0.181850263148017,0.484752338886189));
#118638=DIRECTION('',(-0.978147600733807,-0.207911690817753,1.37739719617122E-16));
#118639=DIRECTION('',(-0.489078856702205,-0.103956920166127,0.866022419268946));
#118640=DIRECTION('center_axis',(0.207912617177324,-0.978147403828168,1.64037046383705E-6));
#118641=DIRECTION('ref_axis',(0.84714667788957,0.180066585253091,-0.49991852437768));
#118642=DIRECTION('',(-0.978147600733807,-0.207911690817753,1.37739719617122E-16));
#118643=DIRECTION('center_axis',(0.207910764792092,-0.978147797564805,1.6397775222343E-6));
#118644=DIRECTION('ref_axis',(0.84711805703836,0.180060501475129,0.499969212300196));
#118645=DIRECTION('',(-0.489078703542019,-0.103956887610927,-0.866022509672761));
#118646=DIRECTION('',(-0.978147600733807,-0.207911690817753,1.37739719617122E-16));
#118647=DIRECTION('center_axis',(-2.80862404029962E-16,-1.47193748793057E-17,
-1.));
#118648=DIRECTION('ref_axis',(-1.,-1.64025481450153E-49,2.80862404029962E-16));
#118649=DIRECTION('',(-0.994521895368274,-0.104528463267647,2.80862404029962E-16));
#118650=DIRECTION('center_axis',(2.80862404029962E-16,1.47193748793057E-17,
1.));
#118651=DIRECTION('ref_axis',(-1.,-2.66453525910038E-15,2.80862404029962E-16));
#118652=DIRECTION('',(0.994521895368274,0.104528463267647,-2.80862404029962E-16));
#118653=DIRECTION('center_axis',(-2.80862404029962E-16,-1.47193748793057E-17,
-1.));
#118654=DIRECTION('ref_axis',(-1.,6.73550486588661E-34,2.80862404029962E-16));
#118655=DIRECTION('center_axis',(0.104528463267647,-0.994521895368274,-1.47193748793057E-17));
#118656=DIRECTION('ref_axis',(2.80862404029962E-16,1.47193748793057E-17,
1.));
#118657=DIRECTION('center_axis',(0.104528463267645,-0.994521895368274,4.75541990743991E-15));
#118658=DIRECTION('ref_axis',(0.869860024050967,0.0914259726160544,0.484752338920876));
#118659=DIRECTION('',(0.527021726387054,0.0553922155203039,0.848044693619246));
#118660=DIRECTION('',(-0.994521895368274,-0.104528463267647,2.80862404029962E-16));
#118661=DIRECTION('',(0.527021204990425,0.0553921607193091,-0.848045021223099));
#118662=DIRECTION('center_axis',(0.104528463267658,-0.994521895368273,1.5816943740677E-14));
#118663=DIRECTION('ref_axis',(0.86985815903197,0.0914257765946603,-0.484755722544434));
#118664=DIRECTION('',(0.994521895368274,0.104528463267647,-1.40045497140052E-16));
#118665=DIRECTION('',(0.497265932938971,0.052264755605219,0.866022509672735));
#118666=DIRECTION('center_axis',(-0.104529404915867,0.994521796395255,1.6399888852479E-6));
#118667=DIRECTION('ref_axis',(0.861327901069651,0.0905292105225472,0.499918702271794));
#118668=DIRECTION('',(0.994521895368274,0.104528463267647,-1.40045497140052E-16));
#118669=DIRECTION('center_axis',(-0.104527521530161,0.994521994347069,1.64014404434785E-6));
#118670=DIRECTION('ref_axis',(0.861299008823205,0.0905261736006209,-0.499969028334151));
#118671=DIRECTION('',(0.497266088663028,0.052264771972486,-0.866022419268946));
#118672=DIRECTION('',(0.994521895368274,0.104528463267647,-1.40045497140052E-16));
#118673=DIRECTION('center_axis',(0.104528463267647,-0.994521895368274,-1.47193748793057E-17));
#118674=DIRECTION('ref_axis',(2.80862404029962E-16,1.47193748793057E-17,
1.));
#118675=DIRECTION('center_axis',(-0.104528463267646,0.994521895368274,2.06757434494494E-16));
#118676=DIRECTION('ref_axis',(0.869858159016553,0.0914257765930377,-0.484755722572404));
#118677=DIRECTION('',(-0.527021204990406,-0.0553921607193066,0.848045021223111));
#118678=DIRECTION('',(0.994521895368274,0.104528463267647,-2.80862404029962E-16));
#118679=DIRECTION('',(-0.527021726387066,-0.0553922155203067,-0.848044693619239));
#118680=DIRECTION('center_axis',(-0.104528463267645,0.994521895368274,-5.92704510275897E-15));
#118681=DIRECTION('ref_axis',(0.869860024069577,0.0914259726180108,0.484752338887112));
#118682=DIRECTION('',(-0.994521895368274,-0.104528463267647,1.40045497140052E-16));
#118683=DIRECTION('',(-0.497266088663036,-0.0522647719724824,0.866022419268942));
#118684=DIRECTION('center_axis',(0.104529405134733,-0.99452179637225,1.64037042377313E-6));
#118685=DIRECTION('ref_axis',(0.86132800319141,0.0905292212562273,-0.499918524378763));
#118686=DIRECTION('',(-0.994521895368274,-0.104528463267647,1.40045497140052E-16));
#118687=DIRECTION('center_axis',(0.104527521740379,-0.994521994324975,1.63977757288379E-6));
#118688=DIRECTION('ref_axis',(0.861298903204249,0.0905261624998609,0.499969212294324));
#118689=DIRECTION('',(-0.497265932938974,-0.0522647556052289,-0.866022509672732));
#118690=DIRECTION('',(-0.994521895368274,-0.104528463267647,1.40045497140052E-16));
#118691=DIRECTION('center_axis',(-2.81633813779821E-16,0.,-1.));
#118692=DIRECTION('ref_axis',(-1.,0.,2.81633813779821E-16));
#118693=DIRECTION('',(-1.,0.,2.81633813779821E-16));
#118694=DIRECTION('',(1.,0.,-2.81633813779821E-16));
#118695=DIRECTION('center_axis',(0.,-1.,0.));
#118696=DIRECTION('ref_axis',(2.81633813779821E-16,0.,1.));
#118697=DIRECTION('center_axis',(0.,-1.,0.));
#118698=DIRECTION('ref_axis',(0.874651456242421,0.,0.484752338924746));
#118699=DIRECTION('',(0.529924709392058,0.,0.848044693619236));
#118700=DIRECTION('',(-1.,0.,2.81633813779821E-16));
#118701=DIRECTION('',(0.529924185123408,0.,-0.848045021223102));
#118702=DIRECTION('center_axis',(0.,-1.,0.));
#118703=DIRECTION('ref_axis',(0.874649580953487,0.,-0.484755722542694));
#118704=DIRECTION('',(1.,0.,-1.40816906889911E-16));
#118705=DIRECTION('',(0.500005012714997,0.,0.866022509672743));
#118706=DIRECTION('center_axis',(-9.46835258364187E-7,0.999999999998207,
1.6399888598465E-6));
#118707=DIRECTION('ref_axis',(0.866072335963656,1.66721433923257E-10,0.499918702269136));
#118708=DIRECTION('',(1.,0.,-1.40816906889911E-16));
#118709=DIRECTION('center_axis',(9.46924641656899E-7,0.999999999998207,
1.64014402974537E-6));
#118710=DIRECTION('ref_axis',(0.866043284545415,-5.65099970348825E-11,-0.499969028334545));
#118711=DIRECTION('',(0.500005169296866,0.,-0.866022419268931));
#118712=DIRECTION('',(1.,0.,-1.40816906889911E-16));
#118713=DIRECTION('center_axis',(0.,-1.,0.));
#118714=DIRECTION('ref_axis',(2.81633813779821E-16,0.,1.));
#118715=DIRECTION('center_axis',(0.,1.,0.));
#118716=DIRECTION('ref_axis',(0.87464958093593,0.,-0.484755722574372));
#118717=DIRECTION('',(-0.529924185123418,0.,0.848045021223096));
#118718=DIRECTION('',(1.,0.,-2.81633813779821E-16));
#118719=DIRECTION('',(-0.529924709392048,0.,-0.848044693619242));
#118720=DIRECTION('center_axis',(0.,1.,0.));
#118721=DIRECTION('ref_axis',(0.874651456262688,0.,0.484752338888178));
#118722=DIRECTION('',(-1.,0.,1.40816906889911E-16));
#118723=DIRECTION('',(-0.500005169296866,0.,0.866022419268931));
#118724=DIRECTION('center_axis',(9.47055351910275E-7,-0.999999999998206,
1.64037042964274E-6));
#118725=DIRECTION('ref_axis',(0.866072438647891,1.66973546088714E-10,-0.499918524376218));
#118726=DIRECTION('',(-1.,0.,1.40816906889911E-16));
#118727=DIRECTION('center_axis',(-9.46713274271685E-7,-0.999999999998207,
1.63977757417297E-6));
#118728=DIRECTION('ref_axis',(0.86604317834294,-5.62709268826161E-11,0.499969212297776));
#118729=DIRECTION('',(-0.500005012715,0.,-0.866022509672741));
#118730=DIRECTION('',(-1.,0.,1.40816906889911E-16));
#118731=DIRECTION('center_axis',(-2.80862404029962E-16,1.47193748793076E-17,
-1.));
#118732=DIRECTION('ref_axis',(-1.,7.08928067504585E-50,2.80862404029962E-16));
#118733=DIRECTION('',(-0.994521895368273,0.104528463267661,2.80862404029962E-16));
#118734=DIRECTION('center_axis',(2.80862404029962E-16,-1.47193748793076E-17,
1.));
#118735=DIRECTION('ref_axis',(-1.,2.29860575018392E-12,2.80862404029996E-16));
#118736=DIRECTION('',(0.994521895368273,-0.104528463267661,-2.80862404029962E-16));
#118737=DIRECTION('center_axis',(-2.80862404029962E-16,1.47193748793076E-17,
-1.));
#118738=DIRECTION('ref_axis',(-1.,-6.73550486588744E-34,2.80862404029962E-16));
#118739=DIRECTION('center_axis',(-0.104528463267661,-0.994521895368273,
1.47193748793076E-17));
#118740=DIRECTION('ref_axis',(2.80862404029962E-16,-1.47193748793076E-17,
1.));
#118741=DIRECTION('center_axis',(-0.104528463267661,-0.994521895368273,
6.20272161839949E-15));
#118742=DIRECTION('ref_axis',(0.869860024050468,-0.091425972616011,0.484752338921779));
#118743=DIRECTION('',(0.527021726387064,-0.0553922155203117,0.84804469361924));
#118744=DIRECTION('',(-0.994521895368273,0.104528463267661,2.80862404029962E-16));
#118745=DIRECTION('',(0.527021204990404,-0.0553921607193148,-0.848045021223112));
#118746=DIRECTION('center_axis',(-0.104528463267662,-0.994521895368273,
-2.75676579358242E-16));
#118747=DIRECTION('ref_axis',(0.869858159031523,-0.0914257765946247,-0.484755722545241));
#118748=DIRECTION('',(0.994521895368273,-0.104528463267661,-1.40045497140051E-16));
#118749=DIRECTION('',(0.497265932938997,-0.0522647556052269,0.866022509672719));
#118750=DIRECTION('center_axis',(0.104527521619062,0.994521994337726,1.6399888905836E-6));
#118751=DIRECTION('ref_axis',(0.861327901106544,-0.0905292101911616,0.499918702268239));
#118752=DIRECTION('',(0.994521895368273,-0.104528463267661,-1.40045497140051E-16));
#118753=DIRECTION('center_axis',(0.104529405004776,0.99452179638591,1.64014405953898E-6));
#118754=DIRECTION('ref_axis',(0.861299008813205,-0.0905261737132212,-0.499969028330989));
#118755=DIRECTION('',(0.497266088663028,-0.0522647719724816,-0.866022419268946));
#118756=DIRECTION('',(0.994521895368273,-0.104528463267661,-1.40045497140051E-16));
#118757=DIRECTION('center_axis',(-0.104528463267661,-0.994521895368273,
1.47193748793076E-17));
#118758=DIRECTION('ref_axis',(2.80862404029962E-16,-1.47193748793076E-17,
1.));
#118759=DIRECTION('center_axis',(0.104528463267664,0.994521895368272,1.32324758076483E-14));
#118760=DIRECTION('ref_axis',(0.869858159015868,-0.0914257765929747,-0.484755722573645));
#118761=DIRECTION('',(-0.527021204990425,0.055392160719319,0.848045021223099));
#118762=DIRECTION('',(0.994521895368273,-0.104528463267661,-2.80862404029962E-16));
#118763=DIRECTION('',(-0.52702172638706,0.0553922155203111,-0.848044693619242));
#118764=DIRECTION('center_axis',(0.104528463267665,0.994521895368272,-9.6142185097091E-15));
#118765=DIRECTION('ref_axis',(0.869860024069494,-0.0914259726180126,0.484752338887261));
#118766=DIRECTION('',(-0.994521895368273,0.104528463267661,1.40045497140051E-16));
#118767=DIRECTION('',(-0.497266088663009,0.0522647719724833,0.866022419268957));
#118768=DIRECTION('center_axis',(-0.104527521400192,-0.994521994360729,
1.64037043556414E-6));
#118769=DIRECTION('ref_axis',(0.8613280032289,-0.0905292209244034,-0.49991852437426));
#118770=DIRECTION('',(-0.994521895368273,0.104528463267661,1.40045497140051E-16));
#118771=DIRECTION('center_axis',(-0.104529404794561,-0.994521796408005,
1.63977758411581E-6));
#118772=DIRECTION('ref_axis',(0.861298903190469,-0.090526162611589,0.499969212297833));
#118773=DIRECTION('',(-0.497265932938974,0.0522647556052289,-0.866022509672732));
#118774=DIRECTION('',(-0.994521895368273,0.104528463267661,1.40045497140051E-16));
#118775=DIRECTION('center_axis',(-2.78556626507032E-16,2.92774812072093E-17,
-1.));
#118776=DIRECTION('ref_axis',(-1.,5.40378097023072E-49,2.78556626507032E-16));
#118777=DIRECTION('',(-0.978147600733804,0.207911690817766,2.78556626507032E-16));
#118778=DIRECTION('center_axis',(2.78556626507032E-16,-2.92774812072093E-17,
1.));
#118779=DIRECTION('ref_axis',(-1.,2.43272069155864E-12,2.78556626507103E-16));
#118780=DIRECTION('',(0.978147600733804,-0.207911690817766,-2.78556626507032E-16));
#118781=DIRECTION('center_axis',(-2.78556626507032E-16,2.92774812072093E-17,
-1.));
#118782=DIRECTION('ref_axis',(-1.,-1.27221405500129E-33,2.78556626507032E-16));
#118783=DIRECTION('center_axis',(-0.207911690817766,-0.978147600733804,
2.92774812072093E-17));
#118784=DIRECTION('ref_axis',(2.78556626507032E-16,-2.92774812072093E-17,
1.));
#118785=DIRECTION('center_axis',(-0.207911690817774,-0.978147600733803,
1.44730171095997E-14));
#118786=DIRECTION('ref_axis',(0.855538223402714,-0.181850263143766,0.484752338923156));
#118787=DIRECTION('',(0.518344583061382,-0.110177542335815,0.848044693619247));
#118788=DIRECTION('',(-0.978147600733804,0.207911690817766,2.78556626507032E-16));
#118789=DIRECTION('',(0.518344070249263,-0.110177433334233,-0.848045021223111));
#118790=DIRECTION('center_axis',(-0.207911690817754,-0.978147600733807,
2.06757434518653E-14));
#118791=DIRECTION('ref_axis',(0.855536389092462,-0.181849873249085,-0.484755722542728));
#118792=DIRECTION('',(0.978147600733804,-0.207911690817766,-1.37739719617121E-16));
#118793=DIRECTION('',(0.489078703542068,-0.103956887610929,0.866022509672733));
#118794=DIRECTION('center_axis',(0.207910764672729,0.978147797590176,1.63998893124938E-6));
#118795=DIRECTION('ref_axis',(0.847146577519436,-0.180066563577629,0.499918702269128));
#118796=DIRECTION('',(0.978147600733804,-0.207911690817766,-1.37739719617121E-16));
#118797=DIRECTION('center_axis',(0.207912617049499,0.978147403855338,1.64014410136726E-6));
#118798=DIRECTION('ref_axis',(0.847118160895452,-0.180060523665948,-0.499969028339007));
#118799=DIRECTION('',(0.489078856702189,-0.103956920166141,-0.866022419268953));
#118800=DIRECTION('',(0.978147600733804,-0.207911690817766,-1.37739719617121E-16));
#118801=DIRECTION('center_axis',(-0.207911690817766,-0.978147600733804,
2.92774812072093E-17));
#118802=DIRECTION('ref_axis',(2.78556626507032E-16,-2.92774812072093E-17,
1.));
#118803=DIRECTION('center_axis',(0.207911690817771,0.978147600733803,9.09732711775842E-15));
#118804=DIRECTION('ref_axis',(0.85553638907625,-0.18184987324564,-0.484755722572633));
#118805=DIRECTION('',(-0.518344070249254,0.110177433334231,0.848045021223118));
#118806=DIRECTION('',(0.978147600733804,-0.207911690817766,-2.78556626507032E-16));
#118807=DIRECTION('',(-0.518344583061409,0.110177542335818,-0.84804469361923));
#118808=DIRECTION('center_axis',(0.20791169081778,0.978147600733801,-1.84014074701936E-14));
#118809=DIRECTION('ref_axis',(0.855538223422332,-0.18185026314794,0.484752338886967));
#118810=DIRECTION('',(-0.978147600733804,0.207911690817766,1.37739719617121E-16));
#118811=DIRECTION('',(-0.489078856702197,0.103956920166125,0.86602241926895));
#118812=DIRECTION('center_axis',(-0.207910764457494,-0.978147797635925,
1.64037038904585E-6));
#118813=DIRECTION('ref_axis',(0.847146677957487,-0.180066584926125,-0.499918524380359));
#118814=DIRECTION('',(-0.978147600733804,0.207911690817766,1.37739719617121E-16));
#118815=DIRECTION('center_axis',(-0.207912616842688,-0.978147403899298,
1.63977753411228E-6));
#118816=DIRECTION('ref_axis',(0.847118057017983,-0.180060501585866,0.499969212294841));
#118817=DIRECTION('',(-0.489078703542045,0.103956887610933,-0.866022509672745));
#118818=DIRECTION('',(-0.978147600733804,0.207911690817766,1.37739719617121E-16));
#118819=DIRECTION('center_axis',(-2.74741743792087E-16,4.3514817324298E-17,
-1.));
#118820=DIRECTION('ref_axis',(-1.,-3.66113503437316E-49,2.74741743792087E-16));
#118821=DIRECTION('',(-0.951056516295151,0.309016994374954,2.74741743792088E-16));
#118822=DIRECTION('center_axis',(2.74741743792087E-16,-4.3514817324298E-17,
1.));
#118823=DIRECTION('ref_axis',(-1.,2.73292499741728E-12,2.74741743792206E-16));
#118824=DIRECTION('',(0.951056516295151,-0.309016994374954,-2.74741743792088E-16));
#118825=DIRECTION('center_axis',(-2.74741743792087E-16,4.3514817324298E-17,
-1.));
#118826=DIRECTION('ref_axis',(-1.,-1.72487465929319E-33,2.74741743792087E-16));
#118827=DIRECTION('center_axis',(-0.309016994374955,-0.951056516295151,
4.3514817324298E-17));
#118828=DIRECTION('ref_axis',(2.74741743792087E-16,-4.3514817324298E-17,
1.));
#118829=DIRECTION('center_axis',(-0.309016994374931,-0.951056516295159,
-5.10001555290581E-14));
#118830=DIRECTION('ref_axis',(0.831842966947536,-0.270282164134083,0.484752338922586));
#118831=DIRECTION('',(0.50398834801313,-0.163755740941351,0.848044693619237));
#118832=DIRECTION('',(-0.951056516295151,0.309016994374955,2.74741743792087E-16));
#118833=DIRECTION('',(0.50398784940401,-0.163755578933432,-0.848045021223106));
#118834=DIRECTION('center_axis',(-0.309016994374948,-0.951056516295153,
1.61270798924553E-14));
#118835=DIRECTION('ref_axis',(0.83184118344023,-0.27028158463743,-0.484755722543466));
#118836=DIRECTION('',(0.951056516295151,-0.309016994374955,-1.33924836902177E-16));
#118837=DIRECTION('',(0.475533025522889,-0.154510046201595,0.866022509672715));
#118838=DIRECTION('center_axis',(0.30901609388058,0.951056808881625,1.63998881953568E-6));
#118839=DIRECTION('ref_axis',(0.823683738751792,-0.267631070011922,0.499918702270823));
#118840=DIRECTION('',(0.951056516295151,-0.309016994374955,-1.33924836902177E-16));
#118841=DIRECTION('center_axis',(0.309017894953228,0.951056223677647,1.64014400566146E-6));
#118842=DIRECTION('ref_axis',(0.823656109143692,-0.267622092842761,-0.499969028333491));
#118843=DIRECTION('',(0.475533174441011,-0.154510094588075,-0.866022419268947));
#118844=DIRECTION('',(0.951056516295151,-0.309016994374955,-1.33924836902177E-16));
#118845=DIRECTION('center_axis',(-0.309016994374955,-0.951056516295151,
4.3514817324298E-17));
#118846=DIRECTION('ref_axis',(2.74741743792087E-16,-4.3514817324298E-17,
1.));
#118847=DIRECTION('center_axis',(0.309016994374951,0.951056516295153,1.18540929110179E-14));
#118848=DIRECTION('ref_axis',(0.831841183424048,-0.27028158463216,-0.484755722574172));
#118849=DIRECTION('',(-0.503987849403999,0.16375557893344,0.848045021223111));
#118850=DIRECTION('',(0.951056516295151,-0.309016994374955,-2.74741743792087E-16));
#118851=DIRECTION('',(-0.503988348013112,0.163755740941343,-0.848044693619249));
#118852=DIRECTION('center_axis',(0.309016994374947,0.951056516295154,3.17027993868513E-14));
#118853=DIRECTION('ref_axis',(0.831842966966367,-0.270282164140207,0.484752338886856));
#118854=DIRECTION('',(-0.951056516295151,0.309016994374955,1.33924836902177E-16));
#118855=DIRECTION('',(-0.475533174441046,0.154510094588057,0.86602241926893));
#118856=DIRECTION('center_axis',(-0.309016093671271,-0.951056808949632,
1.64037037088597E-6));
#118857=DIRECTION('ref_axis',(0.823683836409809,-0.267631101742673,-0.499918524378945));
#118858=DIRECTION('',(-0.951056516295151,0.309016994374955,1.33924836902177E-16));
#118859=DIRECTION('center_axis',(-0.309017894752234,-0.951056223742955,
1.63977758583762E-6));
#118860=DIRECTION('ref_axis',(0.82365600813909,-0.267622060024133,0.499969212296936));
#118861=DIRECTION('',(-0.475533025522828,0.154510046201581,-0.866022509672751));
#118862=DIRECTION('',(-0.951056516295151,0.309016994374955,1.33924836902177E-16));
#118863=DIRECTION('center_axis',(-2.69459552538469E-16,5.72753959967207E-17,
-1.));
#118864=DIRECTION('ref_axis',(-1.,-2.14642227784473E-49,2.69459552538469E-16));
#118865=DIRECTION('',(-0.913545457642598,0.406736643075807,2.69459552538469E-16));
#118866=DIRECTION('center_axis',(2.69459552538469E-16,-5.72753959967207E-17,
1.));
#118867=DIRECTION('ref_axis',(-1.,1.34203759216689E-12,2.69459552538546E-16));
#118868=DIRECTION('',(0.913545457642598,-0.406736643075807,-2.69459552538469E-16));
#118869=DIRECTION('center_axis',(-2.69459552538469E-16,5.72753959967207E-17,
-1.));
#118870=DIRECTION('ref_axis',(-1.,-1.96778773707772E-33,2.69459552538469E-16));
#118871=DIRECTION('center_axis',(-0.406736643075807,-0.913545457642598,
5.72753959967207E-17));
#118872=DIRECTION('ref_axis',(2.69459552538469E-16,-5.72753959967207E-17,
1.));
#118873=DIRECTION('center_axis',(-0.406736643075794,-0.913545457642604,
-3.39082115139216E-14));
#118874=DIRECTION('ref_axis',(0.79903386487193,-0.355752797173939,0.484752338922407));
#118875=DIRECTION('',(0.484110311157676,-0.215539797381039,0.848044693619245));
#118876=DIRECTION('',(-0.913545457642598,0.406736643075807,2.69459552538469E-16));
#118877=DIRECTION('',(0.484109832214419,-0.215539584141775,-0.848045021223117));
#118878=DIRECTION('center_axis',(-0.406736643075826,-0.913545457642589,
-5.91326262723355E-14));
#118879=DIRECTION('ref_axis',(0.799032151707498,-0.355752034423976,-0.484755722545787));
#118880=DIRECTION('',(0.913545457642598,-0.406736643075807,-1.28642645648558E-16));
#118881=DIRECTION('',(0.456777308164325,-0.20337036039277,0.866022509672739));
#118882=DIRECTION('center_axis',(0.406735778098031,0.913545842753553,1.63998883072505E-6));
#118883=DIRECTION('ref_axis',(0.791196448575512,-0.352263354437553,0.49991870227258));
#118884=DIRECTION('',(0.913545457642598,-0.406736643075807,-1.28642645648558E-16));
#118885=DIRECTION('center_axis',(0.406737508133729,0.913545072492033,1.64014393715232E-6));
#118886=DIRECTION('ref_axis',(0.791169908694848,-0.352251538365742,-0.499969028335509));
#118887=DIRECTION('',(0.456777451208943,-0.203370424080329,-0.866022419268952));
#118888=DIRECTION('',(0.913545457642598,-0.406736643075807,-1.28642645648558E-16));
#118889=DIRECTION('center_axis',(-0.406736643075807,-0.913545457642598,
5.72753959967207E-17));
#118890=DIRECTION('ref_axis',(2.69459552538469E-16,-5.72753959967207E-17,
1.));
#118891=DIRECTION('center_axis',(0.406736643075835,0.913545457642586,4.19028400575536E-14));
#118892=DIRECTION('ref_axis',(0.799032151693359,-0.355752034417699,-0.484755722573699));
#118893=DIRECTION('',(-0.484109832214429,0.215539584141774,0.848045021223112));
#118894=DIRECTION('',(0.913545457642598,-0.406736643075807,-2.69459552538469E-16));
#118895=DIRECTION('',(-0.484110311157675,0.215539797381046,-0.848044693619243));
#118896=DIRECTION('center_axis',(0.406736643075761,0.913545457642618,6.54731726467587E-14));
#118897=DIRECTION('ref_axis',(0.799033864888832,-0.355752797181447,0.484752338889038));
#118898=DIRECTION('',(-0.913545457642598,0.406736643075807,1.28642645648558E-16));
#118899=DIRECTION('',(-0.45677745120894,0.203370424080363,0.866022419268946));
#118900=DIRECTION('center_axis',(-0.406735777896922,-0.913545842843092,
1.6403704946483E-6));
#118901=DIRECTION('ref_axis',(0.791196542383054,-0.352263396203092,-0.499918524378287));
#118902=DIRECTION('',(-0.913545457642598,0.406736643075807,1.28642645648558E-16));
#118903=DIRECTION('center_axis',(-0.406737507940716,-0.913545072577969,
1.63977761028004E-6));
#118904=DIRECTION('ref_axis',(0.79116981167336,-0.352251495168743,0.499969212300243));
#118905=DIRECTION('',(-0.456777308164316,0.203370360392784,-0.86602250967274));
#118906=DIRECTION('',(-0.913545457642598,0.406736643075807,1.28642645648558E-16));
#118907=DIRECTION('center_axis',(-2.6276792553892E-16,7.04084534449562E-17,
-1.));
#118908=DIRECTION('ref_axis',(-1.,-1.29000548981482E-48,2.6276792553892E-16));
#118909=DIRECTION('',(-0.866025403784435,0.500000000000007,2.6276792553892E-16));
#118910=DIRECTION('center_axis',(2.6276792553892E-16,-7.04084534449562E-17,
1.));
#118911=DIRECTION('ref_axis',(-1.,-2.95344831741964E-33,2.6276792553892E-16));
#118912=DIRECTION('',(0.866025403784435,-0.500000000000007,-2.6276792553892E-16));
#118913=DIRECTION('center_axis',(-2.6276792553892E-16,7.04084534449562E-17,
-1.));
#118914=DIRECTION('ref_axis',(-1.,-1.94784780003327E-33,2.6276792553892E-16));
#118915=DIRECTION('center_axis',(-0.500000000000007,-0.866025403784435,
7.04084534449562E-17));
#118916=DIRECTION('ref_axis',(2.6276792553892E-16,-7.04084534449563E-17,
1.));
#118917=DIRECTION('center_axis',(-0.500000000000008,-0.866025403784434,
2.67406220882127E-14));
#118918=DIRECTION('ref_axis',(0.757470380563247,-0.437325728121353,0.484752338924217));
#118919=DIRECTION('',(0.458928260426606,-0.264962354696021,0.848044693619239));
#118920=DIRECTION('',(-0.866025403784435,0.500000000000007,2.6276792553892E-16));
#118921=DIRECTION('',(0.458927806396623,-0.264962092561713,-0.848045021223108));
#118922=DIRECTION('center_axis',(-0.49999999999998,-0.86602540378445,3.36325426817012E-14));
#118923=DIRECTION('ref_axis',(0.757468756514672,-0.437324790476473,-0.48475572254366));
#118924=DIRECTION('',(0.866025403784435,-0.500000000000007,-1.2195101864901E-16));
#118925=DIRECTION('',(0.433017043030766,-0.250002506357508,0.866022509672731));
#118926=DIRECTION('center_axis',(0.499999180015706,0.866025877200521,1.63998891403729E-6));
#118927=DIRECTION('ref_axis',(0.750040644540434,-0.433036167836086,0.499918702273888));
#118928=DIRECTION('',(0.866025403784435,-0.500000000000007,-1.2195101864901E-16));
#118929=DIRECTION('center_axis',(0.500000820059955,0.866024930320532,1.64014408707965E-6));
#118930=DIRECTION('ref_axis',(0.750015485168957,-0.43302164232397,-0.499969028326582));
#118931=DIRECTION('',(0.433017178634565,-0.25000258464842,-0.866022419268965));
#118932=DIRECTION('',(0.866025403784435,-0.500000000000007,-1.2195101864901E-16));
#118933=DIRECTION('center_axis',(-0.500000000000007,-0.866025403784435,
7.04084534449562E-17));
#118934=DIRECTION('ref_axis',(2.6276792553892E-16,-7.04084534449563E-17,
1.));
#118935=DIRECTION('center_axis',(0.499999999999996,0.866025403784441,-1.68162713388849E-14));
#118936=DIRECTION('ref_axis',(0.757468756500421,-0.437324790468254,-0.484755722573343));
#118937=DIRECTION('',(-0.458927806396634,0.264962092561705,0.848045021223105));
#118938=DIRECTION('',(0.866025403784435,-0.500000000000007,-2.6276792553892E-16));
#118939=DIRECTION('',(-0.458928260426591,0.264962354696021,-0.848044693619248));
#118940=DIRECTION('center_axis',(0.499999999999975,0.866025403784453,5.47217885068675E-14));
#118941=DIRECTION('ref_axis',(0.757470380580991,-0.437325728131605,0.48475233888724));
#118942=DIRECTION('',(-0.866025403784435,0.500000000000007,1.2195101864901E-16));
#118943=DIRECTION('',(-0.4330171786346,0.25000258464842,0.866022419268947));
#118944=DIRECTION('center_axis',(-0.499999179825081,-0.866025877310578,
1.64037050618159E-6));
#118945=DIRECTION('ref_axis',(0.750040733469961,-0.433036219179273,-0.499918524376487));
#118946=DIRECTION('',(-0.866025403784435,0.500000000000007,1.2195101864901E-16));
#118947=DIRECTION('center_axis',(-0.500000819876874,-0.866024930426235,
1.63977758687028E-6));
#118948=DIRECTION('ref_axis',(0.750015393191711,-0.433021589220595,0.499969212296472));
#118949=DIRECTION('',(-0.433017043030732,0.250002506357505,-0.866022509672749));
#118950=DIRECTION('',(-0.866025403784435,0.500000000000007,1.2195101864901E-16));
#118951=DIRECTION('center_axis',(-2.54740177659162E-16,8.27701011433327E-17,
-1.));
#118952=DIRECTION('ref_axis',(-1.,5.97523333326789E-49,2.54740177659162E-16));
#118953=DIRECTION('',(-0.809016994374943,0.58778525229248,2.54740177659162E-16));
#118954=DIRECTION('center_axis',(2.54740177659162E-16,-8.27701011433327E-17,
1.));
#118955=DIRECTION('ref_axis',(-1.,1.29496413592278E-12,2.54740177659269E-16));
#118956=DIRECTION('',(0.809016994374943,-0.58778525229248,-2.54740177659162E-16));
#118957=DIRECTION('center_axis',(-2.54740177659162E-16,8.27701011433327E-17,
-1.));
#118958=DIRECTION('ref_axis',(-1.,-1.62537491717902E-33,2.54740177659162E-16));
#118959=DIRECTION('center_axis',(-0.58778525229248,-0.809016994374943,8.27701011433327E-17));
#118960=DIRECTION('ref_axis',(2.54740177659162E-16,-8.27701011433327E-17,
1.));
#118961=DIRECTION('center_axis',(-0.587785252292429,-0.809016994374979,
-1.15232783844045E-13));
#118962=DIRECTION('ref_axis',(0.707607892254803,-0.51410722687536,0.484752338924985));
#118963=DIRECTION('',(0.428718095637373,-0.311481929006023,0.848044693619241));
#118964=DIRECTION('',(-0.809016994374943,0.58778525229248,2.54740177659162E-16));
#118965=DIRECTION('',(0.428717671495124,-0.311481620848633,-0.848045021223112));
#118966=DIRECTION('center_axis',(-0.58778525229247,-0.809016994374949,3.08757768881199E-14));
#118967=DIRECTION('ref_axis',(0.707606375113238,-0.514106124607496,-0.484755722545042));
#118968=DIRECTION('',(0.809016994374943,-0.58778525229248,-1.13923270769252E-16));
#118969=DIRECTION('',(0.404512552559091,-0.293895572546238,0.866022509672727));
#118970=DIRECTION('center_axis',(0.587784486285597,0.809017550909304,1.63998890801182E-6));
#118971=DIRECTION('ref_axis',(0.700667238252392,-0.509064546364368,0.499918702265284));
#118972=DIRECTION('',(0.809016994374943,-0.58778525229248,-1.13923270769252E-16));
#118973=DIRECTION('center_axis',(0.587786018369505,0.809016437785187,1.64014391821798E-6));
#118974=DIRECTION('ref_axis',(0.700643735029245,-0.50904747054913,-0.499969028332557));
#118975=DIRECTION('',(0.404512679236492,-0.29389566458268,-0.866022419268936));
#118976=DIRECTION('',(0.809016994374943,-0.58778525229248,-1.13923270769252E-16));
#118977=DIRECTION('center_axis',(-0.58778525229248,-0.809016994374943,8.27701011433327E-17));
#118978=DIRECTION('ref_axis',(2.54740177659162E-16,-8.27701011433327E-17,
1.));
#118979=DIRECTION('center_axis',(0.587785252292486,0.809016994374938,3.58379553123822E-15));
#118980=DIRECTION('ref_axis',(0.70760637510063,-0.514106124598336,-0.48475572257316));
#118981=DIRECTION('',(-0.428717671495123,0.311481620848639,0.84804502122311));
#118982=DIRECTION('',(0.809016994374943,-0.58778525229248,-2.54740177659162E-16));
#118983=DIRECTION('',(-0.428718095637372,0.311481929006025,-0.84804469361924));
#118984=DIRECTION('center_axis',(0.587785252292497,0.80901699437493,-3.52865941001464E-14));
#118985=DIRECTION('ref_axis',(0.707607892272525,-0.514107226888236,0.484752338885458));
#118986=DIRECTION('',(-0.809016994374943,0.58778525229248,1.13923270769252E-16));
#118987=DIRECTION('',(-0.404512679236479,0.293895664582671,0.866022419268945));
#118988=DIRECTION('center_axis',(-0.587784486107549,-0.809017551038662,
1.64037043199241E-6));
#118989=DIRECTION('ref_axis',(0.700667321322997,-0.509064606718372,-0.499918524378449));
#118990=DIRECTION('',(-0.809016994374943,0.58778525229248,1.13923270769252E-16));
#118991=DIRECTION('center_axis',(-0.587786018198577,-0.809016437909375,
1.63977768068271E-6));
#118992=DIRECTION('ref_axis',(0.70064364911207,-0.509047408126312,0.499969212290924));
#118993=DIRECTION('',(-0.404512552559121,0.293895572546191,-0.866022509672728));
#118994=DIRECTION('',(-0.809016994374943,0.58778525229248,1.13923270769252E-16));
#118995=DIRECTION('center_axis',(-2.45464262584879E-16,9.42249022928256E-17,
-1.));
#118996=DIRECTION('ref_axis',(-1.,8.38955225566875E-49,2.45464262584879E-16));
#118997=DIRECTION('',(-0.743144825477389,0.669130606358864,2.45464262584879E-16));
#118998=DIRECTION('center_axis',(2.45464262584879E-16,-9.42249022928256E-17,
1.));
#118999=DIRECTION('ref_axis',(-1.,-7.62234719786647E-12,2.4546426258416E-16));
#119000=DIRECTION('',(0.743144825477389,-0.669130606358864,-2.45464262584879E-16));
#119001=DIRECTION('center_axis',(-2.45464262584879E-16,9.42249022928256E-17,
-1.));
#119002=DIRECTION('ref_axis',(-1.,-9.76293207909489E-34,2.45464262584879E-16));
#119003=DIRECTION('center_axis',(-0.669130606358865,-0.743144825477389,
9.42249022928256E-17));
#119004=DIRECTION('ref_axis',(2.45464262584879E-16,-9.42249022928256E-17,
1.));
#119005=DIRECTION('center_axis',(-0.669130606358877,-0.743144825477377,
4.76920373325794E-14));
#119006=DIRECTION('ref_axis',(0.649992703803605,-0.585256059268853,0.484752338922848));
#119007=DIRECTION('',(0.393810805677312,-0.35458884212006,0.848044693619234));
#119008=DIRECTION('',(-0.743144825477389,0.669130606358864,2.45464262584879E-16));
#119009=DIRECTION('',(0.393810416069776,-0.354588491315847,-0.848045021223108));
#119010=DIRECTION('center_axis',(-0.669130606358856,-0.743144825477396,
-2.75676579358212E-16));
#119011=DIRECTION('ref_axis',(0.649991310190513,-0.585254804453987,-0.484755722545227));
#119012=DIRECTION('',(0.743144825477389,-0.669130606358864,-1.04647355694968E-16));
#119013=DIRECTION('',(0.37157613791192,-0.334568657340491,0.866022509672724));
#119014=DIRECTION('center_axis',(0.669129902721955,0.743145459032495,1.63998880765904E-6));
#119015=DIRECTION('ref_axis',(0.64361717507148,-0.579515507189562,0.499918702270512));
#119016=DIRECTION('',(0.743144825477389,-0.669130606358864,-1.04647355694968E-16));
#119017=DIRECTION('center_axis',(0.669131310059846,0.743144191859766,1.64014407726852E-6));
#119018=DIRECTION('ref_axis',(0.643595585511056,-0.579496068162464,-0.499969028335681));
#119019=DIRECTION('',(0.371576254274848,-0.334568762114175,-0.86602241926896));
#119020=DIRECTION('',(0.743144825477389,-0.669130606358864,-1.04647355694968E-16));
#119021=DIRECTION('center_axis',(-0.669130606358865,-0.743144825477389,
9.42249022928256E-17));
#119022=DIRECTION('ref_axis',(2.45464262584879E-16,-9.42249022928256E-17,
1.));
#119023=DIRECTION('center_axis',(0.669130606358884,0.743144825477371,6.75407619348737E-14));
#119024=DIRECTION('ref_axis',(0.649991310179091,-0.585254804443703,-0.484755722572959));
#119025=DIRECTION('',(-0.393810416069765,0.354588491315848,0.848045021223112));
#119026=DIRECTION('',(0.743144825477389,-0.669130606358864,-2.45464262584879E-16));
#119027=DIRECTION('',(-0.393810805677311,0.354588842120039,-0.848044693619244));
#119028=DIRECTION('center_axis',(0.669130606358803,0.743144825477444,1.49140995376402E-13));
#119029=DIRECTION('ref_axis',(0.649992703817709,-0.585256059281564,0.48475233888859));
#119030=DIRECTION('',(-0.743144825477389,0.669130606358864,1.04647355694968E-16));
#119031=DIRECTION('',(-0.371576254274903,0.334568762114161,0.866022419268941));
#119032=DIRECTION('center_axis',(-0.669129902558327,-0.743145459179825,
1.64037054921456E-6));
#119033=DIRECTION('ref_axis',(0.643617251381923,-0.579515575899465,-0.499918524375213));
#119034=DIRECTION('',(-0.743144825477389,0.669130606358864,1.04647355694968E-16));
#119035=DIRECTION('center_axis',(-0.669131309902758,-0.743144192001209,
1.63977761561624E-6));
#119036=DIRECTION('ref_axis',(0.643595506588468,-0.579495997099911,0.499969212296431));
#119037=DIRECTION('',(-0.371576137911887,0.334568657340422,-0.866022509672765));
#119038=DIRECTION('',(-0.743144825477389,0.669130606358864,1.04647355694968E-16));
#119039=DIRECTION('center_axis',(-2.35041809182734E-16,1.0464735569497E-16,
-1.));
#119040=DIRECTION('ref_axis',(-1.,-8.2261945837542E-49,2.35041809182734E-16));
#119041=DIRECTION('',(-0.669130606358852,0.7431448254774,2.35041809182734E-16));
#119042=DIRECTION('center_axis',(2.35041809182734E-16,-1.0464735569497E-16,
1.));
#119043=DIRECTION('ref_axis',(-1.,3.73923114693753E-12,2.35041809183126E-16));
#119044=DIRECTION('',(0.669130606358852,-0.7431448254774,-2.35041809182734E-16));
#119045=DIRECTION('center_axis',(-2.35041809182734E-16,1.0464735569497E-16,
-1.));
#119046=DIRECTION('ref_axis',(-1.,6.39873354143184E-36,2.35041809182734E-16));
#119047=DIRECTION('center_axis',(-0.7431448254774,-0.669130606358852,1.0464735569497E-16));
#119048=DIRECTION('ref_axis',(2.35041809182734E-16,-1.0464735569497E-16,
1.));
#119049=DIRECTION('center_axis',(-0.743144825477404,-0.669130606358848,
1.40595023350398E-14));
#119050=DIRECTION('ref_axis',(0.585256059269162,-0.649992703803956,0.484752338922004));
#119051=DIRECTION('',(0.354588842120045,-0.393810805677304,0.848044693619245));
#119052=DIRECTION('',(-0.669130606358852,0.7431448254774,2.35041809182734E-16));
#119053=DIRECTION('',(0.354588491315847,-0.393810416069776,-0.848045021223108));
#119054=DIRECTION('center_axis',(-0.743144825477429,-0.66913060635882,-8.628676933912E-14));
#119055=DIRECTION('ref_axis',(0.585254804454475,-0.649991310191057,-0.484755722543908));
#119056=DIRECTION('',(0.669130606358852,-0.7431448254774,-9.42249022928238E-17));
#119057=DIRECTION('',(0.334568657340465,-0.37157613791193,0.86602250967273));
#119058=DIRECTION('center_axis',(0.743144191919539,0.669131309993462,1.63998908117698E-6));
#119059=DIRECTION('ref_axis',(0.579515507436183,-0.643617174847078,0.499918702273529));
#119060=DIRECTION('',(0.669130606358852,-0.7431448254774,-9.42249022928238E-17));
#119061=DIRECTION('center_axis',(0.743145459092382,0.669129902655443,1.64014420223656E-6));
#119062=DIRECTION('ref_axis',(0.579496068080972,-0.643595585589479,-0.499969028329185));
#119063=DIRECTION('',(0.334568762114161,-0.371576254274903,-0.866022419268941));
#119064=DIRECTION('',(0.669130606358852,-0.7431448254774,-9.42249022928238E-17));
#119065=DIRECTION('center_axis',(-0.7431448254774,-0.669130606358852,1.0464735569497E-16));
#119066=DIRECTION('ref_axis',(2.35041809182734E-16,-1.0464735569497E-16,
1.));
#119067=DIRECTION('center_axis',(0.743144825477371,0.669130606358884,-6.75407619348654E-14));
#119068=DIRECTION('ref_axis',(0.585254804442919,-0.649991310178221,-0.484755722575073));
#119069=DIRECTION('',(-0.354588491315845,0.393810416069787,0.848045021223104));
#119070=DIRECTION('',(0.669130606358852,-0.7431448254774,-2.35041809182734E-16));
#119071=DIRECTION('',(-0.354588842120022,0.393810805677308,-0.848044693619253));
#119072=DIRECTION('center_axis',(0.743144825477395,0.669130606358858,3.80433592642209E-14));
#119073=DIRECTION('ref_axis',(0.585256059281062,-0.649992703817192,0.484752338889889));
#119074=DIRECTION('',(-0.669130606358852,0.7431448254774,9.42249022928238E-17));
#119075=DIRECTION('',(-0.334568762114157,0.371576254274933,0.86602241926893));
#119076=DIRECTION('center_axis',(-0.743144191772411,-0.669131310156863,
1.64037026881083E-6));
#119077=DIRECTION('ref_axis',(0.57951557614673,-0.643617251157489,-0.499918524377524));
#119078=DIRECTION('',(-0.669130606358852,0.7431448254774,9.42249022928238E-17));
#119079=DIRECTION('center_axis',(-0.743145458950914,-0.669129902812561,
1.63977760012488E-6));
#119080=DIRECTION('ref_axis',(0.579495997013497,-0.643595506660734,0.499969212303564));
#119081=DIRECTION('',(-0.33456865734047,0.371576137911897,-0.866022509672742));
#119082=DIRECTION('',(-0.669130606358852,0.7431448254774,9.42249022928238E-17));
#119083=DIRECTION('center_axis',(-2.23587008033241E-16,1.13923270769253E-16,
-1.));
#119084=DIRECTION('ref_axis',(-1.,-9.24278289080685E-49,2.23587008033241E-16));
#119085=DIRECTION('',(-0.587785252292466,0.809016994374953,2.23587008033241E-16));
#119086=DIRECTION('center_axis',(2.23587008033241E-16,-1.13923270769253E-16,
1.));
#119087=DIRECTION('ref_axis',(-1.,1.22390986234677E-12,2.23587008033381E-16));
#119088=DIRECTION('',(0.587785252292466,-0.809016994374953,-2.23587008033241E-16));
#119089=DIRECTION('center_axis',(-2.23587008033241E-16,1.13923270769253E-16,
-1.));
#119090=DIRECTION('ref_axis',(-1.,1.31193432862173E-33,2.23587008033241E-16));
#119091=DIRECTION('center_axis',(-0.809016994374953,-0.587785252292466,
1.13923270769253E-16));
#119092=DIRECTION('ref_axis',(2.23587008033241E-16,-1.13923270769253E-16,
1.));
#119093=DIRECTION('center_axis',(-0.809016994374928,-0.5877852522925,-5.81677449547676E-14));
#119094=DIRECTION('ref_axis',(0.514107226876155,-0.707607892255909,0.484752338922526));
#119095=DIRECTION('',(0.311481929006022,-0.428718095637368,0.848044693619243));
#119096=DIRECTION('',(-0.587785252292466,0.809016994374953,2.23587008033241E-16));
#119097=DIRECTION('',(0.311481620848633,-0.428717671495124,-0.848045021223112));
#119098=DIRECTION('center_axis',(-0.809016994374957,-0.58778525229246,-2.37081858248063E-14));
#119099=DIRECTION('ref_axis',(0.514106124608047,-0.707606375114021,-0.484755722543313));
#119100=DIRECTION('',(0.587785252292466,-0.809016994374953,-8.27701011433307E-17));
#119101=DIRECTION('',(0.293895572546188,-0.40451255255907,0.866022509672753));
#119102=DIRECTION('center_axis',(0.809016437837667,0.587786018297274,1.63998894088962E-6));
#119103=DIRECTION('ref_axis',(0.509064546633985,-0.700667238056223,0.499918702265677));
#119104=DIRECTION('',(0.587785252292466,-0.809016994374953,-8.27701011433307E-17));
#119105=DIRECTION('center_axis',(0.809017550961879,0.587784486213233,1.64014416574423E-6));
#119106=DIRECTION('ref_axis',(0.509047470456718,-0.700643735094342,-0.499969028335422));
#119107=DIRECTION('',(0.293895664582671,-0.404512679236479,-0.866022419268945));
#119108=DIRECTION('',(0.587785252292466,-0.809016994374953,-8.27701011433307E-17));
#119109=DIRECTION('center_axis',(-0.809016994374953,-0.587785252292466,
1.13923270769253E-16));
#119110=DIRECTION('ref_axis',(2.23587008033241E-16,-1.13923270769253E-16,
1.));
#119111=DIRECTION('center_axis',(0.809016994374949,0.587785252292471,6.67137321968949E-14));
#119112=DIRECTION('ref_axis',(0.514106124598002,-0.70760637510014,-0.48475572257423));
#119113=DIRECTION('',(-0.311481620848613,0.428717671495137,0.848045021223112));
#119114=DIRECTION('',(0.587785252292466,-0.809016994374953,-2.23587008033241E-16));
#119115=DIRECTION('',(-0.311481929006029,0.428718095637372,-0.848044693619239));
#119116=DIRECTION('center_axis',(0.809016994374976,0.587785252292435,-6.72650700034043E-14));
#119117=DIRECTION('ref_axis',(0.514107226886512,-0.707607892270182,0.484752338890708));
#119118=DIRECTION('',(-0.587785252292466,0.809016994374953,8.27701011433307E-17));
#119119=DIRECTION('',(-0.293895664582653,0.40451267923649,0.866022419268946));
#119120=DIRECTION('center_axis',(-0.809016437708326,-0.587786018475295,
1.64037045092715E-6));
#119121=DIRECTION('ref_axis',(0.509064606988709,-0.700667321126964,-0.499918524377919));
#119122=DIRECTION('',(-0.587785252292466,0.809016994374953,8.27701011433307E-17));
#119123=DIRECTION('center_axis',(-0.809017550837631,-0.587784486384246,
1.63977765520619E-6));
#119124=DIRECTION('ref_axis',(0.509047408030807,-0.700643649172062,0.499969212304091));
#119125=DIRECTION('',(-0.293895572546191,0.404512552559121,-0.866022509672728));
#119126=DIRECTION('',(-0.587785252292466,0.809016994374953,8.27701011433307E-17));
#119127=DIRECTION('center_axis',(-2.11225360334865E-16,1.21951018649011E-16,
-1.));
#119128=DIRECTION('ref_axis',(-1.,1.27854015281794E-48,2.11225360334865E-16));
#119129=DIRECTION('',(-0.499999999999992,0.866025403784443,2.11225360334865E-16));
#119130=DIRECTION('center_axis',(2.11225360334865E-16,-1.21951018649011E-16,
1.));
#119131=DIRECTION('ref_axis',(-1.,2.39808173319034E-12,2.11225360335157E-16));
#119132=DIRECTION('',(0.499999999999992,-0.866025403784443,-2.11225360334865E-16));
#119133=DIRECTION('center_axis',(-2.11225360334865E-16,1.21951018649011E-16,
-1.));
#119134=DIRECTION('ref_axis',(-1.,2.91189697534881E-33,2.11225360334865E-16));
#119135=DIRECTION('center_axis',(-0.866025403784443,-0.499999999999992,
1.21951018649011E-16));
#119136=DIRECTION('ref_axis',(2.11225360334865E-16,-1.21951018649011E-16,
1.));
#119137=DIRECTION('center_axis',(-0.866025403784462,-0.49999999999996,5.32055676600482E-14));
#119138=DIRECTION('ref_axis',(0.437325728121712,-0.757470380563887,0.484752338922892));
#119139=DIRECTION('',(0.264962354696012,-0.458928260426601,0.848044693619245));
#119140=DIRECTION('',(-0.499999999999992,0.866025403784443,2.11225360334865E-16));
#119141=DIRECTION('',(0.264962092561693,-0.458927806396636,-0.848045021223108));
#119142=DIRECTION('center_axis',(-0.866025403784433,-0.500000000000009,
2.35703475351271E-14));
#119143=DIRECTION('ref_axis',(0.437324790476389,-0.757468756514523,-0.484755722543968));
#119144=DIRECTION('',(0.499999999999992,-0.866025403784443,-7.04084534449541E-17));
#119145=DIRECTION('',(0.250002506357496,-0.433017043030782,0.866022509672727));
#119146=DIRECTION('center_axis',(0.866024930365251,0.500000819982501,1.63998888959419E-6));
#119147=DIRECTION('ref_axis',(0.433036168125046,-0.750040644374085,0.499918702273163));
#119148=DIRECTION('',(0.499999999999992,-0.866025403784443,-7.04084534449541E-17));
#119149=DIRECTION('center_axis',(0.866025877245205,0.499999179938311,1.6401439968823E-6));
#119150=DIRECTION('ref_axis',(0.433021642224347,-0.750015485222529,-0.499969028332501));
#119151=DIRECTION('',(0.250002584648424,-0.433017178634642,-0.866022419268925));
#119152=DIRECTION('',(0.499999999999992,-0.866025403784443,-7.04084534449541E-17));
#119153=DIRECTION('center_axis',(-0.866025403784443,-0.499999999999992,
1.21951018649011E-16));
#119154=DIRECTION('ref_axis',(2.11225360334865E-16,-1.21951018649011E-16,
1.));
#119155=DIRECTION('center_axis',(0.866025403784414,0.500000000000044,-1.1413010384097E-13));
#119156=DIRECTION('ref_axis',(0.437324790468524,-0.75746875650092,-0.484755722572319));
#119157=DIRECTION('',(-0.264962092561688,0.458927806396626,0.848045021223114));
#119158=DIRECTION('',(0.499999999999992,-0.866025403784443,-2.11225360334865E-16));
#119159=DIRECTION('',(-0.264962354696018,0.4589282604266,-0.848044693619243));
#119160=DIRECTION('center_axis',(0.86602540378443,0.500000000000014,4.09379626865015E-14));
#119161=DIRECTION('ref_axis',(0.437325728131046,-0.757470380580035,0.484752338889239));
#119162=DIRECTION('',(-0.499999999999992,0.866025403784443,7.04084534449541E-17));
#119163=DIRECTION('',(-0.250002584648412,0.433017178634622,0.866022419268938));
#119164=DIRECTION('center_axis',(-0.866024930255216,-0.500000820173085,
1.64037040754986E-6));
#119165=DIRECTION('ref_axis',(0.433036219468253,-0.750040733302616,-0.49991852437724));
#119166=DIRECTION('',(-0.499999999999992,0.866025403784443,7.04084534449541E-17));
#119167=DIRECTION('center_axis',(-0.866025877139515,-0.499999180121372,
1.63977754297659E-6));
#119168=DIRECTION('ref_axis',(0.433021589122641,-0.750015393247174,0.499969212298108));
#119169=DIRECTION('',(-0.250002506357496,0.433017043030747,-0.866022509672744));
#119170=DIRECTION('',(-0.499999999999992,0.866025403784443,7.04084534449541E-17));
#119171=DIRECTION('center_axis',(-1.98092302886629E-16,1.28642645648559E-16,
-1.));
#119172=DIRECTION('ref_axis',(-1.,3.58748490176176E-52,1.98092302886629E-16));
#119173=DIRECTION('',(-0.406736643075792,0.913545457642605,1.98092302886629E-16));
#119174=DIRECTION('center_axis',(1.98092302886629E-16,-1.28642645648559E-16,
1.));
#119175=DIRECTION('ref_axis',(-1.,-7.04858393874019E-12,1.98092302885722E-16));
#119176=DIRECTION('',(0.406736643075792,-0.913545457642605,-1.98092302886629E-16));
#119177=DIRECTION('center_axis',(-1.98092302886629E-16,1.28642645648559E-16,
-1.));
#119178=DIRECTION('ref_axis',(-1.,4.76114818715962E-33,1.98092302886629E-16));
#119179=DIRECTION('center_axis',(-0.913545457642605,-0.406736643075792,
1.28642645648559E-16));
#119180=DIRECTION('ref_axis',(1.98092302886629E-16,-1.28642645648559E-16,
1.));
#119181=DIRECTION('center_axis',(-0.913545457642622,-0.406736643075753,
7.88434836827655E-14));
#119182=DIRECTION('ref_axis',(0.355752797173625,-0.799033864871266,0.484752338923733));
#119183=DIRECTION('',(0.215539797381043,-0.484110311157696,0.848044693619233));
#119184=DIRECTION('',(-0.406736643075792,0.913545457642605,1.98092302886629E-16));
#119185=DIRECTION('',(0.21553958414176,-0.48410983221444,-0.848045021223109));
#119186=DIRECTION('center_axis',(-0.91354545764262,-0.406736643075758,-4.30055463798799E-14));
#119187=DIRECTION('ref_axis',(0.355752034424546,-0.799032151708817,-0.484755722543195));
#119188=DIRECTION('',(0.406736643075792,-0.913545457642605,-5.72753959967185E-17));
#119189=DIRECTION('',(0.20337036039277,-0.456777308164325,0.866022509672739));
#119190=DIRECTION('center_axis',(0.913545072528382,0.40673750805209,1.63998879457736E-6));
#119191=DIRECTION('ref_axis',(0.352263354742908,-0.791196448441526,0.499918702269468));
#119192=DIRECTION('',(0.406736643075792,-0.913545457642605,-5.72753959967185E-17));
#119193=DIRECTION('center_axis',(0.91354584278993,0.406735778016327,1.6401441017111E-6));
#119194=DIRECTION('ref_axis',(0.352251538262862,-0.791169908741651,-0.499969028333931));
#119195=DIRECTION('',(0.203370424080329,-0.456777451208978,-0.866022419268934));
#119196=DIRECTION('',(0.406736643075792,-0.913545457642605,-5.72753959967185E-17));
#119197=DIRECTION('center_axis',(-0.913545457642605,-0.406736643075792,
1.28642645648559E-16));
#119198=DIRECTION('ref_axis',(1.98092302886629E-16,-1.28642645648559E-16,
1.));
#119199=DIRECTION('center_axis',(0.91354545764259,0.406736643075824,-5.29299032305855E-14));
#119200=DIRECTION('ref_axis',(0.35575203441816,-0.799032151694434,-0.484755722571589));
#119201=DIRECTION('',(-0.215539584141764,0.484109832214436,0.848045021223111));
#119202=DIRECTION('',(0.406736643075792,-0.913545457642605,-1.98092302886629E-16));
#119203=DIRECTION('',(-0.215539797381044,0.48411031115771,-0.848044693619224));
#119204=DIRECTION('center_axis',(0.913545457642615,0.406736643075768,-3.6802814940392E-14));
#119205=DIRECTION('ref_axis',(0.355752797182121,-0.799033864890364,0.484752338886018));
#119206=DIRECTION('',(-0.406736643075792,0.913545457642605,5.72753959967185E-17));
#119207=DIRECTION('',(-0.203370424080329,0.456777451208908,0.86602241926897));
#119208=DIRECTION('center_axis',(-0.913545072438882,-0.406737508253109,
1.64037028550778E-6));
#119209=DIRECTION('ref_axis',(0.352263396509503,-0.791196542250226,-0.499918524372597));
#119210=DIRECTION('',(-0.406736643075792,0.913545457642605,5.72753959967185E-17));
#119211=DIRECTION('center_axis',(-0.913545842703948,-0.406735778209447,
1.63977759031303E-6));
#119212=DIRECTION('ref_axis',(0.352251495066461,-0.791169811720368,0.499969212297917));
#119213=DIRECTION('',(-0.20337036039277,0.45677730816429,-0.866022509672757));
#119214=DIRECTION('',(-0.406736643075792,0.913545457642605,5.72753959967185E-17));
#119215=DIRECTION('center_axis',(-1.84331724214206E-16,1.33924836902178E-16,
-1.));
#119216=DIRECTION('ref_axis',(-1.,-8.60748644135896E-49,1.84331724214206E-16));
#119217=DIRECTION('',(-0.309016994374938,0.951056516295157,1.84331724214206E-16));
#119218=DIRECTION('center_axis',(1.84331724214206E-16,-1.33924836902178E-16,
1.));
#119219=DIRECTION('ref_axis',(-1.,-6.90292267790937E-12,1.84331724213282E-16));
#119220=DIRECTION('',(0.309016994374938,-0.951056516295157,-1.84331724214206E-16));
#119221=DIRECTION('center_axis',(-1.84331724214206E-16,1.33924836902178E-16,
-1.));
#119222=DIRECTION('ref_axis',(-1.,6.79952878369311E-33,1.84331724214206E-16));
#119223=DIRECTION('center_axis',(-0.951056516295157,-0.309016994374938,
1.33924836902178E-16));
#119224=DIRECTION('ref_axis',(1.84331724214206E-16,-1.33924836902178E-16,
1.));
#119225=DIRECTION('center_axis',(-0.95105651629516,-0.309016994374928,2.99109020265034E-14));
#119226=DIRECTION('ref_axis',(0.270282164134193,-0.831842966947917,0.484752338921869));
#119227=DIRECTION('',(0.163755740941343,-0.503988348013141,0.848044693619232));
#119228=DIRECTION('',(-0.309016994374938,0.951056516295157,1.84331724214206E-16));
#119229=DIRECTION('',(0.163755578933417,-0.503987849404001,-0.848045021223114));
#119230=DIRECTION('center_axis',(-0.951056516295151,-0.309016994374956,
2.37081858248069E-14));
#119231=DIRECTION('ref_axis',(0.270281584637447,-0.831841183440324,-0.484755722543294));
#119232=DIRECTION('',(0.309016994374938,-0.951056516295157,-4.35148173242957E-17));
#119233=DIRECTION('',(0.15451004620159,-0.475533025522892,0.866022509672715));
#119234=DIRECTION('center_axis',(0.951056223705273,0.309017894868205,1.6399888086916E-6));
#119235=DIRECTION('ref_axis',(0.267631070328562,-0.823683738647293,0.499918702273485));
#119236=DIRECTION('',(0.309016994374938,-0.951056516295157,-4.35148173242957E-17));
#119237=DIRECTION('center_axis',(0.951056808909271,0.309016093795493,1.6401440891452E-6));
#119238=DIRECTION('ref_axis',(0.267622092735315,-0.823656109178786,-0.49996902833319));
#119239=DIRECTION('',(0.154510094588032,-0.475533174441048,-0.866022419268934));
#119240=DIRECTION('',(0.309016994374938,-0.951056516295157,-4.35148173242957E-17));
#119241=DIRECTION('center_axis',(-0.951056516295157,-0.309016994374938,
1.33924836902178E-16));
#119242=DIRECTION('ref_axis',(1.84331724214206E-16,-1.33924836902178E-16,
1.));
#119243=DIRECTION('center_axis',(0.951056516295149,0.30901699437496,-5.03109757269963E-14));
#119244=DIRECTION('ref_axis',(0.270281584632175,-0.831841183424126,-0.48475572257403));
#119245=DIRECTION('',(-0.163755578933422,0.503987849404011,0.848045021223107));
#119246=DIRECTION('',(0.309016994374938,-0.951056516295157,-1.84331724214206E-16));
#119247=DIRECTION('',(-0.163755740941338,0.503988348013136,-0.848044693619236));
#119248=DIRECTION('center_axis',(0.951056516295152,0.309016994374954,2.77054898989464E-14));
#119249=DIRECTION('ref_axis',(0.270282164140366,-0.831842966966927,0.484752338885807));
#119250=DIRECTION('',(-0.309016994374938,0.951056516295157,4.35148173242957E-17));
#119251=DIRECTION('',(-0.154510094588047,0.475533174441005,0.866022419268955));
#119252=DIRECTION('center_axis',(-0.951056223637261,-0.309017895077522,
1.64037037174637E-6));
#119253=DIRECTION('ref_axis',(0.26763110206138,-0.823683836310049,-0.499918524372694));
#119254=DIRECTION('',(-0.309016994374938,0.951056516295157,4.35148173242957E-17));
#119255=DIRECTION('center_axis',(-0.951056808843949,-0.309016093996535,
1.63977763110796E-6));
#119256=DIRECTION('ref_axis',(0.267622059916075,-0.823656008170728,0.499969212302656));
#119257=DIRECTION('',(-0.154510046201584,0.475533025522848,-0.86602250967274));
#119258=DIRECTION('',(-0.309016994374938,0.951056516295157,4.35148173242957E-17));
#119259=DIRECTION('center_axis',(-1.70094388097117E-16,1.37739719617122E-16,
-1.));
#119260=DIRECTION('ref_axis',(-1.,-8.13991384035174E-49,1.70094388097117E-16));
#119261=DIRECTION('',(-0.207911690817749,0.978147600733808,1.70094388097117E-16));
#119262=DIRECTION('center_axis',(1.70094388097117E-16,-1.37739719617122E-16,
1.));
#119263=DIRECTION('ref_axis',(-1.,-9.01323460311687E-12,1.70094388095876E-16));
#119264=DIRECTION('',(0.207911690817749,-0.978147600733808,-1.70094388097117E-16));
#119265=DIRECTION('center_axis',(-1.70094388097117E-16,1.37739719617122E-16,
-1.));
#119266=DIRECTION('ref_axis',(-1.,-7.23724578308818E-33,1.70094388097117E-16));
#119267=DIRECTION('center_axis',(-0.978147600733808,-0.207911690817749,
1.37739719617122E-16));
#119268=DIRECTION('ref_axis',(1.70094388097117E-16,-1.37739719617122E-16,
1.));
#119269=DIRECTION('center_axis',(-0.978147600733812,-0.20791169081773,3.10136080919944E-14));
#119270=DIRECTION('ref_axis',(0.181850263143769,-0.855538223402807,0.484752338922991));
#119271=DIRECTION('',(0.110177542335806,-0.518344583061388,0.848044693619244));
#119272=DIRECTION('',(-0.207911690817749,0.978147600733808,1.70094388097117E-16));
#119273=DIRECTION('',(0.110177433334219,-0.518344070249257,-0.848045021223117));
#119274=DIRECTION('center_axis',(-0.978147600733808,-0.20791169081775,-1.72297862098883E-15));
#119275=DIRECTION('ref_axis',(0.181849873248976,-0.85553638909201,-0.484755722543567));
#119276=DIRECTION('',(0.207911690817749,-0.978147600733808,-2.92774812072069E-17));
#119277=DIRECTION('',(0.103956887610952,-0.489078703542055,0.866022509672737));
#119278=DIRECTION('center_axis',(0.978147403873943,0.207912616961972,1.63998880283903E-6));
#119279=DIRECTION('ref_axis',(0.180066563903965,-0.847146577451112,0.499918702267365));
#119280=DIRECTION('',(0.207911690817749,-0.978147600733808,-2.92774812072069E-17));
#119281=DIRECTION('center_axis',(0.978147797608769,0.207910764585256,1.64014411823538E-6));
#119282=DIRECTION('ref_axis',(0.180060523556428,-0.847118160923886,-0.499969028330273));
#119283=DIRECTION('',(0.103956920166112,-0.48907885670221,-0.866022419268945));
#119284=DIRECTION('',(0.207911690817749,-0.978147600733808,-2.92774812072069E-17));
#119285=DIRECTION('center_axis',(-0.978147600733808,-0.207911690817749,
1.37739719617122E-16));
#119286=DIRECTION('ref_axis',(1.70094388097117E-16,-1.37739719617122E-16,
1.));
#119287=DIRECTION('center_axis',(0.978147600733809,0.207911690817741,1.07513865937135E-14));
#119288=DIRECTION('ref_axis',(0.181849873245357,-0.855536389075001,-0.484755722574944));
#119289=DIRECTION('',(-0.110177433334221,0.518344070249267,0.848045021223111));
#119290=DIRECTION('',(0.207911690817749,-0.978147600733808,-1.70094388097117E-16));
#119291=DIRECTION('',(-0.110177542335799,0.518344583061388,-0.848044693619245));
#119292=DIRECTION('center_axis',(0.978147600733805,0.20791169081776,9.71759720336066E-15));
#119293=DIRECTION('ref_axis',(0.181850263147746,-0.855538223421482,0.48475233888854));
#119294=DIRECTION('',(-0.207911690817749,0.978147600733808,2.92774812072069E-17));
#119295=DIRECTION('',(-0.103956920166105,0.489078856702183,0.866022419268961));
#119296=DIRECTION('center_axis',(-0.978147403828172,-0.207912617177303,
1.64037044886142E-6));
#119297=DIRECTION('ref_axis',(0.180066585253005,-0.84714667788922,-0.499918524378303));
#119298=DIRECTION('',(-0.207911690817749,0.978147600733808,2.92774812072069E-17));
#119299=DIRECTION('center_axis',(-0.978147797564805,-0.207910764792092,
1.63977752223455E-6));
#119300=DIRECTION('ref_axis',(0.18006050147523,-0.847118057038833,0.499969212299358));
#119301=DIRECTION('',(-0.103956887610913,0.489078703542031,-0.866022509672756));
#119302=DIRECTION('',(-0.207911690817749,0.978147600733808,2.92774812072069E-17));
#119303=DIRECTION('center_axis',(-1.55536281769216E-16,1.40045497140052E-16,
-1.));
#119304=DIRECTION('ref_axis',(-1.,-1.27395445529282E-48,1.55536281769216E-16));
#119305=DIRECTION('',(-0.104528463267644,0.994521895368274,1.55536281769216E-16));
#119306=DIRECTION('center_axis',(1.55536281769216E-16,-1.40045497140052E-16,
1.));
#119307=DIRECTION('ref_axis',(-1.,2.20623519453511E-12,1.55536281769525E-16));
#119308=DIRECTION('',(0.104528463267644,-0.994521895368274,-1.55536281769216E-16));
#119309=DIRECTION('center_axis',(-1.55536281769216E-16,1.40045497140052E-16,
-1.));
#119310=DIRECTION('ref_axis',(-1.,-5.31960080738386E-33,1.55536281769216E-16));
#119311=DIRECTION('center_axis',(-0.994521895368274,-0.104528463267644,
1.40045497140052E-16));
#119312=DIRECTION('ref_axis',(1.55536281769216E-16,-1.40045497140052E-16,
1.));
#119313=DIRECTION('center_axis',(-0.994521895368274,-0.104528463267649,
-1.28189580113589E-14));
#119314=DIRECTION('ref_axis',(0.091425972615971,-0.869860024050217,0.484752338922238));
#119315=DIRECTION('',(0.0553922155203038,-0.527021726387067,0.848044693619238));
#119316=DIRECTION('',(-0.104528463267644,0.994521895368274,1.55536281769216E-16));
#119317=DIRECTION('',(0.0553921607193063,-0.527021204990403,-0.848045021223113));
#119318=DIRECTION('center_axis',(-0.994521895368274,-0.104528463267645,
2.65338707632273E-15));
#119319=DIRECTION('ref_axis',(0.0914257765947348,-0.86985815903272,-0.484755722543072));
#119320=DIRECTION('',(0.104528463267644,-0.994521895368274,-1.47193748793052E-17));
#119321=DIRECTION('',(0.0522647556052278,-0.497265932938971,0.866022509672734));
#119322=DIRECTION('center_axis',(0.994521796395258,0.104529404915842,1.63998884832503E-6));
#119323=DIRECTION('ref_axis',(0.0905292105225956,-0.86132790107014,0.499918702270942));
#119324=DIRECTION('',(0.104528463267644,-0.994521895368274,-1.47193748793052E-17));
#119325=DIRECTION('center_axis',(0.994521994347068,0.104527521530174,1.64014401740936E-6));
#119326=DIRECTION('ref_axis',(0.0905261736006642,-0.861299008823645,-0.499969028333385));
#119327=DIRECTION('',(0.0522647719724824,-0.497266088663036,-0.866022419268942));
#119328=DIRECTION('',(0.104528463267644,-0.994521895368274,-1.47193748793052E-17));
#119329=DIRECTION('center_axis',(-0.994521895368274,-0.104528463267644,
1.40045497140052E-16));
#119330=DIRECTION('ref_axis',(1.55536281769216E-16,-1.40045497140052E-16,
1.));
#119331=DIRECTION('center_axis',(0.994521895368274,0.104528463267644,-4.41082526921583E-15));
#119332=DIRECTION('ref_axis',(0.0914257765929005,-0.86985815901529,-0.484755722574695));
#119333=DIRECTION('',(-0.0553921607193094,0.527021204990428,0.848045021223097));
#119334=DIRECTION('',(0.104528463267644,-0.994521895368274,-1.55536281769216E-16));
#119335=DIRECTION('',(-0.0553922155203033,0.527021726387038,-0.848044693619256));
#119336=DIRECTION('center_axis',(0.994521895368273,0.104528463267653,1.47142340632461E-14));
#119337=DIRECTION('ref_axis',(0.0914259726180641,-0.869860024070109,0.484752338886148));
#119338=DIRECTION('',(-0.104528463267644,0.994521895368274,1.47193748793052E-17));
#119339=DIRECTION('',(-0.0522647719724787,0.497266088663077,0.866022419268918));
#119340=DIRECTION('center_axis',(-0.99452179637225,-0.104529405134733,1.64037043048663E-6));
#119341=DIRECTION('ref_axis',(0.0905292212563007,-0.86132800319214,-0.499918524377491));
#119342=DIRECTION('',(-0.104528463267644,0.994521895368274,1.47193748793052E-17));
#119343=DIRECTION('center_axis',(-0.994521994324975,-0.104527521740383,
1.63977755580007E-6));
#119344=DIRECTION('ref_axis',(0.0905261624996592,-0.86129890320238,0.499969212297581));
#119345=DIRECTION('',(-0.0522647556052262,0.497265932938956,-0.866022509672743));
#119346=DIRECTION('',(-0.104528463267644,0.994521895368274,1.47193748793052E-17));
#119347=DIRECTION('center_axis',(-1.40816906889909E-16,1.4081690688991E-16,
-1.));
#119348=DIRECTION('ref_axis',(0.,1.,1.40816906889911E-16));
#119349=DIRECTION('',(1.04744440165294E-14,1.,1.40816906889909E-16));
#119350=DIRECTION('',(-1.04744440165294E-14,-1.,-1.40816906889909E-16));
#119351=DIRECTION('center_axis',(-1.,1.04744440165294E-14,1.4081690688991E-16));
#119352=DIRECTION('ref_axis',(1.40816906889909E-16,-1.40816906889911E-16,
1.));
#119353=DIRECTION('center_axis',(-1.,1.0218985244156E-14,-3.06110401690849E-16));
#119354=DIRECTION('ref_axis',(9.08643805832666E-15,0.874651456244175,-0.484752338921582));
#119355=DIRECTION('',(-5.41813057753239E-15,-0.529924709392051,0.84804469361924));
#119356=DIRECTION('',(1.04744440165294E-14,1.,1.40816906889909E-16));
#119357=DIRECTION('',(-5.67613898822991E-15,-0.529924185123396,-0.84804502122311));
#119358=DIRECTION('center_axis',(-1.,1.053745470252E-14,1.67445974214341E-16));
#119359=DIRECTION('ref_axis',(9.29775073408821E-15,0.874649580953058,0.484755722543468));
#119360=DIRECTION('',(-1.04744440165294E-14,-1.,1.4749788077992E-30));
#119361=DIRECTION('',(-5.23017107763447E-15,-0.500005012715,0.866022509672741));
#119362=DIRECTION('center_axis',(0.999999999998207,9.4683525304529E-7,1.63998886848176E-6));
#119363=DIRECTION('ref_axis',(1.66712501830529E-10,-0.866072335961381,0.499918702273076));
#119364=DIRECTION('',(-1.04744440165294E-14,-1.,1.4749788077992E-30));
#119365=DIRECTION('center_axis',(0.999999999998207,-9.46924657962836E-7,
1.64014403941177E-6));
#119366=DIRECTION('ref_axis',(-5.65192953370995E-11,-0.866043284547938,
-0.499969028330174));
#119367=DIRECTION('',(-5.36780659828042E-15,-0.50000516929684,-0.866022419268946));
#119368=DIRECTION('',(-1.04744440165294E-14,-1.,1.4749788077992E-30));
#119369=DIRECTION('center_axis',(-1.,1.04744440165294E-14,1.4081690688991E-16));
#119370=DIRECTION('ref_axis',(1.40816906889909E-16,-1.40816906889911E-16,
1.));
#119371=DIRECTION('center_axis',(1.,-1.03422010861309E-14,-3.74411322160043E-16));
#119372=DIRECTION('ref_axis',(9.22729987696341E-15,0.874649580936984,0.484755722572471));
#119373=DIRECTION('',(5.62453772470057E-15,0.529924185123411,0.8480450212231));
#119374=DIRECTION('',(-1.04744440165294E-14,-1.,-1.40816906889909E-16));
#119375=DIRECTION('',(5.41813057753243E-15,0.529924709392042,-0.848044693619246));
#119376=DIRECTION('center_axis',(1.,-1.04142386870038E-14,9.91450061389626E-17));
#119377=DIRECTION('ref_axis',(9.15688980706914E-15,0.874651456262602,-0.484752338888334));
#119378=DIRECTION('',(1.04744440165294E-14,1.,-1.4749788077992E-30));
#119379=DIRECTION('',(5.50544266490316E-15,0.500005169296855,0.866022419268938));
#119380=DIRECTION('center_axis',(-0.999999999998206,-9.4705534023739E-7,
1.64037042763668E-6));
#119381=DIRECTION('ref_axis',(1.66964445788292E-10,-0.86607243864958,-0.499918524373292));
#119382=DIRECTION('',(1.04744440165294E-14,1.,-1.4749788077992E-30));
#119383=DIRECTION('center_axis',(-0.999999999998207,9.46713293518364E-7,
1.6397775892974E-6));
#119384=DIRECTION('ref_axis',(-5.6280035541352E-11,-0.866043178343455,0.499969212296884));
#119385=DIRECTION('',(5.09253499664393E-15,0.500005012714985,-0.86602250967275));
#119386=DIRECTION('',(1.04744440165294E-14,1.,-1.4749788077992E-30));
#119387=DIRECTION('center_axis',(-1.26097532010602E-16,1.40045497140051E-16,
-1.));
#119388=DIRECTION('ref_axis',(0.,1.,1.40045497140051E-16));
#119389=DIRECTION('',(0.104528463267664,0.994521895368272,1.26097532010602E-16));
#119390=DIRECTION('center_axis',(1.26097532010602E-16,-1.40045497140051E-16,
1.));
#119391=DIRECTION('ref_axis',(1.94422256072357E-12,1.,1.40045497139806E-16));
#119392=DIRECTION('',(-0.104528463267664,-0.994521895368272,-1.26097532010602E-16));
#119393=DIRECTION('center_axis',(-1.26097532010602E-16,1.40045497140051E-16,
-1.));
#119394=DIRECTION('ref_axis',(2.83644037037302E-33,1.,1.40045497140051E-16));
#119395=DIRECTION('center_axis',(-0.994521895368272,0.104528463267664,1.40045497140051E-16));
#119396=DIRECTION('ref_axis',(1.26097532010602E-16,-1.40045497140051E-16,
1.));
#119397=DIRECTION('center_axis',(-0.994521895368272,0.104528463267663,-3.37703732557294E-15));
#119398=DIRECTION('ref_axis',(0.0914259726159238,0.869860024049577,-0.484752338923395));
#119399=DIRECTION('',(-0.0553922155203143,-0.527021726387072,0.848044693619234));
#119400=DIRECTION('',(0.104528463267664,0.994521895368272,1.26097532010602E-16));
#119401=DIRECTION('',(-0.0553921607193168,-0.527021204990409,-0.848045021223109));
#119402=DIRECTION('center_axis',(-0.994521895368273,0.104528463267661,6.06488474588053E-15));
#119403=DIRECTION('ref_axis',(0.0914257765946926,0.869858159032147,0.484755722544108));
#119404=DIRECTION('',(-0.104528463267664,-0.994521895368272,1.4719374879308E-17));
#119405=DIRECTION('',(-0.0522647556052199,-0.497265932938945,0.86602250967275));
#119406=DIRECTION('center_axis',(0.994521994337725,-0.104527521619066,1.63998887836188E-6));
#119407=DIRECTION('ref_axis',(0.0905292101911294,0.86132790110626,-0.499918702268733));
#119408=DIRECTION('',(-0.104528463267664,-0.994521895368272,1.4719374879308E-17));
#119409=DIRECTION('center_axis',(0.994521796385908,-0.104529405004792,1.64014407563316E-6));
#119410=DIRECTION('ref_axis',(0.0905261737131063,0.861299008812056,0.49996902833299));
#119411=DIRECTION('',(-0.052264771972493,-0.497266088662982,-0.866022419268971));
#119412=DIRECTION('',(-0.104528463267664,-0.994521895368272,1.4719374879308E-17));
#119413=DIRECTION('center_axis',(-0.994521895368272,0.104528463267664,1.40045497140051E-16));
#119414=DIRECTION('ref_axis',(1.26097532010602E-16,-1.40045497140051E-16,
1.));
#119415=DIRECTION('center_axis',(0.994521895368272,-0.104528463267665,2.27433177943941E-15));
#119416=DIRECTION('ref_axis',(0.0914257765929865,0.869858159015916,0.484755722573557));
#119417=DIRECTION('',(0.055392160719317,0.527021204990424,0.848045021223099));
#119418=DIRECTION('',(-0.104528463267664,-0.994521895368272,-1.26097532010602E-16));
#119419=DIRECTION('',(0.055392215520313,0.527021726387063,-0.84804469361924));
#119420=DIRECTION('center_axis',(0.994521895368273,-0.104528463267659,1.52655870960609E-14));
#119421=DIRECTION('ref_axis',(0.0914259726179232,0.869860024068582,-0.484752338888914));
#119422=DIRECTION('',(0.104528463267664,0.994521895368272,-1.4719374879308E-17));
#119423=DIRECTION('',(0.0522647719724912,0.497266088663035,0.866022419268941));
#119424=DIRECTION('center_axis',(-0.994521994360727,0.104527521400209,1.64037038848631E-6));
#119425=DIRECTION('ref_axis',(0.0905292209241732,0.861328003226788,0.499918524377938));
#119426=DIRECTION('',(0.104528463267664,0.994521895368272,-1.4719374879308E-17));
#119427=DIRECTION('center_axis',(-0.994521796408004,0.104529404794571,1.63977760137252E-6));
#119428=DIRECTION('ref_axis',(0.0905261626116839,0.861298903191368,-0.499969212296267));
#119429=DIRECTION('',(0.0522647556052202,0.497265932938941,-0.866022509672752));
#119430=DIRECTION('',(0.104528463267664,0.994521895368272,-1.4719374879308E-17));
#119431=DIRECTION('center_axis',(-1.11539425682701E-16,1.37739719617121E-16,
-1.));
#119432=DIRECTION('ref_axis',(0.,1.,1.37739719617121E-16));
#119433=DIRECTION('',(0.20791169081777,0.978147600733803,1.11539425682701E-16));
#119434=DIRECTION('center_axis',(1.11539425682701E-16,-1.37739719617121E-16,
1.));
#119435=DIRECTION('ref_axis',(2.43272069155864E-12,1.,1.3773971961685E-16));
#119436=DIRECTION('',(-0.20791169081777,-0.978147600733803,-1.11539425682701E-16));
#119437=DIRECTION('center_axis',(-1.11539425682701E-16,1.37739719617121E-16,
-1.));
#119438=DIRECTION('ref_axis',(2.25178493903968E-33,1.,1.37739719617121E-16));
#119439=DIRECTION('center_axis',(-0.978147600733803,0.20791169081777,1.37739719617121E-16));
#119440=DIRECTION('ref_axis',(1.11539425682701E-16,-1.37739719617121E-16,
1.));
#119441=DIRECTION('center_axis',(-0.978147600733801,0.207911690817781,1.02000311058135E-14));
#119442=DIRECTION('ref_axis',(0.181850263143849,0.855538223403061,-0.484752338922513));
#119443=DIRECTION('',(-0.110177542335815,-0.518344583061384,0.848044693619245));
#119444=DIRECTION('',(0.20791169081777,0.978147600733803,1.11539425682701E-16));
#119445=DIRECTION('',(-0.110177433334236,-0.518344070249262,-0.848045021223112));
#119446=DIRECTION('center_axis',(-0.978147600733804,0.207911690817767,8.33921652558567E-15));
#119447=DIRECTION('ref_axis',(0.181849873248782,0.855536389091008,0.484755722545409));
#119448=DIRECTION('',(-0.20791169081777,-0.978147600733803,2.92774812072098E-17));
#119449=DIRECTION('',(-0.103956887610934,-0.489078703542056,0.866022509672739));
#119450=DIRECTION('center_axis',(0.978147797590165,-0.20791076467278,1.63998884165523E-6));
#119451=DIRECTION('ref_axis',(0.180066563577549,0.847146577519057,-0.4999187022698));
#119452=DIRECTION('',(-0.20791169081777,-0.978147600733803,2.92774812072098E-17));
#119453=DIRECTION('center_axis',(0.978147403855348,-0.207912617049456,1.64014400359551E-6));
#119454=DIRECTION('ref_axis',(0.180060523666452,0.847118160897777,0.499969028334887));
#119455=DIRECTION('',(-0.103956920166134,-0.489078856702197,-0.866022419268949));
#119456=DIRECTION('',(-0.20791169081777,-0.978147600733803,2.92774812072098E-17));
#119457=DIRECTION('center_axis',(-0.978147600733803,0.20791169081777,1.37739719617121E-16));
#119458=DIRECTION('ref_axis',(1.11539425682701E-16,-1.37739719617121E-16,
1.));
#119459=DIRECTION('center_axis',(0.9781476007338,-0.207911690817786,3.72163382090106E-14));
#119460=DIRECTION('ref_axis',(0.181849873245445,0.855536389075333,0.484755722574325));
#119461=DIRECTION('',(0.110177433334237,0.518344070249278,0.848045021223102));
#119462=DIRECTION('',(-0.20791169081777,-0.978147600733803,-1.11539425682701E-16));
#119463=DIRECTION('',(0.110177542335821,0.518344583061396,-0.848044693619237));
#119464=DIRECTION('center_axis',(0.9781476007338,-0.207911690817784,-3.30122628397866E-14));
#119465=DIRECTION('ref_axis',(0.181850263147825,0.855538223421808,-0.484752338887935));
#119466=DIRECTION('',(0.20791169081777,0.978147600733803,-2.92774812072098E-17));
#119467=DIRECTION('',(0.103956920166143,0.489078856702196,0.866022419268949));
#119468=DIRECTION('center_axis',(-0.978147797635926,0.207910764457488,1.64037041047626E-6));
#119469=DIRECTION('ref_axis',(0.180066584926733,0.847146677960321,0.499918524375339));
#119470=DIRECTION('',(0.20791169081777,0.978147600733803,-2.92774812072098E-17));
#119471=DIRECTION('center_axis',(-0.978147403899287,0.207912616842742,1.63977762800927E-6));
#119472=DIRECTION('ref_axis',(0.180060501585904,0.847118057018156,-0.499969212294534));
#119473=DIRECTION('',(0.103956887610928,0.489078703542026,-0.866022509672757));
#119474=DIRECTION('',(0.20791169081777,0.978147600733803,-2.92774812072098E-17));
#119475=DIRECTION('center_axis',(-9.73020895656121E-17,1.33924836902177E-16,
-1.));
#119476=DIRECTION('ref_axis',(0.,1.,1.33924836902177E-16));
#119477=DIRECTION('',(0.309016994374957,0.95105651629515,9.73020895656121E-17));
#119478=DIRECTION('center_axis',(9.73020895656121E-17,-1.33924836902177E-16,
1.));
#119479=DIRECTION('ref_axis',(2.04991579266789E-12,1.,1.33924836901977E-16));
#119480=DIRECTION('',(-0.309016994374957,-0.95105651629515,-9.73020895656121E-17));
#119481=DIRECTION('center_axis',(-9.73020895656121E-17,1.33924836902177E-16,
-1.));
#119482=DIRECTION('ref_axis',(1.59316208980364E-33,1.,1.33924836902177E-16));
#119483=DIRECTION('center_axis',(-0.95105651629515,0.309016994374957,1.33924836902177E-16));
#119484=DIRECTION('ref_axis',(9.73020895656121E-17,-1.33924836902177E-16,
1.));
#119485=DIRECTION('center_axis',(-0.951056516295151,0.309016994374954,-1.10270606549325E-15));
#119486=DIRECTION('ref_axis',(0.270282164133958,0.831842966947162,-0.484752338923296));
#119487=DIRECTION('',(-0.163755740941356,-0.503988348013123,0.84804469361924));
#119488=DIRECTION('',(0.309016994374957,0.95105651629515,9.73020895656121E-17));
#119489=DIRECTION('',(-0.163755578933431,-0.503987849404003,-0.84804502122311));
#119490=DIRECTION('center_axis',(-0.951056516295154,0.309016994374946,1.48865352853434E-14));
#119491=DIRECTION('ref_axis',(0.270281584636996,0.831841183438903,0.484755722545985));
#119492=DIRECTION('',(-0.309016994374957,-0.95105651629515,4.35148173242984E-17));
#119493=DIRECTION('',(-0.15451004620158,-0.475533025522863,0.866022509672732));
#119494=DIRECTION('center_axis',(0.95105680888162,-0.309016093880593,1.6399887814086E-6));
#119495=DIRECTION('ref_axis',(0.26763107001171,0.823683738751163,-0.499918702271972));
#119496=DIRECTION('',(-0.309016994374957,-0.95105651629515,4.35148173242984E-17));
#119497=DIRECTION('center_axis',(0.951056223677639,-0.30901789495325,1.64014400927579E-6));
#119498=DIRECTION('ref_axis',(0.267622092842645,0.823656109143276,0.499969028334239));
#119499=DIRECTION('',(-0.154510094588055,-0.475533174441005,-0.866022419268954));
#119500=DIRECTION('',(-0.309016994374957,-0.95105651629515,4.35148173242984E-17));
#119501=DIRECTION('center_axis',(-0.95105651629515,0.309016994374957,1.33924836902177E-16));
#119502=DIRECTION('ref_axis',(9.73020895656121E-17,-1.33924836902177E-16,
1.));
#119503=DIRECTION('center_axis',(0.951056516295148,-0.309016994374965,3.72163382090098E-15));
#119504=DIRECTION('ref_axis',(0.270281584632176,0.831841183424041,0.484755722574176));
#119505=DIRECTION('',(0.163755578933424,0.503987849404003,0.848045021223111));
#119506=DIRECTION('',(-0.309016994374957,-0.95105651629515,-9.73020895656121E-17));
#119507=DIRECTION('',(0.163755740941359,0.503988348013123,-0.84804469361924));
#119508=DIRECTION('center_axis',(0.951056516295157,-0.309016994374937,1.83324883410909E-14));
#119509=DIRECTION('ref_axis',(0.27028216414016,0.83184296696627,-0.48475233888705));
#119510=DIRECTION('',(0.309016994374957,0.95105651629515,-4.35148173242984E-17));
#119511=DIRECTION('',(0.15451009458807,0.475533174440996,0.866022419268956));
#119512=DIRECTION('center_axis',(-0.951056808949647,0.309016093671226,1.64037042347201E-6));
#119513=DIRECTION('ref_axis',(0.267631101743148,0.823683836411319,0.499918524376203));
#119514=DIRECTION('',(0.309016994374957,0.95105651629515,-4.35148173242984E-17));
#119515=DIRECTION('center_axis',(-0.951056223742963,0.309017894752208,1.63977752868973E-6));
#119516=DIRECTION('ref_axis',(0.26762206002332,0.82365600813657,-0.499969212301523));
#119517=DIRECTION('',(0.154510046201593,0.475533025522812,-0.866022509672758));
#119518=DIRECTION('',(0.309016994374957,0.95105651629515,-4.35148173242984E-17));
#119519=DIRECTION('center_axis',(-8.35415108931894E-17,1.28642645648558E-16,
-1.));
#119520=DIRECTION('ref_axis',(0.,1.,1.28642645648558E-16));
#119521=DIRECTION('',(0.40673664307581,0.913545457642596,8.35415108931894E-17));
#119522=DIRECTION('center_axis',(8.35415108931894E-17,-1.28642645648558E-16,
1.));
#119523=DIRECTION('ref_axis',(2.68585154117318E-12,1.,1.28642645648334E-16));
#119524=DIRECTION('',(-0.40673664307581,-0.913545457642596,-8.35415108931894E-17));
#119525=DIRECTION('center_axis',(-8.35415108931894E-17,1.28642645648558E-16,
-1.));
#119526=DIRECTION('ref_axis',(9.26572950507599E-34,1.,1.28642645648558E-16));
#119527=DIRECTION('center_axis',(-0.913545457642596,0.40673664307581,1.28642645648558E-16));
#119528=DIRECTION('ref_axis',(8.35415108931894E-17,-1.28642645648558E-16,
1.));
#119529=DIRECTION('center_axis',(-0.913545457642591,0.406736643075822,2.2329797826238E-14));
#119530=DIRECTION('ref_axis',(0.355752797174115,0.799033864872324,-0.484752338921629));
#119531=DIRECTION('',(-0.215539797381059,-0.484110311157677,0.848044693619239));
#119532=DIRECTION('',(0.40673664307581,0.913545457642596,8.35415108931894E-17));
#119533=DIRECTION('',(-0.215539584141775,-0.484109832214432,-0.84804502122311));
#119534=DIRECTION('center_axis',(-0.913545457642595,0.406736643075814,-9.64868027753666E-16));
#119535=DIRECTION('ref_axis',(0.355752034424621,0.799032151708906,0.484755722542993));
#119536=DIRECTION('',(-0.40673664307581,-0.913545457642596,5.72753959967212E-17));
#119537=DIRECTION('',(-0.20337036039277,-0.456777308164325,0.866022509672739));
#119538=DIRECTION('center_axis',(0.913545842753538,-0.406735778098066,1.6399887859702E-6));
#119539=DIRECTION('ref_axis',(0.352263354438556,0.79119644857774,-0.499918702268347));
#119540=DIRECTION('',(-0.40673664307581,-0.913545457642596,5.72753959967212E-17));
#119541=DIRECTION('center_axis',(0.913545072491979,-0.406737508133851,1.64014419087578E-6));
#119542=DIRECTION('ref_axis',(0.352251538365721,0.791169908694829,0.499969028335555));
#119543=DIRECTION('',(-0.203370424080349,-0.456777451208949,-0.866022419268945));
#119544=DIRECTION('',(-0.40673664307581,-0.913545457642596,5.72753959967212E-17));
#119545=DIRECTION('center_axis',(-0.913545457642596,0.40673664307581,1.28642645648558E-16));
#119546=DIRECTION('ref_axis',(8.35415108931894E-17,-1.28642645648558E-16,
1.));
#119547=DIRECTION('center_axis',(0.913545457642598,-0.406736643075806,-1.40595055456267E-14));
#119548=DIRECTION('ref_axis',(0.355752034417943,0.799032151693909,0.484755722572614));
#119549=DIRECTION('',(0.215539584141768,0.484109832214442,0.848045021223106));
#119550=DIRECTION('',(-0.40673664307581,-0.913545457642596,-8.35415108931894E-17));
#119551=DIRECTION('',(0.215539797381042,0.484110311157656,-0.848044693619255));
#119552=DIRECTION('center_axis',(0.9135454576426,-0.406736643075802,2.04000622141478E-14));
#119553=DIRECTION('ref_axis',(0.355752797181682,0.799033864889318,-0.484752338888064));
#119554=DIRECTION('',(0.40673664307581,0.913545457642596,-5.72753959967212E-17));
#119555=DIRECTION('',(0.20337042408034,0.456777451208963,0.866022419268939));
#119556=DIRECTION('center_axis',(-0.91354584284308,0.406735777896949,1.64037046486978E-6));
#119557=DIRECTION('ref_axis',(0.352263396203314,0.791196542383525,0.499918524377384));
#119558=DIRECTION('',(0.40673664307581,0.913545457642596,-5.72753959967212E-17));
#119559=DIRECTION('center_axis',(-0.913545072577964,0.406737507940728,1.6397775875592E-6));
#119560=DIRECTION('ref_axis',(0.352251495168338,0.791169811672393,-0.499969212302058));
#119561=DIRECTION('',(0.203370360392774,0.456777308164295,-0.866022509672753));
#119562=DIRECTION('',(0.40673664307581,0.913545457642596,-5.72753959967212E-17));
#119563=DIRECTION('center_axis',(-7.04084534449538E-17,1.2195101864901E-16,
-1.));
#119564=DIRECTION('ref_axis',(0.,1.,1.2195101864901E-16));
#119565=DIRECTION('',(0.50000000000001,0.866025403784433,7.04084534449538E-17));
#119566=DIRECTION('center_axis',(7.04084534449538E-17,-1.2195101864901E-16,
1.));
#119567=DIRECTION('ref_axis',(2.63700172808967E-12,1.,1.21951018648824E-16));
#119568=DIRECTION('',(-0.50000000000001,-0.866025403784433,-7.04084534449538E-17));
#119569=DIRECTION('center_axis',(-7.04084534449538E-17,1.2195101864901E-16,
-1.));
#119570=DIRECTION('ref_axis',(3.09764893063008E-34,1.,1.2195101864901E-16));
#119571=DIRECTION('center_axis',(-0.866025403784433,0.50000000000001,1.2195101864901E-16));
#119572=DIRECTION('ref_axis',(7.04084534449538E-17,-1.2195101864901E-16,
1.));
#119573=DIRECTION('center_axis',(-0.866025403784415,0.500000000000041,4.54866252015975E-14));
#119574=DIRECTION('ref_axis',(0.437325728121414,0.757470380563304,-0.484752338924073));
#119575=DIRECTION('',(-0.264962354696027,-0.458928260426592,0.848044693619245));
#119576=DIRECTION('',(0.50000000000001,0.866025403784433,7.04084534449538E-17));
#119577=DIRECTION('',(-0.264962092561705,-0.458927806396623,-0.848045021223111));
#119578=DIRECTION('center_axis',(-0.866025403784399,0.500000000000068,-9.57976113269888E-14));
#119579=DIRECTION('ref_axis',(0.437324790477049,0.757468756515617,0.484755722541663));
#119580=DIRECTION('',(-0.50000000000001,-0.866025403784433,7.04084534449566E-17));
#119581=DIRECTION('',(-0.250002506357495,-0.433017043030775,0.866022509672731));
#119582=DIRECTION('center_axis',(0.866025877200486,-0.499999180015767,1.63998881574967E-6));
#119583=DIRECTION('ref_axis',(0.433036167836511,0.750040644541146,-0.499918702272451));
#119584=DIRECTION('',(-0.50000000000001,-0.866025403784433,7.04084534449566E-17));
#119585=DIRECTION('center_axis',(0.866024930320552,-0.50000082005992,1.6401440734818E-6));
#119586=DIRECTION('ref_axis',(0.433021642322727,0.750015485166862,0.499969028330801));
#119587=DIRECTION('',(-0.250002584648428,-0.433017178634614,-0.866022419268938));
#119588=DIRECTION('',(-0.50000000000001,-0.866025403784433,7.04084534449566E-17));
#119589=DIRECTION('center_axis',(-0.866025403784433,0.50000000000001,1.2195101864901E-16));
#119590=DIRECTION('ref_axis',(7.04084534449538E-17,-1.2195101864901E-16,
1.));
#119591=DIRECTION('center_axis',(0.866025403784456,-0.49999999999997,-7.02975277281265E-14));
#119592=DIRECTION('ref_axis',(0.437324790468275,0.757468756500457,0.484755722573268));
#119593=DIRECTION('',(0.264962092561697,0.458927806396632,0.848045021223108));
#119594=DIRECTION('',(-0.50000000000001,-0.866025403784433,-7.04084534449538E-17));
#119595=DIRECTION('',(0.264962354696035,0.458928260426609,-0.848044693619234));
#119596=DIRECTION('center_axis',(0.866025403784424,-0.500000000000025,-2.88081959645749E-14));
#119597=DIRECTION('ref_axis',(0.43732572813103,0.757470380579976,-0.484752338889345));
#119598=DIRECTION('',(0.50000000000001,0.866025403784433,-7.04084534449566E-17));
#119599=DIRECTION('',(0.250002584648412,0.433017178634587,0.866022419268956));
#119600=DIRECTION('center_axis',(-0.866025877310554,0.499999179825123,1.64037042562383E-6));
#119601=DIRECTION('ref_axis',(0.433036219179545,0.75004073347043,0.499918524375547));
#119602=DIRECTION('',(0.50000000000001,0.866025403784433,-7.04084534449566E-17));
#119603=DIRECTION('center_axis',(-0.86602493042628,0.500000819876797,1.63977742833608E-6));
#119604=DIRECTION('ref_axis',(0.433021589220767,0.750015393192006,-0.499969212295879));
#119605=DIRECTION('',(0.250002506357492,0.43301704303074,-0.866022509672749));
#119606=DIRECTION('',(0.50000000000001,0.866025403784433,-7.04084534449566E-17));
#119607=DIRECTION('center_axis',(-5.80468057465775E-17,1.13923270769251E-16,
-1.));
#119608=DIRECTION('ref_axis',(0.,1.,1.13923270769251E-16));
#119609=DIRECTION('',(0.587785252292482,0.809016994374941,5.80468057465775E-17));
#119610=DIRECTION('center_axis',(5.80468057465775E-17,-1.13923270769251E-16,
1.));
#119611=DIRECTION('ref_axis',(2.03917556295366E-34,1.,1.13923270769251E-16));
#119612=DIRECTION('',(-0.587785252292482,-0.809016994374941,-5.80468057465775E-17));
#119613=DIRECTION('center_axis',(-5.80468057465775E-17,1.13923270769251E-16,
-1.));
#119614=DIRECTION('ref_axis',(-2.10605807273598E-34,1.,1.13923270769251E-16));
#119615=DIRECTION('center_axis',(-0.809016994374941,0.587785252292482,1.13923270769251E-16));
#119616=DIRECTION('ref_axis',(5.80468057465775E-17,-1.13923270769251E-16,
1.));
#119617=DIRECTION('center_axis',(-0.809016994374934,0.587785252292492,1.68162674987722E-14));
#119618=DIRECTION('ref_axis',(0.514107226875554,0.707607892255063,-0.484752338924398));
#119619=DIRECTION('',(-0.311481929006024,-0.428718095637375,0.848044693619239));
#119620=DIRECTION('',(0.587785252292482,0.809016994374941,5.80468057465775E-17));
#119621=DIRECTION('',(-0.31148162084864,-0.428717671495099,-0.848045021223122));
#119622=DIRECTION('center_axis',(-0.809016994374973,0.587785252292438,7.37434849783257E-14));
#119623=DIRECTION('ref_axis',(0.514106124608232,0.707606375114275,0.484755722542748));
#119624=DIRECTION('',(-0.587785252292482,-0.809016994374941,8.2770101143333E-17));
#119625=DIRECTION('',(-0.293895572546169,-0.404512552559093,0.866022509672749));
#119626=DIRECTION('center_axis',(0.809017550909317,-0.587784486285578,1.63998898495591E-6));
#119627=DIRECTION('ref_axis',(0.509064546362255,0.700667238249452,-0.499918702271557));
#119628=DIRECTION('',(-0.587785252292482,-0.809016994374941,8.2770101143333E-17));
#119629=DIRECTION('center_axis',(0.809016437785117,-0.587786018369602,1.64014408828489E-6));
#119630=DIRECTION('ref_axis',(0.509047470548778,0.700643735028728,0.49996902833364));
#119631=DIRECTION('',(-0.293895664582707,-0.404512679236446,-0.866022419268948));
#119632=DIRECTION('',(-0.587785252292482,-0.809016994374941,8.2770101143333E-17));
#119633=DIRECTION('center_axis',(-0.809016994374941,0.587785252292482,1.13923270769251E-16));
#119634=DIRECTION('ref_axis',(5.80468057465775E-17,-1.13923270769251E-16,
1.));
#119635=DIRECTION('center_axis',(0.809016994374913,-0.58778525229252,1.10546308309721E-13));
#119636=DIRECTION('ref_axis',(0.514106124598513,0.707606375100899,0.48475572257258));
#119637=DIRECTION('',(0.311481620848643,0.42871767149512,0.84804502122311));
#119638=DIRECTION('',(-0.587785252292482,-0.809016994374941,-5.80468057465775E-17));
#119639=DIRECTION('',(0.31148192900604,0.428718095637378,-0.848044693619232));
#119640=DIRECTION('center_axis',(0.809016994374959,-0.587785252292457,6.781642303623E-14));
#119641=DIRECTION('ref_axis',(0.514107226887019,0.707607892270838,-0.484752338889211));
#119642=DIRECTION('',(0.587785252292482,0.809016994374941,-8.2770101143333E-17));
#119643=DIRECTION('',(0.293895664582671,0.404512679236479,0.866022419268945));
#119644=DIRECTION('center_axis',(-0.809017551038645,0.587784486107572,1.64037042958252E-6));
#119645=DIRECTION('ref_axis',(0.509064606719795,0.700667321324917,0.499918524374308));
#119646=DIRECTION('',(0.587785252292482,0.809016994374941,-8.2770101143333E-17));
#119647=DIRECTION('center_axis',(-0.809016437909404,0.587786018198536,1.63977756741941E-6));
#119648=DIRECTION('ref_axis',(0.509047408125916,0.700643649111502,-0.499969212292123));
#119649=DIRECTION('',(0.293895572546207,0.404512552559083,-0.866022509672741));
#119650=DIRECTION('',(0.587785252292482,0.809016994374941,-8.2770101143333E-17));
#119651=DIRECTION('center_axis',(-4.65920045970846E-17,1.04647355694968E-16,
-1.));
#119652=DIRECTION('ref_axis',(0.,1.,1.04647355694968E-16));
#119653=DIRECTION('',(0.669130606358867,0.743144825477386,4.65920045970846E-17));
#119654=DIRECTION('center_axis',(4.65920045970846E-17,-1.04647355694968E-16,
1.));
#119655=DIRECTION('ref_axis',(-5.08215691752411E-12,1.,1.04647355695205E-16));
#119656=DIRECTION('',(-0.669130606358867,-0.743144825477386,-4.65920045970846E-17));
#119657=DIRECTION('center_axis',(-4.65920045970846E-17,1.04647355694968E-16,
-1.));
#119658=DIRECTION('ref_axis',(-6.01228899222973E-34,1.,1.04647355694968E-16));
#119659=DIRECTION('center_axis',(-0.743144825477386,0.669130606358867,1.04647355694968E-16));
#119660=DIRECTION('ref_axis',(4.65920045970846E-17,-1.04647355694968E-16,
1.));
#119661=DIRECTION('center_axis',(-0.743144825477412,0.669130606358838,-6.09245101184987E-14));
#119662=DIRECTION('ref_axis',(0.585256059268807,0.649992703803544,-0.484752338922985));
#119663=DIRECTION('',(-0.354588842120043,-0.393810805677315,0.84804469361924));
#119664=DIRECTION('',(0.669130606358867,0.743144825477386,4.65920045970846E-17));
#119665=DIRECTION('',(-0.354588491315847,-0.393810416069776,-0.848045021223108));
#119666=DIRECTION('center_axis',(-0.743144825477402,0.66913060635885,4.3281222959236E-14));
#119667=DIRECTION('ref_axis',(0.585254804454853,0.649991310191455,0.484755722542919));
#119668=DIRECTION('',(-0.669130606358867,-0.743144825477386,9.42249022928259E-17));
#119669=DIRECTION('',(-0.334568657340454,-0.371576137911918,0.866022509672739));
#119670=DIRECTION('center_axis',(0.743145459032515,-0.669129902721933,1.6399889188559E-6));
#119671=DIRECTION('ref_axis',(0.579515507189717,0.643617175071609,-0.499918702270166));
#119672=DIRECTION('',(-0.669130606358867,-0.743144825477386,9.42249022928259E-17));
#119673=DIRECTION('center_axis',(0.743144191859766,-0.669131310059846,1.6401440772679E-6));
#119674=DIRECTION('ref_axis',(0.579496068163272,0.643595585511955,0.499969028333588));
#119675=DIRECTION('',(-0.334568762114156,-0.371576254274936,-0.86602241926893));
#119676=DIRECTION('',(-0.669130606358867,-0.743144825477386,9.42249022928259E-17));
#119677=DIRECTION('center_axis',(-0.743144825477386,0.669130606358867,1.04647355694968E-16));
#119678=DIRECTION('ref_axis',(4.65920045970846E-17,-1.04647355694968E-16,
1.));
#119679=DIRECTION('center_axis',(0.743144825477406,-0.669130606358846,-1.31222051759166E-13));
#119680=DIRECTION('ref_axis',(0.585254804443108,0.649991310178355,0.484755722574664));
#119681=DIRECTION('',(0.354588491315847,0.39381041606979,0.848045021223102));
#119682=DIRECTION('',(-0.669130606358867,-0.743144825477386,-4.65920045970846E-17));
#119683=DIRECTION('',(0.354588842120062,0.393810805677307,-0.848044693619236));
#119684=DIRECTION('center_axis',(0.743144825477372,-0.669130606358882,-7.33299533643765E-14));
#119685=DIRECTION('ref_axis',(0.585256059281577,0.649992703817746,-0.484752338888524));
#119686=DIRECTION('',(0.669130606358867,0.743144825477386,-9.42249022928259E-17));
#119687=DIRECTION('',(0.334568762114183,0.371576254274923,0.866022419268924));
#119688=DIRECTION('center_axis',(-0.743145459179742,0.66912990255842,1.64037033353259E-6));
#119689=DIRECTION('ref_axis',(0.579515575898918,0.643617251381315,0.499918524376628));
#119690=DIRECTION('',(0.669130606358867,0.743144825477386,-9.42249022928259E-17));
#119691=DIRECTION('center_axis',(-0.7431441920012,0.669131309902768,1.63977763833729E-6));
#119692=DIRECTION('ref_axis',(0.579495997100135,0.643595506588717,-0.499969212295851));
#119693=DIRECTION('',(0.33456865734047,0.371576137911861,-0.866022509672757));
#119694=DIRECTION('',(0.669130606358867,0.743144825477386,-9.42249022928259E-17));
#119695=DIRECTION('center_axis',(-3.61695511949404E-17,9.42249022928235E-17,
-1.));
#119696=DIRECTION('ref_axis',(0.,1.,9.42249022928235E-17));
#119697=DIRECTION('',(0.743144825477402,0.66913060635885,3.61695511949404E-17));
#119698=DIRECTION('center_axis',(3.61695511949404E-17,-9.42249022928235E-17,
1.));
#119699=DIRECTION('ref_axis',(1.24700250125898E-12,1.,9.42249022927784E-17));
#119700=DIRECTION('',(-0.743144825477402,-0.66913060635885,-3.61695511949404E-17));
#119701=DIRECTION('center_axis',(-3.61695511949404E-17,9.42249022928235E-17,
-1.));
#119702=DIRECTION('ref_axis',(-8.43711753644599E-34,1.,9.42249022928235E-17));
#119703=DIRECTION('center_axis',(-0.66913060635885,0.743144825477402,9.42249022928235E-17));
#119704=DIRECTION('ref_axis',(3.61695511949404E-17,-9.42249022928235E-17,
1.));
#119705=DIRECTION('center_axis',(-0.669130606358838,0.743144825477412,6.09245101184987E-14));
#119706=DIRECTION('ref_axis',(0.649992703804063,0.585256059269274,-0.484752338921726));
#119707=DIRECTION('',(-0.393810805677328,-0.35458884212003,0.84804469361924));
#119708=DIRECTION('',(0.743144825477402,0.66913060635885,3.61695511949404E-17));
#119709=DIRECTION('',(-0.393810416069783,-0.354588491315852,-0.848045021223102));
#119710=DIRECTION('center_axis',(-0.669130606358808,0.74314482547744,-6.53353493078877E-14));
#119711=DIRECTION('ref_axis',(0.649991310191615,0.585254804454945,0.484755722542594));
#119712=DIRECTION('',(-0.743144825477402,-0.66913060635885,1.0464735569497E-16));
#119713=DIRECTION('',(-0.371576137911934,-0.334568657340433,0.86602250967274));
#119714=DIRECTION('center_axis',(0.669131309993433,-0.743144191919564,1.63998895207813E-6));
#119715=DIRECTION('ref_axis',(0.643617174847078,0.579515507436224,-0.499918702273481));
#119716=DIRECTION('',(-0.743144825477402,-0.66913060635885,1.0464735569497E-16));
#119717=DIRECTION('center_axis',(0.669129902655543,-0.743145459092292,1.64014393853014E-6));
#119718=DIRECTION('ref_axis',(0.643595585587858,0.579496068079491,0.499969028332989));
#119719=DIRECTION('',(-0.371576254274944,-0.334568762114131,-0.866022419268936));
#119720=DIRECTION('',(-0.743144825477402,-0.66913060635885,1.0464735569497E-16));
#119721=DIRECTION('center_axis',(-0.66913060635885,0.743144825477402,9.42249022928235E-17));
#119722=DIRECTION('ref_axis',(3.61695511949404E-17,-9.42249022928235E-17,
1.));
#119723=DIRECTION('center_axis',(0.669130606358856,-0.743144825477396,-2.31568326633862E-14));
#119724=DIRECTION('ref_axis',(0.649991310178348,0.585254804443017,0.484755722574783));
#119725=DIRECTION('',(0.393810416069767,0.354588491315837,0.848045021223116));
#119726=DIRECTION('',(-0.743144825477402,-0.66913060635885,-3.61695511949404E-17));
#119727=DIRECTION('',(0.393810805677295,0.354588842120035,-0.848044693619253));
#119728=DIRECTION('center_axis',(0.669130606358837,-0.743144825477414,2.34325038946298E-14));
#119729=DIRECTION('ref_axis',(0.649992703818525,0.585256059282238,-0.484752338886682));
#119730=DIRECTION('',(0.743144825477402,0.66913060635885,-1.0464735569497E-16));
#119731=DIRECTION('',(0.371576254274883,0.33456876211414,0.866022419268959));
#119732=DIRECTION('center_axis',(-0.66913131015695,0.743144191772332,1.64037043491853E-6));
#119733=DIRECTION('ref_axis',(0.643617251158306,0.579515576147492,0.499918524375589));
#119734=DIRECTION('',(0.743144825477402,0.66913060635885,-1.0464735569497E-16));
#119735=DIRECTION('center_axis',(-0.669129902812644,0.743145458950839,1.6397773398599E-6));
#119736=DIRECTION('ref_axis',(0.643595506659834,0.579495997012642,-0.499969212305713));
#119737=DIRECTION('',(0.371576137911907,0.334568657340444,-0.866022509672747));
#119738=DIRECTION('',(0.743144825477402,0.66913060635885,-1.0464735569497E-16));
#119739=DIRECTION('center_axis',(-2.68936361206573E-17,8.27701011433304E-17,
-1.));
#119740=DIRECTION('ref_axis',(0.,1.,8.27701011433304E-17));
#119741=DIRECTION('',(0.809016994374955,0.587785252292463,2.68936361206573E-17));
#119742=DIRECTION('center_axis',(2.68936361206573E-17,-8.27701011433304E-17,
1.));
#119743=DIRECTION('ref_axis',(-7.43345068374092E-34,1.,8.27701011433304E-17));
#119744=DIRECTION('',(-0.809016994374955,-0.587785252292463,-2.68936361206573E-17));
#119745=DIRECTION('center_axis',(-2.68936361206573E-17,8.27701011433304E-17,
-1.));
#119746=DIRECTION('ref_axis',(-9.35397677642637E-34,1.,8.27701011433303E-17));
#119747=DIRECTION('center_axis',(-0.587785252292463,0.809016994374955,8.27701011433303E-17));
#119748=DIRECTION('ref_axis',(2.68936361206573E-17,-8.27701011433304E-17,
1.));
#119749=DIRECTION('center_axis',(-0.587785252292444,0.809016994374969,1.57135614332808E-14));
#119750=DIRECTION('ref_axis',(0.707607892255383,0.514107226875742,-0.484752338923732));
#119751=DIRECTION('',(-0.428718095637369,-0.31148192900601,0.848044693619247));
#119752=DIRECTION('',(0.809016994374955,0.587785252292463,2.68936361206573E-17));
#119753=DIRECTION('',(-0.428717671495124,-0.311481620848633,-0.848045021223112));
#119754=DIRECTION('center_axis',(-0.587785252292501,0.809016994374927,9.01462414501431E-14));
#119755=DIRECTION('ref_axis',(0.707606375113487,0.514106124607646,0.484755722544519));
#119756=DIRECTION('',(-0.809016994374955,-0.587785252292463,1.13923270769253E-16));
#119757=DIRECTION('',(-0.404512552559104,-0.293895572546205,0.866022509672732));
#119758=DIRECTION('center_axis',(0.587786018297244,-0.809016437837688,1.63998890629073E-6));
#119759=DIRECTION('ref_axis',(0.700667238054952,0.509064546633043,-0.499918702268419));
#119760=DIRECTION('',(-0.809016994374955,-0.587785252292463,1.13923270769253E-16));
#119761=DIRECTION('center_axis',(0.58778448621328,-0.809017550961845,1.64014403044851E-6));
#119762=DIRECTION('ref_axis',(0.700643735097504,0.509047470458993,0.499969028328675));
#119763=DIRECTION('',(-0.40451267923645,-0.293895664582675,-0.866022419268957));
#119764=DIRECTION('',(-0.809016994374955,-0.587785252292463,1.13923270769253E-16));
#119765=DIRECTION('center_axis',(-0.587785252292463,0.809016994374955,8.27701011433303E-17));
#119766=DIRECTION('ref_axis',(2.68936361206573E-17,-8.27701011433304E-17,
1.));
#119767=DIRECTION('center_axis',(0.587785252292418,-0.809016994374988,4.46596058508136E-14));
#119768=DIRECTION('ref_axis',(0.707606375100562,0.514106124598224,0.484755722573379));
#119769=DIRECTION('',(0.428717671495113,0.311481620848634,0.848045021223117));
#119770=DIRECTION('',(-0.809016994374955,-0.587785252292463,-2.68936361206573E-17));
#119771=DIRECTION('',(0.428718095637379,0.311481929006014,-0.84804469361924));
#119772=DIRECTION('center_axis',(0.587785252292438,-0.809016994374973,-5.15515085681819E-14));
#119773=DIRECTION('ref_axis',(0.707607892271254,0.514107226887285,-0.484752338888322));
#119774=DIRECTION('',(0.809016994374955,0.587785252292463,-1.13923270769253E-16));
#119775=DIRECTION('',(0.404512679236446,0.293895664582707,0.866022419268948));
#119776=DIRECTION('center_axis',(-0.587786018475273,0.809016437708342,1.64037041133668E-6));
#119777=DIRECTION('ref_axis',(0.700667321128982,0.509064606990169,0.499918524373603));
#119778=DIRECTION('',(0.809016994374955,0.587785252292463,-1.13923270769253E-16));
#119779=DIRECTION('center_axis',(-0.587784486384226,0.809017550837646,1.63977767104282E-6));
#119780=DIRECTION('ref_axis',(0.700643649177376,0.50904740803465,-0.499969212292732));
#119781=DIRECTION('',(0.404512552559085,0.293895572546138,-0.866022509672763));
#119782=DIRECTION('',(0.809016994374955,0.587785252292463,-1.13923270769253E-16));
#119783=DIRECTION('center_axis',(-1.88658882408992E-17,7.04084534449537E-17,
-1.));
#119784=DIRECTION('ref_axis',(0.,1.,7.04084534449537E-17));
#119785=DIRECTION('',(0.866025403784445,0.499999999999989,1.88658882408992E-17));
#119786=DIRECTION('center_axis',(1.88658882408992E-17,-7.04084534449537E-17,
1.));
#119787=DIRECTION('ref_axis',(2.39808173319034E-12,1.,7.04084534449084E-17));
#119788=DIRECTION('',(-0.866025403784445,-0.499999999999989,-1.88658882408992E-17));
#119789=DIRECTION('center_axis',(-1.88658882408992E-17,7.04084534449537E-17,
-1.));
#119790=DIRECTION('ref_axis',(-8.89395021849233E-34,1.,7.04084534449537E-17));
#119791=DIRECTION('center_axis',(-0.499999999999989,0.866025403784445,7.04084534449537E-17));
#119792=DIRECTION('ref_axis',(1.88658882408992E-17,-7.04084534449537E-17,
1.));
#119793=DIRECTION('center_axis',(-0.500000000000001,0.866025403784438,3.58379471285317E-15));
#119794=DIRECTION('ref_axis',(0.757470380565452,0.437325728122635,-0.484752338919614));
#119795=DIRECTION('',(-0.458928260426618,-0.264962354696007,0.848044693619237));
#119796=DIRECTION('',(0.866025403784445,0.499999999999989,1.88658882408991E-17));
#119797=DIRECTION('',(-0.458927806396625,-0.264962092561694,-0.848045021223113));
#119798=DIRECTION('center_axis',(-0.49999999999998,0.86602540378445,-3.36325426817012E-14));
#119799=DIRECTION('ref_axis',(0.757468756515611,0.437324790477015,0.484755722541703));
#119800=DIRECTION('',(-0.866025403784445,-0.499999999999989,1.21951018649011E-16));
#119801=DIRECTION('',(-0.433017043030788,-0.2500025063575,0.866022509672722));
#119802=DIRECTION('center_axis',(0.50000081998251,-0.866024930365246,1.63998892746333E-6));
#119803=DIRECTION('ref_axis',(0.750040644373928,0.433036168124944,-0.499918702273488));
#119804=DIRECTION('',(-0.866025403784445,-0.499999999999989,1.21951018649011E-16));
#119805=DIRECTION('center_axis',(0.499999179938316,-0.866025877245202,1.64014398672678E-6));
#119806=DIRECTION('ref_axis',(0.750015485223452,0.43302164222488,0.499969028330653));
#119807=DIRECTION('',(-0.433017178634633,-0.250002584648383,-0.866022419268941));
#119808=DIRECTION('',(-0.866025403784445,-0.499999999999989,1.21951018649011E-16));
#119809=DIRECTION('center_axis',(-0.499999999999989,0.866025403784445,7.04084534449537E-17));
#119810=DIRECTION('ref_axis',(1.88658882408992E-17,-7.04084534449537E-17,
1.));
#119811=DIRECTION('center_axis',(0.499999999999953,-0.866025403784466,8.87678585429635E-14));
#119812=DIRECTION('ref_axis',(0.757468756498903,0.437324790467367,0.484755722576515));
#119813=DIRECTION('',(0.458927806396636,0.264962092561686,0.848045021223109));
#119814=DIRECTION('',(-0.866025403784445,-0.499999999999989,-1.88658882408991E-17));
#119815=DIRECTION('',(0.458928260426592,0.264962354696007,-0.848044693619251));
#119816=DIRECTION('center_axis',(0.499999999999964,-0.866025403784459,-4.21785070103366E-14));
#119817=DIRECTION('ref_axis',(0.757470380579776,0.437325728130884,-0.48475233888979));
#119818=DIRECTION('',(0.866025403784445,0.499999999999989,-1.21951018649011E-16));
#119819=DIRECTION('',(0.433017178634602,0.250002584648404,0.866022419268951));
#119820=DIRECTION('center_axis',(-0.500000820173088,0.866024930255214,1.64037045316471E-6));
#119821=DIRECTION('ref_axis',(0.750040733303908,0.433036219468976,0.499918524374674));
#119822=DIRECTION('',(0.866025403784445,0.499999999999989,-1.21951018649011E-16));
#119823=DIRECTION('center_axis',(-0.499999180121355,0.866025877139526,1.63977753161604E-6));
#119824=DIRECTION('ref_axis',(0.750015393246846,0.433021589122425,-0.499969212298786));
#119825=DIRECTION('',(0.43301704303074,0.250002506357492,-0.866022509672749));
#119826=DIRECTION('',(0.866025403784445,0.499999999999989,-1.21951018649011E-16));
#119827=DIRECTION('center_axis',(-1.2174261241351E-17,5.72753959967181E-17,
-1.));
#119828=DIRECTION('ref_axis',(0.,1.,5.72753959967181E-17));
#119829=DIRECTION('',(0.913545457642606,0.406736643075789,1.2174261241351E-17));
#119830=DIRECTION('center_axis',(1.2174261241351E-17,-5.72753959967181E-17,
1.));
#119831=DIRECTION('ref_axis',(-7.04858393874019E-12,1.,5.72753959968039E-17));
#119832=DIRECTION('',(-0.913545457642606,-0.406736643075789,-1.2174261241351E-17));
#119833=DIRECTION('center_axis',(-1.2174261241351E-17,5.72753959967181E-17,
-1.));
#119834=DIRECTION('ref_axis',(6.97285633565874E-34,1.,5.72753959967181E-17));
#119835=DIRECTION('center_axis',(-0.406736643075789,0.913545457642606,5.72753959967181E-17));
#119836=DIRECTION('ref_axis',(1.2174261241351E-17,-5.72753959967181E-17,
1.));
#119837=DIRECTION('center_axis',(-0.406736643075804,0.913545457642599,-8.27029549119977E-16));
#119838=DIRECTION('ref_axis',(0.79903386487198,0.355752797173954,-0.484752338922314));
#119839=DIRECTION('',(-0.484110311157678,-0.215539797381027,0.848044693619247));
#119840=DIRECTION('',(0.913545457642606,0.406736643075789,1.2174261241351E-17));
#119841=DIRECTION('',(-0.484109832214435,-0.215539584141758,-0.848045021223113));
#119842=DIRECTION('center_axis',(-0.406736643075777,0.913545457642611,-2.15027731899433E-14));
#119843=DIRECTION('ref_axis',(0.799032151708161,0.355752034424262,0.484755722544485));
#119844=DIRECTION('',(-0.913545457642606,-0.406736643075789,1.2864264564856E-16));
#119845=DIRECTION('',(-0.456777308164333,-0.203370360392756,0.866022509672737));
#119846=DIRECTION('center_axis',(0.40673750805212,-0.913545072528368,1.63998882745409E-6));
#119847=DIRECTION('ref_axis',(0.791196448443063,0.352263354743605,-0.499918702266544));
#119848=DIRECTION('',(-0.913545457642606,-0.406736643075789,1.2864264564856E-16));
#119849=DIRECTION('center_axis',(0.40673577801635,-0.913545842789919,1.64014404421889E-6));
#119850=DIRECTION('ref_axis',(0.7911699087431,0.352251538263499,0.49996902833119));
#119851=DIRECTION('',(-0.456777451208922,-0.203370424080335,-0.866022419268962));
#119852=DIRECTION('',(-0.913545457642606,-0.406736643075789,1.2864264564856E-16));
#119853=DIRECTION('center_axis',(-0.406736643075789,0.913545457642606,5.72753959967181E-17));
#119854=DIRECTION('ref_axis',(1.2174261241351E-17,-5.72753959967181E-17,
1.));
#119855=DIRECTION('center_axis',(0.406736643075782,-0.913545457642609,-4.4108252692162E-15));
#119856=DIRECTION('ref_axis',(0.799032151693547,0.355752034417747,0.484755722573354));
#119857=DIRECTION('',(0.48410983221443,0.215539584141761,0.848045021223115));
#119858=DIRECTION('',(-0.913545457642606,-0.406736643075789,-1.2174261241351E-17));
#119859=DIRECTION('',(0.484110311157677,0.215539797381033,-0.848044693619246));
#119860=DIRECTION('center_axis',(0.406736643075817,-0.913545457642593,4.39704043669829E-14));
#119861=DIRECTION('ref_axis',(0.799033864889481,0.355752797181736,-0.484752338887755));
#119862=DIRECTION('',(0.913545457642606,0.406736643075789,-1.2864264564856E-16));
#119863=DIRECTION('',(0.45677745120894,0.203370424080363,0.866022419268946));
#119864=DIRECTION('center_axis',(-0.406737508253128,0.913545072438873,1.64037036124584E-6));
#119865=DIRECTION('ref_axis',(0.791196542247866,0.35226339650843,0.499918524377089));
#119866=DIRECTION('',(0.913545457642606,0.406736643075789,-1.2864264564856E-16));
#119867=DIRECTION('center_axis',(-0.406735778209486,0.913545842703931,1.63977751199266E-6));
#119868=DIRECTION('ref_axis',(0.79116981172108,0.352251495066775,-0.499969212296569));
#119869=DIRECTION('',(0.456777308164311,0.203370360392764,-0.866022509672747));
#119870=DIRECTION('',(0.913545457642606,0.406736643075789,-1.2864264564856E-16));
#119871=DIRECTION('center_axis',(-6.89206998773264E-18,4.35148173242952E-17,
-1.));
#119872=DIRECTION('ref_axis',(0.,1.,4.35148173242952E-17));
#119873=DIRECTION('',(0.951056516295158,0.309016994374935,6.89206998773264E-18));
#119874=DIRECTION('center_axis',(6.89206998773264E-18,-4.35148173242952E-17,
1.));
#119875=DIRECTION('ref_axis',(-6.90292267790937E-12,1.,4.35148173243428E-17));
#119876=DIRECTION('',(-0.951056516295158,-0.309016994374935,-6.89206998773264E-18));
#119877=DIRECTION('center_axis',(-6.89206998773264E-18,4.35148173242952E-17,
-1.));
#119878=DIRECTION('ref_axis',(2.99907166502443E-34,1.,4.35148173242952E-17));
#119879=DIRECTION('center_axis',(-0.309016994374935,0.951056516295158,4.35148173242952E-17));
#119880=DIRECTION('ref_axis',(6.89206998773264E-18,-4.35148173242952E-17,
1.));
#119881=DIRECTION('center_axis',(-0.309016994374926,0.95105651629516,4.13514774560007E-15));
#119882=DIRECTION('ref_axis',(0.831842966945941,0.270282164133536,-0.484752338925627));
#119883=DIRECTION('',(-0.503988348013125,-0.163755740941349,0.84804469361924));
#119884=DIRECTION('',(0.951056516295158,0.309016994374935,6.89206998773264E-18));
#119885=DIRECTION('',(-0.503987849404011,-0.163755578933422,-0.848045021223107));
#119886=DIRECTION('center_axis',(-0.309016994374912,0.951056516295165,-4.49352824353855E-14));
#119887=DIRECTION('ref_axis',(0.831841183439609,0.270281584637207,0.484755722544655));
#119888=DIRECTION('',(-0.951056516295158,-0.309016994374935,1.33924836902178E-16));
#119889=DIRECTION('',(-0.475533025522885,-0.154510046201587,0.866022509672719));
#119890=DIRECTION('center_axis',(0.30901789486823,-0.951056223705265,1.63998885189632E-6));
#119891=DIRECTION('ref_axis',(0.8236837386523,0.26763107033019,-0.499918702264364));
#119892=DIRECTION('',(-0.951056516295158,-0.309016994374935,1.33924836902178E-16));
#119893=DIRECTION('center_axis',(0.309016093795513,-0.951056808909264,1.64014401908765E-6));
#119894=DIRECTION('ref_axis',(0.823656109180483,0.267622092735848,0.499969028330108));
#119895=DIRECTION('',(-0.475533174441007,-0.154510094588029,-0.866022419268957));
#119896=DIRECTION('',(-0.951056516295158,-0.309016994374935,1.33924836902178E-16));
#119897=DIRECTION('center_axis',(-0.309016994374935,0.951056516295158,4.35148173242952E-17));
#119898=DIRECTION('ref_axis',(6.89206998773264E-18,-4.35148173242952E-17,
1.));
#119899=DIRECTION('center_axis',(0.309016994374914,-0.951056516295165,2.96352322775422E-14));
#119900=DIRECTION('ref_axis',(0.831841183423017,0.27028158463181,0.484755722576136));
#119901=DIRECTION('',(0.503987849404013,0.163755578933423,0.848045021223105));
#119902=DIRECTION('',(-0.951056516295158,-0.309016994374935,-6.89206998773264E-18));
#119903=DIRECTION('',(0.503988348013112,0.163755740941343,-0.848044693619249));
#119904=DIRECTION('center_axis',(0.309016994374935,-0.951056516295158,1.92973561485194E-14));
#119905=DIRECTION('ref_axis',(0.831842966965813,0.27028216413999,-0.484752338887928));
#119906=DIRECTION('',(0.951056516295158,0.309016994374935,-1.33924836902178E-16));
#119907=DIRECTION('',(0.475533174441017,0.154510094588048,0.866022419268948));
#119908=DIRECTION('center_axis',(-0.309017895077531,0.951056223637258,1.64037041727555E-6));
#119909=DIRECTION('ref_axis',(0.823683836307394,0.267631102060501,0.49991852437754));
#119910=DIRECTION('',(0.951056516295158,0.309016994374935,-1.33924836902178E-16));
#119911=DIRECTION('center_axis',(-0.309016093996569,0.951056808843938,1.63977753815644E-6));
#119912=DIRECTION('ref_axis',(0.823656008171523,0.267622059916318,-0.499969212301216));
#119913=DIRECTION('',(0.47553302552284,0.15451004620159,-0.866022509672743));
#119914=DIRECTION('',(0.951056516295158,0.309016994374935,-1.33924836902178E-16));
#119915=DIRECTION('center_axis',(-3.07718727278846E-18,2.92774812072065E-17,
-1.));
#119916=DIRECTION('ref_axis',(0.,1.,2.92774812072065E-17));
#119917=DIRECTION('',(0.978147600733808,0.207911690817747,3.07718727278847E-18));
#119918=DIRECTION('center_axis',(3.07718727278846E-18,-2.92774812072065E-17,
1.));
#119919=DIRECTION('ref_axis',(2.25419682919892E-12,1.,2.92774812071996E-17));
#119920=DIRECTION('',(-0.978147600733808,-0.207911690817747,-3.07718727278847E-18));
#119921=DIRECTION('center_axis',(-3.07718727278846E-18,2.92774812072065E-17,
-1.));
#119922=DIRECTION('ref_axis',(9.00922925501191E-35,1.,2.92774812072065E-17));
#119923=DIRECTION('center_axis',(-0.207911690817747,0.978147600733808,2.92774812072065E-17));
#119924=DIRECTION('ref_axis',(3.07718727278847E-18,-2.92774812072065E-17,
1.));
#119925=DIRECTION('center_axis',(-0.207911690817745,0.978147600733809,2.75676516373318E-15));
#119926=DIRECTION('ref_axis',(0.855538223402063,0.18185026314361,-0.484752338924365));
#119927=DIRECTION('',(-0.518344583061394,-0.110177542335804,0.84804469361924));
#119928=DIRECTION('',(0.978147600733808,0.207911690817747,3.07718727278847E-18));
#119929=DIRECTION('',(-0.51834407024927,-0.110177433334225,-0.848045021223109));
#119930=DIRECTION('center_axis',(-0.207911690817745,0.978147600733809,7.0986719184735E-15));
#119931=DIRECTION('ref_axis',(0.855536389092103,0.181849873248987,0.484755722543399));
#119932=DIRECTION('',(-0.978147600733808,-0.207911690817747,1.37739719617122E-16));
#119933=DIRECTION('',(-0.489078703542048,-0.103956887610933,0.866022509672743));
#119934=DIRECTION('center_axis',(0.20791261696197,-0.978147403873944,1.63998878691659E-6));
#119935=DIRECTION('ref_axis',(0.847146577451719,0.1800665639041,-0.499918702266288));
#119936=DIRECTION('',(-0.978147600733808,-0.207911690817747,1.37739719617122E-16));
#119937=DIRECTION('center_axis',(0.207910764585278,-0.978147797608764,1.64014406418637E-6));
#119938=DIRECTION('ref_axis',(0.847118160921327,0.180060523555876,0.499969028334809));
#119939=DIRECTION('',(-0.489078856702224,-0.103956920166124,-0.866022419268935));
#119940=DIRECTION('',(-0.978147600733808,-0.207911690817747,1.37739719617122E-16));
#119941=DIRECTION('center_axis',(-0.207911690817747,0.978147600733808,2.92774812072065E-17));
#119942=DIRECTION('ref_axis',(3.07718727278847E-18,-2.92774812072065E-17,
1.));
#119943=DIRECTION('center_axis',(0.20791169081776,-0.978147600733805,-3.47352489950765E-14));
#119944=DIRECTION('ref_axis',(0.85553638907458,0.181849873245263,0.484755722575723));
#119945=DIRECTION('',(0.51834407024926,0.110177433334222,0.848045021223115));
#119946=DIRECTION('',(-0.978147600733808,-0.207911690817747,-3.07718727278847E-18));
#119947=DIRECTION('',(0.518344583061389,0.110177542335803,-0.848044693619244));
#119948=DIRECTION('center_axis',(0.207911690817756,-0.978147600733806,2.61203499296049E-14));
#119949=DIRECTION('ref_axis',(0.85553822342184,0.18185026314781,-0.484752338887884));
#119950=DIRECTION('',(0.978147600733808,0.207911690817747,-1.37739719617122E-16));
#119951=DIRECTION('',(0.48907885670221,0.103956920166112,0.866022419268945));
#119952=DIRECTION('center_axis',(-0.207912617177295,0.978147403828174,1.64037044739867E-6));
#119953=DIRECTION('ref_axis',(0.847146677890568,0.180066585253285,0.499918524375919));
#119954=DIRECTION('',(0.978147600733808,0.207911690817747,-1.37739719617122E-16));
#119955=DIRECTION('center_axis',(-0.207910764792043,0.978147797564815,1.63977759590673E-6));
#119956=DIRECTION('ref_axis',(0.847118057037499,0.180060501474941,-0.499969212301723));
#119957=DIRECTION('',(0.489078703542054,0.103956887610909,-0.866022509672743));
#119958=DIRECTION('',(0.978147600733808,0.207911690817747,-1.37739719617122E-16));
#119959=DIRECTION('center_axis',(-7.71409749858844E-19,1.47193748793047E-17,
-1.));
#119960=DIRECTION('ref_axis',(0.,1.,1.47193748793047E-17));
#119961=DIRECTION('',(0.994521895368275,0.10452846326764,7.71409749858844E-19));
#119962=DIRECTION('center_axis',(7.71409749858844E-19,-1.47193748793047E-17,
1.));
#119963=DIRECTION('ref_axis',(2.20623519453511E-12,1.,1.4719374879303E-17));
#119964=DIRECTION('',(-0.994521895368275,-0.10452846326764,-7.71409749858844E-19));
#119965=DIRECTION('center_axis',(-7.71409749858844E-19,1.47193748793047E-17,
-1.));
#119966=DIRECTION('ref_axis',(1.1354669293723E-35,1.,1.47193748793047E-17));
#119967=DIRECTION('center_axis',(-0.10452846326764,0.994521895368275,1.47193748793047E-17));
#119968=DIRECTION('ref_axis',(7.71409749858844E-19,-1.47193748793047E-17,
1.));
#119969=DIRECTION('center_axis',(-0.104528463267633,0.994521895368276,1.65405909823986E-14));
#119970=DIRECTION('ref_axis',(0.869860024050798,0.0914259726160318,-0.484752338921184));
#119971=DIRECTION('',(-0.527021726387079,-0.0553922155203004,0.848044693619231));
#119972=DIRECTION('',(0.994521895368275,0.10452846326764,7.71409749858844E-19));
#119973=DIRECTION('',(-0.527021204990416,-0.0553921607193045,-0.848045021223105));
#119974=DIRECTION('center_axis',(-0.104528463267648,0.994521895368274,1.14061184709465E-14));
#119975=DIRECTION('ref_axis',(0.869858159032786,0.0914257765947394,0.484755722542953));
#119976=DIRECTION('',(-0.994521895368275,-0.10452846326764,1.40045497140052E-16));
#119977=DIRECTION('',(-0.497265932938979,-0.0522647556052154,0.86602250967273));
#119978=DIRECTION('center_axis',(0.104529404915859,-0.994521796395256,1.63998887728709E-6));
#119979=DIRECTION('ref_axis',(0.861327901070781,0.0905292105226631,-0.499918702269825));
#119980=DIRECTION('',(-0.994521895368275,-0.10452846326764,1.40045497140052E-16));
#119981=DIRECTION('center_axis',(0.104527521530148,-0.99452199434707,1.64014406315375E-6));
#119982=DIRECTION('ref_axis',(0.861299008823921,0.0905261736006938,0.499969028332904));
#119983=DIRECTION('',(-0.497266088662994,-0.0522647719724685,-0.866022419268966));
#119984=DIRECTION('',(-0.994521895368275,-0.10452846326764,1.40045497140052E-16));
#119985=DIRECTION('center_axis',(-0.10452846326764,0.994521895368275,1.47193748793047E-17));
#119986=DIRECTION('ref_axis',(7.71409749858844E-19,-1.47193748793047E-17,
1.));
#119987=DIRECTION('center_axis',(0.104528463267637,-0.994521895368275,3.58379553123799E-15));
#119988=DIRECTION('ref_axis',(0.869858159015688,0.0914257765929404,0.484755722573974));
#119989=DIRECTION('',(0.527021204990409,0.0553921607193052,0.848045021223109));
#119990=DIRECTION('',(-0.994521895368275,-0.10452846326764,-7.71409749858844E-19));
#119991=DIRECTION('',(0.52702172638707,0.0553922155203008,-0.848044693619237));
#119992=DIRECTION('center_axis',(0.104528463267642,-0.994521895368275,3.99730948790747E-15));
#119993=DIRECTION('ref_axis',(0.86986002406859,0.0914259726178999,-0.484752338888904));
#119994=DIRECTION('',(0.994521895368275,0.10452846326764,-1.40045497140052E-16));
#119995=DIRECTION('',(0.497266088663062,0.0522647719724771,0.866022419268927));
#119996=DIRECTION('center_axis',(-0.104529405134726,0.994521796372251,1.6403704192978E-6));
#119997=DIRECTION('ref_axis',(0.861328003192725,0.0905292212563617,0.499918524376472));
#119998=DIRECTION('',(0.994521895368275,0.10452846326764,-1.40045497140052E-16));
#119999=DIRECTION('center_axis',(-0.104527521740357,0.994521994324977,1.6397776076981E-6));
#120000=DIRECTION('ref_axis',(0.861298903199663,0.0905261624993766,-0.499969212302312));
#120001=DIRECTION('',(0.497265932938956,0.0522647556052086,-0.866022509672744));
#120002=DIRECTION('',(0.994521895368275,0.10452846326764,-1.40045497140052E-16));
#120003=DIRECTION('center_axis',(0.994521895368273,-0.104528463267654,7.71409749859047E-19));
#120004=DIRECTION('ref_axis',(0.104528463267654,0.994521895368273,1.12125269189207E-32));
#120005=DIRECTION('center_axis',(-0.994521895368273,0.104528463267654,-7.71409749859047E-19));
#120006=DIRECTION('ref_axis',(-0.104528463267654,-0.994521895368273,-5.60397807285558E-36));
#120007=DIRECTION('center_axis',(0.978147600733806,-0.20791169081776,3.07718727278885E-18));
#120008=DIRECTION('ref_axis',(0.20791169081776,0.978147600733805,5.3337836051253E-32));
#120009=DIRECTION('center_axis',(-0.978147600733806,0.20791169081776,-3.07718727278885E-18));
#120010=DIRECTION('ref_axis',(-0.20791169081776,-0.978147600733805,2.17629115865656E-35));
#120011=DIRECTION('center_axis',(0.951056516295153,-0.309016994374948,6.89206998773323E-18));
#120012=DIRECTION('ref_axis',(0.309016994374948,0.951056516295153,2.1129734794752E-32));
#120013=DIRECTION('center_axis',(-0.951056516295153,0.309016994374948,-6.89206998773323E-18));
#120014=DIRECTION('ref_axis',(-0.309016994374948,-0.951056516295153,-3.51157074825093E-34));
#120015=DIRECTION('center_axis',(0.913545457642601,-0.406736643075801,1.21742612413517E-17));
#120016=DIRECTION('ref_axis',(0.406736643075801,0.913545457642601,-1.81348366517715E-31));
#120017=DIRECTION('center_axis',(-0.913545457642601,0.406736643075801,-1.21742612413517E-17));
#120018=DIRECTION('ref_axis',(-0.406736643075801,-0.9135454576426,1.31266757742093E-34));
#120019=DIRECTION('center_axis',(0.866025403784438,-0.500000000000001,1.88658882409001E-17));
#120020=DIRECTION('ref_axis',(0.500000000000001,0.866025403784438,8.56587576076706E-32));
#120021=DIRECTION('center_axis',(-0.866025403784438,0.500000000000001,-1.88658882409001E-17));
#120022=DIRECTION('ref_axis',(-0.500000000000001,-0.866025403784438,6.22903900877646E-34));
#120023=DIRECTION('center_axis',(0.809016994374947,-0.587785252292474,2.68936361206584E-17));
#120024=DIRECTION('ref_axis',(0.587785252292474,0.809016994374947,-4.93427012362456E-31));
#120025=DIRECTION('center_axis',(-0.809016994374947,0.587785252292474,-2.68936361206584E-17));
#120026=DIRECTION('ref_axis',(-0.587785252292474,-0.809016994374947,1.15372963471371E-33));
#120027=DIRECTION('center_axis',(0.743144825477393,-0.669130606358859,3.61695511949416E-17));
#120028=DIRECTION('ref_axis',(0.669130606358859,0.743144825477393,6.27086406135521E-31));
#120029=DIRECTION('center_axis',(-0.743144825477393,0.669130606358859,-3.61695511949416E-17));
#120030=DIRECTION('ref_axis',(-0.669130606358859,-0.743144825477393,7.72831234962683E-33));
#120031=DIRECTION('center_axis',(0.669130606358857,-0.743144825477395,4.6592004597086E-17));
#120032=DIRECTION('ref_axis',(0.743144825477396,0.669130606358857,-6.54359212772961E-31));
#120033=DIRECTION('center_axis',(-0.669130606358857,0.743144825477395,-4.6592004597086E-17));
#120034=DIRECTION('ref_axis',(-0.743144825477395,-0.669130606358857,4.37914107422688E-33));
#120035=DIRECTION('center_axis',(0.587785252292471,-0.809016994374949,5.8046805746579E-17));
#120036=DIRECTION('ref_axis',(0.809016994374949,0.587785252292471,1.26008547401877E-30));
#120037=DIRECTION('center_axis',(-0.587785252292471,0.809016994374949,-5.8046805746579E-17));
#120038=DIRECTION('ref_axis',(-0.809016994374949,-0.587785252292472,3.97684690788254E-33));
#120039=DIRECTION('center_axis',(0.499999999999998,-0.86602540378444,7.04084534449555E-17));
#120040=DIRECTION('ref_axis',(0.86602540378444,0.499999999999998,-7.7693955971012E-31));
#120041=DIRECTION('center_axis',(-0.499999999999998,0.86602540378444,-7.04084534449555E-17));
#120042=DIRECTION('ref_axis',(-0.86602540378444,-0.499999999999998,4.12230412422948E-33));
#120043=DIRECTION('center_axis',(0.406736643075798,-0.913545457642602,8.35415108931911E-17));
#120044=DIRECTION('ref_axis',(0.913545457642602,0.406736643075798,1.52177632324919E-30));
#120045=DIRECTION('center_axis',(-0.406736643075798,0.913545457642602,-8.35415108931911E-17));
#120046=DIRECTION('ref_axis',(-0.913545457642602,-0.406736643075798,-8.4716126159886E-33));
#120047=DIRECTION('center_axis',(0.309016994374945,-0.951056516295155,9.73020895656139E-17));
#120048=DIRECTION('ref_axis',(0.951056516295154,0.309016994374945,2.18819993268723E-32));
#120049=DIRECTION('center_axis',(-0.309016994374945,0.951056516295155,-9.73020895656139E-17));
#120050=DIRECTION('ref_axis',(-0.951056516295154,-0.309016994374945,-3.99634687419351E-33));
#120051=DIRECTION('center_axis',(0.207911690817756,-0.978147600733806,1.11539425682703E-16));
#120052=DIRECTION('ref_axis',(0.978147600733806,0.207911690817756,-1.55106258718425E-30));
#120053=DIRECTION('center_axis',(-0.207911690817756,0.978147600733806,-1.11539425682703E-16));
#120054=DIRECTION('ref_axis',(-0.978147600733806,-0.207911690817756,-8.73440025092029E-33));
#120055=DIRECTION('center_axis',(0.10452846326765,-0.994521895368274,1.26097532010604E-16));
#120056=DIRECTION('ref_axis',(0.994521895368274,0.10452846326765,-1.41047068150179E-30));
#120057=DIRECTION('center_axis',(-0.10452846326765,0.994521895368274,-1.26097532010604E-16));
#120058=DIRECTION('ref_axis',(-0.994521895368274,-0.10452846326765,6.75407294460559E-34));
#120059=DIRECTION('center_axis',(-3.49148133884313E-15,-1.,1.40816906889911E-16));
#120060=DIRECTION('ref_axis',(1.,-3.49148133884313E-15,4.91659602599735E-31));
#120061=DIRECTION('center_axis',(3.49148133884313E-15,1.,-1.40816906889911E-16));
#120062=DIRECTION('ref_axis',(-1.,3.49148133884313E-15,8.75811540203011E-47));
#120063=DIRECTION('center_axis',(-0.104528463267657,-0.994521895368273,
1.55536281769218E-16));
#120064=DIRECTION('ref_axis',(0.994521895368273,-0.104528463267657,2.79416186164968E-30));
#120065=DIRECTION('center_axis',(0.104528463267657,0.994521895368273,-1.55536281769218E-16));
#120066=DIRECTION('ref_axis',(-0.994521895368273,0.104528463267657,-2.13589730221744E-33));
#120067=DIRECTION('center_axis',(-0.207911690817763,-0.978147600733805,
1.70094388097119E-16));
#120068=DIRECTION('ref_axis',(0.978147600733805,-0.207911690817763,-3.06962581902968E-30));
#120069=DIRECTION('center_axis',(0.207911690817763,0.978147600733805,-1.70094388097119E-16));
#120070=DIRECTION('ref_axis',(-0.978147600733805,0.207911690817763,-1.74175573100342E-33));
#120071=DIRECTION('center_axis',(-0.309016994374951,-0.951056516295152,
1.84331724214208E-16));
#120072=DIRECTION('ref_axis',(0.951056516295152,-0.309016994374951,1.20064847815822E-30));
#120073=DIRECTION('center_axis',(0.309016994374951,0.951056516295152,-1.84331724214208E-16));
#120074=DIRECTION('ref_axis',(-0.951056516295152,0.309016994374951,-1.12286633426729E-32));
#120075=DIRECTION('center_axis',(-0.406736643075804,-0.913545457642599,
1.98092302886631E-16));
#120076=DIRECTION('ref_axis',(0.913545457642599,-0.406736643075804,-2.28374368880912E-30));
#120077=DIRECTION('center_axis',(0.406736643075804,0.913545457642599,-1.98092302886631E-16));
#120078=DIRECTION('ref_axis',(-0.913545457642599,0.406736643075804,-2.42004257715226E-33));
#120079=DIRECTION('center_axis',(-0.500000000000004,-0.866025403784436,
2.11225360334866E-16));
#120080=DIRECTION('ref_axis',(0.866025403784436,-0.500000000000004,1.67705471180066E-30));
#120081=DIRECTION('center_axis',(0.500000000000004,0.866025403784436,-2.11225360334866E-16));
#120082=DIRECTION('ref_axis',(-0.866025403784436,0.500000000000004,-2.24248448190466E-35));
#120083=DIRECTION('center_axis',(-0.587785252292477,-0.809016994374945,
2.23587008033243E-16));
#120084=DIRECTION('ref_axis',(0.809016994374945,-0.587785252292477,-3.32537644322472E-30));
#120085=DIRECTION('center_axis',(0.587785252292477,0.809016994374945,-2.23587008033243E-16));
#120086=DIRECTION('ref_axis',(-0.809016994374945,0.587785252292477,5.18779161054862E-33));
#120087=DIRECTION('center_axis',(-0.669130606358862,-0.743144825477391,
2.35041809182736E-16));
#120088=DIRECTION('ref_axis',(0.743144825477391,-0.669130606358862,4.90467981149431E-30));
#120089=DIRECTION('center_axis',(0.669130606358862,0.743144825477391,-2.35041809182736E-16));
#120090=DIRECTION('ref_axis',(-0.743144825477391,0.669130606358862,7.02183635389561E-33));
#120091=DIRECTION('center_axis',(-0.743144825477398,-0.669130606358854,
2.4546426258488E-16));
#120092=DIRECTION('ref_axis',(0.669130606358854,-0.743144825477398,-2.63996916307136E-30));
#120093=DIRECTION('center_axis',(0.743144825477398,0.669130606358854,-2.4546426258488E-16));
#120094=DIRECTION('ref_axis',(-0.669130606358854,0.743144825477398,-2.15782657736967E-33));
#120095=DIRECTION('center_axis',(-0.809016994374951,-0.587785252292469,
2.54740177659163E-16));
#120096=DIRECTION('ref_axis',(0.587785252292469,-0.80901699437495,6.34109604668436E-30));
#120097=DIRECTION('center_axis',(0.809016994374951,0.587785252292469,-2.54740177659163E-16));
#120098=DIRECTION('ref_axis',(-0.587785252292469,0.809016994374951,-1.15824900225317E-32));
#120099=DIRECTION('center_axis',(-0.866025403784442,-0.499999999999995,
2.62767925538921E-16));
#120100=DIRECTION('ref_axis',(0.499999999999995,-0.866025403784442,-1.95659843043102E-30));
#120101=DIRECTION('center_axis',(0.866025403784442,0.499999999999995,-2.62767925538921E-16));
#120102=DIRECTION('ref_axis',(-0.499999999999995,0.866025403784442,-1.55538326215048E-32));
#120103=DIRECTION('center_axis',(-0.913545457642603,-0.406736643075795,
2.6945955253847E-16));
#120104=DIRECTION('ref_axis',(0.406736643075795,-0.913545457642603,3.70089423175768E-30));
#120105=DIRECTION('center_axis',(0.913545457642603,0.406736643075795,-2.6945955253847E-16));
#120106=DIRECTION('ref_axis',(-0.406736643075795,0.913545457642603,-1.0068664273239E-32));
#120107=DIRECTION('center_axis',(-0.951056516295156,-0.309016994374942,
2.74741743792088E-16));
#120108=DIRECTION('ref_axis',(0.309016994374942,-0.951056516295155,1.00850339716061E-30));
#120109=DIRECTION('center_axis',(0.951056516295156,0.309016994374942,-2.74741743792088E-16));
#120110=DIRECTION('ref_axis',(-0.309016994374942,0.951056516295156,-2.05892830670188E-33));
#120111=DIRECTION('center_axis',(-0.978147600733807,-0.207911690817753,
2.78556626507032E-16));
#120112=DIRECTION('ref_axis',(0.207911690817753,-0.978147600733807,-2.97094794484635E-30));
#120113=DIRECTION('center_axis',(0.978147600733807,0.207911690817753,-2.78556626507032E-16));
#120114=DIRECTION('ref_axis',(-0.207911690817753,0.978147600733807,2.71817545091438E-33));
#120115=DIRECTION('center_axis',(-0.994521895368274,-0.104528463267647,
2.80862404029962E-16));
#120116=DIRECTION('ref_axis',(0.104528463267647,-0.994521895368274,-2.37338795252393E-30));
#120117=DIRECTION('center_axis',(0.994521895368274,0.104528463267647,-2.80862404029962E-16));
#120118=DIRECTION('ref_axis',(-0.104528463267647,0.994521895368274,5.68888447571522E-33));
#120119=DIRECTION('center_axis',(-1.,0.,2.81633813779821E-16));
#120120=DIRECTION('ref_axis',(2.81633813779821E-16,0.,1.));
#120121=DIRECTION('center_axis',(1.,0.,-2.81633813779821E-16));
#120122=DIRECTION('ref_axis',(-2.81633813779821E-16,0.,-1.));
#120123=DIRECTION('center_axis',(-0.994521895368273,0.104528463267661,2.80862404029962E-16));
#120124=DIRECTION('ref_axis',(-0.104528463267661,-0.994521895368273,-5.04412614481267E-30));
#120125=DIRECTION('center_axis',(0.994521895368273,-0.104528463267661,-2.80862404029962E-16));
#120126=DIRECTION('ref_axis',(0.104528463267661,0.994521895368273,6.74219343631748E-33));
#120127=DIRECTION('center_axis',(-0.978147600733804,0.207911690817766,2.78556626507032E-16));
#120128=DIRECTION('ref_axis',(-0.207911690817766,-0.978147600733804,-4.05861451950599E-30));
#120129=DIRECTION('center_axis',(0.978147600733804,-0.207911690817766,-2.78556626507032E-16));
#120130=DIRECTION('ref_axis',(0.207911690817766,0.978147600733804,1.6755092077588E-33));
#120131=DIRECTION('center_axis',(-0.951056516295151,0.309016994374955,2.74741743792088E-16));
#120132=DIRECTION('ref_axis',(-0.309016994374955,-0.951056516295151,2.69510815298916E-30));
#120133=DIRECTION('center_axis',(0.951056516295151,-0.309016994374955,-2.74741743792088E-16));
#120134=DIRECTION('ref_axis',(0.309016994374954,0.951056516295151,1.52765009372192E-33));
#120135=DIRECTION('center_axis',(-0.913545457642598,0.406736643075807,2.69459552538469E-16));
#120136=DIRECTION('ref_axis',(-0.406736643075807,-0.913545457642598,-2.24713220158703E-30));
#120137=DIRECTION('center_axis',(0.913545457642598,-0.406736643075807,-2.69459552538469E-16));
#120138=DIRECTION('ref_axis',(0.406736643075807,0.913545457642598,4.89387255474364E-33));
#120139=DIRECTION('center_axis',(-0.866025403784435,0.500000000000007,2.6276792553892E-16));
#120140=DIRECTION('ref_axis',(-0.500000000000007,-0.866025403784435,3.04674772188031E-30));
#120141=DIRECTION('center_axis',(0.866025403784435,-0.500000000000007,-2.6276792553892E-16));
#120142=DIRECTION('ref_axis',(0.500000000000007,0.866025403784435,1.00882858511171E-32));
#120143=DIRECTION('center_axis',(-0.809016994374943,0.58778525229248,2.54740177659162E-16));
#120144=DIRECTION('ref_axis',(-0.58778525229248,-0.809016994374943,-2.90930572432627E-30));
#120145=DIRECTION('center_axis',(0.809016994374943,-0.58778525229248,-2.54740177659162E-16));
#120146=DIRECTION('ref_axis',(0.58778525229248,0.809016994374943,-3.19259242211985E-33));
#120147=DIRECTION('center_axis',(-0.743144825477389,0.669130606358864,2.45464262584879E-16));
#120148=DIRECTION('ref_axis',(-0.669130606358864,-0.743144825477389,-5.46633698419621E-31));
#120149=DIRECTION('center_axis',(0.743144825477389,-0.669130606358864,-2.45464262584879E-16));
#120150=DIRECTION('ref_axis',(0.669130606358864,0.743144825477388,3.38071403517698E-33));
#120151=DIRECTION('center_axis',(-0.669130606358852,0.7431448254774,2.35041809182734E-16));
#120152=DIRECTION('ref_axis',(-0.7431448254774,-0.669130606358852,-1.71651837522136E-30));
#120153=DIRECTION('center_axis',(0.669130606358852,-0.7431448254774,-2.35041809182734E-16));
#120154=DIRECTION('ref_axis',(0.7431448254774,0.669130606358852,1.79927205836015E-32));
#120155=DIRECTION('center_axis',(-0.587785252292466,0.809016994374953,2.23587008033241E-16));
#120156=DIRECTION('ref_axis',(-0.809016994374953,-0.587785252292466,-8.24500195267044E-31));
#120157=DIRECTION('center_axis',(0.587785252292466,-0.809016994374953,-2.23587008033241E-16));
#120158=DIRECTION('ref_axis',(0.809016994374953,0.587785252292466,2.52047245046794E-33));
#120159=DIRECTION('center_axis',(-0.499999999999992,0.866025403784443,2.11225360334865E-16));
#120160=DIRECTION('ref_axis',(-0.866025403784443,-0.499999999999992,-8.42158487461594E-31));
#120161=DIRECTION('center_axis',(0.499999999999992,-0.866025403784443,-2.11225360334865E-16));
#120162=DIRECTION('ref_axis',(0.866025403784443,0.499999999999992,1.18398846415295E-32));
#120163=DIRECTION('center_axis',(-0.406736643075792,0.913545457642605,1.98092302886629E-16));
#120164=DIRECTION('ref_axis',(-0.913545457642605,-0.406736643075792,-3.87293527714641E-30));
#120165=DIRECTION('center_axis',(0.406736643075792,-0.913545457642605,-1.98092302886629E-16));
#120166=DIRECTION('ref_axis',(0.913545457642605,0.406736643075792,-1.20511778983704E-32));
#120167=DIRECTION('center_axis',(-0.309016994374938,0.951056516295157,1.84331724214206E-16));
#120168=DIRECTION('ref_axis',(-0.951056516295157,-0.309016994374938,1.32922675182072E-30));
#120169=DIRECTION('center_axis',(0.309016994374938,-0.951056516295157,-1.84331724214206E-16));
#120170=DIRECTION('ref_axis',(0.951056516295157,0.309016994374938,-4.09124323265046E-33));
#120171=DIRECTION('center_axis',(-0.207911690817749,0.978147600733808,1.70094388097117E-16));
#120172=DIRECTION('ref_axis',(-0.978147600733808,-0.207911690817749,-1.14066107666938E-30));
#120173=DIRECTION('center_axis',(0.207911690817749,-0.978147600733808,-1.70094388097117E-16));
#120174=DIRECTION('ref_axis',(0.978147600733808,0.207911690817749,2.34967611901948E-34));
#120175=DIRECTION('center_axis',(-0.104528463267644,0.994521895368275,1.55536281769216E-16));
#120176=DIRECTION('ref_axis',(-0.994521895368274,-0.104528463267644,-7.70551591036319E-31));
#120177=DIRECTION('center_axis',(0.104528463267644,-0.994521895368275,-1.55536281769216E-16));
#120178=DIRECTION('ref_axis',(0.994521895368274,0.104528463267644,1.28454224350036E-33));
#120179=DIRECTION('center_axis',(1.04744440165294E-14,1.,1.40816906889909E-16));
#120180=DIRECTION('ref_axis',(-1.,1.04744440165294E-14,1.47497880779919E-30));
#120181=DIRECTION('center_axis',(-1.04744440165294E-14,-1.,-1.40816906889909E-16));
#120182=DIRECTION('ref_axis',(1.,-1.04744440165294E-14,5.25486924121806E-46));
#120183=DIRECTION('center_axis',(0.104528463267664,0.994521895368272,1.26097532010602E-16));
#120184=DIRECTION('ref_axis',(-0.994521895368272,0.104528463267664,-1.87870457210236E-30));
#120185=DIRECTION('center_axis',(-0.104528463267664,-0.994521895368272,
-1.26097532010602E-16));
#120186=DIRECTION('ref_axis',(0.994521895368272,-0.104528463267664,1.52293880083755E-33));
#120187=DIRECTION('center_axis',(0.20791169081777,0.978147600733803,1.11539425682701E-16));
#120188=DIRECTION('ref_axis',(-0.978147600733803,0.20791169081777,-1.23488624019268E-30));
#120189=DIRECTION('center_axis',(-0.20791169081777,-0.978147600733803,-1.11539425682701E-16));
#120190=DIRECTION('ref_axis',(0.978147600733803,-0.20791169081777,6.98244303227918E-33));
#120191=DIRECTION('center_axis',(0.309016994374957,0.95105651629515,9.73020895656121E-17));
#120192=DIRECTION('ref_axis',(-0.95105651629515,0.309016994374957,1.25555458542293E-30));
#120193=DIRECTION('center_axis',(-0.309016994374957,-0.95105651629515,-9.73020895656121E-17));
#120194=DIRECTION('ref_axis',(0.95105651629515,-0.309016994374957,-1.05677412542168E-33));
#120195=DIRECTION('center_axis',(0.40673664307581,0.913545457642596,8.35415108931894E-17));
#120196=DIRECTION('ref_axis',(-0.913545457642597,0.40673664307581,-3.95491880831218E-31));
#120197=DIRECTION('center_axis',(-0.40673664307581,-0.913545457642596,-8.35415108931894E-17));
#120198=DIRECTION('ref_axis',(0.913545457642596,-0.40673664307581,1.14994985725664E-33));
#120199=DIRECTION('center_axis',(0.50000000000001,0.866025403784433,7.04084534449538E-17));
#120200=DIRECTION('ref_axis',(-0.866025403784433,0.50000000000001,-1.35169061292236E-30));
#120201=DIRECTION('center_axis',(-0.50000000000001,-0.866025403784433,-7.04084534449538E-17));
#120202=DIRECTION('ref_axis',(0.866025403784433,-0.50000000000001,3.15276542668096E-33));
#120203=DIRECTION('center_axis',(0.587785252292482,0.809016994374941,5.80468057465775E-17));
#120204=DIRECTION('ref_axis',(-0.809016994374941,0.587785252292482,-4.87668228627595E-31));
#120205=DIRECTION('center_axis',(-0.587785252292482,-0.809016994374941,
-5.80468057465775E-17));
#120206=DIRECTION('ref_axis',(0.809016994374941,-0.587785252292482,-7.07752156141996E-33));
#120207=DIRECTION('center_axis',(0.669130606358867,0.743144825477386,4.65920045970846E-17));
#120208=DIRECTION('ref_axis',(-0.743144825477386,0.669130606358867,6.2996129283645E-32));
#120209=DIRECTION('center_axis',(-0.669130606358867,-0.743144825477386,
-4.65920045970846E-17));
#120210=DIRECTION('ref_axis',(0.743144825477386,-0.669130606358867,-1.70435726196324E-33));
#120211=DIRECTION('center_axis',(0.743144825477402,0.66913060635885,3.61695511949404E-17));
#120212=DIRECTION('ref_axis',(-0.66913060635885,0.743144825477402,-1.54743219885707E-31));
#120213=DIRECTION('center_axis',(-0.743144825477402,-0.66913060635885,-3.61695511949404E-17));
#120214=DIRECTION('ref_axis',(0.66913060635885,-0.743144825477402,-1.64364935203297E-33));
#120215=DIRECTION('center_axis',(0.809016994374955,0.587785252292463,2.68936361206573E-17));
#120216=DIRECTION('ref_axis',(-0.587785252292463,0.809016994374955,-6.32658501432878E-31));
#120217=DIRECTION('center_axis',(-0.809016994374955,-0.587785252292463,
-2.68936361206573E-17));
#120218=DIRECTION('ref_axis',(0.587785252292463,-0.809016994374955,5.77490301261619E-34));
#120219=DIRECTION('center_axis',(0.866025403784445,0.499999999999989,1.88658882408992E-17));
#120220=DIRECTION('ref_axis',(-0.499999999999989,0.866025403784445,-9.02647084236321E-33));
#120221=DIRECTION('center_axis',(-0.866025403784445,-0.499999999999989,
-1.88658882408992E-17));
#120222=DIRECTION('ref_axis',(0.499999999999989,-0.866025403784445,-2.17992890695449E-34));
#120223=DIRECTION('center_axis',(0.913545457642606,0.406736643075789,1.2174261241351E-17));
#120224=DIRECTION('ref_axis',(-0.406736643075789,0.913545457642606,-1.9369316171316E-31));
#120225=DIRECTION('center_axis',(-0.913545457642606,-0.406736643075789,
-1.2174261241351E-17));
#120226=DIRECTION('ref_axis',(0.406736643075789,-0.913545457642606,-6.72158879142273E-34));
#120227=DIRECTION('center_axis',(0.951056516295158,0.309016994374935,6.89206998773264E-18));
#120228=DIRECTION('ref_axis',(-0.309016994374935,0.951056516295158,7.38462266190487E-32));
#120229=DIRECTION('center_axis',(-0.951056516295158,-0.309016994374935,
-6.89206998773264E-18));
#120230=DIRECTION('ref_axis',(0.309016994374935,-0.951056516295158,1.7074848336093E-34));
#120231=DIRECTION('center_axis',(0.978147600733808,0.207911690817747,3.07718727278847E-18));
#120232=DIRECTION('ref_axis',(-0.207911690817747,0.978147600733808,-1.89718420003736E-32));
#120233=DIRECTION('center_axis',(-0.978147600733808,-0.207911690817747,
-3.07718727278847E-18));
#120234=DIRECTION('ref_axis',(0.207911690817747,-0.978147600733808,5.10419938729071E-35));
#120235=DIRECTION('center_axis',(0.994521895368275,0.10452846326764,7.71409749858844E-19));
#120236=DIRECTION('ref_axis',(-0.10452846326764,0.994521895368275,-1.11530674608181E-33));
#120237=DIRECTION('center_axis',(-0.994521895368275,-0.10452846326764,-7.71409749858844E-19));
#120238=DIRECTION('ref_axis',(0.10452846326764,-0.994521895368275,2.19054274915971E-35));
#120239=DIRECTION('center_axis',(-0.497265934575652,0.0522647557772525,
0.866022508722578));
#120240=DIRECTION('ref_axis',(0.104528463268683,0.994521895368165,5.94450124796257E-13));
#120241=DIRECTION('center_axis',(-0.86127722484323,0.0904936763723186,0.500012436348305));
#120242=DIRECTION('ref_axis',(0.49716964624231,-0.0532497882904349,0.866017784403023));
#120243=DIRECTION('center_axis',(0.497265943181924,-0.0522647566817888,
-0.866022503726309));
#120244=DIRECTION('ref_axis',(-0.867207748104374,9.14067291315517E-16,-0.497946504785143));
#120245=DIRECTION('center_axis',(0.994521895368276,-0.104528463267628,0.));
#120246=DIRECTION('ref_axis',(0.104528463267628,0.994521895368276,0.));
#120247=DIRECTION('center_axis',(-0.994521895368273,0.104528463267654,1.40045497140051E-16));
#120248=DIRECTION('ref_axis',(-0.104528463267654,-0.994521895368273,1.88774370219345E-33));
#120249=DIRECTION('center_axis',(-0.994521895368276,0.104528463267629,-1.42777936329238E-15));
#120250=DIRECTION('ref_axis',(-0.104528463267629,-0.994521895368276,-1.03141617847887E-30));
#120251=DIRECTION('center_axis',(-0.994521895368273,0.104528463267654,1.40045497140051E-16));
#120252=DIRECTION('ref_axis',(-0.104528463267654,-0.994521895368273,1.88774370219345E-33));
#120253=DIRECTION('center_axis',(0.994521895368276,-0.104528463267628,0.));
#120254=DIRECTION('ref_axis',(0.104528463267628,0.994521895368276,0.));
#120255=DIRECTION('center_axis',(-0.527021232978597,0.0553921636609763,
-0.848045003637587));
#120256=DIRECTION('ref_axis',(-0.849349030019387,-1.18520091513627E-15,
0.527831625809904));
#120257=DIRECTION('center_axis',(0.497266077958583,-0.0522647708474063,
0.866022425483288));
#120258=DIRECTION('ref_axis',(0.867207670398076,2.13898382432694E-16,-0.497946640115929));
#120259=DIRECTION('center_axis',(0.52702120261152,-0.0553921822138802,0.848045021297509));
#120260=DIRECTION('ref_axis',(0.842941044395424,-0.0929299148179921,-0.529919264233215));
#120261=DIRECTION('center_axis',(-0.527021177161361,0.0553921577943484,
-0.84804503870864));
#120262=DIRECTION('ref_axis',(-0.84934906486751,-4.67755375184424E-16,0.527831569734783));
#120263=DIRECTION('center_axis',(0.497266090634776,-0.0522647827596761,
0.866022417485766));
#120264=DIRECTION('ref_axis',(0.86079389248998,-0.0950466972174585,-0.500000000000001));
#120265=DIRECTION('center_axis',(0.861296695145091,-0.0904912830030048,
0.499979330205374));
#120266=DIRECTION('ref_axis',(0.497340894869929,-0.0513033469932807,-0.866036951219326));
#120267=DIRECTION('center_axis',(-0.104769627595161,-0.994496518411991,
6.79203329632462E-15));
#120268=DIRECTION('ref_axis',(0.994496518411991,-0.104769627595161,3.19732566850161E-29));
#120269=DIRECTION('center_axis',(-0.994521895368273,0.104528463267654,1.40045497140051E-16));
#120270=DIRECTION('ref_axis',(-0.104528463267654,-0.994521895368273,1.88774370219345E-33));
#120271=DIRECTION('center_axis',(0.994521895368276,-0.104528463267627,0.));
#120272=DIRECTION('ref_axis',(0.104528463267627,0.994521895368276,0.));
#120273=DIRECTION('center_axis',(-7.71409749859041E-19,-1.47193748793066E-17,
-1.));
#120274=DIRECTION('ref_axis',(0.,1.,0.));
#120275=DIRECTION('center_axis',(-0.104287292793436,-0.994547213842468,
0.));
#120276=DIRECTION('ref_axis',(0.994547213842468,-0.104287292793436,0.));
#120277=DIRECTION('center_axis',(0.52702169399903,-0.0553922121162226,-0.848044713969295));
#120278=DIRECTION('ref_axis',(-0.849348742192381,8.56035801599993E-16,-0.527832088960325));
#120279=DIRECTION('center_axis',(0.52702117716142,-0.0553921577944011,0.8480450387086));
#120280=DIRECTION('ref_axis',(0.849349064867473,2.16233168370015E-16,-0.527831569734843));
#120281=DIRECTION('center_axis',(0.527021729069701,-0.0553921904551721,
-0.848044693589295));
#120282=DIRECTION('ref_axis',(-0.842916495802325,0.0931523188055466,-0.529919264233222));
#120283=DIRECTION('center_axis',(0.527021758969982,-0.0553922189448986,
-0.848044673146731));
#120284=DIRECTION('ref_axis',(-0.849348701629304,3.9911212985723E-16,-0.527832154231452));
#120285=DIRECTION('center_axis',(-0.527021202762352,0.0553921822934361,
-0.848045021198577));
#120286=DIRECTION('ref_axis',(0.843841975851001,-0.0843581246018643,-0.529919264233275));
#120287=DIRECTION('center_axis',(0.527021232978612,-0.0553921636609779,
0.848045003637578));
#120288=DIRECTION('ref_axis',(0.849349030019378,-4.13967457904561E-16,-0.527831625809918));
#120289=DIRECTION('center_axis',(-0.10478522557409,-0.994494875050338,0.));
#120290=DIRECTION('ref_axis',(0.994494875050338,-0.10478522557409,0.));
#120291=DIRECTION('center_axis',(0.994521895368276,-0.104528463267629,0.));
#120292=DIRECTION('ref_axis',(0.104528463267629,0.994521895368276,0.));
#120293=DIRECTION('center_axis',(-7.71409749859041E-19,-1.47193748793066E-17,
-1.));
#120294=DIRECTION('ref_axis',(0.,1.,0.));
#120295=DIRECTION('center_axis',(-0.104271693993672,-0.994548849394382,
6.79239069704775E-15));
#120296=DIRECTION('ref_axis',(0.994548849394382,-0.104271693993672,1.8061767832882E-30));
#120297=DIRECTION('center_axis',(0.994521895368273,-0.104528463267654,-1.40045497140051E-16));
#120298=DIRECTION('ref_axis',(0.104528463267654,0.994521895368273,-3.47023617217699E-30));
#120299=DIRECTION('center_axis',(0.861270944309928,-0.0905534316539297,
-0.500012436348519));
#120300=DIRECTION('ref_axis',(0.497376550150566,-0.0512812291022556,0.866017784402886));
#120301=DIRECTION('center_axis',(-0.527021758969975,0.0553922189448978,
0.848044673146736));
#120302=DIRECTION('ref_axis',(0.849348701629309,-8.88691521652723E-16,0.527832154231445));
#120303=DIRECTION('center_axis',(-0.497265930897887,0.0522647452181895,
0.866022511471576));
#120304=DIRECTION('ref_axis',(-0.861737632556526,0.0860712067763655,-0.499999999999934));
#120305=DIRECTION('center_axis',(0.497265943181814,-0.0522647566817776,
-0.866022503726373));
#120306=DIRECTION('ref_axis',(-0.867207748104437,-2.31772315575697E-16,
-0.497946504785033));
#120307=DIRECTION('center_axis',(-0.52702172888514,0.055392190353939,0.848044693710603));
#120308=DIRECTION('ref_axis',(-0.843864204095268,0.0841354767099045,-0.5299192642332));
#120309=DIRECTION('center_axis',(-0.527021693998978,0.0553922121161999,
0.848044713969329));
#120310=DIRECTION('ref_axis',(0.849348742192414,-1.18056289443676E-16,0.527832088960272));
#120311=DIRECTION('center_axis',(0.994521895368276,-0.104528463267629,0.));
#120312=DIRECTION('ref_axis',(0.104528463267629,0.994521895368276,0.));
#120313=DIRECTION('center_axis',(-0.994521895368276,0.104528463267629,0.));
#120314=DIRECTION('ref_axis',(-0.104528463267629,-0.994521895368276,0.));
#120315=DIRECTION('center_axis',(0.994521895368273,-0.104528463267654,-1.40045497140051E-16));
#120316=DIRECTION('ref_axis',(0.104528463267654,0.994521895368273,-3.47023617217699E-30));
#120317=DIRECTION('center_axis',(0.994521895368276,-0.104528463267629,-7.13889681646191E-16));
#120318=DIRECTION('ref_axis',(0.104528463267629,0.994521895368276,-5.15708089239434E-31));
#120319=DIRECTION('center_axis',(0.994521895368273,-0.104528463267654,-1.40045497140051E-16));
#120320=DIRECTION('ref_axis',(0.104528463267654,0.994521895368273,-3.47023617217699E-30));
#120321=DIRECTION('center_axis',(-0.861289491529685,0.0905598208268781,
-0.4999793302051));
#120322=DIRECTION('ref_axis',(0.497139368681443,-0.0532207405949754,-0.866036951219484));
#120323=DIRECTION('center_axis',(0.497266077958573,-0.0522647708473857,
0.866022425483295));
#120324=DIRECTION('ref_axis',(0.867207670398082,-3.99694090177787E-16,-0.497946640115919));
#120325=DIRECTION('center_axis',(0.497266086881316,-0.0522647717852188,
0.866022420303298));
#120326=DIRECTION('ref_axis',(-0.104528463263483,-0.994521895368712,-2.44773579649901E-12));
#120327=DIRECTION('center_axis',(-0.489078705154303,0.103956887953619,0.866022508721101));
#120328=DIRECTION('ref_axis',(0.207911690815745,0.978147600734234,-1.18890024958885E-12));
#120329=DIRECTION('center_axis',(-0.84709989316159,0.180025927305589,0.500012436348723));
#120330=DIRECTION('ref_axis',(0.488879980351047,-0.104926459533017,0.866017784402737));
#120331=DIRECTION('center_axis',(0.489078713616375,-0.103956889752293,-0.866022503726307));
#120332=DIRECTION('ref_axis',(-0.8707403454847,1.23854993518449E-15,-0.491743073916843));
#120333=DIRECTION('center_axis',(0.978147600733807,-0.207911690817754,0.));
#120334=DIRECTION('ref_axis',(0.207911690817754,0.978147600733807,0.));
#120335=DIRECTION('center_axis',(-0.978147600733806,0.20791169081776,1.37739719617122E-16));
#120336=DIRECTION('ref_axis',(-0.20791169081776,-0.978147600733805,-5.54372792423441E-34));
#120337=DIRECTION('center_axis',(-0.978147600733806,0.207911690817757,0.));
#120338=DIRECTION('ref_axis',(-0.207911690817757,-0.978147600733806,0.));
#120339=DIRECTION('center_axis',(-0.978147600733806,0.20791169081776,1.37739719617122E-16));
#120340=DIRECTION('ref_axis',(-0.20791169081776,-0.978147600733805,-5.54372792423441E-34));
#120341=DIRECTION('center_axis',(0.978147600733806,-0.207911690817757,0.));
#120342=DIRECTION('ref_axis',(0.207911690817757,0.978147600733806,0.));
#120343=DIRECTION('center_axis',(-0.518344097776643,0.110177439185352,-0.848045003637588));
#120344=DIRECTION('ref_axis',(-0.853239582811875,-1.68392254271072E-15,
0.521519140898028));
#120345=DIRECTION('center_axis',(0.489078846174041,-0.103956917928293,0.866022425483266));
#120346=DIRECTION('ref_axis',(0.870740269393754,4.19086328667376E-16,-0.491743208652741));
#120347=DIRECTION('center_axis',(0.518344065636325,-0.110177454463846,0.848045021297497));
#120348=DIRECTION('ref_axis',(0.828609503966741,-0.180532167024357,-0.529919264233224));
#120349=DIRECTION('center_axis',(-0.518344042878402,0.11017742751637,-0.848045038708646));
#120350=DIRECTION('ref_axis',(-0.853239616987301,8.06953644704382E-16,0.521519084984782));
#120351=DIRECTION('center_axis',(0.48907885753683,-0.103956931094349,0.866022417485779));
#120352=DIRECTION('ref_axis',(0.846143288282877,-0.18450348423235,-0.499999999999963));
#120353=DIRECTION('center_axis',(0.847119506978939,-0.180025582247288,0.499979330205044));
#120354=DIRECTION('ref_axis',(0.489253749388313,-0.103008581350701,-0.866036951219516));
#120355=DIRECTION('center_axis',(-0.208148881407599,-0.978097154258597,
0.));
#120356=DIRECTION('ref_axis',(0.978097154258597,-0.2081488814076,0.));
#120357=DIRECTION('center_axis',(-0.978147600733806,0.20791169081776,1.37739719617122E-16));
#120358=DIRECTION('ref_axis',(-0.20791169081776,-0.978147600733805,-5.54372792423441E-34));
#120359=DIRECTION('center_axis',(0.978147600733806,-0.207911690817757,0.));
#120360=DIRECTION('ref_axis',(0.207911690817757,0.978147600733806,0.));
#120361=DIRECTION('center_axis',(-3.07718727278886E-18,-2.92774812072083E-17,
-1.));
#120362=DIRECTION('ref_axis',(0.,1.,0.));
#120363=DIRECTION('center_axis',(-0.20767448800182,-0.978197989689808,0.));
#120364=DIRECTION('ref_axis',(0.978197989689808,-0.20767448800182,0.));
#120365=DIRECTION('center_axis',(0.518344551206617,-0.11017753556485,-0.848044713969297));
#120366=DIRECTION('ref_axis',(-0.85323930054102,-8.4671885596076E-16,-0.521519602711414));
#120367=DIRECTION('center_axis',(0.518344042878406,-0.110177427516371,0.848045038708643));
#120368=DIRECTION('ref_axis',(0.853239616987298,-2.86146343343731E-16,-0.521519084984786));
#120369=DIRECTION('center_axis',(0.518344588349843,-0.110177517686205,-0.848044693589281));
#120370=DIRECTION('ref_axis',(-0.828561842307295,0.18075078662857,-0.529919264233236));
#120371=DIRECTION('center_axis',(0.518344615107834,-0.110177549147491,-0.848044673146742));
#120372=DIRECTION('ref_axis',(-0.853239260760976,-2.80784050022121E-15,
-0.521519667794095));
#120373=DIRECTION('center_axis',(-0.518344065777496,0.110177454561188,-0.848045021198564));
#120374=DIRECTION('ref_axis',(0.83040149609203,-0.172101506915709,-0.529919264233205));
#120375=DIRECTION('center_axis',(0.518344097776693,-0.110177439185362,0.848045003637556));
#120376=DIRECTION('ref_axis',(0.853239582811844,4.32157940244689E-18,-0.521519140898079));
#120377=DIRECTION('center_axis',(-0.208164222161104,-0.978093889466682,
0.));
#120378=DIRECTION('ref_axis',(0.978093889466682,-0.208164222161104,0.));
#120379=DIRECTION('center_axis',(0.978147600733806,-0.207911690817757,0.));
#120380=DIRECTION('ref_axis',(0.207911690817757,0.978147600733806,0.));
#120381=DIRECTION('center_axis',(-3.07718727278886E-18,-2.92774812072083E-17,
-1.));
#120382=DIRECTION('ref_axis',(0.,1.,0.));
#120383=DIRECTION('center_axis',(-0.207659145615656,-0.978201246800563,
0.));
#120384=DIRECTION('ref_axis',(0.978201246800563,-0.207659145615656,0.));
#120385=DIRECTION('center_axis',(0.978147600733806,-0.20791169081776,-1.37739719617122E-16));
#120386=DIRECTION('ref_axis',(0.20791169081776,0.978147600733806,-3.77399900463914E-31));
#120387=DIRECTION('center_axis',(0.847087400906584,-0.180084698746639,-0.500012436347998));
#120388=DIRECTION('ref_axis',(0.489291521293116,-0.10299031162228,0.866017784403192));
#120389=DIRECTION('center_axis',(-0.518344615107832,0.110177549147519,0.848044673146739));
#120390=DIRECTION('ref_axis',(0.853239260760976,2.80072453551802E-15,0.521519667794095));
#120391=DIRECTION('center_axis',(-0.489078702597035,0.103956877071927,0.866022511471528));
#120392=DIRECTION('ref_axis',(-0.848020052664818,0.175675810168452,-0.500000000000017));
#120393=DIRECTION('center_axis',(0.489078713616259,-0.103956889752268,-0.866022503726375));
#120394=DIRECTION('ref_axis',(-0.870740345484766,2.53322569711339E-15,-0.491743073916726));
#120395=DIRECTION('center_axis',(-0.518344588176244,0.11017751756908,0.848044693710606));
#120396=DIRECTION('ref_axis',(-0.830446875604741,0.171882402219908,-0.529919264233183));
#120397=DIRECTION('center_axis',(-0.518344551206558,0.110177535564884,0.848044713969329));
#120398=DIRECTION('ref_axis',(0.853239300541055,1.68070280509443E-15,0.521519602711356));
#120399=DIRECTION('center_axis',(0.978147600733806,-0.207911690817757,0.));
#120400=DIRECTION('ref_axis',(0.207911690817757,0.978147600733806,0.));
#120401=DIRECTION('center_axis',(-0.978147600733806,0.207911690817757,0.));
#120402=DIRECTION('ref_axis',(-0.207911690817757,-0.978147600733806,0.));
#120403=DIRECTION('center_axis',(0.978147600733806,-0.20791169081776,-1.37739719617122E-16));
#120404=DIRECTION('ref_axis',(0.20791169081776,0.978147600733806,-3.77399900463914E-31));
#120405=DIRECTION('center_axis',(0.978147600733806,-0.207911690817757,-2.83991567709912E-15));
#120406=DIRECTION('ref_axis',(0.207911690817757,0.978147600733806,-3.75217731718872E-32));
#120407=DIRECTION('center_axis',(0.978147600733806,-0.20791169081776,-1.37739719617122E-16));
#120408=DIRECTION('ref_axis',(0.20791169081776,0.978147600733806,-3.77399900463914E-31));
#120409=DIRECTION('center_axis',(-0.847105178672012,0.18009299163106,-0.499979330205193));
#120410=DIRECTION('ref_axis',(0.488852904976213,-0.104894406041813,-0.866036951219434));
#120411=DIRECTION('center_axis',(0.489078846174021,-0.10395691792829,0.866022425483278));
#120412=DIRECTION('ref_axis',(0.870740269393765,2.98920110677976E-15,-0.491743208652721));
#120413=DIRECTION('center_axis',(0.489078854952772,-0.103956919794272,0.866022420301561));
#120414=DIRECTION('ref_axis',(-0.207911690815506,-0.978147600734285,-1.36373851518786E-12));
#120415=DIRECTION('center_axis',(-0.475533027087639,0.154510046710004,0.866022508722804));
#120416=DIRECTION('ref_axis',(0.309016994373617,0.951056516295586,-7.69288396791546E-13));
#120417=DIRECTION('center_axis',(-0.823641557784419,0.267585776505498,0.500012436347742));
#120418=DIRECTION('ref_axis',(0.475234043097329,-0.155453534467842,0.866017784403312));
#120419=DIRECTION('center_axis',(0.475533035318149,-0.154510049384271,-0.866022503726305));
#120420=DIRECTION('ref_axis',(-0.876548788012431,-5.39585338525745E-15,
-0.481313018974075));
#120421=DIRECTION('center_axis',(0.951056516295146,-0.309016994374972,0.));
#120422=DIRECTION('ref_axis',(0.309016994374972,0.951056516295146,0.));
#120423=DIRECTION('center_axis',(-0.951056516295153,0.309016994374948,1.33924836902177E-16));
#120424=DIRECTION('ref_axis',(-0.309016994374948,-0.951056516295153,2.44548634228625E-33));
#120425=DIRECTION('center_axis',(-0.951056516295148,0.309016994374964,0.));
#120426=DIRECTION('ref_axis',(-0.309016994374964,-0.951056516295148,0.));
#120427=DIRECTION('center_axis',(-0.951056516295153,0.309016994374948,1.33924836902177E-16));
#120428=DIRECTION('ref_axis',(-0.309016994374948,-0.951056516295153,-9.88046530179205E-33));
#120429=DIRECTION('center_axis',(0.951056516295165,-0.309016994374914,0.));
#120430=DIRECTION('ref_axis',(0.309016994374914,0.951056516295164,0.));
#120431=DIRECTION('center_axis',(-0.503987876168977,0.163755587629901,-0.848045003637584));
#120432=DIRECTION('ref_axis',(-0.859649462041493,-1.98479274860628E-15,
0.510884333691857));
#120433=DIRECTION('center_axis',(0.475533164204456,-0.154510091261994,0.86602242548326));
#120434=DIRECTION('ref_axis',(0.87654871462881,-1.83225743718063E-16,-0.481313152617483));
#120435=DIRECTION('center_axis',(0.503987842609227,-0.163755599460403,0.848045021297491));
#120436=DIRECTION('ref_axis',(0.805199544420487,-0.266156471008179,-0.529919264233254));
#120437=DIRECTION('center_axis',(-0.503987822791217,0.163755570286415,-0.848045038708641));
#120438=DIRECTION('ref_axis',(-0.859649495083695,-2.20730751304904E-15,
0.510884278092748));
#120439=DIRECTION('center_axis',(0.475533174128361,-0.154510105545038,0.866022417485753));
#120440=DIRECTION('ref_axis',(0.822222161142858,-0.271938812466216,-0.500000000000033));
#120441=DIRECTION('center_axis',(0.823661100222795,-0.267587483540072,0.499979330205226));
#120442=DIRECTION('ref_axis',(0.475806237441931,-0.153585232147895,-0.866036951219421));
#120443=DIRECTION('center_axis',(-0.309247612517368,-0.950981553003163,
0.));
#120444=DIRECTION('ref_axis',(0.950981553003163,-0.309247612517368,0.));
#120445=DIRECTION('center_axis',(-0.951056516295153,0.309016994374948,1.33924836902177E-16));
#120446=DIRECTION('ref_axis',(-0.309016994374948,-0.951056516295153,2.44548634228625E-33));
#120447=DIRECTION('center_axis',(0.951056516295165,-0.309016994374914,0.));
#120448=DIRECTION('ref_axis',(0.309016994374914,0.951056516295164,0.));
#120449=DIRECTION('center_axis',(-6.89206998773325E-18,-4.35148173242971E-17,
-1.));
#120450=DIRECTION('ref_axis',(0.,1.,0.));
#120451=DIRECTION('center_axis',(-0.308786358061007,-0.95113142366101,0.));
#120452=DIRECTION('ref_axis',(0.95113142366101,-0.308786358061007,0.));
#120453=DIRECTION('center_axis',(0.503988317040591,-0.163755730877772,-0.848044713969304));
#120454=DIRECTION('ref_axis',(-0.859649189130459,-2.98011051076997E-15,
-0.510884792910637));
#120455=DIRECTION('center_axis',(0.503987822791257,-0.163755570286477,0.848045038708605));
#120456=DIRECTION('ref_axis',(0.859649495083668,3.24166635856024E-15,-0.510884278092793));
#120457=DIRECTION('center_axis',(0.50398835585061,-0.163755716975207,-0.84804469358928));
#120458=DIRECTION('ref_axis',(-0.80512929187801,0.266368911013597,-0.529919264233189));
#120459=DIRECTION('center_axis',(0.503988379172007,-0.163755751065444,-0.848044673146743));
#120460=DIRECTION('ref_axis',(-0.859649150669465,-1.48397689224786E-15,
-0.510884857627692));
#120461=DIRECTION('center_axis',(-0.503987842737447,0.163755599578063,-0.84804502119857));
#120462=DIRECTION('ref_axis',(0.807862963766411,-0.257959309134419,-0.529919264233189));
#120463=DIRECTION('center_axis',(0.503987876169007,-0.163755587629911,0.848045003637564));
#120464=DIRECTION('ref_axis',(0.859649462041474,1.63915119993853E-16,-0.510884333691888));
#120465=DIRECTION('center_axis',(-0.309262527968962,-0.950976702550723,
-1.68971643309507E-14));
#120466=DIRECTION('ref_axis',(0.950976702550723,-0.309262527968962,2.40620234987808E-29));
#120467=DIRECTION('center_axis',(0.951056516295148,-0.309016994374964,-5.19628367180436E-14));
#120468=DIRECTION('ref_axis',(0.309016994374964,0.951056516295148,4.43497354731716E-28));
#120469=DIRECTION('center_axis',(-6.89206998773325E-18,-4.35148173242971E-17,
-1.));
#120470=DIRECTION('ref_axis',(0.,1.,0.));
#120471=DIRECTION('center_axis',(-0.308771440182806,-0.951136266645025,
0.));
#120472=DIRECTION('ref_axis',(0.951136266645025,-0.308771440182806,0.));
#120473=DIRECTION('center_axis',(0.951056516295153,-0.309016994374948,-1.33924836902177E-16));
#120474=DIRECTION('ref_axis',(0.309016994374948,0.951056516295153,2.18771486896698E-30));
#120475=DIRECTION('center_axis',(0.823622990673383,-0.267642920194819,-0.500012436349159));
#120476=DIRECTION('ref_axis',(0.475845712144249,-0.153571010716547,0.866017784402509));
#120477=DIRECTION('center_axis',(-0.503988379172001,0.163755751065515,0.848044673146732));
#120478=DIRECTION('ref_axis',(0.859649150669465,1.54206212768985E-15,0.510884857627692));
#120479=DIRECTION('center_axis',(-0.475533025685691,0.154510035618062,0.866022511471565));
#120480=DIRECTION('ref_axis',(-0.825011387615653,0.26335567262647,-0.499999999999955));
#120481=DIRECTION('center_axis',(0.475533035318008,-0.154510049384248,-0.866022503726387));
#120482=DIRECTION('ref_axis',(-0.87654878801251,1.1206608856956E-15,-0.481313018973931));
#120483=DIRECTION('center_axis',(-0.503988355688897,0.163755716844529,0.848044693710618));
#120484=DIRECTION('ref_axis',(-0.807930997359887,0.257746148176091,-0.529919264233191));
#120485=DIRECTION('center_axis',(-0.50398831704056,0.163755730877767,0.848044713969324));
#120486=DIRECTION('ref_axis',(0.859649189130477,-3.08352198662565E-15,0.510884792910606));
#120487=DIRECTION('center_axis',(0.951056516295148,-0.309016994374964,-5.19628367180436E-14));
#120488=DIRECTION('ref_axis',(0.309016994374964,0.951056516295148,4.43497354731716E-28));
#120489=DIRECTION('center_axis',(-0.951056516295148,0.309016994374964,0.));
#120490=DIRECTION('ref_axis',(-0.309016994374964,-0.951056516295148,0.));
#120491=DIRECTION('center_axis',(0.951056516295153,-0.309016994374948,-1.33924836902177E-16));
#120492=DIRECTION('ref_axis',(0.309016994374948,0.951056516295153,2.18771486896698E-30));
#120493=DIRECTION('center_axis',(0.951056516295148,-0.309016994374964,1.68837491218278E-14));
#120494=DIRECTION('ref_axis',(0.309016994374964,0.951056516295148,-1.43380940262431E-28));
#120495=DIRECTION('center_axis',(0.951056516295153,-0.309016994374948,-1.33924836902177E-16));
#120496=DIRECTION('ref_axis',(0.309016994374948,0.951056516295153,2.18771486896698E-30));
#120497=DIRECTION('center_axis',(-0.823639804208726,0.267653025932271,-0.499979330205069));
#120498=DIRECTION('ref_axis',(0.475210466544137,-0.155418826431445,-0.866036951219506));
#120499=DIRECTION('center_axis',(0.475533164204417,-0.154510091261981,0.866022425483284));
#120500=DIRECTION('ref_axis',(0.876548714628833,4.04293055823746E-15,-0.481313152617442));
#120501=DIRECTION('center_axis',(0.475533172741623,-0.154510094035866,0.866022420300602));
#120502=DIRECTION('ref_axis',(-0.309016994371688,-0.951056516296213,-1.95818863719932E-12));
#120503=DIRECTION('center_axis',(-0.456777309666909,0.203370361061781,0.866022508723105));
#120504=DIRECTION('ref_axis',(0.406736643080227,0.91354545764063,2.76244469758968E-12));
#120505=DIRECTION('center_axis',(-0.791159233140786,0.352213899941099,0.500012436349702));
#120506=DIRECTION('ref_axis',(0.456381342218119,-0.204277427960925,0.866017784402178));
#120507=DIRECTION('center_axis',(0.456777317573273,-0.203370364581912,-0.86602250372631));
#120508=DIRECTION('ref_axis',(-0.884507036382098,5.88362210846088E-15,-0.466526850878444));
#120509=DIRECTION('center_axis',(0.913545457642594,-0.406736643075817,6.10247733350035E-14));
#120510=DIRECTION('ref_axis',(0.406736643075817,0.913545457642593,6.78980940604894E-28));
#120511=DIRECTION('center_axis',(-0.913545457642601,0.406736643075801,1.28642645648559E-16));
#120512=DIRECTION('ref_axis',(-0.406736643075801,-0.9135454576426,-7.47472011570615E-33));
#120513=DIRECTION('center_axis',(-0.913545457642598,0.406736643075807,0.));
#120514=DIRECTION('ref_axis',(-0.406736643075807,-0.913545457642598,0.));
#120515=DIRECTION('center_axis',(-0.913545457642601,0.406736643075801,1.28642645648559E-16));
#120516=DIRECTION('ref_axis',(-0.406736643075801,-0.9135454576426,-7.47472011570615E-33));
#120517=DIRECTION('center_axis',(0.913545457642594,-0.406736643075817,0.));
#120518=DIRECTION('ref_axis',(0.406736643075817,0.913545457642593,0.));
#120519=DIRECTION('center_axis',(-0.48410985792377,0.215539595588306,-0.848045003637576));
#120520=DIRECTION('ref_axis',(-0.868458021515995,5.72874239606451E-16,0.495762710240013));
#120521=DIRECTION('center_axis',(0.456777441376059,-0.203370419702482,0.8660224254833));
#120522=DIRECTION('ref_axis',(0.884506966812066,3.90936356972174E-15,-0.466526982779044));
#120523=DIRECTION('center_axis',(0.48410982330659,-0.215539603856382,0.848045021297511));
#120524=DIRECTION('ref_axis',(0.77296765014953,-0.348864709044782,-0.52991926423316));
#120525=DIRECTION('center_axis',(-0.484109806651296,0.21553957276033,-0.84804503870864));
#120526=DIRECTION('ref_axis',(-0.868458052949953,-3.34246373676304E-15,
0.495762655175213));
#120527=DIRECTION('center_axis',(0.456777449752137,-0.20337043494584,0.866022417485756));
#120528=DIRECTION('ref_axis',(0.789292595943427,-0.356394722167529,-0.500000000000016));
#120529=DIRECTION('center_axis',(0.791178490090755,-0.352217640366503,0.499979330205125));
#120530=DIRECTION('ref_axis',(0.457145692791346,-0.202479170989976,-0.86603695121948));
#120531=DIRECTION('center_axis',(-0.406958162070229,-0.913446798847323,
0.));
#120532=DIRECTION('ref_axis',(0.913446798847323,-0.406958162070229,0.));
#120533=DIRECTION('center_axis',(-0.913545457642601,0.406736643075801,1.28642645648559E-16));
#120534=DIRECTION('ref_axis',(-0.406736643075801,-0.9135454576426,-7.47472011570615E-33));
#120535=DIRECTION('center_axis',(0.913545457642598,-0.406736643075807,0.));
#120536=DIRECTION('ref_axis',(0.406736643075807,0.913545457642598,0.));
#120537=DIRECTION('center_axis',(-1.21742612413517E-17,-5.72753959967198E-17,
-1.));
#120538=DIRECTION('ref_axis',(0.,1.,-1.12832121675104E-16));
#120539=DIRECTION('center_axis',(-0.406515100163544,-0.913644062717546,
0.));
#120540=DIRECTION('ref_axis',(0.913644062717546,-0.406515100163544,0.));
#120541=DIRECTION('center_axis',(0.48411028140672,-0.215539784135064,-0.848044713969326));
#120542=DIRECTION('ref_axis',(-0.868457761888285,1.62534225110956E-15,-0.495763165045559));
#120543=DIRECTION('center_axis',(0.484109806651295,-0.21553957276033,0.848045038708641));
#120544=DIRECTION('ref_axis',(0.868458052949953,2.8886639606392E-15,-0.495762655175212));
#120545=DIRECTION('center_axis',(0.484110321455164,-0.215539774370365,-0.848044693589288));
#120546=DIRECTION('ref_axis',(-0.772875576449771,0.349068641848483,-0.529919264233232));
#120547=DIRECTION('center_axis',(0.484110341087615,-0.215539810706674,-0.848044673146742));
#120548=DIRECTION('ref_axis',(-0.868457725299268,3.55645384105659E-15,-0.495763229140706));
#120549=DIRECTION('center_axis',(-0.484109823426766,0.21553960397576,-0.848045021198567));
#120550=DIRECTION('ref_axis',(0.776473315751262,-0.340990855186454,-0.529919264233196));
#120551=DIRECTION('center_axis',(0.484109857923801,-0.21553959558832,0.848045003637555));
#120552=DIRECTION('ref_axis',(0.868458021515976,-2.41205393455667E-15,-0.495762710240047));
#120553=DIRECTION('center_axis',(-0.406972488803041,-0.913440415876952,
0.));
#120554=DIRECTION('ref_axis',(0.913440415876952,-0.406972488803041,0.));
#120555=DIRECTION('center_axis',(0.913545457642598,-0.406736643075807,0.));
#120556=DIRECTION('ref_axis',(0.406736643075807,0.913545457642598,0.));
#120557=DIRECTION('center_axis',(-1.21742612413517E-17,-5.72753959967198E-17,
-1.));
#120558=DIRECTION('ref_axis',(0.,1.,0.));
#120559=DIRECTION('center_axis',(-0.406500770236728,-0.913650438514067,
2.49595411736509E-14));
#120560=DIRECTION('ref_axis',(0.913650438514067,-0.406500770236727,-1.61030417725217E-28));
#120561=DIRECTION('center_axis',(0.913545457642601,-0.406736643075801,-1.28642645648559E-16));
#120562=DIRECTION('ref_axis',(0.406736643075801,0.913545457642601,7.9109897830696E-31));
#120563=DIRECTION('center_axis',(0.791134794601138,-0.352268789800911,-0.500012436348953));
#120564=DIRECTION('ref_axis',(0.457186437804586,-0.202469153665354,0.8660177844026));
#120565=DIRECTION('center_axis',(-0.484110341087606,0.215539810706706,0.848044673146739));
#120566=DIRECTION('ref_axis',(0.868457725299272,-5.00491300951417E-15,0.495763229140701));
#120567=DIRECTION('center_axis',(-0.456777309432038,0.203370349885425,0.86602251147156));
#120568=DIRECTION('ref_axis',(-0.792963725161865,0.348150155216779,-0.499999999999951));
#120569=DIRECTION('center_axis',(0.456777317573163,-0.203370364581863,-0.866022503726379));
#120570=DIRECTION('ref_axis',(-0.88450703638216,-1.63558781625489E-15,-0.466526850878326));
#120571=DIRECTION('center_axis',(-0.484110321307456,0.215539774224879,0.848044693710585));
#120572=DIRECTION('ref_axis',(-0.776563258031751,0.340785973404991,-0.529919264233265));
#120573=DIRECTION('center_axis',(-0.484110281406723,0.215539784135065,0.848044713969325));
#120574=DIRECTION('ref_axis',(0.868457761888284,-9.9277303974391E-16,0.495763165045561));
#120575=DIRECTION('center_axis',(0.913545457642598,-0.406736643075807,0.));
#120576=DIRECTION('ref_axis',(0.406736643075807,0.913545457642598,0.));
#120577=DIRECTION('center_axis',(-0.913545457642598,0.406736643075807,0.));
#120578=DIRECTION('ref_axis',(-0.406736643075807,-0.913545457642598,0.));
#120579=DIRECTION('center_axis',(0.913545457642601,-0.406736643075801,-1.28642645648559E-16));
#120580=DIRECTION('ref_axis',(0.406736643075801,0.913545457642601,7.9109897830696E-31));
#120581=DIRECTION('center_axis',(0.913545457642598,-0.406736643075807,2.22228536467272E-14));
#120582=DIRECTION('ref_axis',(0.406736643075807,0.913545457642598,3.85652098937002E-31));
#120583=DIRECTION('center_axis',(0.913545457642601,-0.406736643075801,-1.28642645648559E-16));
#120584=DIRECTION('ref_axis',(0.406736643075801,0.913545457642601,7.9109897830696E-31));
#120585=DIRECTION('center_axis',(-0.791150459692759,0.352280597670772,-0.499979330205419));
#120586=DIRECTION('ref_axis',(0.456361522793348,-0.204240445643174,-0.866036951219296));
#120587=DIRECTION('center_axis',(0.456777441376069,-0.203370419702468,0.866022425483298));
#120588=DIRECTION('ref_axis',(0.884506966812062,6.03592299906791E-15,-0.466526982779053));
#120589=DIRECTION('center_axis',(0.456777449576405,-0.203370423353496,0.866022420300707));
#120590=DIRECTION('ref_axis',(-0.406736643068955,-0.913545457645649,-4.33598912519089E-12));
#120591=DIRECTION('center_axis',(-0.433017044461004,0.250002507183264,0.866022508719224));
#120592=DIRECTION('ref_axis',(0.499999999999256,0.866025403784868,-4.89547161594789E-13));
#120593=DIRECTION('center_axis',(-0.750008802378745,0.4329830941858,0.500012436349029));
#120594=DIRECTION('ref_axis',(0.432528431855697,-0.250863215188869,0.866017784402581));
#120595=DIRECTION('center_axis',(0.433017051950287,-0.250002511507195,-0.866022503726305));
#120596=DIRECTION('ref_axis',(-0.894424794863779,-2.9162281599034E-15,-0.447218387740136));
#120597=DIRECTION('center_axis',(0.86602540378444,-0.499999999999998,-6.09762352041363E-14));
#120598=DIRECTION('ref_axis',(0.499999999999998,0.86602540378444,8.28350179725319E-28));
#120599=DIRECTION('center_axis',(-0.866025403784438,0.500000000000001,1.2195101864901E-16));
#120600=DIRECTION('ref_axis',(-0.500000000000001,-0.866025403784438,6.92065314020432E-33));
#120601=DIRECTION('center_axis',(-0.866025403784433,0.50000000000001,0.));
#120602=DIRECTION('ref_axis',(-0.50000000000001,-0.866025403784433,0.));
#120603=DIRECTION('center_axis',(-0.866025403784438,0.500000000000001,1.2195101864901E-16));
#120604=DIRECTION('ref_axis',(-0.500000000000001,-0.866025403784438,6.92065314020432E-33));
#120605=DIRECTION('center_axis',(0.86602540378444,-0.499999999999998,0.));
#120606=DIRECTION('ref_axis',(0.499999999999998,0.86602540378444,0.));
#120607=DIRECTION('center_axis',(-0.458927830768609,0.264962106632866,-0.848045003637597));
#120608=DIRECTION('ref_axis',(-0.879478602053342,2.04159790904447E-15,0.475938429348062));
#120609=DIRECTION('center_axis',(0.433017169313211,-0.250002579266684,0.866022425483301));
#120610=DIRECTION('ref_axis',(0.894424730216421,1.52776146092203E-15,-0.447218517033097));
#120611=DIRECTION('center_axis',(0.458927795478264,-0.264962111234757,0.848045021297502));
#120612=DIRECTION('ref_axis',(0.7322669605685,-0.427750712277967,-0.529919264233206));
#120613=DIRECTION('center_axis',(-0.45892778216322,0.264962078570532,-0.848045038708636));
#120614=DIRECTION('ref_axis',(-0.879478631391242,-3.91934596708905E-15,
0.475938375135046));
#120615=DIRECTION('center_axis',(0.433017176052958,-0.250002595297057,0.866022417485747));
#120616=DIRECTION('ref_axis',(0.747715375894778,-0.436945896708641,-0.500000000000013));
#120617=DIRECTION('center_axis',(0.750027562856299,-0.432988827019191,0.499979330205145));
#120618=DIRECTION('ref_axis',(0.433476564275525,-0.249154705647712,-0.866036951219455));
#120619=DIRECTION('center_axis',(-0.500209992837911,-0.865904130412309,
0.));
#120620=DIRECTION('ref_axis',(0.865904130412309,-0.500209992837911,0.));
#120621=DIRECTION('center_axis',(-0.866025403784438,0.500000000000001,1.2195101864901E-16));
#120622=DIRECTION('ref_axis',(-0.500000000000001,-0.866025403784438,6.92065314020432E-33));
#120623=DIRECTION('center_axis',(0.866025403784433,-0.50000000000001,0.));
#120624=DIRECTION('ref_axis',(0.50000000000001,0.866025403784433,0.));
#120625=DIRECTION('center_axis',(-1.88658882409001E-17,-7.04084534449554E-17,
-1.));
#120626=DIRECTION('ref_axis',(0.,1.,-1.12832121675104E-16));
#120627=DIRECTION('center_axis',(-0.499789977759974,-0.86614662623062,0.));
#120628=DIRECTION('ref_axis',(0.86614662623062,-0.499789977759974,0.));
#120629=DIRECTION('center_axis',(0.458928232223209,-0.264962338412804,-0.848044713969316));
#120630=DIRECTION('ref_axis',(-0.879478359737741,-7.92594685885185E-17,
-0.475938877118704));
#120631=DIRECTION('center_axis',(0.458927782163206,-0.264962078570532,0.848045038708643));
#120632=DIRECTION('ref_axis',(0.879478631391249,-1.80847170028479E-16,-0.475938375135033));
#120633=DIRECTION('center_axis',(0.45892827307444,-0.264962332885194,-0.848044693589287));
#120634=DIRECTION('ref_axis',(-0.732154074464041,0.427943903613827,-0.529919264233207));
#120635=DIRECTION('center_axis',(0.458928288799672,-0.264962371077207,-0.848044673146733));
#120636=DIRECTION('ref_axis',(-0.879478325588501,4.31424957953392E-16,-0.475938940222427));
#120637=DIRECTION('center_axis',(-0.458927795586795,0.264962111363442,-0.848045021198564));
#120638=DIRECTION('ref_axis',(0.736576463604698,-0.420286434063858,-0.529919264233226));
#120639=DIRECTION('center_axis',(0.458927830768629,-0.264962106632886,0.848045003637581));
#120640=DIRECTION('ref_axis',(0.87947860205333,4.54286346810456E-15,-0.475938429348083));
#120641=DIRECTION('center_axis',(-0.500223573885338,-0.86589628485713,2.36549702850838E-14));
#120642=DIRECTION('ref_axis',(0.86589628485713,-0.500223573885338,2.17560721291705E-28));
#120643=DIRECTION('center_axis',(0.866025403784433,-0.50000000000001,0.));
#120644=DIRECTION('ref_axis',(0.50000000000001,0.866025403784433,0.));
#120645=DIRECTION('center_axis',(-1.88658882409001E-17,-7.04084534449554E-17,
-1.));
#120646=DIRECTION('ref_axis',(0.,1.,-1.20114286872534E-16));
#120647=DIRECTION('center_axis',(-0.499776392786186,-0.866154464985102,
-2.36620233737285E-14));
#120648=DIRECTION('ref_axis',(0.866154464985102,-0.499776392786186,2.10998669647211E-28));
#120649=DIRECTION('center_axis',(0.866025403784438,-0.500000000000001,-1.2195101864901E-16));
#120650=DIRECTION('ref_axis',(0.500000000000001,0.866025403784438,1.24416343873374E-30));
#120651=DIRECTION('center_axis',(0.749978760163569,-0.433035128829407,-0.500012436348552));
#120652=DIRECTION('ref_axis',(-0.433518133149823,0.249149002262184,-0.866017784402867));
#120653=DIRECTION('center_axis',(-0.458928288799668,0.264962371077193,0.84804467314674));
#120654=DIRECTION('ref_axis',(0.879478325588503,-1.89639858451521E-15,0.475938940222423));
#120655=DIRECTION('center_axis',(-0.433017045389765,0.250002496040436,0.866022511471538));
#120656=DIRECTION('ref_axis',(-0.752228186192807,0.429130231860971,-0.500000000000028));
#120657=DIRECTION('center_axis',(0.433017051950197,-0.250002511507151,-0.866022503726362));
#120658=DIRECTION('ref_axis',(-0.894424794863829,-5.98165056151269E-15,
-0.447218387740037));
#120659=DIRECTION('center_axis',(-0.458928272943999,0.264962332722854,0.848044693710598));
#120660=DIRECTION('ref_axis',(-0.736687329156677,0.420092076162478,-0.529919264233242));
#120661=DIRECTION('center_axis',(-0.458928232223181,0.264962338412833,0.848044713969322));
#120662=DIRECTION('ref_axis',(0.879478359737755,5.09289574828741E-15,0.475938877118678));
#120663=DIRECTION('center_axis',(0.866025403784433,-0.50000000000001,-1.36592399683214E-14));
#120664=DIRECTION('ref_axis',(0.50000000000001,0.866025403784433,-1.33215113601878E-31));
#120665=DIRECTION('center_axis',(-0.866025403784433,0.50000000000001,0.));
#120666=DIRECTION('ref_axis',(-0.50000000000001,-0.866025403784433,0.));
#120667=DIRECTION('center_axis',(0.866025403784438,-0.500000000000001,-1.2195101864901E-16));
#120668=DIRECTION('ref_axis',(0.500000000000001,0.866025403784438,1.24416343873374E-30));
#120669=DIRECTION('center_axis',(0.866025403784433,-0.50000000000001,0.));
#120670=DIRECTION('ref_axis',(0.50000000000001,0.866025403784433,0.));
#120671=DIRECTION('center_axis',(0.866025403784438,-0.500000000000001,-1.2195101864901E-16));
#120672=DIRECTION('ref_axis',(0.500000000000001,0.866025403784438,1.24416343873374E-30));
#120673=DIRECTION('center_axis',(-0.749993105181574,0.433048509462462,-0.4999793302052));
#120674=DIRECTION('ref_axis',(-0.432512586708856,0.250824363770665,0.866036951219436));
#120675=DIRECTION('center_axis',(0.433017169313192,-0.250002579266708,0.866022425483304));
#120676=DIRECTION('ref_axis',(0.894424730216429,-3.15083324732399E-15,-0.44721851703308));
#120677=DIRECTION('center_axis',(0.433017177087157,-0.250002583755012,0.866022420300588));
#120678=DIRECTION('ref_axis',(-0.499999999997495,-0.866025403785885,-1.67844740331651E-12));
#120679=DIRECTION('center_axis',(-0.404512553894058,0.293895573516091,0.866022508720042));
#120680=DIRECTION('ref_axis',(0.58778525229198,0.809016994375305,-3.49676543998341E-13));
#120681=DIRECTION('center_axis',(-0.700641118228541,0.509008435041967,0.500012436348926));
#120682=DIRECTION('ref_axis',(0.403936649474811,-0.294700492550331,0.866017784402639));
#120683=DIRECTION('center_axis',(0.404512560891457,-0.293895578600019,-0.866022503726315));
#120684=DIRECTION('ref_axis',(-0.906035256115487,-3.15407140147818E-15,
-0.423202214875754));
#120685=DIRECTION('center_axis',(0.809016994374931,-0.587785252292496,0.));
#120686=DIRECTION('ref_axis',(0.587785252292496,0.809016994374931,0.));
#120687=DIRECTION('center_axis',(-0.809016994374947,0.587785252292474,1.13923270769252E-16));
#120688=DIRECTION('ref_axis',(-0.587785252292474,-0.809016994374947,8.80720662300256E-33));
#120689=DIRECTION('center_axis',(-0.809016994374931,0.587785252292496,-3.21147992436134E-14));
#120690=DIRECTION('ref_axis',(-0.587785252292496,-0.809016994374931,2.25632648858384E-30));
#120691=DIRECTION('center_axis',(-0.809016994374947,0.587785252292474,1.13923270769252E-16));
#120692=DIRECTION('ref_axis',(-0.587785252292474,-0.809016994374947,8.80720662300256E-33));
#120693=DIRECTION('center_axis',(0.80901699437495,-0.58778525229247,0.));
#120694=DIRECTION('ref_axis',(0.58778525229247,0.80901699437495,0.));
#120695=DIRECTION('center_axis',(-0.428717694262756,0.311481637390311,-0.848045003637588));
#120696=DIRECTION('ref_axis',(-0.892442058026273,-6.51151864539323E-15,
0.451162025292277));
#120697=DIRECTION('center_axis',(0.404512670528671,-0.293895658256118,0.866022425483293));
#120698=DIRECTION('ref_axis',(0.906035197473499,1.81134782246753E-15,-0.423202340422589));
#120699=DIRECTION('center_axis',(0.428717658681014,-0.311481638283158,0.848045021297519));
#120700=DIRECTION('ref_axis',(0.683543400918347,-0.501950189217554,-0.529919264233186));
#120701=DIRECTION('center_axis',(-0.428717648856913,0.311481604401034,-0.848045038708652));
#120702=DIRECTION('ref_axis',(-0.89244208477774,-4.94272061273143E-15,0.451161972375288));
#120703=DIRECTION('center_axis',(0.404512675553166,-0.293895674906847,0.866022417485753));
#120704=DIRECTION('ref_axis',(0.69794602971643,-0.512709800572455,-0.500000000000025));
#120705=DIRECTION('center_axis',(0.700659176689928,-0.509016097474107,0.499979330205182));
#120706=DIRECTION('ref_axis',(0.405058175792842,-0.29310044924206,-0.866036951219449));
#120707=DIRECTION('center_axis',(-0.587981418248406,-0.808874435122407,
7.63199572093835E-14));
#120708=DIRECTION('ref_axis',(0.808874435122407,-0.587981418248406,4.48144986036732E-28));
#120709=DIRECTION('center_axis',(-0.809016994374947,0.587785252292474,1.13923270769252E-16));
#120710=DIRECTION('ref_axis',(-0.587785252292474,-0.809016994374947,8.80720662300256E-33));
#120711=DIRECTION('center_axis',(0.809016994374969,-0.587785252292444,0.));
#120712=DIRECTION('ref_axis',(0.587785252292444,0.809016994374969,0.));
#120713=DIRECTION('center_axis',(-2.68936361206584E-17,-8.27701011433319E-17,
-1.));
#120714=DIRECTION('ref_axis',(0.,1.,-1.12832121675104E-16));
#120715=DIRECTION('center_axis',(-0.587589051772239,-0.809159506053906,
0.));
#120716=DIRECTION('ref_axis',(0.809159506053906,-0.587589051772239,0.));
#120717=DIRECTION('center_axis',(0.428718069290544,-0.311481909863919,-0.848044713969325));
#120718=DIRECTION('ref_axis',(-0.892441837073393,5.69339720065885E-15,-0.451162462358149));
#120719=DIRECTION('center_axis',(0.428717648856975,-0.311481604401136,0.848045038708583));
#120720=DIRECTION('ref_axis',(0.892442084777698,-4.42555422208939E-15,-0.451161972375372));
#120721=DIRECTION('center_axis',(0.428718110495911,-0.311481908636537,-0.848044693589292));
#120722=DIRECTION('ref_axis',(-0.683410939222547,0.502130522419756,-0.529919264233165));
#120723=DIRECTION('center_axis',(0.428718122142701,-0.311481948263287,-0.848044673146729));
#120724=DIRECTION('ref_axis',(-0.892441805934776,-6.12251068898412E-15,
-0.45116252395326));
#120725=DIRECTION('center_axis',(-0.428717658775709,0.311481638422204,-0.848045021198577));
#120726=DIRECTION('ref_axis',(0.688609525574901,-0.494977266833597,-0.529919264233195));
#120727=DIRECTION('center_axis',(0.428717694262811,-0.31148163739035,0.848045003637546));
#120728=DIRECTION('ref_axis',(0.892442058026239,-8.51765461603545E-15,-0.451162025292345));
#120729=DIRECTION('center_axis',(-0.587994104813606,-0.808865212939984,
0.));
#120730=DIRECTION('ref_axis',(0.808865212939984,-0.587994104813606,0.));
#120731=DIRECTION('center_axis',(0.809016994374931,-0.587785252292496,-7.63170283020858E-14));
#120732=DIRECTION('ref_axis',(0.587785252292496,0.809016994374931,-5.02862541378261E-30));
#120733=DIRECTION('center_axis',(-2.68936361206584E-17,-8.27701011433319E-17,
-1.));
#120734=DIRECTION('ref_axis',(0.,1.,-1.20114286872534E-16));
#120735=DIRECTION('center_axis',(-0.587576360591353,-0.80916872188328,-3.21033860361202E-14));
#120736=DIRECTION('ref_axis',(0.80916872188328,-0.587576360591353,4.80687827587565E-28));
#120737=DIRECTION('center_axis',(0.809016994374947,-0.587785252292474,-1.13923270769252E-16));
#120738=DIRECTION('ref_axis',(0.587785252292474,0.809016994374947,1.19410145339382E-30));
#120739=DIRECTION('center_axis',(0.700605801486325,-0.509057044367352,-0.500012436349018));
#120740=DIRECTION('ref_axis',(-0.40510011313772,0.293099122199729,-0.866017784402581));
#120741=DIRECTION('center_axis',(-0.428718122142726,0.311481948263255,0.848044673146729));
#120742=DIRECTION('ref_axis',(0.892441805934764,-1.37149456183714E-15,0.451162523953283));
#120743=DIRECTION('center_axis',(-0.404512555984775,0.293895562530571,0.866022511471558));
#120744=DIRECTION('ref_axis',(-0.703251077802595,0.505408667881258,-0.49999999999998));
#120745=DIRECTION('center_axis',(0.404512560891371,-0.293895578599957,-0.866022503726376));
#120746=DIRECTION('ref_axis',(-0.906035256115534,-6.84927325568381E-15,
-0.423202214875654));
#120747=DIRECTION('center_axis',(-0.428718110383012,0.311481908461646,0.848044693710603));
#120748=DIRECTION('ref_axis',(-0.688740099725524,0.494795562252288,-0.529919264233258));
#120749=DIRECTION('center_axis',(-0.428718069290536,0.311481909863913,0.848044713969331));
#120750=DIRECTION('ref_axis',(0.892441837073398,-1.59472440562988E-15,0.451162462358138));
#120751=DIRECTION('center_axis',(0.809016994374931,-0.587785252292496,0.));
#120752=DIRECTION('ref_axis',(0.587785252292496,0.809016994374931,0.));
#120753=DIRECTION('center_axis',(-0.80901699437495,0.58778525229247,0.));
#120754=DIRECTION('ref_axis',(-0.58778525229247,-0.80901699437495,0.));
#120755=DIRECTION('center_axis',(0.809016994374947,-0.587785252292474,-1.13923270769252E-16));
#120756=DIRECTION('ref_axis',(0.587785252292474,0.809016994374947,1.19410145339382E-30));
#120757=DIRECTION('center_axis',(0.809016994374931,-0.587785252292496,-4.42022290584682E-14));
#120758=DIRECTION('ref_axis',(0.587785252292496,0.809016994374931,4.35974171970421E-30));
#120759=DIRECTION('center_axis',(0.809016994374947,-0.587785252292474,-1.13923270769252E-16));
#120760=DIRECTION('ref_axis',(0.587785252292474,0.809016994374947,1.19410145339382E-30));
#120761=DIRECTION('center_axis',(-0.700618669263857,0.509071851162881,-0.4999793302053));
#120762=DIRECTION('ref_axis',(-0.403924952204904,0.29466019770054,0.866036951219372));
#120763=DIRECTION('center_axis',(0.404512670528677,-0.293895658256122,0.866022425483289));
#120764=DIRECTION('ref_axis',(0.906035197473497,3.93346248258234E-15,-0.423202340422595));
#120765=DIRECTION('center_axis',(0.404512677786642,-0.293895663529335,0.866022420303616));
#120766=DIRECTION('ref_axis',(-0.58778525229999,-0.809016994369486,5.3500510981539E-12));
#120767=DIRECTION('center_axis',(-0.371576139133635,0.334568658440529,0.866022508723559));
#120768=DIRECTION('ref_axis',(0.669130606356872,0.743144825479183,-1.53857679357235E-12));
#120769=DIRECTION('center_axis',(-0.643597063369161,0.57945697296553,0.500012436349555));
#120770=DIRECTION('ref_axis',(0.370919252615107,-0.33530896966599,0.86601778440225));
#120771=DIRECTION('center_axis',(0.371576145565852,-0.334568664232084,-0.866022503726309));
#120772=DIRECTION('ref_axis',(-0.918982183096513,-7.2095623261364E-15,-0.394299058014557));
#120773=DIRECTION('center_axis',(0.743144825477406,-0.669130606358845,-7.71624360992626E-14));
#120774=DIRECTION('ref_axis',(0.669130606358845,0.743144825477406,4.74868592476285E-30));
#120775=DIRECTION('center_axis',(-0.743144825477393,0.669130606358859,1.04647355694969E-16));
#120776=DIRECTION('ref_axis',(-0.669130606358859,-0.743144825477393,1.70053300922835E-32));
#120777=DIRECTION('center_axis',(-0.743144825477406,0.669130606358845,0.));
#120778=DIRECTION('ref_axis',(-0.669130606358845,-0.743144825477406,0.));
#120779=DIRECTION('center_axis',(-0.743144825477393,0.669130606358859,1.04647355694969E-16));
#120780=DIRECTION('ref_axis',(-0.669130606358859,-0.743144825477393,1.70053300922835E-32));
#120781=DIRECTION('center_axis',(0.743144825477382,-0.669130606358872,0.));
#120782=DIRECTION('ref_axis',(0.669130606358872,0.743144825477382,0.));
#120783=DIRECTION('center_axis',(-0.393810436983632,0.354588510146749,-0.848045003637584));
#120784=DIRECTION('ref_axis',(-0.906978223357768,-5.83873457091855E-16,
0.421177518814558));
#120785=DIRECTION('center_axis',(0.371576246276125,-0.334568754912021,0.866022425483293));
#120786=DIRECTION('ref_axis',(0.918982131463643,6.34168247799913E-15,-0.394299178353873));
#120787=DIRECTION('center_axis',(0.393810401508524,-0.354588507309826,0.848045021297504));
#120788=DIRECTION('ref_axis',(0.627330796737913,-0.570650194829292,-0.52991926423321));
#120789=DIRECTION('center_axis',(-0.393810395274862,0.354588472592004,-0.848045038708633));
#120790=DIRECTION('ref_axis',(-0.906978247051285,1.62635303421704E-15,0.421177467792116));
#120791=DIRECTION('center_axis',(0.37157624953938,-0.334568771989208,0.866022417485761));
#120792=DIRECTION('ref_axis',(0.640529840782192,-0.582856348569324,-0.499999999999975));
#120793=DIRECTION('center_axis',(0.643614221961268,-0.579466481046713,0.499979330205291));
#120794=DIRECTION('ref_axis',(0.372201885200888,-0.333834922941829,-0.866036951219362));
#120795=DIRECTION('center_axis',(-0.669310796197597,-0.742982542253409,
0.));
#120796=DIRECTION('ref_axis',(0.742982542253409,-0.669310796197597,0.));
#120797=DIRECTION('center_axis',(-0.743144825477393,0.669130606358859,1.04647355694969E-16));
#120798=DIRECTION('ref_axis',(-0.669130606358859,-0.743144825477393,1.70053300922835E-32));
#120799=DIRECTION('center_axis',(0.743144825477382,-0.669130606358872,0.));
#120800=DIRECTION('ref_axis',(0.669130606358872,0.743144825477382,0.));
#120801=DIRECTION('center_axis',(-3.61695511949416E-17,-9.42249022928248E-17,
-1.));
#120802=DIRECTION('ref_axis',(0.,1.,-1.12832121675104E-16));
#120803=DIRECTION('center_axis',(-0.668950377172406,-0.743307065001333,
0.));
#120804=DIRECTION('ref_axis',(0.743307065001333,-0.668950377172406,0.));
#120805=DIRECTION('center_axis',(0.393810781475684,-0.35458882032882,-0.848044713969332));
#120806=DIRECTION('ref_axis',(-0.906978027661852,2.89845252510014E-15,-0.421177940232649));
#120807=DIRECTION('center_axis',(0.39381039527486,-0.354588472592002,0.848045038708635));
#120808=DIRECTION('ref_axis',(0.906978247051286,-2.65749036098971E-15,-0.421177467792113));
#120809=DIRECTION('center_axis',(0.393810822586016,-0.354588823412691,-0.848044693589276));
#120810=DIRECTION('ref_axis',(-0.627180210717368,0.570815694142259,-0.529919264233156));
#120811=DIRECTION('center_axis',(0.393810830024562,-0.354588864042303,-0.848044673146736));
#120812=DIRECTION('ref_axis',(-0.906978000082633,-7.8483346287888E-15,-0.421177999622614));
#120813=DIRECTION('center_axis',(-0.393810401582675,0.354588507464094,-0.848045021198567));
#120814=DIRECTION('ref_axis',(0.633098037491572,-0.564245025072303,-0.529919264233219));
#120815=DIRECTION('center_axis',(0.393810436983644,-0.35458851014676,0.848045003637574));
#120816=DIRECTION('ref_axis',(0.90697822335776,-1.35612861251301E-15,-0.421177518814574));
#120817=DIRECTION('center_axis',(-0.6693224492839,-0.74297204448391,3.65697438038149E-14));
#120818=DIRECTION('ref_axis',(0.74297204448391,-0.6693224492839,5.21231353425566E-29));
#120819=DIRECTION('center_axis',(0.743144825477406,-0.669130606358845,3.65592620896166E-14));
#120820=DIRECTION('ref_axis',(0.669130606358845,0.743144825477406,-1.6162287319392E-30));
#120821=DIRECTION('center_axis',(-3.61695511949416E-17,-9.42249022928248E-17,
-1.));
#120822=DIRECTION('ref_axis',(0.,1.,-1.20114286872534E-16));
#120823=DIRECTION('center_axis',(-0.668938718831589,-0.743317556935091,
0.));
#120824=DIRECTION('ref_axis',(0.743317556935091,-0.668938718831589,0.));
#120825=DIRECTION('center_axis',(0.743144825477393,-0.669130606358859,-1.04647355694969E-16));
#120826=DIRECTION('ref_axis',(0.669130606358859,0.743144825477393,-1.0963218983187E-31));
#120827=DIRECTION('center_axis',(0.643556859035248,-0.579501624401408,-0.500012436350153));
#120828=DIRECTION('ref_axis',(-0.372243731481368,0.333837986862428,-0.866017784401954));
#120829=DIRECTION('center_axis',(-0.393810830024468,0.354588864042396,0.848044673146741));
#120830=DIRECTION('ref_axis',(0.90697800008267,-6.46020788503429E-15,0.421177999622535));
#120831=DIRECTION('center_axis',(-0.371576142362482,0.33456864774147,0.866022511471533));
#120832=DIRECTION('ref_axis',(-0.646569003441366,0.576149740769561,-0.500000000000006));
#120833=DIRECTION('center_axis',(0.371576145565767,-0.334568664232008,-0.866022503726374));
#120834=DIRECTION('ref_axis',(-0.918982183096555,4.84816140359523E-15,-0.39429905801446));
#120835=DIRECTION('center_axis',(-0.3938108224892,0.354588823230052,0.848044693710601));
#120836=DIRECTION('ref_axis',(-0.633246889647289,0.564077964599343,-0.529919264233238));
#120837=DIRECTION('center_axis',(-0.393810781475669,0.354588820328864,0.848044713969321));
#120838=DIRECTION('ref_axis',(0.906978027661855,-6.11429089785958E-15,0.421177940232642));
#120839=DIRECTION('center_axis',(0.743144825477406,-0.669130606358845,3.65592620896146E-14));
#120840=DIRECTION('ref_axis',(0.669130606358845,0.743144825477406,1.03271697859918E-30));
#120841=DIRECTION('center_axis',(-0.743144825477406,0.669130606358845,0.));
#120842=DIRECTION('ref_axis',(-0.669130606358845,-0.743144825477406,0.));
#120843=DIRECTION('center_axis',(0.743144825477393,-0.669130606358859,-1.04647355694969E-16));
#120844=DIRECTION('ref_axis',(0.669130606358859,0.743144825477393,-1.0963218983187E-31));
#120845=DIRECTION('center_axis',(0.743144825477406,-0.669130606358845,4.06031740096457E-14));
#120846=DIRECTION('ref_axis',(0.669130606358845,0.743144825477406,2.80523855531594E-30));
#120847=DIRECTION('center_axis',(0.743144825477393,-0.669130606358859,-1.04647355694969E-16));
#120848=DIRECTION('ref_axis',(0.669130606358859,0.743144825477393,-1.0963218983187E-31));
#120849=DIRECTION('center_axis',(-0.643568108591829,0.579517695132094,-0.499979330205082));
#120850=DIRECTION('ref_axis',(-0.3709118314048,0.335267672832272,0.866036951219502));
#120851=DIRECTION('center_axis',(0.371576246276117,-0.334568754912014,0.866022425483298));
#120852=DIRECTION('ref_axis',(0.918982131463646,3.28768502367003E-15,-0.394299178353865));
#120853=DIRECTION('center_axis',(0.371576252946115,-0.334568760917775,0.86602242030127));
#120854=DIRECTION('ref_axis',(-0.66913060635473,-0.743144825481112,-3.25199184387666E-12));
#120855=DIRECTION('center_axis',(-0.334568658443921,0.371576139137501,0.86602250872059));
#120856=DIRECTION('ref_axis',(0.743144825478317,0.669130606357834,7.34320742387398E-13));
#120857=DIRECTION('center_axis',(-0.579501624400846,0.643556859036295,0.500012436349456));
#120858=DIRECTION('ref_axis',(0.333837986833296,-0.372243731506635,0.866017784402323));
#120859=DIRECTION('center_axis',(0.334568664232049,-0.371576145565884,-0.866022503726308));
#120860=DIRECTION('ref_axis',(1.54577326889484E-15,0.9189821830965,-0.394299058014588));
#120861=DIRECTION('center_axis',(0.669130606358845,-0.743144825477406,0.));
#120862=DIRECTION('ref_axis',(0.743144825477406,0.669130606358845,0.));
#120863=DIRECTION('center_axis',(-0.669130606358857,0.743144825477395,9.42249022928245E-17));
#120864=DIRECTION('ref_axis',(-0.743144825477395,-0.669130606358857,-2.92763886583203E-33));
#120865=DIRECTION('center_axis',(-0.669130606358845,0.743144825477406,0.));
#120866=DIRECTION('ref_axis',(-0.743144825477406,-0.669130606358845,0.));
#120867=DIRECTION('center_axis',(-0.669130606358857,0.743144825477395,9.42249022928245E-17));
#120868=DIRECTION('ref_axis',(-0.743144825477395,-0.669130606358857,-2.92763886583203E-33));
#120869=DIRECTION('center_axis',(0.669130606358872,-0.743144825477382,0.));
#120870=DIRECTION('ref_axis',(0.743144825477382,0.669130606358872,0.));
#120871=DIRECTION('center_axis',(-0.354588510146771,0.393810436983657,-0.848045003637563));
#120872=DIRECTION('ref_axis',(4.10739333192291E-15,0.906978223357754,0.421177518814587));
#120873=DIRECTION('center_axis',(0.334568754912014,-0.371576246276117,0.866022425483298));
#120874=DIRECTION('ref_axis',(-3.2863782672971E-15,-0.918982131463647,-0.394299178353865));
#120875=DIRECTION('center_axis',(0.354588475166891,-0.393810430450173,0.848045021297495));
#120876=DIRECTION('ref_axis',(0.564245025068685,-0.633098037494793,-0.529919264233223));
#120877=DIRECTION('center_axis',(-0.354588472592013,0.393810395274872,-0.848045038708624));
#120878=DIRECTION('ref_axis',(2.79096370469408E-15,0.90697824705128,0.421177467792126));
#120879=DIRECTION('center_axis',(0.334568756368268,-0.371576263604501,0.866022417485777));
#120880=DIRECTION('ref_axis',(0.57609587287032,-0.646617000442945,-0.499999999999953));
#120881=DIRECTION('center_axis',(0.579517695132538,-0.643568108591555,0.499979330204919));
#120882=DIRECTION('ref_axis',(0.335267672837596,-0.370911831399782,-0.86603695121959));
#120883=DIRECTION('center_axis',(-0.743307065001336,-0.668950377172403,
0.));
#120884=DIRECTION('ref_axis',(0.668950377172402,-0.743307065001336,0.));
#120885=DIRECTION('center_axis',(-0.669130606358857,0.743144825477395,9.42249022928245E-17));
#120886=DIRECTION('ref_axis',(-0.743144825477395,-0.669130606358857,-2.92763886583203E-33));
#120887=DIRECTION('center_axis',(0.669130606358872,-0.743144825477382,0.));
#120888=DIRECTION('ref_axis',(0.743144825477382,0.669130606358872,0.));
#120889=DIRECTION('center_axis',(-4.6592004597086E-17,-1.04647355694969E-16,
-1.));
#120890=DIRECTION('ref_axis',(0.,1.,-1.12832121675104E-16));
#120891=DIRECTION('center_axis',(-0.742982542253406,-0.669310796197601,
0.));
#120892=DIRECTION('ref_axis',(0.669310796197601,-0.742982542253406,0.));
#120893=DIRECTION('center_axis',(0.354588820328813,-0.393810781475714,-0.848044713969321));
#120894=DIRECTION('ref_axis',(8.39746514209146E-15,0.906978027661839,-0.421177940232676));
#120895=DIRECTION('center_axis',(0.354588472591992,-0.393810395274849,0.848045038708644));
#120896=DIRECTION('ref_axis',(7.73991416207292E-15,-0.906978247051291,-0.421177467792101));
#120897=DIRECTION('center_axis',(0.354588860891521,-0.393810788839952,-0.848044693589264));
#120898=DIRECTION('ref_axis',(-0.564077964590164,0.633246889655487,-0.529919264233212));
#120899=DIRECTION('center_axis',(0.354588864042362,-0.393810830024499,-0.848044673146741));
#120900=DIRECTION('ref_axis',(3.45335519356911E-15,0.906978000082659,-0.421177999622559));
#120901=DIRECTION('center_axis',(-0.354588475218221,0.393810430617001,-0.848045021198562));
#120902=DIRECTION('ref_axis',(0.570650194826636,-0.627330796740326,-0.529919264233213));
#120903=DIRECTION('center_axis',(0.35458851014676,-0.393810436983644,0.848045003637574));
#120904=DIRECTION('ref_axis',(1.6043859838781E-15,-0.906978223357761,-0.421177518814573));
#120905=DIRECTION('center_axis',(-0.743317556935091,-0.668938718831589,
0.));
#120906=DIRECTION('ref_axis',(0.668938718831589,-0.743317556935091,0.));
#120907=DIRECTION('center_axis',(0.669130606358845,-0.743144825477406,0.));
#120908=DIRECTION('ref_axis',(0.743144825477406,0.669130606358845,0.));
#120909=DIRECTION('center_axis',(-4.6592004597086E-17,-1.04647355694969E-16,
-1.));
#120910=DIRECTION('ref_axis',(0.,1.,-1.20114286872534E-16));
#120911=DIRECTION('center_axis',(-0.742972044483927,-0.669322449283882,
4.02398997762828E-15));
#120912=DIRECTION('ref_axis',(0.669322449283881,-0.742972044483927,-6.6843319428275E-29));
#120913=DIRECTION('center_axis',(0.669130606358857,-0.743144825477395,-9.42249022928245E-17));
#120914=DIRECTION('ref_axis',(0.743144825477395,0.669130606358857,1.50824901715581E-30));
#120915=DIRECTION('center_axis',(0.579456972966088,-0.643597063368669,-0.500012436349541));
#120916=DIRECTION('ref_axis',(-0.335308969655252,0.370919252624765,-0.866017784402271));
#120917=DIRECTION('center_axis',(-0.354588864042302,0.393810830024563,0.848044673146736));
#120918=DIRECTION('ref_axis',(-8.30756835896895E-15,-0.906978000082633,
0.421177999622615));
#120919=DIRECTION('center_axis',(-0.334568662772257,0.371576128828625,0.866022511471565));
#120920=DIRECTION('ref_axis',(-0.582802983772218,0.640578396534151,-0.499999999999936));
#120921=DIRECTION('center_axis',(0.334568664232006,-0.371576145565766,-0.866022503726375));
#120922=DIRECTION('ref_axis',(-5.31150746435353E-15,0.918982183096555,-0.394299058014458));
#120923=DIRECTION('center_axis',(-0.354588860817823,0.393810788644961,0.848044693710628));
#120924=DIRECTION('ref_axis',(-0.570815694139697,0.627180210719711,-0.529919264233142));
#120925=DIRECTION('center_axis',(-0.354588820328737,0.39381078147576,0.848044713969332));
#120926=DIRECTION('ref_axis',(2.72603440059969E-15,-0.906978027661821,0.421177940232716));
#120927=DIRECTION('center_axis',(0.669130606358845,-0.743144825477406,-4.04391192003352E-15));
#120928=DIRECTION('ref_axis',(0.743144825477406,0.669130606358845,-2.84816967279441E-31));
#120929=DIRECTION('center_axis',(-0.669130606358875,0.743144825477379,0.));
#120930=DIRECTION('ref_axis',(-0.743144825477379,-0.669130606358875,0.));
#120931=DIRECTION('center_axis',(0.669130606358857,-0.743144825477395,-9.42249022928245E-17));
#120932=DIRECTION('ref_axis',(0.743144825477395,0.669130606358857,1.50824901715581E-30));
#120933=DIRECTION('center_axis',(0.669130606358845,-0.743144825477406,0.));
#120934=DIRECTION('ref_axis',(0.743144825477406,0.669130606358845,0.));
#120935=DIRECTION('center_axis',(0.669130606358857,-0.743144825477395,-9.42249022928245E-17));
#120936=DIRECTION('ref_axis',(0.743144825477395,0.669130606358857,1.50824901715581E-30));
#120937=DIRECTION('center_axis',(-0.579466481046794,0.643614221961154,-0.499979330205343));
#120938=DIRECTION('ref_axis',(-0.333834922953757,0.372201885190229,0.866036951219345));
#120939=DIRECTION('center_axis',(0.334568754912021,-0.371576246276125,0.866022425483293));
#120940=DIRECTION('ref_axis',(-6.32948812453082E-15,-0.918982131463643,
-0.394299178353873));
#120941=DIRECTION('center_axis',(0.334568760919757,-0.371576252948344,0.866022420299548));
#120942=DIRECTION('ref_axis',(-0.743144825478174,-0.669130606357993,6.99353084714793E-13));
#120943=DIRECTION('center_axis',(-0.293895573513778,0.404512553890826,0.866022508722336));
#120944=DIRECTION('ref_axis',(0.80901699437535,0.587785252291919,4.19611852796817E-13));
#120945=DIRECTION('center_axis',(-0.509057044367578,0.700605801486098,0.500012436349106));
#120946=DIRECTION('ref_axis',(0.293099122201432,-0.405100113136594,0.866017784402531));
#120947=DIRECTION('center_axis',(0.293895578600017,-0.40451256089147,-0.86602250372631));
#120948=DIRECTION('ref_axis',(6.99855896983189E-15,0.906035256115482,-0.423202214875765));
#120949=DIRECTION('center_axis',(0.587785252292434,-0.809016994374976,0.));
#120950=DIRECTION('ref_axis',(0.809016994374976,0.587785252292434,0.));
#120951=DIRECTION('center_axis',(-0.587785252292471,0.809016994374949,8.27701011433315E-17));
#120952=DIRECTION('ref_axis',(-0.809016994374949,-0.587785252292471,1.88536659549102E-32));
#120953=DIRECTION('center_axis',(-0.587785252292496,0.809016994374931,0.));
#120954=DIRECTION('ref_axis',(-0.809016994374931,-0.587785252292496,0.));
#120955=DIRECTION('center_axis',(-0.587785252292471,0.809016994374949,8.27701011433315E-17));
#120956=DIRECTION('ref_axis',(-0.809016994374949,-0.587785252292471,1.54176213488025E-33));
#120957=DIRECTION('center_axis',(0.58778525229247,-0.80901699437495,0.));
#120958=DIRECTION('ref_axis',(0.80901699437495,0.58778525229247,0.));
#120959=DIRECTION('center_axis',(-0.311481637390324,0.428717694262775,-0.848045003637574));
#120960=DIRECTION('ref_axis',(-8.00971604565638E-16,0.892442058026262,0.451162025292301));
#120961=DIRECTION('center_axis',(0.293895658256083,-0.404512670528688,0.866022425483297));
#120962=DIRECTION('ref_axis',(8.0628843439915E-15,-0.906035197473492,-0.423202340422605));
#120963=DIRECTION('center_axis',(0.311481603279599,-0.428717684112632,0.848045021297497));
#120964=DIRECTION('ref_axis',(0.494977266813993,-0.688609525588986,-0.529919264233205));
#120965=DIRECTION('center_axis',(-0.31148160440103,0.428717648856906,-0.848045038708657));
#120966=DIRECTION('ref_axis',(2.39813197791476E-15,0.892442084777744,0.451161972375281));
#120967=DIRECTION('center_axis',(0.293895657890439,-0.404512687916314,0.866022417485751));
#120968=DIRECTION('ref_axis',(0.505350078027568,-0.703293181139626,-0.500000000000036));
#120969=DIRECTION('center_axis',(0.509071851162742,-0.700618669263935,0.499979330205332));
#120970=DIRECTION('ref_axis',(0.294660197708544,-0.403924952199123,-0.866036951219345));
#120971=DIRECTION('center_axis',(-0.809159506053914,-0.587589051772227,
0.));
#120972=DIRECTION('ref_axis',(0.587589051772227,-0.809159506053914,0.));
#120973=DIRECTION('center_axis',(-0.587785252292471,0.809016994374949,8.27701011433315E-17));
#120974=DIRECTION('ref_axis',(-0.809016994374949,-0.587785252292471,1.88536659549102E-32));
#120975=DIRECTION('center_axis',(0.58778525229246,-0.809016994374957,0.));
#120976=DIRECTION('ref_axis',(0.809016994374957,0.58778525229246,0.));
#120977=DIRECTION('center_axis',(-5.8046805746579E-17,-1.13923270769252E-16,
-1.));
#120978=DIRECTION('ref_axis',(0.,1.,-1.12832121675104E-16));
#120979=DIRECTION('center_axis',(-0.808874435122371,-0.587981418248456,
0.));
#120980=DIRECTION('ref_axis',(0.587981418248456,-0.808874435122371,0.));
#120981=DIRECTION('center_axis',(0.311481909863959,-0.42871806929052,-0.848044713969322));
#120982=DIRECTION('ref_axis',(-4.58604169299522E-15,0.892441837073402,-0.45116246235813));
#120983=DIRECTION('center_axis',(0.311481604401026,-0.428717648856901,0.848045038708661));
#120984=DIRECTION('ref_axis',(-4.08016432328408E-16,-0.892442084777747,
-0.451161972375276));
#120985=DIRECTION('center_axis',(0.311481949429352,-0.428718080858207,-0.848044693589286));
#120986=DIRECTION('ref_axis',(-0.49479556222845,0.688740099742701,-0.529919264233191));
#120987=DIRECTION('center_axis',(0.311481948263326,-0.428718122142675,-0.848044673146728));
#120988=DIRECTION('ref_axis',(-9.98849586125472E-16,0.892441805934786,-0.451162523953241));
#120989=DIRECTION('center_axis',(-0.311481603317813,0.428717684280574,-0.848045021198561));
#120990=DIRECTION('ref_axis',(0.501950189215672,-0.683543400919725,-0.529919264233192));
#120991=DIRECTION('center_axis',(0.311481637390342,-0.4287176942628,0.848045003637555));
#120992=DIRECTION('ref_axis',(-8.8971283331398E-15,-0.892442058026248,-0.451162025292327));
#120993=DIRECTION('center_axis',(-0.809168721883308,-0.587576360591314,
1.08417291060497E-13));
#120994=DIRECTION('ref_axis',(0.587576360591314,-0.809168721883308,-1.4872443511391E-27));
#120995=DIRECTION('center_axis',(0.587785252292496,-0.809016994374931,4.42022290584706E-14));
#120996=DIRECTION('ref_axis',(0.809016994374931,0.587785252292496,1.60275226051148E-30));
#120997=DIRECTION('center_axis',(-5.8046805746579E-17,-1.13923270769252E-16,
-1.));
#120998=DIRECTION('ref_axis',(0.,1.,-1.20114286872534E-16));
#120999=DIRECTION('center_axis',(-0.808865212939984,-0.587994104813606,
0.));
#121000=DIRECTION('ref_axis',(0.587994104813606,-0.808865212939984,0.));
#121001=DIRECTION('center_axis',(0.587785252292471,-0.809016994374949,-8.27701011433315E-17));
#121002=DIRECTION('ref_axis',(0.809016994374949,0.587785252292471,6.81387014938251E-31));
#121003=DIRECTION('center_axis',(0.509008435040905,-0.700641118228933,-0.500012436349457));
#121004=DIRECTION('ref_axis',(-0.294700492553427,0.403936649473218,-0.866017784402329));
#121005=DIRECTION('center_axis',(-0.311481948263287,0.428718122142701,0.848044673146729));
#121006=DIRECTION('ref_axis',(-6.11337967909926E-15,-0.892441805934776,
0.45116252395326));
#121007=DIRECTION('center_axis',(-0.293895578892578,0.40451254409714,0.86602251147153));
#121008=DIRECTION('ref_axis',(-0.512651652659763,0.697988741331279,-0.499999999999991));
#121009=DIRECTION('center_axis',(0.293895578599952,-0.404512560891364,-0.866022503726381));
#121010=DIRECTION('ref_axis',(4.4423106715044E-15,0.906035256115537,-0.423202214875647));
#121011=DIRECTION('center_axis',(-0.311481949376662,0.428718080656496,0.848044693710611));
#121012=DIRECTION('ref_axis',(-0.502130522402205,0.683410939235411,-0.529919264233206));
#121013=DIRECTION('center_axis',(-0.311481909863924,0.42871806929054,0.848044713969325));
#121014=DIRECTION('ref_axis',(-5.18787663535866E-16,-0.892441837073395,
0.451162462358144));
#121015=DIRECTION('center_axis',(0.587785252292496,-0.809016994374931,0.));
#121016=DIRECTION('ref_axis',(0.809016994374931,0.587785252292496,0.));
#121017=DIRECTION('center_axis',(-0.587785252292496,0.809016994374931,0.));
#121018=DIRECTION('ref_axis',(-0.809016994374931,-0.587785252292496,0.));
#121019=DIRECTION('center_axis',(0.587785252292471,-0.809016994374949,-8.27701011433315E-17));
#121020=DIRECTION('ref_axis',(0.809016994374949,0.587785252292471,6.81387014938251E-31));
#121021=DIRECTION('center_axis',(0.587785252292496,-0.809016994374931,6.42295984872268E-14));
#121022=DIRECTION('ref_axis',(0.809016994374931,0.587785252292496,4.46555866784231E-30));
#121023=DIRECTION('center_axis',(0.587785252292471,-0.809016994374949,-8.27701011433315E-17));
#121024=DIRECTION('ref_axis',(0.809016994374949,0.587785252292471,6.81387014938251E-31));
#121025=DIRECTION('center_axis',(-0.50901609747414,0.700659176689939,-0.499979330205134));
#121026=DIRECTION('ref_axis',(-0.293100449232374,0.405058175799812,0.866036951219467));
#121027=DIRECTION('center_axis',(0.293895658256105,-0.404512670528654,0.866022425483306));
#121028=DIRECTION('ref_axis',(4.45081872959523E-15,-0.906035197473508,-0.42320234042257));
#121029=DIRECTION('center_axis',(0.293895663527827,-0.404512677784641,0.866022420305062));
#121030=DIRECTION('ref_axis',(-0.809016994377093,-0.58778525228952,2.06309159991821E-12));
#121031=DIRECTION('center_axis',(-0.250002507183327,0.43301704446117,0.866022508719123));
#121032=DIRECTION('ref_axis',(0.866025403781571,0.500000000004967,-3.3219271679524E-12));
#121033=DIRECTION('center_axis',(-0.433035128829051,0.74997876016359,0.500012436348829));
#121034=DIRECTION('ref_axis',(0.249149002214356,-0.433518133177727,0.866017784402659));
#121035=DIRECTION('center_axis',(0.250002511507192,-0.433017051950268,-0.866022503726315));
#121036=DIRECTION('ref_axis',(-2.44740229890228E-15,0.894424794863789,-0.447218387740117));
#121037=DIRECTION('center_axis',(0.50000000000001,-0.866025403784433,0.));
#121038=DIRECTION('ref_axis',(0.866025403784433,0.50000000000001,0.));
#121039=DIRECTION('center_axis',(-0.499999999999998,0.86602540378444,7.0408453444955E-17));
#121040=DIRECTION('ref_axis',(-0.86602540378444,-0.499999999999998,-4.55018569865247E-33));
#121041=DIRECTION('center_axis',(-0.50000000000001,0.866025403784433,0.));
#121042=DIRECTION('ref_axis',(-0.866025403784433,-0.50000000000001,0.));
#121043=DIRECTION('center_axis',(-0.499999999999998,0.86602540378444,7.0408453444955E-17));
#121044=DIRECTION('ref_axis',(-0.86602540378444,-0.499999999999998,-4.55018569865247E-33));
#121045=DIRECTION('center_axis',(0.499999999999998,-0.86602540378444,0.));
#121046=DIRECTION('ref_axis',(0.86602540378444,0.499999999999998,0.));
#121047=DIRECTION('center_axis',(-0.264962106632886,0.458927830768629,-0.848045003637581));
#121048=DIRECTION('ref_axis',(4.53285787055483E-15,0.87947860205333,0.475938429348083));
#121049=DIRECTION('center_axis',(0.250002579266718,-0.43301716931321,0.866022425483292));
#121050=DIRECTION('ref_axis',(-2.13567853825987E-15,-0.89442473021642,-0.447218517033099));
#121051=DIRECTION('center_axis',(0.26496207377333,-0.458927817106627,0.848045021297503));
#121052=DIRECTION('ref_axis',(0.420286434054155,-0.736576463610279,-0.529919264233164));
#121053=DIRECTION('center_axis',(-0.264962078570523,0.45892778216319,-0.848045038708655));
#121054=DIRECTION('ref_axis',(-5.22840048568667E-15,0.879478631391258,0.475938375135017));
#121055=DIRECTION('center_axis',(0.25000257708735,-0.433017186566276,0.866022417485778));
#121056=DIRECTION('ref_axis',(0.429067561974281,-0.752263934574464,-0.499999999999992));
#121057=DIRECTION('center_axis',(0.43304850946242,-0.749993105181578,0.499979330205231));
#121058=DIRECTION('ref_axis',(0.250824363783207,-0.432512586701642,-0.866036951219406));
#121059=DIRECTION('center_axis',(-0.866146626230631,-0.499789977759954,
0.));
#121060=DIRECTION('ref_axis',(0.499789977759954,-0.866146626230631,0.));
#121061=DIRECTION('center_axis',(-0.499999999999998,0.86602540378444,7.0408453444955E-17));
#121062=DIRECTION('ref_axis',(-0.86602540378444,-0.499999999999998,-4.55018569865247E-33));
#121063=DIRECTION('center_axis',(0.500000000000051,-0.866025403784409,0.));
#121064=DIRECTION('ref_axis',(0.866025403784409,0.500000000000051,0.));
#121065=DIRECTION('center_axis',(-7.04084534449556E-17,-1.21951018649011E-16,
-1.));
#121066=DIRECTION('ref_axis',(0.,1.,-1.12832121675104E-16));
#121067=DIRECTION('center_axis',(-0.865904130412286,-0.500209992837952,
0.));
#121068=DIRECTION('ref_axis',(0.500209992837952,-0.865904130412285,0.));
#121069=DIRECTION('center_axis',(0.264962338412812,-0.458928232223238,-0.848044713969298));
#121070=DIRECTION('ref_axis',(2.57596116508717E-15,0.879478359737724,-0.475938877118735));
#121071=DIRECTION('center_axis',(0.264962078570518,-0.458927782163196,0.848045038708653));
#121072=DIRECTION('ref_axis',(3.68379810748961E-15,-0.879478631391255,-0.475938375135022));
#121073=DIRECTION('center_axis',(0.264962376556172,-0.458928247861003,-0.84804469358928));
#121074=DIRECTION('ref_axis',(-0.420092076158454,0.736687329159001,-0.529919264233201));
#121075=DIRECTION('center_axis',(0.264962371077221,-0.458928288799652,-0.848044673146739));
#121076=DIRECTION('ref_axis',(-5.61404975480703E-15,0.87947832558851,-0.475938940222411));
#121077=DIRECTION('center_axis',(-0.264962073789195,0.458927817280317,-0.848045021198552));
#121078=DIRECTION('ref_axis',(0.42775071226884,-0.732266960573829,-0.52991926423321));
#121079=DIRECTION('center_axis',(0.264962106632913,-0.458927830768691,0.848045003637539));
#121080=DIRECTION('ref_axis',(6.83278157480275E-15,-0.879478602053292,-0.475938429348154));
#121081=DIRECTION('center_axis',(-0.86615446498511,-0.499776392786171,0.));
#121082=DIRECTION('ref_axis',(0.499776392786171,-0.86615446498511,0.));
#121083=DIRECTION('center_axis',(0.50000000000001,-0.866025403784433,1.36592399683214E-14));
#121084=DIRECTION('ref_axis',(0.866025403784433,0.50000000000001,3.78074180857848E-32));
#121085=DIRECTION('center_axis',(-7.04084534449556E-17,-1.21951018649011E-16,
-1.));
#121086=DIRECTION('ref_axis',(0.,1.,-1.20114286872534E-16));
#121087=DIRECTION('center_axis',(-0.865896284857144,-0.500223573885314,
1.9979245236123E-14));
#121088=DIRECTION('ref_axis',(0.500223573885314,-0.865896284857144,3.61209325582807E-28));
#121089=DIRECTION('center_axis',(0.499999999999998,-0.86602540378444,-7.0408453444955E-17));
#121090=DIRECTION('ref_axis',(0.86602540378444,0.499999999999998,-9.66189415760573E-31));
#121091=DIRECTION('center_axis',(0.432983094185433,-0.750008802378803,-0.50001243634926));
#121092=DIRECTION('ref_axis',(-0.250863215179511,0.432528431861373,-0.866017784402457));
#121093=DIRECTION('center_axis',(-0.264962371077247,0.458928288799648,0.848044673146733));
#121094=DIRECTION('ref_axis',(5.87156122999725E-15,-0.87947832558851,0.47593894022241));
#121095=DIRECTION('center_axis',(-0.250002513557899,0.433017035276017,0.866022511471556));
#121096=DIRECTION('ref_axis',(-0.436883602758814,0.747751775417836,-0.499999999999954));
#121097=DIRECTION('center_axis',(0.250002511507137,-0.433017051950172,-0.866022503726379));
#121098=DIRECTION('ref_axis',(-1.53955398992304E-15,0.894424794863842,-0.447218387740011));
#121099=DIRECTION('center_axis',(-0.264962376528112,0.458928247652971,0.848044693710625));
#121100=DIRECTION('ref_axis',(-0.427943903631055,0.732154074454021,-0.529919264233139));
#121101=DIRECTION('center_axis',(-0.264962338412751,0.458928232223239,0.848044713969316));
#121102=DIRECTION('ref_axis',(-5.96114674208875E-16,-0.879478359737728,
0.475938877118728));
#121103=DIRECTION('center_axis',(0.50000000000001,-0.866025403784433,7.46354751724617E-14));
#121104=DIRECTION('ref_axis',(0.866025403784433,0.50000000000001,5.01950811882019E-30));
#121105=DIRECTION('center_axis',(-0.499999999999998,0.86602540378444,0.));
#121106=DIRECTION('ref_axis',(-0.86602540378444,-0.499999999999998,0.));
#121107=DIRECTION('center_axis',(0.499999999999998,-0.86602540378444,-7.0408453444955E-17));
#121108=DIRECTION('ref_axis',(0.86602540378444,0.499999999999998,-4.74656639208921E-31));
#121109=DIRECTION('center_axis',(0.50000000000001,-0.866025403784433,4.73169952358149E-14));
#121110=DIRECTION('ref_axis',(0.866025403784433,0.50000000000001,9.25800991341574E-31));
#121111=DIRECTION('center_axis',(0.499999999999998,-0.86602540378444,-7.0408453444955E-17));
#121112=DIRECTION('ref_axis',(0.86602540378444,0.499999999999998,-4.74656639208921E-31));
#121113=DIRECTION('center_axis',(-0.43298882701923,0.750027562856223,-0.499979330205226));
#121114=DIRECTION('ref_axis',(-0.249154705657362,0.433476564270054,0.866036951219417));
#121115=DIRECTION('center_axis',(0.250002579266723,-0.433017169313219,0.866022425483285));
#121116=DIRECTION('ref_axis',(-4.93751510904469E-15,-0.894424730216415,
-0.447218517033108));
#121117=DIRECTION('center_axis',(0.250002583755585,-0.43301717708815,0.866022420299926));
#121118=DIRECTION('ref_axis',(-0.866025403781823,-0.500000000004529,-3.00721826427187E-12));
#121119=DIRECTION('center_axis',(-0.203370361061121,0.456777309665475,0.866022508724017));
#121120=DIRECTION('ref_axis',(0.91354545764447,0.406736643071602,2.62257407997201E-12));
#121121=DIRECTION('center_axis',(-0.352268789802114,0.791134794600335,0.500012436349378));
#121122=DIRECTION('ref_axis',(0.202469153705661,-0.457186437787129,0.866017784402393));
#121123=DIRECTION('center_axis',(0.203370364581923,-0.45677731757327,-0.866022503726308));
#121124=DIRECTION('ref_axis',(3.44850229257831E-15,0.8845070363821,-0.466526850878441));
#121125=DIRECTION('center_axis',(0.406736643075797,-0.913545457642603,0.));
#121126=DIRECTION('ref_axis',(0.913545457642603,0.406736643075797,0.));
#121127=DIRECTION('center_axis',(-0.406736643075798,0.913545457642602,5.72753959967194E-17));
#121128=DIRECTION('ref_axis',(-0.913545457642602,-0.406736643075798,-5.41935833849719E-34));
#121129=DIRECTION('center_axis',(-0.406736643075807,0.913545457642598,0.));
#121130=DIRECTION('ref_axis',(-0.913545457642598,-0.406736643075807,0.));
#121131=DIRECTION('center_axis',(-0.406736643075798,0.913545457642602,5.72753959967194E-17));
#121132=DIRECTION('ref_axis',(-0.913545457642602,-0.406736643075798,-5.41935833849719E-34));
#121133=DIRECTION('center_axis',(0.406736643075817,-0.913545457642594,0.));
#121134=DIRECTION('ref_axis',(0.913545457642593,0.406736643075817,0.));
#121135=DIRECTION('center_axis',(-0.215539595588311,0.484109857923781,-0.848045003637569));
#121136=DIRECTION('ref_axis',(2.23395688692736E-15,0.868458021515989,0.495762710240024));
#121137=DIRECTION('center_axis',(0.203370419702463,-0.456777441376072,0.866022425483297));
#121138=DIRECTION('ref_axis',(-6.45206232673447E-15,-0.88450696681206,-0.466526982779055));
#121139=DIRECTION('center_axis',(0.215539564334499,-0.484109840902877,0.848045021297505));
#121140=DIRECTION('ref_axis',(0.340990855180419,-0.776473315753921,-0.529919264233183));
#121141=DIRECTION('center_axis',(-0.215539572760312,0.484109806651254,-0.848045038708669));
#121142=DIRECTION('ref_axis',(2.33490112882762E-15,0.868458052949978,0.495762655175168));
#121143=DIRECTION('center_axis',(0.203370415729658,-0.456777458307689,0.866022417485779));
#121144=DIRECTION('ref_axis',(0.348084091917939,-0.792992726923577,-0.499999999999973));
#121145=DIRECTION('center_axis',(0.352280597670804,-0.791150459692759,0.499979330205397));
#121146=DIRECTION('ref_axis',(0.204240445633901,-0.456361522797458,-0.866036951219318));
#121147=DIRECTION('center_axis',(-0.913644062717548,-0.406515100163541,
0.));
#121148=DIRECTION('ref_axis',(0.406515100163541,-0.913644062717548,0.));
#121149=DIRECTION('center_axis',(-0.406736643075798,0.913545457642602,5.72753959967194E-17));
#121150=DIRECTION('ref_axis',(-0.913545457642602,-0.406736643075798,-5.41935833849719E-34));
#121151=DIRECTION('center_axis',(0.406736643075807,-0.913545457642598,0.));
#121152=DIRECTION('ref_axis',(0.913545457642598,0.406736643075807,0.));
#121153=DIRECTION('center_axis',(-8.35415108931911E-17,-1.28642645648559E-16,
-1.));
#121154=DIRECTION('ref_axis',(0.,1.,-1.12832121675104E-16));
#121155=DIRECTION('center_axis',(-0.913446798847332,-0.406958162070208,
0.));
#121156=DIRECTION('ref_axis',(0.406958162070208,-0.913446798847332,0.));
#121157=DIRECTION('center_axis',(0.215539784135028,-0.484110281406739,-0.848044713969325));
#121158=DIRECTION('ref_axis',(2.06854852506343E-15,0.868457761888277,-0.495763165045573));
#121159=DIRECTION('center_axis',(0.215539572760318,-0.484109806651269,0.848045038708658));
#121160=DIRECTION('ref_axis',(3.65071283929963E-15,-0.868458052949968,-0.495762655175186));
#121161=DIRECTION('center_axis',(0.215539820427322,-0.484110300949258,-0.848044693589304));
#121162=DIRECTION('ref_axis',(-0.340785973393802,0.776563258036676,-0.529919264233243));
#121163=DIRECTION('center_axis',(0.215539810706706,-0.484110341087606,-0.848044673146739));
#121164=DIRECTION('ref_axis',(-5.01178427115621E-15,0.868457725299272,-0.495763229140701));
#121165=DIRECTION('center_axis',(-0.215539564340934,0.484109841073328,-0.848045021198567));
#121166=DIRECTION('ref_axis',(0.348864709025402,-0.772967650158224,-0.529919264233237));
#121167=DIRECTION('center_axis',(0.215539595588311,-0.484109857923781,0.848045003637569));
#121168=DIRECTION('ref_axis',(-2.23395688692736E-15,-0.868458021515989,
-0.495762710240024));
#121169=DIRECTION('center_axis',(-0.913650438514067,-0.406500770236727,
-2.49595411736522E-14));
#121170=DIRECTION('ref_axis',(0.406500770236727,-0.913650438514067,-1.62456620638984E-28));
#121171=DIRECTION('center_axis',(0.406736643075807,-0.913545457642598,0.));
#121172=DIRECTION('ref_axis',(0.913545457642598,0.406736643075807,0.));
#121173=DIRECTION('center_axis',(-8.35415108931911E-17,-1.28642645648559E-16,
-1.));
#121174=DIRECTION('ref_axis',(0.,1.,-1.20114286872534E-16));
#121175=DIRECTION('center_axis',(-0.913440415876952,-0.406972488803039,
2.71806413419028E-15));
#121176=DIRECTION('ref_axis',(0.406972488803039,-0.913440415876953,-4.76606432941746E-29));
#121177=DIRECTION('center_axis',(0.406736643075798,-0.913545457642602,-5.72753959967194E-17));
#121178=DIRECTION('ref_axis',(0.913545457642602,0.406736643075798,-5.47412728233073E-31));
#121179=DIRECTION('center_axis',(0.352213899941388,-0.79115923314136,-0.500012436348591));
#121180=DIRECTION('ref_axis',(-0.2042774279645,0.456381342215308,-0.866017784402816));
#121181=DIRECTION('center_axis',(-0.215539810706709,0.484110341087599,0.848044673146742));
#121182=DIRECTION('ref_axis',(-3.47902836708183E-15,-0.868457725299276,
0.495763229140693));
#121183=DIRECTION('center_axis',(-0.203370368361164,0.456777301206146,0.86602251147154));
#121184=DIRECTION('ref_axis',(-0.356328964666388,0.789322284583287,-0.5));
#121185=DIRECTION('center_axis',(0.203370364581877,-0.456777317573194,-0.86602250372636));
#121186=DIRECTION('ref_axis',(-5.71178009095155E-16,0.884507036382143,-0.466526850878359));
#121187=DIRECTION('center_axis',(-0.215539820426654,0.484110300737056,0.84804469371061));
#121188=DIRECTION('ref_axis',(-0.349068641861699,0.772875576443818,-0.529919264233209));
#121189=DIRECTION('center_axis',(-0.21553978413504,0.484110281406731,0.848044713969326));
#121190=DIRECTION('ref_axis',(-4.09518441222106E-16,-0.868457761888281,
0.495763165045567));
#121191=DIRECTION('center_axis',(0.406736643075807,-0.913545457642598,0.));
#121192=DIRECTION('ref_axis',(0.913545457642598,0.406736643075807,0.));
#121193=DIRECTION('center_axis',(-0.406736643075797,0.913545457642603,0.));
#121194=DIRECTION('ref_axis',(-0.913545457642603,-0.406736643075797,0.));
#121195=DIRECTION('center_axis',(0.406736643075798,-0.913545457642602,-5.72753959967194E-17));
#121196=DIRECTION('ref_axis',(0.913545457642602,0.406736643075798,-5.47412728233073E-31));
#121197=DIRECTION('center_axis',(0.406736643075807,-0.913545457642598,4.99133465116398E-14));
#121198=DIRECTION('ref_axis',(0.913545457642598,0.406736643075807,-2.16629559445036E-31));
#121199=DIRECTION('center_axis',(0.406736643075798,-0.913545457642602,-5.72753959967194E-17));
#121200=DIRECTION('ref_axis',(0.913545457642602,0.406736643075798,-5.47412728233073E-31));
#121201=DIRECTION('center_axis',(-0.352217640366552,0.79117849009073,-0.49997933020513));
#121202=DIRECTION('ref_axis',(-0.202479170978456,0.457145692796473,0.866036951219467));
#121203=DIRECTION('center_axis',(0.20337041970247,-0.456777441376074,0.866022425483294));
#121204=DIRECTION('ref_axis',(2.38658905335212E-15,-0.884506966812058,-0.46652698277906));
#121205=DIRECTION('center_axis',(0.203370423351772,-0.456777449572533,0.866022420303154));
#121206=DIRECTION('ref_axis',(-0.913545457644961,-0.4067366430705,3.35689480664158E-12));
#121207=DIRECTION('center_axis',(-0.154510046710301,0.475533027088488,0.866022508722285));
#121208=DIRECTION('ref_axis',(0.951056516295949,0.309016994372499,1.50360913918416E-12));
#121209=DIRECTION('center_axis',(-0.267642920195437,0.823622990673084,0.500012436349322));
#121210=DIRECTION('ref_axis',(0.153571010753323,-0.475845712132491,0.866017784402448));
#121211=DIRECTION('center_axis',(0.154510049384272,-0.475533035318153,-0.866022503726303));
#121212=DIRECTION('ref_axis',(-5.19003034006092E-15,0.876548788012428,-0.481313018974081));
#121213=DIRECTION('center_axis',(0.309016994374956,-0.951056516295151,-5.19628367180438E-14));
#121214=DIRECTION('ref_axis',(0.951056516295151,0.309016994374956,-4.37244376738262E-28));
#121215=DIRECTION('center_axis',(-0.309016994374945,0.951056516295154,4.35148173242966E-17));
#121216=DIRECTION('ref_axis',(-0.951056516295154,-0.309016994374945,1.82501959765721E-33));
#121217=DIRECTION('center_axis',(-0.309016994374964,0.951056516295148,4.35209621571297E-14));
#121218=DIRECTION('ref_axis',(-0.951056516295148,-0.309016994374964,3.68292735906465E-28));
#121219=DIRECTION('center_axis',(-0.309016994374945,0.951056516295154,4.35148173242966E-17));
#121220=DIRECTION('ref_axis',(-0.951056516295154,-0.309016994374945,1.82501959765721E-33));
#121221=DIRECTION('center_axis',(0.309016994374972,-0.951056516295146,0.));
#121222=DIRECTION('ref_axis',(0.951056516295146,0.309016994374972,0.));
#121223=DIRECTION('center_axis',(-0.163755587629913,0.503987876169014,-0.84804500363756));
#121224=DIRECTION('ref_axis',(1.56016625491565E-15,0.85964946204147,0.510884333691895));
#121225=DIRECTION('center_axis',(0.154510091261934,-0.475533164204412,0.866022425483295));
#121226=DIRECTION('ref_axis',(-2.58053144970935E-15,-0.876548714628837,
-0.481313152617434));
#121227=DIRECTION('center_axis',(0.163755558325956,-0.503987855974596,0.848045021297504));
#121228=DIRECTION('ref_axis',(0.257959309140313,-0.807862963764521,-0.5299192642332));
#121229=DIRECTION('center_axis',(-0.16375557028641,0.5039878227912,-0.848045038708652));
#121230=DIRECTION('ref_axis',(-1.11721014982679E-15,0.859649495083705,0.51088427809273));
#121231=DIRECTION('center_axis',(0.154510085544824,-0.475533180626773,0.866022417485781));
#121232=DIRECTION('ref_axis',(0.263286939714861,-0.825033325009131,-0.499999999999961));
#121233=DIRECTION('center_axis',(0.267653025932118,-0.823639804208658,0.499979330205263));
#121234=DIRECTION('ref_axis',(0.15541882643006,-0.475210466544791,-0.866036951219395));
#121235=DIRECTION('center_axis',(-0.951131423661017,-0.308786358060986,
0.));
#121236=DIRECTION('ref_axis',(0.308786358060986,-0.951131423661017,0.));
#121237=DIRECTION('center_axis',(-0.309016994374945,0.951056516295154,4.35148173242966E-17));
#121238=DIRECTION('ref_axis',(-0.951056516295154,-0.309016994374945,1.82501959765721E-33));
#121239=DIRECTION('center_axis',(0.309016994374922,-0.951056516295162,0.));
#121240=DIRECTION('ref_axis',(0.951056516295162,0.309016994374922,0.));
#121241=DIRECTION('center_axis',(-9.73020895656139E-17,-1.33924836902177E-16,
-1.));
#121242=DIRECTION('ref_axis',(0.,1.,-1.12832121675104E-16));
#121243=DIRECTION('center_axis',(-0.95098155300316,-0.309247612517378,0.));
#121244=DIRECTION('ref_axis',(0.309247612517378,-0.95098155300316,0.));
#121245=DIRECTION('center_axis',(0.163755730877736,-0.50398831704057,-0.848044713969324));
#121246=DIRECTION('ref_axis',(-1.7259771747372E-15,0.859649189130473,-0.510884792910613));
#121247=DIRECTION('center_axis',(0.163755570286409,-0.503987822791198,0.848045038708653));
#121248=DIRECTION('ref_axis',(1.48111944464757E-15,-0.859649495083707,-0.510884278092728));
#121249=DIRECTION('center_axis',(0.163755764936523,-0.503988340267036,-0.848044693589278));
#121250=DIRECTION('ref_axis',(-0.257746148173802,0.8079309973606,-0.529919264233218));
#121251=DIRECTION('center_axis',(0.163755751065515,-0.503988379172001,-0.848044673146732));
#121252=DIRECTION('ref_axis',(1.54456827304165E-15,0.859649150669465,-0.510884857627692));
#121253=DIRECTION('center_axis',(-0.163755558314028,0.503987856144943,-0.848045021198572));
#121254=DIRECTION('ref_axis',(0.266156471017446,-0.805199544417445,-0.529919264233221));
#121255=DIRECTION('center_axis',(0.1637555876299,-0.503987876168974,0.848045003637586));
#121256=DIRECTION('ref_axis',(-1.26854127671567E-15,-0.859649462041495,
-0.510884333691853));
#121257=DIRECTION('center_axis',(-0.951136266645027,-0.308771440182801,
9.11326423007149E-15));
#121258=DIRECTION('ref_axis',(0.308771440182801,-0.951136266645027,3.37083122818363E-29));
#121259=DIRECTION('center_axis',(0.309016994374964,-0.951056516295148,5.19628367180436E-14));
#121260=DIRECTION('ref_axis',(0.951056516295148,0.309016994374964,4.44026606255851E-28));
#121261=DIRECTION('center_axis',(-9.73020895656139E-17,-1.33924836902177E-16,
-1.));
#121262=DIRECTION('ref_axis',(0.,1.,-1.20114286872534E-16));
#121263=DIRECTION('center_axis',(-0.950976702550722,-0.309262527968967,
9.08207363789511E-15));
#121264=DIRECTION('ref_axis',(0.309262527968967,-0.950976702550722,-3.06533934379229E-29));
#121265=DIRECTION('center_axis',(0.309016994374945,-0.951056516295154,-4.35148173242966E-17));
#121266=DIRECTION('ref_axis',(0.951056516295154,0.309016994374945,1.86718128389415E-31));
#121267=DIRECTION('center_axis',(0.267585776504499,-0.823641557783651,-0.500012436349542));
#121268=DIRECTION('ref_axis',(-0.155453534481129,0.475234043094898,-0.866017784402261));
#121269=DIRECTION('center_axis',(-0.163755751065466,0.503988379172,0.848044673146743));
#121270=DIRECTION('ref_axis',(-4.67841503723397E-16,-0.859649150669469,
0.510884857627686));
#121271=DIRECTION('center_axis',(-0.154510054857217,0.475533019434505,0.866022511471568));
#121272=DIRECTION('ref_axis',(-0.271870311893668,0.822244813611426,-0.499999999999951));
#121273=DIRECTION('center_axis',(0.154510049384245,-0.475533035318,-0.866022503726391));
#121274=DIRECTION('ref_axis',(-2.49680260156733E-15,0.876548788012514,-0.481313018973924));
#121275=DIRECTION('center_axis',(-0.163755764952581,0.503988340057641,0.848044693710619));
#121276=DIRECTION('ref_axis',(-0.266368911015747,0.805129291877293,-0.529919264233198));
#121277=DIRECTION('center_axis',(-0.16375573087769,0.503988317040577,0.848044713969329));
#121278=DIRECTION('ref_axis',(1.0945036666319E-15,-0.859649189130472,0.510884792910616));
#121279=DIRECTION('center_axis',(0.309016994374964,-0.951056516295148,-8.44187456091391E-15));
#121280=DIRECTION('ref_axis',(0.951056516295148,0.309016994374964,-7.18667850250016E-29));
#121281=DIRECTION('center_axis',(-0.309016994374964,0.951056516295148,0.));
#121282=DIRECTION('ref_axis',(-0.951056516295148,-0.309016994374964,0.));
#121283=DIRECTION('center_axis',(0.309016994374945,-0.951056516295154,-4.35148173242966E-17));
#121284=DIRECTION('ref_axis',(0.951056516295154,0.309016994374945,1.86718128389415E-31));
#121285=DIRECTION('center_axis',(0.309016994374964,-0.951056516295148,6.88465858398714E-14));
#121286=DIRECTION('ref_axis',(0.951056516295148,0.309016994374964,5.83027010874528E-28));
#121287=DIRECTION('center_axis',(0.309016994374945,-0.951056516295154,-4.35148173242966E-17));
#121288=DIRECTION('ref_axis',(0.951056516295154,0.309016994374945,1.86718128389415E-31));
#121289=DIRECTION('center_axis',(-0.26758748354017,0.823661100222697,-0.499979330205336));
#121290=DIRECTION('ref_axis',(-0.153585232129532,0.475806237448003,0.866036951219342));
#121291=DIRECTION('center_axis',(0.154510091261981,-0.475533164204417,0.866022425483283));
#121292=DIRECTION('ref_axis',(-4.11550578150327E-15,-0.876548714628833,
-0.481313152617442));
#121293=DIRECTION('center_axis',(0.154510094034046,-0.475533172736068,0.866022420303978));
#121294=DIRECTION('ref_axis',(-0.951056516294272,-0.309016994377662,-1.67844740330627E-12));
#121295=DIRECTION('center_axis',(-0.103956887953752,0.489078705154832,0.866022508720786));
#121296=DIRECTION('ref_axis',(0.978147600734425,0.207911690814845,1.74838271998191E-12));
#121297=DIRECTION('center_axis',(-0.180084698747213,0.847087400905701,0.500012436349287));
#121298=DIRECTION('ref_axis',(0.102990311637667,-0.489291521291171,0.866017784402461));
#121299=DIRECTION('center_axis',(0.103956889752271,-0.489078713616369,-0.866022503726313));
#121300=DIRECTION('ref_axis',(-2.07612945625426E-15,0.870740345484704,-0.491743073916836));
#121301=DIRECTION('center_axis',(0.20791169081776,-0.978147600733806,5.34430112114423E-14));
#121302=DIRECTION('ref_axis',(0.978147600733806,0.20791169081776,-1.51620216886627E-28));
#121303=DIRECTION('center_axis',(-0.207911690817756,0.978147600733806,2.92774812072079E-17));
#121304=DIRECTION('ref_axis',(-0.978147600733806,-0.207911690817756,7.12388199405101E-34));
#121305=DIRECTION('center_axis',(-0.207911690817757,0.978147600733806,0.));
#121306=DIRECTION('ref_axis',(-0.978147600733806,-0.207911690817757,0.));
#121307=DIRECTION('center_axis',(-0.207911690817756,0.978147600733806,2.92774812072079E-17));
#121308=DIRECTION('ref_axis',(-0.978147600733806,-0.207911690817756,2.97300070454562E-33));
#121309=DIRECTION('center_axis',(0.207911690817754,-0.978147600733807,0.));
#121310=DIRECTION('ref_axis',(0.978147600733807,0.207911690817754,0.));
#121311=DIRECTION('center_axis',(-0.110177439185354,0.518344097776653,-0.848045003637581));
#121312=DIRECTION('ref_axis',(3.05434332738335E-15,0.853239582811869,0.521519140898039));
#121313=DIRECTION('center_axis',(0.103956917928293,-0.489078846174039,0.866022425483267));
#121314=DIRECTION('ref_axis',(-2.14699126507327E-16,-0.870740269393755,
-0.491743208652739));
#121315=DIRECTION('center_axis',(0.110177412155606,-0.518344074629213,0.848045021297501));
#121316=DIRECTION('ref_axis',(0.172101506940156,-0.830401496086937,-0.529919264233246));
#121317=DIRECTION('center_axis',(-0.110177427516371,0.518344042878406,-0.848045038708643));
#121318=DIRECTION('ref_axis',(-2.82117091702483E-16,0.853239616987298,0.521519084984786));
#121319=DIRECTION('center_axis',(0.103956910522966,-0.489078861909437,0.866022417485766));
#121320=DIRECTION('ref_axis',(0.175605160701873,-0.848034685337139,-0.500000000000009));
#121321=DIRECTION('center_axis',(0.180092991630808,-0.847105178671968,0.499979330205358));
#121322=DIRECTION('ref_axis',(0.104894406056248,-0.488852904973306,-0.866036951219327));
#121323=DIRECTION('center_axis',(-0.978197989689806,-0.20767448800183,0.));
#121324=DIRECTION('ref_axis',(0.20767448800183,-0.978197989689806,0.));
#121325=DIRECTION('center_axis',(-0.207911690817756,0.978147600733806,2.92774812072079E-17));
#121326=DIRECTION('ref_axis',(-0.978147600733806,-0.207911690817756,7.12388199405101E-34));
#121327=DIRECTION('center_axis',(0.207911690817757,-0.978147600733806,0.));
#121328=DIRECTION('ref_axis',(0.978147600733806,0.207911690817757,0.));
#121329=DIRECTION('center_axis',(-1.11539425682703E-16,-1.37739719617122E-16,
-1.));
#121330=DIRECTION('ref_axis',(0.,1.,-1.12832121675104E-16));
#121331=DIRECTION('center_axis',(-0.978097154258596,-0.208148881407602,
0.));
#121332=DIRECTION('ref_axis',(0.208148881407602,-0.978097154258596,0.));
#121333=DIRECTION('center_axis',(0.110177535564839,-0.518344551206567,-0.848044713969329));
#121334=DIRECTION('ref_axis',(2.56145575730607E-15,0.853239300541051,-0.521519602711363));
#121335=DIRECTION('center_axis',(0.110177427516339,-0.518344042878476,0.848045038708604));
#121336=DIRECTION('ref_axis',(-3.25887323275919E-16,-0.853239616987256,
-0.521519084984855));
#121337=DIRECTION('center_axis',(0.110177567011331,-0.518344577865485,-0.848044693589268));
#121338=DIRECTION('ref_axis',(-0.171882402211984,0.830446875606389,-0.529919264233171));
#121339=DIRECTION('center_axis',(0.110177549147492,-0.518344615107839,-0.848044673146738));
#121340=DIRECTION('ref_axis',(3.51301149947466E-15,0.853239260760973,-0.5215196677941));
#121341=DIRECTION('center_axis',(-0.110177412122692,0.518344074798062,-0.848045021198573));
#121342=DIRECTION('ref_axis',(0.180532167016074,-0.82860950396856,-0.529919264233202));
#121343=DIRECTION('center_axis',(0.110177439185352,-0.518344097776644,0.848045003637587));
#121344=DIRECTION('ref_axis',(-1.85242200733935E-15,-0.853239582811874,
-0.52151914089803));
#121345=DIRECTION('center_axis',(-0.978201246800567,-0.207659145615639,
2.01562116103772E-15));
#121346=DIRECTION('ref_axis',(0.207659145615639,-0.978201246800567,-8.39542909145296E-30));
#121347=DIRECTION('center_axis',(0.207911690817757,-0.978147600733806,0.));
#121348=DIRECTION('ref_axis',(0.978147600733806,0.207911690817757,0.));
#121349=DIRECTION('center_axis',(-1.11539425682703E-16,-1.37739719617122E-16,
-1.));
#121350=DIRECTION('ref_axis',(0.,1.,-1.20114286872534E-16));
#121351=DIRECTION('center_axis',(-0.978093889466682,-0.208164222161104,
0.));
#121352=DIRECTION('ref_axis',(0.208164222161104,-0.978093889466682,0.));
#121353=DIRECTION('center_axis',(0.207911690817756,-0.978147600733806,-2.92774812072079E-17));
#121354=DIRECTION('ref_axis',(0.978147600733806,0.207911690817756,2.34344808075099E-32));
#121355=DIRECTION('center_axis',(0.180025927305188,-0.847099893161506,-0.50001243634901));
#121356=DIRECTION('ref_axis',(-0.10492645948944,0.488879980360625,-0.86601778440261));
#121357=DIRECTION('center_axis',(-0.110177549147462,0.51834461510784,0.848044673146742));
#121358=DIRECTION('ref_axis',(-3.39955805632352E-15,-0.853239260760973,
0.521519667794099));
#121359=DIRECTION('center_axis',(-0.103956896856937,0.489078698391551,0.866022511471557));
#121360=DIRECTION('ref_axis',(-0.184432991092221,0.84615865639774,-0.499999999999948));
#121361=DIRECTION('center_axis',(0.103956889752284,-0.489078713616333,-0.866022503726332));
#121362=DIRECTION('ref_axis',(-1.29450859536298E-15,0.870740345484724,-0.491743073916801));
#121363=DIRECTION('center_axis',(-0.110177567041078,0.518344577660644,0.848044693710607));
#121364=DIRECTION('ref_axis',(-0.180750786618421,0.828561842309514,-0.529919264233229));
#121365=DIRECTION('center_axis',(-0.110177535564859,0.518344551206575,0.848044713969322));
#121366=DIRECTION('ref_axis',(-5.71220637831577E-16,-0.853239300541045,
0.521519602711372));
#121367=DIRECTION('center_axis',(0.207911690817757,-0.978147600733806,0.));
#121368=DIRECTION('ref_axis',(0.978147600733806,0.207911690817757,0.));
#121369=DIRECTION('center_axis',(-0.207911690817754,0.978147600733807,0.));
#121370=DIRECTION('ref_axis',(-0.978147600733807,-0.207911690817754,0.));
#121371=DIRECTION('center_axis',(0.207911690817756,-0.978147600733806,-2.92774812072079E-17));
#121372=DIRECTION('ref_axis',(0.978147600733806,0.207911690817756,2.34344808075099E-32));
#121373=DIRECTION('center_axis',(0.207911690817757,-0.978147600733806,8.51974703129737E-15));
#121374=DIRECTION('ref_axis',(0.978147600733806,0.207911690817757,3.738030205808E-32));
#121375=DIRECTION('center_axis',(0.207911690817756,-0.978147600733806,-2.92774812072079E-17));
#121376=DIRECTION('ref_axis',(0.978147600733806,0.207911690817756,2.34344808075099E-32));
#121377=DIRECTION('center_axis',(-0.180025582247462,0.847119506978757,-0.499979330205289));
#121378=DIRECTION('ref_axis',(-0.10300858135653,0.489253749387328,0.866036951219379));
#121379=DIRECTION('center_axis',(0.103956917928286,-0.489078846174001,0.866022425483289));
#121380=DIRECTION('ref_axis',(-6.13614011915674E-16,-0.870740269393776,
-0.491743208652701));
#121381=DIRECTION('center_axis',(0.103956919793741,-0.489078854950233,0.866022420303058));
#121382=DIRECTION('ref_axis',(-0.978147600733392,-0.207911690819706,-1.11896493554894E-12));
#121383=DIRECTION('center_axis',(-0.052264755777721,0.497265934580226,0.866022508719923));
#121384=DIRECTION('ref_axis',(0.994521895368293,0.104528463267463,1.04902963199238E-13));
#121385=DIRECTION('center_axis',(-0.0905534316534342,0.861270944310183,
0.50001243634817));
#121386=DIRECTION('ref_axis',(0.0512812291175601,-0.497376550148614,0.866017784403101));
#121387=DIRECTION('center_axis',(0.0522647566818157,-0.497265943181917,
-0.866022503726311));
#121388=DIRECTION('ref_axis',(1.36013666080525E-16,0.867207748104378,-0.497946504785137));
#121389=DIRECTION('center_axis',(0.104528463267629,-0.994521895368276,0.));
#121390=DIRECTION('ref_axis',(0.994521895368276,0.104528463267629,0.));
#121391=DIRECTION('center_axis',(-0.10452846326765,0.994521895368274,1.47193748793062E-17));
#121392=DIRECTION('ref_axis',(-0.994521895368274,-0.10452846326765,-3.45914136257457E-34));
#121393=DIRECTION('center_axis',(-0.104528463267629,0.994521895368276,-7.13889681646191E-16));
#121394=DIRECTION('ref_axis',(-0.994521895368276,-0.104528463267629,5.1828952049124E-31));
#121395=DIRECTION('center_axis',(-0.10452846326765,0.994521895368274,1.47193748793062E-17));
#121396=DIRECTION('ref_axis',(-0.994521895368274,-0.10452846326765,-3.45914136257457E-34));
#121397=DIRECTION('center_axis',(0.104528463267629,-0.994521895368276,0.));
#121398=DIRECTION('ref_axis',(0.994521895368276,0.104528463267629,0.));
#121399=DIRECTION('center_axis',(-0.0553921636609753,0.527021232978588,
-0.848045003637593));
#121400=DIRECTION('ref_axis',(5.60271951820181E-16,0.849349030019393,0.527831625809894));
#121401=DIRECTION('center_axis',(0.0522647708473854,-0.497266077958573,
0.866022425483295));
#121402=DIRECTION('ref_axis',(4.11267918639886E-16,-0.867207670398082,-0.497946640115918));
#121403=DIRECTION('center_axis',(0.0553921391946266,-0.527021207133024,
0.848045021297509));
#121404=DIRECTION('ref_axis',(0.0843581245662561,-0.843841975854613,-0.529919264233191));
#121405=DIRECTION('center_axis',(-0.0553921577943468,0.527021177161346,
-0.84804503870865));
#121406=DIRECTION('ref_axis',(-5.13852306535033E-16,0.84934906486752,0.527831569734768));
#121407=DIRECTION('center_axis',(0.0522647618447773,-0.49726609283302,0.866022417485766));
#121408=DIRECTION('ref_axis',(0.0859994148067042,-0.861744800189075,-0.499999999999996));
#121409=DIRECTION('center_axis',(0.0905598208269757,-0.861289491529615,
0.499979330205203));
#121410=DIRECTION('ref_axis',(0.0532207406005999,-0.497139368680954,-0.866036951219419));
#121411=DIRECTION('center_axis',(-0.994547213842469,-0.104287292793432,
6.79237952684971E-15));
#121412=DIRECTION('ref_axis',(0.104287292793432,-0.994547213842469,-7.19249397487602E-30));
#121413=DIRECTION('center_axis',(-0.10452846326765,0.994521895368274,1.47193748793062E-17));
#121414=DIRECTION('ref_axis',(-0.994521895368274,-0.10452846326765,-3.45914136257457E-34));
#121415=DIRECTION('center_axis',(0.104528463267628,-0.994521895368276,0.));
#121416=DIRECTION('ref_axis',(0.994521895368276,0.104528463267628,0.));
#121417=DIRECTION('center_axis',(-1.26097532010604E-16,-1.40045497140051E-16,
-1.));
#121418=DIRECTION('ref_axis',(0.,1.,-1.12832121675104E-16));
#121419=DIRECTION('center_axis',(-0.994496518411991,-0.10476962759516,0.));
#121420=DIRECTION('ref_axis',(0.10476962759516,-0.994496518411991,0.));
#121421=DIRECTION('center_axis',(0.0553922121161709,-0.527021693998982,
-0.848044713969329));
#121422=DIRECTION('ref_axis',(-1.55454699377472E-15,0.849348742192412,-0.527832088960275));
#121423=DIRECTION('center_axis',(0.0553921577943474,-0.527021177161352,
0.848045038708646));
#121424=DIRECTION('ref_axis',(1.53390223113159E-16,-0.849349064867516,-0.527831569734774));
#121425=DIRECTION('center_axis',(0.0553922405987001,-0.527021723799408,
-0.848044693589292));
#121426=DIRECTION('ref_axis',(-0.0841354767049436,0.843864204095777,-0.529919264233178));
#121427=DIRECTION('center_axis',(0.0553922189448978,-0.527021758969975,
-0.848044673146736));
#121428=DIRECTION('ref_axis',(-8.8709924467845E-16,0.849348701629309,-0.527832154231445));
#121429=DIRECTION('center_axis',(-0.0553921391437519,0.527021207297586,
-0.848045021198565));
#121430=DIRECTION('ref_axis',(0.092929914832894,-0.8429410443938,-0.529919264233186));
#121431=DIRECTION('center_axis',(0.0553921636609804,-0.527021232978636,
0.848045003637563));
#121432=DIRECTION('ref_axis',(4.3966219094204E-16,-0.849349030019363,-0.527831625809942));
#121433=DIRECTION('center_axis',(-0.994548849394383,-0.104271693993668,
0.));
#121434=DIRECTION('ref_axis',(0.104271693993668,-0.994548849394383,0.));
#121435=DIRECTION('center_axis',(0.104528463267629,-0.994521895368276,7.13889681646191E-16));
#121436=DIRECTION('ref_axis',(0.994521895368276,0.104528463267629,-5.1828952049124E-31));
#121437=DIRECTION('center_axis',(-1.26097532010604E-16,-1.40045497140051E-16,
-1.));
#121438=DIRECTION('ref_axis',(0.,1.,-1.20114286872534E-16));
#121439=DIRECTION('center_axis',(-0.994494875050338,-0.104785225574086,
-5.72514616500437E-15));
#121440=DIRECTION('ref_axis',(0.104785225574086,-0.994494875050338,8.5757403076988E-30));
#121441=DIRECTION('center_axis',(0.10452846326765,-0.994521895368274,-1.47193748793062E-17));
#121442=DIRECTION('ref_axis',(0.994521895368274,0.10452846326765,1.81599985181705E-32));
#121443=DIRECTION('center_axis',(0.0904936763735575,-0.861277224843726,
-0.500012436347226));
#121444=DIRECTION('ref_axis',(-0.0532497883641599,0.49716964623344,-0.866017784403581));
#121445=DIRECTION('center_axis',(-0.0553922189448982,0.527021758969983,
0.848044673146731));
#121446=DIRECTION('ref_axis',(3.87123138543772E-16,-0.849348701629304,0.527832154231452));
#121447=DIRECTION('center_axis',(-0.0522647653346091,0.4972659287836,0.866022511471556));
#121448=DIRECTION('ref_axis',(-0.0949749838151956,0.860801807879908,-0.499999999999986));
#121449=DIRECTION('center_axis',(0.0522647566817756,-0.497265943181796,
-0.866022503726383));
#121450=DIRECTION('ref_axis',(-8.82337668496122E-16,0.867207748104448,-0.497946504785014));
#121451=DIRECTION('center_axis',(-0.055392240655012,0.527021723598282,0.848044693710605));
#121452=DIRECTION('ref_axis',(-0.0931523188089191,0.842916495801946,-0.529919264233232));
#121453=DIRECTION('center_axis',(-0.0553922121161263,0.527021693999001,
0.84804471396932));
#121454=DIRECTION('ref_axis',(3.59452935077625E-16,-0.849348742192401,0.527832088960293));
#121455=DIRECTION('center_axis',(0.104528463267629,-0.994521895368276,7.13889681646191E-16));
#121456=DIRECTION('ref_axis',(0.994521895368276,0.104528463267629,-5.1828952049124E-31));
#121457=DIRECTION('center_axis',(-0.104528463267628,0.994521895368276,0.));
#121458=DIRECTION('ref_axis',(-0.994521895368276,-0.104528463267628,0.));
#121459=DIRECTION('center_axis',(0.10452846326765,-0.994521895368274,-1.47193748793062E-17));
#121460=DIRECTION('ref_axis',(0.994521895368274,0.10452846326765,1.81599985181705E-32));
#121461=DIRECTION('center_axis',(0.104528463267629,-0.994521895368276,7.13889681646191E-16));
#121462=DIRECTION('ref_axis',(0.994521895368276,0.104528463267629,-5.1828952049124E-31));
#121463=DIRECTION('center_axis',(0.10452846326765,-0.994521895368274,-1.47193748793062E-17));
#121464=DIRECTION('ref_axis',(0.994521895368274,0.10452846326765,1.81599985181705E-32));
#121465=DIRECTION('center_axis',(-0.0904912830026993,0.861296695145209,
-0.499979330205226));
#121466=DIRECTION('ref_axis',(-0.0513033469913138,0.497340894869987,0.86603695121941));
#121467=DIRECTION('center_axis',(0.0522647708473846,-0.497266077958562,
0.866022425483301));
#121468=DIRECTION('ref_axis',(1.07940002356267E-15,-0.867207670398088,-0.497946640115907));
#121469=DIRECTION('center_axis',(0.0522647717852579,-0.49726608688173,0.866022420303058));
#121470=DIRECTION('ref_axis',(-0.994521895368593,-0.104528463264607,1.74838271179562E-12));
#121471=DIRECTION('center_axis',(1.82820803129159E-15,0.500005014362592,
0.866022508721491));
#121472=DIRECTION('ref_axis',(1.,7.55301335024178E-12,-4.37095679990844E-12));
#121473=DIRECTION('center_axis',(-3.00422155937779E-5,0.866018223015147,
0.50001243634849));
#121474=DIRECTION('ref_axis',(-0.000989701348168873,-0.500012217439953,
0.866017784402851));
#121475=DIRECTION('center_axis',(-1.99980824065794E-14,-0.500005023014372,
-0.866022503726316));
#121476=DIRECTION('ref_axis',(2.4869776260939E-28,0.866022503726316,-0.500005023014372));
#121477=DIRECTION('center_axis',(0.,-1.,0.));
#121478=DIRECTION('ref_axis',(0.,0.,-1.));
#121479=DIRECTION('center_axis',(3.49148133884313E-15,1.,-4.91659602599733E-31));
#121480=DIRECTION('ref_axis',(-1.,3.49148133884313E-15,-3.11150763893057E-61));
#121481=DIRECTION('center_axis',(0.,1.,0.));
#121482=DIRECTION('ref_axis',(0.,0.,1.));
#121483=DIRECTION('center_axis',(3.49148133884313E-15,1.,-4.91659602599733E-31));
#121484=DIRECTION('ref_axis',(-1.,3.49148133884313E-15,-3.11150763893057E-61));
#121485=DIRECTION('center_axis',(0.,-1.,0.));
#121486=DIRECTION('ref_axis',(0.,0.,-1.));
#121487=DIRECTION('center_axis',(0.,0.52992421326579,-0.848045003637563));
#121488=DIRECTION('ref_axis',(0.,0.848045003637563,0.52992421326579));
#121489=DIRECTION('center_axis',(0.,-0.500005158533422,0.866022425483294));
#121490=DIRECTION('ref_axis',(0.,-0.866022425483294,-0.500005158533421));
#121491=DIRECTION('center_axis',(-2.16272591755565E-8,-0.529924185004355,
0.848045021297496));
#121492=DIRECTION('ref_axis',(-0.00430950303426538,-0.848037146343315,-0.529919264233227));
#121493=DIRECTION('center_axis',(0.,0.529924157141051,-0.848045038708645));
#121494=DIRECTION('ref_axis',(0.,0.848045038708645,0.529924157141051));
#121495=DIRECTION('center_axis',(-1.05145777036886E-8,-0.500005172385382,
0.866022417485751));
#121496=DIRECTION('ref_axis',(-0.00454855868556522,-0.866013458679398,-0.50000000000003));
#121497=DIRECTION('center_axis',(3.4457674556699E-5,-0.866037336481604,
0.499979330205277));
#121498=DIRECTION('ref_axis',(0.000963977567656715,-0.499979069431795,-0.866036951219384));
#121499=DIRECTION('center_axis',(-0.999999970597889,0.000242495818334613,
1.33391011393658E-16));
#121500=DIRECTION('ref_axis',(-0.000242495818334613,-0.999999970597889,
-6.94884378066767E-34));
#121501=DIRECTION('center_axis',(3.49148133884313E-15,1.,-4.91659602599733E-31));
#121502=DIRECTION('ref_axis',(-1.,3.49148133884313E-15,-3.11150763893057E-61));
#121503=DIRECTION('center_axis',(0.,-1.,0.));
#121504=DIRECTION('ref_axis',(0.,0.,-1.));
#121505=DIRECTION('center_axis',(-1.40816906889911E-16,-1.40816906889911E-16,
-1.));
#121506=DIRECTION('ref_axis',(-1.,4.30611566690962E-33,1.12832121675104E-16));
#121507=DIRECTION('center_axis',(-0.999999970597889,-0.000242495818327663,
1.46730112533024E-16));
#121508=DIRECTION('ref_axis',(0.000242495818327663,-0.999999970597889,8.25475152210998E-34));
#121509=DIRECTION('center_axis',(2.89534733035821E-14,-0.529924676825566,
-0.848044713969328));
#121510=DIRECTION('ref_axis',(-3.85833700151325E-28,0.848044713969328,-0.529924676825566));
#121511=DIRECTION('center_axis',(-4.63346027506605E-14,-0.52992415714112,
0.848045038708602));
#121512=DIRECTION('ref_axis',(-2.08103008143499E-28,-0.848045038708602,
-0.52992415714112));
#121513=DIRECTION('center_axis',(2.5213841626272E-8,-0.529924709439993,
-0.848044693589281));
#121514=DIRECTION('ref_axis',(0.00453325469213716,0.848035979777049,-0.529919264233219));
#121515=DIRECTION('center_axis',(4.63345827774717E-14,-0.529924742154432,
-0.848044673146739));
#121516=DIRECTION('ref_axis',(-1.03497526951197E-27,0.848044673146739,-0.529924742154432));
#121517=DIRECTION('center_axis',(2.1691013480987E-8,0.529924185162642,-0.848045021198586));
#121518=DIRECTION('ref_axis',(0.00430950302060195,-0.848037146343406,-0.529919264233192));
#121519=DIRECTION('center_axis',(0.,-0.52992421326579,0.848045003637563));
#121520=DIRECTION('ref_axis',(0.,-0.848045003637563,-0.52992421326579));
#121521=DIRECTION('center_axis',(-0.99999996667151,0.000258180127967688,
1.60069213043906E-16));
#121522=DIRECTION('ref_axis',(-0.000258180127967688,-0.99999996667151,1.64102447194681E-33));
#121523=DIRECTION('center_axis',(0.,-1.,0.));
#121524=DIRECTION('ref_axis',(0.,0.,-1.));
#121525=DIRECTION('center_axis',(-1.40816906889911E-16,-1.40816906889911E-16,
-1.));
#121526=DIRECTION('ref_axis',(-1.,3.33384117180795E-33,1.20114286872534E-16));
#121527=DIRECTION('center_axis',(-0.99999996667151,-0.000258180127960702,
1.45963035752429E-16));
#121528=DIRECTION('ref_axis',(0.000258180127960701,-0.99999996667151,-2.00104120761843E-33));
#121529=DIRECTION('center_axis',(-3.49148133884313E-15,-1.,4.91659602599733E-31));
#121530=DIRECTION('ref_axis',(1.,-3.49148133884313E-15,3.17373779170918E-59));
#121531=DIRECTION('center_axis',(-3.00422140677667E-5,-0.866018223016196,
-0.500012436346673));
#121532=DIRECTION('ref_axis',(-0.000989701277811038,0.500012217438168,-0.866017784403962));
#121533=DIRECTION('center_axis',(0.,0.529924742154432,0.848044673146739));
#121534=DIRECTION('ref_axis',(0.,-0.848044673146739,0.529924742154432));
#121535=DIRECTION('center_axis',(-1.01121416634232E-8,0.500005009599418,
0.866022511471547));
#121536=DIRECTION('ref_axis',(-0.0044764107678598,0.866013834616202,-0.49999999999998));
#121537=DIRECTION('center_axis',(0.,-0.500005023014331,-0.86602250372634));
#121538=DIRECTION('ref_axis',(0.,0.86602250372634,-0.500005023014331));
#121539=DIRECTION('center_axis',(-2.52896301115931E-8,0.529924709245837,
0.848044693710606));
#121540=DIRECTION('ref_axis',(-0.00453325469037203,0.848035979777047,-0.529919264233237));
#121541=DIRECTION('center_axis',(0.,0.529924676825566,0.848044713969328));
#121542=DIRECTION('ref_axis',(0.,-0.848044713969328,0.529924676825566));
#121543=DIRECTION('center_axis',(0.,-1.,0.));
#121544=DIRECTION('ref_axis',(0.,0.,-1.));
#121545=DIRECTION('center_axis',(0.,1.,0.));
#121546=DIRECTION('ref_axis',(0.,0.,1.));
#121547=DIRECTION('center_axis',(-3.49148133884313E-15,-1.,4.91659602599733E-31));
#121548=DIRECTION('ref_axis',(1.,-3.49148133884313E-15,3.17373779170918E-59));
#121549=DIRECTION('center_axis',(0.,-1.,0.));
#121550=DIRECTION('ref_axis',(0.,0.,-1.));
#121551=DIRECTION('center_axis',(-3.49148133884313E-15,-1.,4.91659602599733E-31));
#121552=DIRECTION('ref_axis',(1.,-3.49148133884313E-15,3.17373779170918E-59));
#121553=DIRECTION('center_axis',(3.4457674514454E-5,0.866037336481586,-0.499979330205309));
#121554=DIRECTION('ref_axis',(0.000963977569514902,0.499979069431826,0.866036951219364));
#121555=DIRECTION('center_axis',(0.,-0.500005158533422,0.866022425483294));
#121556=DIRECTION('ref_axis',(0.,-0.866022425483294,-0.500005158533421));
#121557=DIRECTION('center_axis',(-1.43938253461657E-15,-0.500005167509872,
0.866022420300667));
#121558=DIRECTION('ref_axis',(-1.,1.67844740333716E-12,9.79094318613344E-13));
#121559=DIRECTION('center_axis',(0.0522647557773262,0.497265934576325,0.866022508722187));
#121560=DIRECTION('ref_axis',(0.994521895368361,-0.104528463266816,-4.89547161592758E-13));
#121561=DIRECTION('center_axis',(0.090493676372036,0.861277224842593,0.500012436349452));
#121562=DIRECTION('ref_axis',(-0.0532497883447732,-0.497169646237728,0.866017784402312));
#121563=DIRECTION('center_axis',(-0.0522647566818161,-0.497265943181921,
-0.866022503726309));
#121564=DIRECTION('ref_axis',(1.04964660243371E-15,0.867207748104375,-0.497946504785141));
#121565=DIRECTION('center_axis',(-0.104528463267684,-0.99452189536827,0.));
#121566=DIRECTION('ref_axis',(0.99452189536827,-0.104528463267684,0.));
#121567=DIRECTION('center_axis',(0.104528463267657,0.994521895368273,-1.47193748793071E-17));
#121568=DIRECTION('ref_axis',(-0.994521895368273,0.104528463267657,6.90194618736947E-35));
#121569=DIRECTION('center_axis',(0.104528463267683,0.99452189536827,0.));
#121570=DIRECTION('ref_axis',(-0.99452189536827,0.104528463267683,0.));
#121571=DIRECTION('center_axis',(0.104528463267657,0.994521895368273,-1.47193748793071E-17));
#121572=DIRECTION('ref_axis',(-0.994521895368273,0.104528463267657,6.90194618736947E-35));
#121573=DIRECTION('center_axis',(-0.104528463267683,-0.99452189536827,0.));
#121574=DIRECTION('ref_axis',(0.99452189536827,-0.104528463267683,0.));
#121575=DIRECTION('center_axis',(0.0553921636610116,0.527021232978657,-0.848045003637547));
#121576=DIRECTION('ref_axis',(-1.00433790736153E-15,0.849349030019349,0.527831625809965));
#121577=DIRECTION('center_axis',(-0.0522647708473925,-0.49726607795856,
0.866022425483302));
#121578=DIRECTION('ref_axis',(-1.15905889347861E-15,-0.867207670398089,
-0.497946640115906));
#121579=DIRECTION('center_axis',(-0.055392182216939,-0.527021202611195,
0.84804502129751));
#121580=DIRECTION('ref_axis',(-0.0929299148227876,-0.842941044394903,-0.529919264233203));
#121581=DIRECTION('center_axis',(0.0553921577943745,0.527021177161334,-0.848045038708656));
#121582=DIRECTION('ref_axis',(1.26600207161536E-15,0.849349064867527,0.527831569734757));
#121583=DIRECTION('center_axis',(-0.0522647827511113,-0.497266090635737,
0.866022417485731));
#121584=DIRECTION('ref_axis',(-0.0950466972058103,-0.860793892491238,-0.500000000000051));
#121585=DIRECTION('center_axis',(-0.0904912830032905,-0.861296695145041,
0.499979330205408));
#121586=DIRECTION('ref_axis',(-0.0513033469918369,-0.497340894870115,-0.866036951219305));
#121587=DIRECTION('center_axis',(-0.994496518411991,0.10476962759516,0.));
#121588=DIRECTION('ref_axis',(-0.10476962759516,-0.994496518411991,0.));
#121589=DIRECTION('center_axis',(0.104528463267657,0.994521895368273,-1.47193748793071E-17));
#121590=DIRECTION('ref_axis',(-0.994521895368273,0.104528463267657,6.90194618736947E-35));
#121591=DIRECTION('center_axis',(-0.104528463267683,-0.99452189536827,0.));
#121592=DIRECTION('ref_axis',(0.99452189536827,-0.104528463267683,0.));
#121593=DIRECTION('center_axis',(-1.55536281769218E-16,-1.40045497140051E-16,
-1.));
#121594=DIRECTION('ref_axis',(-1.,6.26344097005036E-33,1.12832121675104E-16));
#121595=DIRECTION('center_axis',(-0.994547213842468,0.104287292793436,0.));
#121596=DIRECTION('ref_axis',(-0.104287292793436,-0.994547213842468,0.));
#121597=DIRECTION('center_axis',(-0.0553922121162014,-0.527021693998993,
-0.84804471396932));
#121598=DIRECTION('ref_axis',(7.7366740613734E-16,0.849348742192405,-0.527832088960287));
#121599=DIRECTION('center_axis',(-0.0553921577943754,-0.527021177161343,
0.84804503870865));
#121600=DIRECTION('ref_axis',(-6.73068733579088E-16,-0.849349064867521,
-0.527831569734766));
#121601=DIRECTION('center_axis',(-0.0553921904483075,-0.527021729070454,
-0.848044693589275));
#121602=DIRECTION('ref_axis',(0.0931523188238882,0.842916495800322,-0.529919264233183));
#121603=DIRECTION('center_axis',(-0.0553922189449272,-0.527021758969979,
-0.848044673146731));
#121604=DIRECTION('ref_axis',(5.44485983564514E-16,0.849348701629306,-0.52783215423145));
#121605=DIRECTION('center_axis',(0.055392182295534,0.52702120276216,-0.848045021198559));
#121606=DIRECTION('ref_axis',(-0.0843581245707786,-0.843841975854142,-0.529919264233221));
#121607=DIRECTION('center_axis',(-0.0553921636610064,-0.527021232978609,
0.848045003637578));
#121608=DIRECTION('ref_axis',(-5.90605431002811E-16,-0.84934903001938,-0.527831625809916));
#121609=DIRECTION('center_axis',(-0.994494875050338,0.10478522557409,0.));
#121610=DIRECTION('ref_axis',(-0.10478522557409,-0.994494875050338,0.));
#121611=DIRECTION('center_axis',(-0.104528463267683,-0.99452189536827,0.));
#121612=DIRECTION('ref_axis',(0.99452189536827,-0.104528463267683,0.));
#121613=DIRECTION('center_axis',(-1.55536281769218E-16,-1.40045497140051E-16,
-1.));
#121614=DIRECTION('ref_axis',(-1.,5.41749190418792E-33,1.20114286872534E-16));
#121615=DIRECTION('center_axis',(-0.994548849394382,0.104271693993676,0.));
#121616=DIRECTION('ref_axis',(-0.104271693993676,-0.994548849394382,0.));
#121617=DIRECTION('center_axis',(-0.104528463267657,-0.994521895368273,
1.47193748793071E-17));
#121618=DIRECTION('ref_axis',(0.994521895368273,-0.104528463267657,1.77461199646142E-32));
#121619=DIRECTION('center_axis',(-0.0905534316536479,-0.861270944310105,
-0.500012436348265));
#121620=DIRECTION('ref_axis',(0.0512812290951098,0.497376550151059,-0.866017784403026));
#121621=DIRECTION('center_axis',(0.0553922189449268,0.527021758969972,0.848044673146736));
#121622=DIRECTION('ref_axis',(-1.02650725247837E-15,-0.84934870162931,0.527832154231442));
#121623=DIRECTION('center_axis',(0.0522647452194355,0.497265930897802,0.86602251147155));
#121624=DIRECTION('ref_axis',(0.086071206774765,0.861737632556662,-0.499999999999975));
#121625=DIRECTION('center_axis',(-0.0522647566818046,-0.497265943181812,
-0.866022503726373));
#121626=DIRECTION('ref_axis',(-1.28065569756335E-16,0.867207748104438,-0.497946504785031));
#121627=DIRECTION('center_axis',(0.0553921903445286,0.527021728886068,0.848044693710641));
#121628=DIRECTION('ref_axis',(0.084135476695041,0.843864204096788,-0.52991926423314));
#121629=DIRECTION('center_axis',(0.0553922121161999,0.527021693998978,0.848044713969329));
#121630=DIRECTION('ref_axis',(-1.1898461170849E-16,-0.849348742192414,0.527832088960272));
#121631=DIRECTION('center_axis',(-0.104528463267683,-0.99452189536827,0.));
#121632=DIRECTION('ref_axis',(0.99452189536827,-0.104528463267683,0.));
#121633=DIRECTION('center_axis',(0.104528463267682,0.99452189536827,0.));
#121634=DIRECTION('ref_axis',(-0.99452189536827,0.104528463267682,0.));
#121635=DIRECTION('center_axis',(-0.104528463267657,-0.994521895368273,
1.47193748793071E-17));
#121636=DIRECTION('ref_axis',(0.994521895368273,-0.104528463267657,1.77461199646142E-32));
#121637=DIRECTION('center_axis',(-0.104528463267683,-0.99452189536827,-5.50515425719855E-14));
#121638=DIRECTION('ref_axis',(0.99452189536827,-0.104528463267683,-6.20682976726545E-31));
#121639=DIRECTION('center_axis',(-0.104528463267657,-0.994521895368273,
1.47193748793071E-17));
#121640=DIRECTION('ref_axis',(0.994521895368273,-0.104528463267657,1.77461199646142E-32));
#121641=DIRECTION('center_axis',(0.0905598208272809,0.861289491529787,-0.499979330204851));
#121642=DIRECTION('ref_axis',(0.0532207405929829,0.497139368681404,0.866036951219629));
#121643=DIRECTION('center_axis',(-0.0522647708474152,-0.497266077958594,
0.866022425483281));
#121644=DIRECTION('ref_axis',(8.80735367310087E-16,-0.867207670398069,-0.49794664011594));
#121645=DIRECTION('center_axis',(-0.0522647717855183,-0.497266086884147,
0.866022420301654));
#121646=DIRECTION('ref_axis',(-0.994521895368054,0.104528463269739,1.1889002440261E-12));
#121647=DIRECTION('center_axis',(0.103956887953211,0.489078705152364,0.866022508722245));
#121648=DIRECTION('ref_axis',(0.978147600733814,-0.20791169081772,0.));
#121649=DIRECTION('center_axis',(0.180025927304861,0.847099893161487,0.500012436349159));
#121650=DIRECTION('ref_axis',(-0.104926459551779,-0.488879980347496,0.866017784402469));
#121651=DIRECTION('center_axis',(-0.103956889752312,-0.489078713616371,
-0.866022503726307));
#121652=DIRECTION('ref_axis',(1.59798216899832E-15,0.870740345484702,-0.49174307391684));
#121653=DIRECTION('center_axis',(-0.207911690817751,-0.978147600733807,
0.));
#121654=DIRECTION('ref_axis',(0.978147600733807,-0.207911690817751,0.));
#121655=DIRECTION('center_axis',(0.207911690817763,0.978147600733805,-2.92774812072088E-17));
#121656=DIRECTION('ref_axis',(-0.978147600733805,0.207911690817763,1.17770789928191E-33));
#121657=DIRECTION('center_axis',(0.207911690817757,0.978147600733806,-2.83991567709928E-15));
#121658=DIRECTION('ref_axis',(-0.978147600733806,0.207911690817757,9.97553654791534E-32));
#121659=DIRECTION('center_axis',(0.207911690817763,0.978147600733805,-2.92774812072088E-17));
#121660=DIRECTION('ref_axis',(-0.978147600733805,0.207911690817763,1.17770789928191E-33));
#121661=DIRECTION('center_axis',(-0.207911690817757,-0.978147600733806,
0.));
#121662=DIRECTION('ref_axis',(0.978147600733806,-0.207911690817757,0.));
#121663=DIRECTION('center_axis',(0.110177439185365,0.518344097776706,-0.848045003637548));
#121664=DIRECTION('ref_axis',(-1.70903056951593E-15,0.853239582811836,0.521519140898093));
#121665=DIRECTION('center_axis',(-0.103956917928266,-0.489078846174005,
0.86602242548329));
#121666=DIRECTION('ref_axis',(8.66848073542193E-16,-0.870740269393775,-0.491743208652703));
#121667=DIRECTION('center_axis',(-0.110177454465019,-0.518344065636052,
0.848045021297512));
#121668=DIRECTION('ref_axis',(-0.180532167030478,-0.828609503965439,-0.529919264233174));
#121669=DIRECTION('center_axis',(0.110177427516371,0.518344042878403,-0.848045038708645));
#121670=DIRECTION('ref_axis',(6.45685183168496E-16,0.8532396169873,0.521519084984783));
#121671=DIRECTION('center_axis',(-0.103956931089751,-0.489078857537854,
0.866022417485753));
#121672=DIRECTION('ref_axis',(-0.184503484221683,-0.846143288285166,-0.500000000000025));
#121673=DIRECTION('center_axis',(-0.180025582247593,-0.847119506978661,
0.499979330205405));
#121674=DIRECTION('ref_axis',(-0.103008581348147,-0.489253749389224,-0.866036951219305));
#121675=DIRECTION('center_axis',(-0.978097154258593,0.208148881407615,0.));
#121676=DIRECTION('ref_axis',(-0.208148881407615,-0.978097154258593,0.));
#121677=DIRECTION('center_axis',(0.207911690817763,0.978147600733805,-2.92774812072088E-17));
#121678=DIRECTION('ref_axis',(-0.978147600733805,0.207911690817763,1.17770789928191E-33));
#121679=DIRECTION('center_axis',(-0.207911690817757,-0.978147600733806,
0.));
#121680=DIRECTION('ref_axis',(0.978147600733806,-0.207911690817757,0.));
#121681=DIRECTION('center_axis',(-1.70094388097119E-16,-1.37739719617122E-16,
-1.));
#121682=DIRECTION('ref_axis',(-1.,-7.04637109130665E-33,2.25664243350207E-16));
#121683=DIRECTION('center_axis',(-0.978197989689808,0.20767448800182,0.));
#121684=DIRECTION('ref_axis',(-0.20767448800182,-0.978197989689808,0.));
#121685=DIRECTION('center_axis',(-0.110177535564866,-0.518344551206614,
-0.848044713969297));
#121686=DIRECTION('ref_axis',(-5.11710185561069E-16,0.853239300541021,-0.521519602711412));
#121687=DIRECTION('center_axis',(-0.110177427516374,-0.518344042878421,
0.848045038708634));
#121688=DIRECTION('ref_axis',(1.65648280181603E-15,-0.853239616987289,-0.521519084984801));
#121689=DIRECTION('center_axis',(-0.110177517687313,-0.518344588349581,
-0.848044693589297));
#121690=DIRECTION('ref_axis',(0.180750786622895,0.828561842308536,-0.529919264233231));
#121691=DIRECTION('center_axis',(-0.110177549147463,-0.51834461510784,-0.848044673146742));
#121692=DIRECTION('ref_axis',(-3.37087989426115E-15,0.853239260760974,-0.521519667794099));
#121693=DIRECTION('center_axis',(0.110177454561672,0.518344065777387,-0.848045021198568));
#121694=DIRECTION('ref_axis',(-0.172101506910798,-0.830401496093066,-0.529919264233176));
#121695=DIRECTION('center_axis',(-0.110177439185362,-0.51834409777669,0.848045003637558));
#121696=DIRECTION('ref_axis',(-3.31296850970174E-16,-0.853239582811845,
-0.521519140898077));
#121697=DIRECTION('center_axis',(-0.978093889466682,0.208164222161104,0.));
#121698=DIRECTION('ref_axis',(-0.208164222161104,-0.978093889466682,0.));
#121699=DIRECTION('center_axis',(-0.207911690817757,-0.978147600733806,
0.));
#121700=DIRECTION('ref_axis',(0.978147600733806,-0.207911690817757,0.));
#121701=DIRECTION('center_axis',(-1.70094388097119E-16,-1.37739719617122E-16,
-1.));
#121702=DIRECTION('ref_axis',(-1.,7.29277756332989E-33,1.20114286872534E-16));
#121703=DIRECTION('center_axis',(-0.978201246800563,0.207659145615656,0.));
#121704=DIRECTION('ref_axis',(-0.207659145615656,-0.978201246800563,0.));
#121705=DIRECTION('center_axis',(-0.207911690817763,-0.978147600733805,
2.92774812072088E-17));
#121706=DIRECTION('ref_axis',(0.978147600733805,-0.207911690817763,-1.90483965589786E-31));
#121707=DIRECTION('center_axis',(-0.180084698747701,-0.8470874009056,-0.500012436349282));
#121708=DIRECTION('ref_axis',(0.102990311613069,0.489291521296384,-0.866017784402441));
#121709=DIRECTION('center_axis',(0.110177549147566,0.518344615107822,0.848044673146739));
#121710=DIRECTION('ref_axis',(1.88294772218094E-15,-0.853239260760981,0.521519667794088));
#121711=DIRECTION('center_axis',(0.103956877071345,0.489078702597146,0.866022511471536));
#121712=DIRECTION('ref_axis',(0.175675810167855,0.848020052664948,-0.500000000000007));
#121713=DIRECTION('center_axis',(-0.103956889752265,-0.489078713616244,
-0.866022503726384));
#121714=DIRECTION('ref_axis',(-5.684684706523E-16,0.870740345484775,-0.49174307391671));
#121715=DIRECTION('center_axis',(0.110177517566025,0.518344588176875,0.848044693710617));
#121716=DIRECTION('ref_axis',(0.171882402211048,0.830446875606581,-0.529919264233172));
#121717=DIRECTION('center_axis',(0.110177535564884,0.518344551206558,0.848044713969329));
#121718=DIRECTION('ref_axis',(1.68081909147871E-15,-0.853239300541055,0.521519602711357));
#121719=DIRECTION('center_axis',(-0.207911690817757,-0.978147600733806,
-2.83991567709928E-15));
#121720=DIRECTION('ref_axis',(0.978147600733806,-0.207911690817757,9.97553654791534E-32));
#121721=DIRECTION('center_axis',(0.207911690817754,0.978147600733807,0.));
#121722=DIRECTION('ref_axis',(-0.978147600733807,0.207911690817754,0.));
#121723=DIRECTION('center_axis',(-0.207911690817763,-0.978147600733805,
2.92774812072088E-17));
#121724=DIRECTION('ref_axis',(0.978147600733805,-0.207911690817763,-1.90483965589786E-31));
#121725=DIRECTION('center_axis',(-0.207911690817757,-0.978147600733806,
-1.98794097396939E-14));
#121726=DIRECTION('ref_axis',(0.978147600733806,-0.207911690817757,1.55832197481668E-31));
#121727=DIRECTION('center_axis',(-0.207911690817763,-0.978147600733805,
2.92774812072088E-17));
#121728=DIRECTION('ref_axis',(0.978147600733805,-0.207911690817763,-1.90483965589786E-31));
#121729=DIRECTION('center_axis',(0.18009299163103,0.847105178671961,-0.49997933020529));
#121730=DIRECTION('ref_axis',(0.104894406038834,0.488852904976947,0.866036951219381));
#121731=DIRECTION('center_axis',(-0.10395691792829,-0.489078846174021,0.866022425483278));
#121732=DIRECTION('ref_axis',(2.98952713487412E-15,-0.870740269393765,-0.491743208652721));
#121733=DIRECTION('center_axis',(-0.103956919794205,-0.48907885495245,0.86602242030175));
#121734=DIRECTION('ref_axis',(-0.978147600733542,0.207911690819,7.34320738951004E-13));
#121735=DIRECTION('center_axis',(0.154510046709505,0.47553302708606,0.86602250872376));
#121736=DIRECTION('ref_axis',(0.951056516296192,-0.309016994371752,-1.92322099198249E-12));
#121737=DIRECTION('center_axis',(0.267585776506576,0.823641557785139,0.500012436345979));
#121738=DIRECTION('ref_axis',(-0.15545353447118,-0.475234043094388,0.866017784404327));
#121739=DIRECTION('center_axis',(-0.154510049384291,-0.475533035318142,
-0.866022503726306));
#121740=DIRECTION('ref_axis',(-4.47004182862588E-15,0.876548788012434,-0.48131301897407));
#121741=DIRECTION('center_axis',(-0.309016994374972,-0.951056516295146,
0.));
#121742=DIRECTION('ref_axis',(0.951056516295146,-0.309016994374972,0.));
#121743=DIRECTION('center_axis',(0.309016994374951,0.951056516295152,-4.35148173242975E-17));
#121744=DIRECTION('ref_axis',(-0.951056516295152,0.309016994374951,-3.06907094049306E-33));
#121745=DIRECTION('center_axis',(0.309016994374964,0.951056516295148,0.));
#121746=DIRECTION('ref_axis',(-0.951056516295148,0.309016994374964,0.));
#121747=DIRECTION('center_axis',(0.309016994374951,0.951056516295152,-4.35148173242975E-17));
#121748=DIRECTION('ref_axis',(-0.951056516295152,0.309016994374951,4.2576019536567E-33));
#121749=DIRECTION('center_axis',(-0.309016994374922,-0.951056516295162,
0.));
#121750=DIRECTION('ref_axis',(0.951056516295162,-0.309016994374922,0.));
#121751=DIRECTION('center_axis',(0.163755587629901,0.503987876168977,-0.848045003637584));
#121752=DIRECTION('ref_axis',(-1.98200124493525E-15,0.859649462041493,0.510884333691857));
#121753=DIRECTION('center_axis',(-0.154510091261978,-0.475533164204395,
0.866022425483296));
#121754=DIRECTION('ref_axis',(5.93903874944703E-17,-0.876548714628845,-0.48131315261742));
#121755=DIRECTION('center_axis',(-0.163755599460449,-0.503987842609208,
0.848045021297493));
#121756=DIRECTION('ref_axis',(-0.266156470996902,-0.805199544424196,-0.529919264233282));
#121757=DIRECTION('center_axis',(0.163755570286413,0.50398782279121,-0.848045038708645));
#121758=DIRECTION('ref_axis',(-7.80935410721728E-16,0.8596494950837,0.51088427809274));
#121759=DIRECTION('center_axis',(-0.154510105543908,-0.47553317412871,0.866022417485762));
#121760=DIRECTION('ref_axis',(-0.271938812465217,-0.822222161143212,-0.499999999999993));
#121761=DIRECTION('center_axis',(-0.267587483539972,-0.823661100222839,
0.499979330205208));
#121762=DIRECTION('ref_axis',(-0.153585232132033,-0.475806237447057,-0.866036951219418));
#121763=DIRECTION('center_axis',(-0.950981553003154,0.309247612517397,0.));
#121764=DIRECTION('ref_axis',(-0.309247612517397,-0.950981553003154,0.));
#121765=DIRECTION('center_axis',(0.309016994374951,0.951056516295152,-4.35148173242975E-17));
#121766=DIRECTION('ref_axis',(-0.951056516295152,0.309016994374951,-3.06907094049306E-33));
#121767=DIRECTION('center_axis',(-0.309016994374972,-0.951056516295146,
0.));
#121768=DIRECTION('ref_axis',(0.951056516295146,-0.309016994374972,0.));
#121769=DIRECTION('center_axis',(-1.84331724214208E-16,-1.33924836902177E-16,
-1.));
#121770=DIRECTION('ref_axis',(-1.,-4.69758072753777E-33,2.25664243350207E-16));
#121771=DIRECTION('center_axis',(-0.951131423661017,0.308786358060986,0.));
#121772=DIRECTION('ref_axis',(-0.308786358060986,-0.951131423661017,0.));
#121773=DIRECTION('center_axis',(-0.163755730877694,-0.503988317040576,
-0.848044713969329));
#121774=DIRECTION('ref_axis',(1.26972035331881E-15,0.859649189130472,-0.510884792910615));
#121775=DIRECTION('center_axis',(-0.163755570286353,-0.503987822791173,
0.848045038708679));
#121776=DIRECTION('ref_axis',(-2.66055794635823E-15,-0.859649495083725,
-0.510884278092698));
#121777=DIRECTION('center_axis',(-0.163755716978191,-0.503988355849649,
-0.848044693589274));
#121778=DIRECTION('ref_axis',(0.266368911012766,0.805129291878272,-0.529919264233208));
#121779=DIRECTION('center_axis',(-0.163755751065448,-0.503988379172006,
-0.848044673146743));
#121780=DIRECTION('ref_axis',(-1.29103448395309E-15,0.859649150669466,-0.510884857627691));
#121781=DIRECTION('center_axis',(0.163755599580733,0.503987842736587,-0.848045021198566));
#121782=DIRECTION('ref_axis',(-0.257959309143581,-0.807862963763467,-0.529919264233216));
#121783=DIRECTION('center_axis',(-0.163755587629911,-0.503987876169007,
0.848045003637564));
#121784=DIRECTION('ref_axis',(1.65328349054603E-16,-0.859649462041474,-0.510884333691888));
#121785=DIRECTION('center_axis',(-0.950976702550718,0.309262527968978,9.08207363789492E-15));
#121786=DIRECTION('ref_axis',(-0.309262527968978,-0.950976702550718,-1.94816382726432E-29));
#121787=DIRECTION('center_axis',(-0.309016994374964,-0.951056516295148,
0.));
#121788=DIRECTION('ref_axis',(0.951056516295148,-0.309016994374964,0.));
#121789=DIRECTION('center_axis',(-1.84331724214208E-16,-1.33924836902177E-16,
-1.));
#121790=DIRECTION('ref_axis',(-1.,-6.6676823436159E-33,2.40228573745067E-16));
#121791=DIRECTION('center_axis',(-0.951136266645025,0.308771440182806,0.));
#121792=DIRECTION('ref_axis',(-0.308771440182806,-0.951136266645025,0.));
#121793=DIRECTION('center_axis',(-0.309016994374951,-0.951056516295152,
4.35148173242975E-17));
#121794=DIRECTION('ref_axis',(0.951056516295152,-0.309016994374951,3.88645736880897E-31));
#121795=DIRECTION('center_axis',(-0.267642920194759,-0.823622990673457,
-0.50001243634907));
#121796=DIRECTION('ref_axis',(0.153571010716792,0.475845712144077,-0.86601778440256));
#121797=DIRECTION('center_axis',(0.163755751065493,0.503988379172008,0.848044673146732));
#121798=DIRECTION('ref_axis',(-5.05660704346617E-15,-0.859649150669462,
0.510884857627698));
#121799=DIRECTION('center_axis',(0.154510035620874,0.475533025684823,0.86602251147154));
#121800=DIRECTION('ref_axis',(0.26335567263134,0.825011387614054,-0.500000000000027));
#121801=DIRECTION('center_axis',(-0.154510049384261,-0.475533035318047,
-0.866022503726363));
#121802=DIRECTION('ref_axis',(1.38257175086461E-15,0.876548788012488,-0.481313018973972));
#121803=DIRECTION('center_axis',(0.163755716843087,0.503988355689364,0.848044693710619));
#121804=DIRECTION('ref_axis',(0.257746148192743,0.80793099735453,-0.52991926423326));
#121805=DIRECTION('center_axis',(0.163755730877767,0.50398831704056,0.848044713969324));
#121806=DIRECTION('ref_axis',(-3.08584552958091E-15,-0.859649189130477,
0.510884792910606));
#121807=DIRECTION('center_axis',(-0.309016994374964,-0.951056516295148,
0.));
#121808=DIRECTION('ref_axis',(0.951056516295148,-0.309016994374964,0.));
#121809=DIRECTION('center_axis',(0.309016994374964,0.951056516295148,0.));
#121810=DIRECTION('ref_axis',(-0.951056516295148,0.309016994374964,0.));
#121811=DIRECTION('center_axis',(-0.309016994374951,-0.951056516295152,
4.35148173242975E-17));
#121812=DIRECTION('ref_axis',(0.951056516295152,-0.309016994374951,3.88645736880897E-31));
#121813=DIRECTION('center_axis',(-0.309016994374964,-0.951056516295148,
-6.88465858398752E-14));
#121814=DIRECTION('ref_axis',(0.951056516295148,-0.309016994374964,5.78888311337089E-28));
#121815=DIRECTION('center_axis',(-0.309016994374951,-0.951056516295152,
4.35148173242975E-17));
#121816=DIRECTION('ref_axis',(0.951056516295152,-0.309016994374951,3.88645736880897E-31));
#121817=DIRECTION('center_axis',(0.267653025931577,0.823639804208476,-0.499979330205854));
#121818=DIRECTION('ref_axis',(0.155418826432177,0.475210466544724,0.866036951219052));
#121819=DIRECTION('center_axis',(-0.154510091261975,-0.475533164204399,
0.866022425483295));
#121820=DIRECTION('ref_axis',(8.01177925627987E-16,-0.876548714628843,-0.481313152617424));
#121821=DIRECTION('center_axis',(-0.154510094034388,-0.475533172737027,
0.86602242030339));
#121822=DIRECTION('ref_axis',(-0.951056516296656,0.309016994370322,-2.79741233884318E-12));
#121823=DIRECTION('center_axis',(0.203370361062807,0.456777309669184,0.866022508721665));
#121824=DIRECTION('ref_axis',(0.913545457643418,-0.406736643073965,-1.18890024959013E-12));
#121825=DIRECTION('center_axis',(0.352213899941551,0.791159233141064,0.500012436348945));
#121826=DIRECTION('ref_axis',(-0.204277427942415,-0.456381342225541,0.866017784402633));
#121827=DIRECTION('center_axis',(-0.203370364581912,-0.456777317573273,
-0.86602250372631));
#121828=DIRECTION('ref_axis',(5.88898682911472E-15,0.884507036382098,-0.466526850878444));
#121829=DIRECTION('center_axis',(-0.406736643075807,-0.913545457642598,
0.));
#121830=DIRECTION('ref_axis',(0.913545457642598,-0.406736643075807,0.));
#121831=DIRECTION('center_axis',(0.406736643075804,0.913545457642599,-5.72753959967203E-17));
#121832=DIRECTION('ref_axis',(-0.913545457642599,0.406736643075804,-3.21579896619707E-33));
#121833=DIRECTION('center_axis',(0.406736643075807,0.913545457642598,0.));
#121834=DIRECTION('ref_axis',(-0.913545457642598,0.406736643075807,0.));
#121835=DIRECTION('center_axis',(0.406736643075804,0.913545457642599,-5.72753959967203E-17));
#121836=DIRECTION('ref_axis',(-0.913545457642599,0.406736643075804,-3.21579896619707E-33));
#121837=DIRECTION('center_axis',(-0.406736643075817,-0.913545457642594,
0.));
#121838=DIRECTION('ref_axis',(0.913545457642593,-0.406736643075817,0.));
#121839=DIRECTION('center_axis',(0.215539595588306,0.48410985792377,-0.848045003637576));
#121840=DIRECTION('ref_axis',(5.65310087418454E-16,0.868458021515995,0.495762710240013));
#121841=DIRECTION('center_axis',(-0.203370419702479,-0.456777441376134,
0.866022425483261));
#121842=DIRECTION('ref_axis',(-3.15644426060647E-15,-0.884506966812025,
-0.466526982779122));
#121843=DIRECTION('center_axis',(-0.21553960384998,-0.484109823309468,0.848045021297495));
#121844=DIRECTION('ref_axis',(-0.348864709042233,-0.772967650150662,-0.529919264233186));
#121845=DIRECTION('center_axis',(0.215539572760321,0.484109806651276,-0.848045038708654));
#121846=DIRECTION('ref_axis',(1.88184919665141E-15,0.868458052949964,0.495762655175193));
#121847=DIRECTION('center_axis',(-0.20337043494672,-0.456777449751744,0.866022417485757));
#121848=DIRECTION('ref_axis',(-0.356394722165886,-0.789292595944163,-0.500000000000026));
#121849=DIRECTION('center_axis',(-0.352217640366916,-0.791178490090378,
0.499979330205431));
#121850=DIRECTION('ref_axis',(-0.202479170969598,-0.457145692800741,-0.866036951219285));
#121851=DIRECTION('center_axis',(-0.913446798847324,0.406958162070226,0.));
#121852=DIRECTION('ref_axis',(-0.406958162070226,-0.913446798847324,0.));
#121853=DIRECTION('center_axis',(0.406736643075804,0.913545457642599,-5.72753959967203E-17));
#121854=DIRECTION('ref_axis',(-0.913545457642599,0.406736643075804,-3.21579896619707E-33));
#121855=DIRECTION('center_axis',(-0.406736643075817,-0.913545457642594,
0.));
#121856=DIRECTION('ref_axis',(0.913545457642593,-0.406736643075817,0.));
#121857=DIRECTION('center_axis',(-1.98092302886631E-16,-1.28642645648559E-16,
-1.));
#121858=DIRECTION('ref_axis',(-1.,-2.74025542439703E-33,2.25664243350207E-16));
#121859=DIRECTION('center_axis',(-0.913644062717546,0.406515100163544,0.));
#121860=DIRECTION('ref_axis',(-0.406515100163544,-0.913644062717546,0.));
#121861=DIRECTION('center_axis',(-0.21553978413504,-0.484110281406731,-0.848044713969326));
#121862=DIRECTION('ref_axis',(-4.09518441222106E-16,0.868457761888281,-0.495763165045567));
#121863=DIRECTION('center_axis',(-0.215539572760312,-0.484109806651254,
0.848045038708669));
#121864=DIRECTION('ref_axis',(2.33490112882762E-15,-0.868458052949978,-0.495762655175168));
#121865=DIRECTION('center_axis',(-0.215539774370682,-0.484110321455004,
-0.848044693589299));
#121866=DIRECTION('ref_axis',(0.349068641869932,0.772875576440141,-0.529919264233148));
#121867=DIRECTION('center_axis',(-0.215539810706662,-0.484110341087621,
-0.848044673146742));
#121868=DIRECTION('ref_axis',(2.48178269179927E-15,0.868457725299266,-0.495763229140711));
#121869=DIRECTION('center_axis',(0.215539603972856,0.484109823428023,-0.848045021198588));
#121870=DIRECTION('ref_axis',(-0.340990855181776,-0.776473315753338,-0.529919264233163));
#121871=DIRECTION('center_axis',(-0.215539595588304,-0.484109857923765,
0.84804500363758));
#121872=DIRECTION('ref_axis',(-1.76895097386485E-15,-0.868458021515998,
-0.495762710240009));
#121873=DIRECTION('center_axis',(-0.913440415876946,0.406972488803054,2.22357395402643E-14));
#121874=DIRECTION('ref_axis',(-0.406972488803054,-0.913440415876946,1.79710587910138E-28));
#121875=DIRECTION('center_axis',(-0.406736643075807,-0.913545457642598,
-1.11114268233636E-14));
#121876=DIRECTION('ref_axis',(0.913545457642598,-0.406736643075807,-1.88066567154315E-32));
#121877=DIRECTION('center_axis',(-1.98092302886631E-16,-1.28642645648559E-16,
-1.));
#121878=DIRECTION('ref_axis',(-1.,-4.68821414785493E-33,2.40228573745067E-16));
#121879=DIRECTION('center_axis',(-0.913650438514062,0.40650077023674,0.));
#121880=DIRECTION('ref_axis',(-0.40650077023674,-0.913650438514061,0.));
#121881=DIRECTION('center_axis',(-0.406736643075804,-0.913545457642599,
5.72753959967203E-17));
#121882=DIRECTION('ref_axis',(0.913545457642599,-0.406736643075804,-1.56826318575927E-31));
#121883=DIRECTION('center_axis',(-0.352268789800919,-0.791134794602218,
-0.500012436347239));
#121884=DIRECTION('ref_axis',(0.202469153662353,0.457186437804045,-0.866017784403588));
#121885=DIRECTION('center_axis',(0.215539810706706,0.484110341087606,0.848044673146739));
#121886=DIRECTION('ref_axis',(-5.01178427115621E-15,-0.868457725299272,
0.495763229140701));
#121887=DIRECTION('center_axis',(0.20337034988946,0.45677730943028,0.86602251147154));
#121888=DIRECTION('ref_axis',(0.348150155232207,0.79296372515504,-0.500000000000032));
#121889=DIRECTION('center_axis',(-0.203370364581871,-0.45677731757318,-0.866022503726368));
#121890=DIRECTION('ref_axis',(3.74161672221887E-15,0.88450703638215,-0.466526850878345));
#121891=DIRECTION('center_axis',(0.215539774220846,0.484110321309208,0.84804469371061));
#121892=DIRECTION('ref_axis',(0.340785973393292,0.776563258036921,-0.529919264233212));
#121893=DIRECTION('center_axis',(0.215539784135144,0.484110281406688,0.848044713969324));
#121894=DIRECTION('ref_axis',(-1.82583604731993E-15,-0.868457761888299,
0.495763165045535));
#121895=DIRECTION('center_axis',(-0.406736643075807,-0.913545457642598,
0.));
#121896=DIRECTION('ref_axis',(0.913545457642598,-0.406736643075807,0.));
#121897=DIRECTION('center_axis',(0.406736643075807,0.913545457642598,0.));
#121898=DIRECTION('ref_axis',(-0.913545457642598,0.406736643075807,0.));
#121899=DIRECTION('center_axis',(-0.406736643075804,-0.913545457642599,
5.72753959967203E-17));
#121900=DIRECTION('ref_axis',(0.913545457642599,-0.406736643075804,-1.56826318575927E-31));
#121901=DIRECTION('center_axis',(-0.406736643075807,-0.913545457642598,
2.22228536467272E-14));
#121902=DIRECTION('ref_axis',(0.913545457642598,-0.406736643075807,3.7613313430863E-32));
#121903=DIRECTION('center_axis',(-0.406736643075804,-0.913545457642599,
5.72753959967203E-17));
#121904=DIRECTION('ref_axis',(0.913545457642599,-0.406736643075804,-1.56826318575927E-31));
#121905=DIRECTION('center_axis',(0.352280597671145,0.791150459692763,-0.499979330205151));
#121906=DIRECTION('ref_axis',(0.204240445639906,0.456361522794511,0.866036951219454));
#121907=DIRECTION('center_axis',(-0.203370419702479,-0.456777441376094,
0.866022425483282));
#121908=DIRECTION('ref_axis',(-2.88067167725014E-15,-0.884506966812047,
-0.466526982779081));
#121909=DIRECTION('center_axis',(-0.203370423352518,-0.456777449574212,
0.866022420302094));
#121910=DIRECTION('ref_axis',(-0.913545457642604,0.406736643075794,0.));
#121911=DIRECTION('center_axis',(0.250002507181115,0.433017044457297,0.866022508721698));
#121912=DIRECTION('ref_axis',(0.86602540378529,-0.499999999998525,-9.79094323187051E-13));
#121913=DIRECTION('center_axis',(0.432983094184821,0.750008802378917,0.500012436349618));
#121914=DIRECTION('ref_axis',(-0.250863215193005,-0.432528431853988,0.866017784402236));
#121915=DIRECTION('center_axis',(-0.250002511507198,-0.433017051950279,
-0.866022503726308));
#121916=DIRECTION('ref_axis',(-6.20218011248958E-16,0.894424794863783,-0.447218387740127));
#121917=DIRECTION('center_axis',(-0.499999999999998,-0.86602540378444,-6.09762352041363E-14));
#121918=DIRECTION('ref_axis',(0.86602540378444,-0.499999999999998,8.3104781865219E-28));
#121919=DIRECTION('center_axis',(0.500000000000004,0.866025403784436,-7.04084534449558E-17));
#121920=DIRECTION('ref_axis',(-0.866025403784436,0.500000000000004,-7.94037779396281E-33));
#121921=DIRECTION('center_axis',(0.50000000000001,0.866025403784433,0.));
#121922=DIRECTION('ref_axis',(-0.866025403784433,0.50000000000001,0.));
#121923=DIRECTION('center_axis',(0.500000000000004,0.866025403784436,-7.04084534449558E-17));
#121924=DIRECTION('ref_axis',(-0.866025403784436,0.500000000000004,-7.94037779396281E-33));
#121925=DIRECTION('center_axis',(-0.50000000000001,-0.866025403784433,0.));
#121926=DIRECTION('ref_axis',(0.866025403784433,-0.50000000000001,0.));
#121927=DIRECTION('center_axis',(0.264962106632886,0.458927830768643,-0.848045003637573));
#121928=DIRECTION('ref_axis',(3.30353726242757E-15,0.879478602053321,0.4759384293481));
#121929=DIRECTION('center_axis',(-0.250002579266717,-0.433017169313223,
0.866022425483286));
#121930=DIRECTION('ref_axis',(-6.14028948685692E-15,-0.894424730216413,
-0.447218517033114));
#121931=DIRECTION('center_axis',(-0.264962111224684,-0.45892779548412,0.84804502129748));
#121932=DIRECTION('ref_axis',(-0.427750712264732,-0.732266960576195,-0.529919264233257));
#121933=DIRECTION('center_axis',(0.264962078570521,0.458927782163201,-0.848045038708649));
#121934=DIRECTION('ref_axis',(2.043795734415E-15,0.879478631391252,0.475938375135027));
#121935=DIRECTION('center_axis',(-0.250002595295631,-0.433017176053763,
0.866022417485756));
#121936=DIRECTION('ref_axis',(-0.43694589671013,-0.747715375893923,-0.499999999999991));
#121937=DIRECTION('center_axis',(-0.432988827019556,-0.750027562855828,
0.499979330205536));
#121938=DIRECTION('ref_axis',(-0.249154705644099,-0.433476564278061,-0.866036951219225));
#121939=DIRECTION('center_axis',(-0.865904130412325,0.500209992837883,0.));
#121940=DIRECTION('ref_axis',(-0.500209992837883,-0.865904130412325,0.));
#121941=DIRECTION('center_axis',(0.500000000000004,0.866025403784436,-7.04084534449558E-17));
#121942=DIRECTION('ref_axis',(-0.866025403784436,0.500000000000004,-7.94037779396281E-33));
#121943=DIRECTION('center_axis',(-0.500000000000022,-0.866025403784426,
0.));
#121944=DIRECTION('ref_axis',(0.866025403784426,-0.500000000000022,0.));
#121945=DIRECTION('center_axis',(-2.11225360334866E-16,-1.2195101864901E-16,
-1.));
#121946=DIRECTION('ref_axis',(-1.,-1.17439518188444E-33,2.25664243350207E-16));
#121947=DIRECTION('center_axis',(-0.866146626230631,0.499789977759954,0.));
#121948=DIRECTION('ref_axis',(-0.499789977759954,-0.866146626230631,0.));
#121949=DIRECTION('center_axis',(-0.264962338412801,-0.458928232223203,
-0.84804471396932));
#121950=DIRECTION('ref_axis',(1.63607178079679E-15,0.879478359737744,-0.475938877118698));
#121951=DIRECTION('center_axis',(-0.264962078570535,-0.458927782163211,
0.848045038708639));
#121952=DIRECTION('ref_axis',(1.55530095974517E-15,-0.879478631391246,-0.475938375135039));
#121953=DIRECTION('center_axis',(-0.264962332884843,-0.458928273074652,
-0.848044693589282));
#121954=DIRECTION('ref_axis',(0.42794390361672,0.732154074462357,-0.529919264233198));
#121955=DIRECTION('center_axis',(-0.264962371077225,-0.458928288799661,
-0.848044673146733));
#121956=DIRECTION('ref_axis',(2.91201203045915E-15,0.879478325588505,-0.475938940222419));
#121957=DIRECTION('center_axis',(0.264962111365172,0.458927795585784,-0.84804502119857));
#121958=DIRECTION('ref_axis',(-0.420286434086469,-0.736576463591759,-0.529919264233277));
#121959=DIRECTION('center_axis',(-0.264962106632899,-0.458927830768652,
0.848045003637564));
#121960=DIRECTION('ref_axis',(-1.62952198067E-16,-0.879478602053315,-0.47593842934811));
#121961=DIRECTION('center_axis',(-0.865896284857136,0.500223573885327,3.67572504896101E-15));
#121962=DIRECTION('ref_axis',(-0.500223573885327,-0.865896284857136,-1.1847470281813E-29));
#121963=DIRECTION('center_axis',(-0.50000000000001,-0.866025403784433,1.36592399683214E-14));
#121964=DIRECTION('ref_axis',(0.866025403784433,-0.50000000000001,-3.78074180857848E-32));
#121965=DIRECTION('center_axis',(-2.11225360334866E-16,-1.2195101864901E-16,
-1.));
#121966=DIRECTION('ref_axis',(-1.,-2.81292848871296E-33,2.40228573745067E-16));
#121967=DIRECTION('center_axis',(-0.866154464985103,0.499776392786184,-2.7306262718275E-14));
#121968=DIRECTION('ref_axis',(-0.499776392786184,-0.866154464985103,-3.39882034587859E-28));
#121969=DIRECTION('center_axis',(-0.500000000000004,-0.866025403784436,
7.04084534449558E-17));
#121970=DIRECTION('ref_axis',(0.866025403784436,-0.500000000000004,-4.66754835686058E-31));
#121971=DIRECTION('center_axis',(-0.433035128829375,-0.749978760163243,
-0.500012436349069));
#121972=DIRECTION('ref_axis',(0.249149002240728,0.433518133162794,-0.866017784402547));
#121973=DIRECTION('center_axis',(0.264962371077208,0.45892828879966,0.848044673146739));
#121974=DIRECTION('ref_axis',(-3.94378445652297E-15,-0.879478325588507,
0.475938940222416));
#121975=DIRECTION('center_axis',(0.250002496041659,0.433017045389097,0.866022511471519));
#121976=DIRECTION('ref_axis',(0.429130231859143,0.752228186193846,-0.500000000000034));
#121977=DIRECTION('center_axis',(-0.250002511507148,-0.433017051950192,
-0.866022503726366));
#121978=DIRECTION('ref_axis',(-4.43899159512102E-15,0.894424794863831,-0.447218387740031));
#121979=DIRECTION('center_axis',(0.264962332718263,0.458928272946614,0.848044693710617));
#121980=DIRECTION('ref_axis',(0.420092076154909,0.736687329161024,-0.529919264233199));
#121981=DIRECTION('center_axis',(0.264962338412815,0.458928232223191,0.848044713969322));
#121982=DIRECTION('ref_axis',(-4.71779924553047E-15,-0.879478359737749,
0.475938877118689));
#121983=DIRECTION('center_axis',(-0.50000000000001,-0.866025403784433,-4.73169952358149E-14));
#121984=DIRECTION('ref_axis',(0.866025403784433,-0.50000000000001,9.25800991341574E-31));
#121985=DIRECTION('center_axis',(0.50000000000001,0.866025403784433,0.));
#121986=DIRECTION('ref_axis',(-0.866025403784433,0.50000000000001,0.));
#121987=DIRECTION('center_axis',(-0.500000000000004,-0.866025403784436,
7.04084534449558E-17));
#121988=DIRECTION('ref_axis',(0.866025403784436,-0.500000000000004,-4.66754835686058E-31));
#121989=DIRECTION('center_axis',(-0.50000000000001,-0.866025403784433,-1.35611710376594E-13));
#121990=DIRECTION('ref_axis',(0.866025403784433,-0.50000000000001,3.75412068987699E-30));
#121991=DIRECTION('center_axis',(-0.500000000000004,-0.866025403784436,
7.04084534449558E-17));
#121992=DIRECTION('ref_axis',(0.866025403784436,-0.500000000000004,-4.66754835686058E-31));
#121993=DIRECTION('center_axis',(0.433048509461931,0.749993105181681,-0.4999793302055));
#121994=DIRECTION('ref_axis',(0.250824363779151,0.432512586704298,0.866036951219254));
#121995=DIRECTION('center_axis',(-0.250002579266721,-0.433017169313215,
0.866022425483288));
#121996=DIRECTION('ref_axis',(3.65468156859272E-15,-0.894424730216417,-0.447218517033104));
#121997=DIRECTION('center_axis',(-0.250002583753713,-0.433017177084928,
0.866022420302078));
#121998=DIRECTION('ref_axis',(-0.86602540378536,0.499999999998404,-1.08399728131085E-12));
#121999=DIRECTION('center_axis',(0.293895573516567,0.404512553894631,0.866022508719613));
#122000=DIRECTION('ref_axis',(0.809016994374147,-0.587785252293575,7.34320742400955E-13));
#122001=DIRECTION('center_axis',(0.509008435042963,0.700641118228318,0.500012436348224));
#122002=DIRECTION('ref_axis',(-0.294700492539324,-0.403936649481947,0.866017784403056));
#122003=DIRECTION('center_axis',(-0.293895578600006,-0.404512560891467,
-0.866022503726315));
#122004=DIRECTION('ref_axis',(-5.69513563873506E-15,0.906035256115484,-0.423202214875761));
#122005=DIRECTION('center_axis',(-0.58778525229247,-0.80901699437495,0.));
#122006=DIRECTION('ref_axis',(0.80901699437495,-0.58778525229247,0.));
#122007=DIRECTION('center_axis',(0.587785252292477,0.809016994374945,-8.27701011433323E-17));
#122008=DIRECTION('ref_axis',(-0.809016994374945,0.587785252292477,1.49515186639062E-33));
#122009=DIRECTION('center_axis',(0.587785252292496,0.809016994374931,0.));
#122010=DIRECTION('ref_axis',(-0.809016994374931,0.587785252292496,0.));
#122011=DIRECTION('center_axis',(0.587785252292477,0.809016994374945,-8.27701011433323E-17));
#122012=DIRECTION('ref_axis',(-0.809016994374945,0.587785252292477,1.49515186639062E-33));
#122013=DIRECTION('center_axis',(-0.58778525229247,-0.80901699437495,0.));
#122014=DIRECTION('ref_axis',(0.80901699437495,-0.58778525229247,0.));
#122015=DIRECTION('center_axis',(0.311481637390311,0.428717694262756,-0.848045003637588));
#122016=DIRECTION('ref_axis',(-6.50621339553239E-15,0.892442058026273,0.451162025292277));
#122017=DIRECTION('center_axis',(-0.293895658256084,-0.404512670528678,
0.866022425483301));
#122018=DIRECTION('ref_axis',(2.74693569375712E-15,-0.906035197473498,-0.423202340422592));
#122019=DIRECTION('center_axis',(-0.311481638270574,-0.42871765869024,0.848045021297477));
#122020=DIRECTION('ref_axis',(-0.501950189192533,-0.683543400936663,-0.52991926423326));
#122021=DIRECTION('center_axis',(0.311481604401037,0.428717648856917,-0.848045038708649));
#122022=DIRECTION('ref_axis',(7.95334372440912E-15,0.892442084777736,0.451161972375297));
#122023=DIRECTION('center_axis',(-0.293895674908046,-0.404512675552269,
0.866022417485765));
#122024=DIRECTION('ref_axis',(-0.512709800570221,-0.697946029718086,-0.500000000000004));
#122025=DIRECTION('center_axis',(-0.509016097474224,-0.7006591766899,0.499979330205102));
#122026=DIRECTION('ref_axis',(-0.293100449236653,-0.405058175796668,-0.866036951219489));
#122027=DIRECTION('center_axis',(-0.808874435122379,0.587981418248444,0.));
#122028=DIRECTION('ref_axis',(-0.587981418248444,-0.808874435122379,0.));
#122029=DIRECTION('center_axis',(0.587785252292477,0.809016994374945,-8.27701011433323E-17));
#122030=DIRECTION('ref_axis',(-0.809016994374945,0.587785252292477,1.49515186639062E-33));
#122031=DIRECTION('center_axis',(-0.58778525229247,-0.80901699437495,0.));
#122032=DIRECTION('ref_axis',(0.80901699437495,-0.58778525229247,0.));
#122033=DIRECTION('center_axis',(-2.23587008033243E-16,-1.13923270769252E-16,
-1.));
#122034=DIRECTION('ref_axis',(-1.,3.91465060628147E-34,2.25664243350207E-16));
#122035=DIRECTION('center_axis',(-0.809159506053914,0.587589051772227,0.));
#122036=DIRECTION('ref_axis',(-0.587589051772227,-0.809159506053914,0.));
#122037=DIRECTION('center_axis',(-0.311481909863919,-0.428718069290544,
-0.848044713969325));
#122038=DIRECTION('ref_axis',(5.77422614531214E-15,0.892441837073393,-0.451162462358149));
#122039=DIRECTION('center_axis',(-0.311481604401053,-0.428717648856938,
0.848045038708632));
#122040=DIRECTION('ref_axis',(2.51748144391242E-16,-0.892442084777725,-0.451161972375319));
#122041=DIRECTION('center_axis',(-0.311481908632573,-0.428718110498838,
-0.848044693589268));
#122042=DIRECTION('ref_axis',(0.502130522422689,0.683410939220382,-0.529919264233177));
#122043=DIRECTION('center_axis',(-0.31148194826326,-0.428718122142703,-0.848044673146738));
#122044=DIRECTION('ref_axis',(-5.37120173115187E-15,0.892441805934777,-0.451162523953258));
#122045=DIRECTION('center_axis',(0.31148163842248,0.428717658775535,-0.848045021198563));
#122046=DIRECTION('ref_axis',(-0.494977266821892,-0.688609525583308,-0.529919264233205));
#122047=DIRECTION('center_axis',(-0.311481637390301,-0.428717694262743,
0.848045003637598));
#122048=DIRECTION('ref_axis',(1.33996802632922E-15,-0.892442058026281,-0.451162025292263));
#122049=DIRECTION('center_axis',(-0.808865212939984,0.587994104813606,0.));
#122050=DIRECTION('ref_axis',(-0.587994104813606,-0.808865212939984,0.));
#122051=DIRECTION('center_axis',(-0.587785252292496,-0.809016994374931,
0.));
#122052=DIRECTION('ref_axis',(0.809016994374931,-0.587785252292496,0.));
#122053=DIRECTION('center_axis',(-2.23587008033243E-16,-1.13923270769252E-16,
-1.));
#122054=DIRECTION('ref_axis',(-1.,-1.25019043942798E-33,2.40228573745067E-16));
#122055=DIRECTION('center_axis',(-0.80916872188328,0.587576360591353,-3.2103386036122E-14));
#122056=DIRECTION('ref_axis',(-0.587576360591353,-0.809168721883279,4.76085920470349E-28));
#122057=DIRECTION('center_axis',(-0.587785252292477,-0.809016994374945,
8.27701011433323E-17));
#122058=DIRECTION('ref_axis',(0.809016994374945,-0.587785252292477,-5.76465719897875E-31));
#122059=DIRECTION('center_axis',(-0.509057044368004,-0.700605801485533,
-0.500012436349463));
#122060=DIRECTION('ref_axis',(0.293099122190527,0.405100113144951,-0.866017784402313));
#122061=DIRECTION('center_axis',(0.311481948263274,0.428718122142712,0.848044673146729));
#122062=DIRECTION('ref_axis',(-5.17619376781642E-15,-0.892441805934769,
0.451162523953273));
#122063=DIRECTION('center_axis',(0.293895562533816,0.404512555982461,0.866022511471537));
#122064=DIRECTION('ref_axis',(0.505408667886166,0.703251077799033,-0.500000000000029));
#122065=DIRECTION('center_axis',(-0.293895578599989,-0.404512560891416,
-0.866022503726345));
#122066=DIRECTION('ref_axis',(-2.21255256144257E-15,0.906035256115509,-0.423202214875706));
#122067=DIRECTION('center_axis',(0.311481908458004,0.428718110385629,0.848044693710618));
#122068=DIRECTION('ref_axis',(0.494795562235362,0.688740099737728,-0.5299192642332));
#122069=DIRECTION('center_axis',(0.311481909863932,0.428718069290522,0.848044713969331));
#122070=DIRECTION('ref_axis',(9.11251128025232E-15,-0.892441837073405,0.451162462358124));
#122071=DIRECTION('center_axis',(-0.587785252292496,-0.809016994374931,
-7.63170283020816E-14));
#122072=DIRECTION('ref_axis',(0.809016994374931,-0.587785252292496,-1.1810600377477E-30));
#122073=DIRECTION('center_axis',(0.587785252292496,0.809016994374931,0.));
#122074=DIRECTION('ref_axis',(-0.809016994374931,0.587785252292496,0.));
#122075=DIRECTION('center_axis',(-0.587785252292477,-0.809016994374945,
8.27701011433323E-17));
#122076=DIRECTION('ref_axis',(0.809016994374945,-0.587785252292477,-5.76465719897875E-31));
#122077=DIRECTION('center_axis',(-0.587785252292496,-0.809016994374931,
0.));
#122078=DIRECTION('ref_axis',(0.809016994374931,-0.587785252292496,0.));
#122079=DIRECTION('center_axis',(-0.587785252292477,-0.809016994374945,
8.27701011433323E-17));
#122080=DIRECTION('ref_axis',(0.809016994374945,-0.587785252292477,-5.76465719897875E-31));
#122081=DIRECTION('center_axis',(0.509071851162668,0.700618669263909,-0.499979330205442));
#122082=DIRECTION('ref_axis',(0.294660197703196,0.403924952203149,0.866036951219287));
#122083=DIRECTION('center_axis',(-0.293895658256125,-0.404512670528681,
0.866022425483286));
#122084=DIRECTION('ref_axis',(5.42521881944202E-15,-0.906035197473494,-0.4232023404226));
#122085=DIRECTION('center_axis',(-0.293895663530527,-0.404512677788301,
0.866022420302436));
#122086=DIRECTION('ref_axis',(-0.809016994372353,0.587785252296044,2.55263875924096E-12));
#122087=DIRECTION('center_axis',(0.334568658441521,0.371576139134707,0.866022508722715));
#122088=DIRECTION('ref_axis',(0.743144825480459,-0.669130606355454,-2.65754173435105E-12));
#122089=DIRECTION('center_axis',(0.579456972966894,0.643597063368936,0.500012436348264));
#122090=DIRECTION('ref_axis',(-0.335308969645359,-0.370919252631962,0.866017784403019));
#122091=DIRECTION('center_axis',(-0.334568664232084,-0.371576145565852,
-0.866022503726309));
#122092=DIRECTION('ref_axis',(-7.22273520455772E-15,0.918982183096513,-0.394299058014557));
#122093=DIRECTION('center_axis',(-0.669130606358875,-0.743144825477379,
0.));
#122094=DIRECTION('ref_axis',(0.743144825477379,-0.669130606358875,0.));
#122095=DIRECTION('center_axis',(0.669130606358862,0.743144825477391,-9.42249022928252E-17));
#122096=DIRECTION('ref_axis',(-0.743144825477391,0.669130606358862,5.64385269611616E-33));
#122097=DIRECTION('center_axis',(0.669130606358845,0.743144825477406,3.25153501695813E-14));
#122098=DIRECTION('ref_axis',(-0.743144825477406,0.669130606358845,-2.32720619691874E-30));
#122099=DIRECTION('center_axis',(0.669130606358862,0.743144825477391,-9.42249022928252E-17));
#122100=DIRECTION('ref_axis',(-0.743144825477391,0.669130606358862,5.64385269611616E-33));
#122101=DIRECTION('center_axis',(-0.669130606358872,-0.743144825477382,
0.));
#122102=DIRECTION('ref_axis',(0.743144825477382,-0.669130606358872,0.));
#122103=DIRECTION('center_axis',(0.354588510146763,0.393810436983647,-0.848045003637571));
#122104=DIRECTION('ref_axis',(2.71562606242776E-17,0.906978223357759,0.421177518814577));
#122105=DIRECTION('center_axis',(-0.334568754912021,-0.371576246276125,
0.866022425483293));
#122106=DIRECTION('ref_axis',(6.32948812453082E-15,-0.918982131463643,-0.394299178353873));
#122107=DIRECTION('center_axis',(-0.354588507312263,-0.393810401506322,
0.848045021297508));
#122108=DIRECTION('ref_axis',(-0.570650194832095,-0.627330796735366,-0.529919264233206));
#122109=DIRECTION('center_axis',(0.354588472592004,0.393810395274862,-0.848045038708633));
#122110=DIRECTION('ref_axis',(1.64363307278047E-15,0.906978247051285,0.421177467792116));
#122111=DIRECTION('center_axis',(-0.334568771992555,-0.371576249536343,
0.866022417485771));
#122112=DIRECTION('ref_axis',(-0.582856348570488,-0.640529840781128,-0.49999999999998));
#122113=DIRECTION('center_axis',(-0.579466481046732,-0.643614221961325,
0.499979330205196));
#122114=DIRECTION('ref_axis',(-0.333834922958285,-0.372201885185958,-0.866036951219435));
#122115=DIRECTION('center_axis',(-0.742982542253438,0.669310796197565,0.));
#122116=DIRECTION('ref_axis',(-0.669310796197565,-0.742982542253438,0.));
#122117=DIRECTION('center_axis',(0.669130606358862,0.743144825477391,-9.42249022928252E-17));
#122118=DIRECTION('ref_axis',(-0.743144825477391,0.669130606358862,5.64385269611616E-33));
#122119=DIRECTION('center_axis',(-0.669130606358869,-0.743144825477384,
0.));
#122120=DIRECTION('ref_axis',(0.743144825477384,-0.669130606358869,0.));
#122121=DIRECTION('center_axis',(-2.35041809182736E-16,-1.04647355694969E-16,
-1.));
#122122=DIRECTION('ref_axis',(-1.,1.56586024251259E-33,2.25664243350207E-16));
#122123=DIRECTION('center_axis',(-0.743307065001301,0.668950377172442,0.));
#122124=DIRECTION('ref_axis',(-0.668950377172442,-0.743307065001301,0.));
#122125=DIRECTION('center_axis',(-0.35458882032882,-0.393810781475684,-0.848044713969332));
#122126=DIRECTION('ref_axis',(2.88783290955208E-15,0.906978027661852,-0.421177940232649));
#122127=DIRECTION('center_axis',(-0.354588472592003,-0.393810395274861,
0.848045038708634));
#122128=DIRECTION('ref_axis',(-2.07668913976795E-15,-0.906978247051285,
-0.421177467792115));
#122129=DIRECTION('center_axis',(-0.35458882341487,-0.393810822584025,-0.848044693589289));
#122130=DIRECTION('ref_axis',(0.570815694127792,0.627180210730487,-0.529919264233212));
#122131=DIRECTION('center_axis',(-0.354588864042336,-0.393810830024532,
-0.848044673146736));
#122132=DIRECTION('ref_axis',(1.70751137071295E-15,0.906978000082644,-0.421177999622591));
#122133=DIRECTION('center_axis',(0.3545885074659,0.393810401581074,-0.848045021198556));
#122134=DIRECTION('ref_axis',(-0.564245025066716,-0.633098037496543,-0.529919264233229));
#122135=DIRECTION('center_axis',(-0.354588510146757,-0.393810436983641,
0.848045003637576));
#122136=DIRECTION('ref_axis',(4.72845601854126E-15,-0.906978223357763,-0.421177518814568));
#122137=DIRECTION('center_axis',(-0.742972044483925,0.669322449283883,0.));
#122138=DIRECTION('ref_axis',(-0.669322449283883,-0.742972044483925,0.));
#122139=DIRECTION('center_axis',(-0.669130606358845,-0.743144825477406,
0.));
#122140=DIRECTION('ref_axis',(0.743144825477406,-0.669130606358845,0.));
#122141=DIRECTION('center_axis',(-2.35041809182736E-16,-1.04647355694969E-16,
-1.));
#122142=DIRECTION('ref_axis',(-1.,0.,2.40228573745067E-16));
#122143=DIRECTION('center_axis',(-0.743317556935059,0.668938718831625,0.));
#122144=DIRECTION('ref_axis',(-0.668938718831625,-0.743317556935059,0.));
#122145=DIRECTION('center_axis',(-0.669130606358862,-0.743144825477391,
9.42249022928252E-17));
#122146=DIRECTION('ref_axis',(0.743144825477391,-0.669130606358862,-1.48947931215863E-30));
#122147=DIRECTION('center_axis',(-0.579501624400555,-0.643556859036987,
-0.500012436348903));
#122148=DIRECTION('ref_axis',(0.333837986843671,0.372243731496557,-0.866017784402655));
#122149=DIRECTION('center_axis',(0.354588864042412,0.393810830024454,0.848044673146741));
#122150=DIRECTION('ref_axis',(-1.10267543862293E-14,-0.906978000082675,
0.421177999622524));
#122151=DIRECTION('center_axis',(0.334568647739183,0.37157614236448,0.866022511471559));
#122152=DIRECTION('ref_axis',(0.576149740773813,0.64656900343761,-0.499999999999964));
#122153=DIRECTION('center_axis',(-0.334568664232057,-0.371576145565822,
-0.866022503726331));
#122154=DIRECTION('ref_axis',(4.82085454881383E-15,0.918982183096526,-0.394299058014526));
#122155=DIRECTION('center_axis',(0.354588823231024,0.393810822488337,0.848044693710595));
#122156=DIRECTION('ref_axis',(0.564077964596703,0.633246889649659,-0.529919264233216));
#122157=DIRECTION('center_axis',(0.354588820328813,0.393810781475714,0.848044713969321));
#122158=DIRECTION('ref_axis',(8.39746514209146E-15,-0.906978027661839,0.421177940232676));
#122159=DIRECTION('center_axis',(-0.669130606358845,-0.743144825477406,
3.65592620896146E-14));
#122160=DIRECTION('ref_axis',(0.743144825477406,-0.669130606358845,9.99649599890217E-31));
#122161=DIRECTION('center_axis',(0.669130606358875,0.743144825477379,0.));
#122162=DIRECTION('ref_axis',(-0.743144825477379,0.669130606358875,0.));
#122163=DIRECTION('center_axis',(-0.669130606358862,-0.743144825477391,
9.42249022928252E-17));
#122164=DIRECTION('ref_axis',(0.743144825477391,-0.669130606358862,-1.48947931215863E-30));
#122165=DIRECTION('center_axis',(-0.669130606358845,-0.743144825477406,
4.0439119200333E-15));
#122166=DIRECTION('ref_axis',(0.743144825477406,-0.669130606358845,-2.12202718326909E-31));
#122167=DIRECTION('center_axis',(-0.669130606358862,-0.743144825477391,
9.42249022928252E-17));
#122168=DIRECTION('ref_axis',(0.743144825477391,-0.669130606358862,-1.48947931215863E-30));
#122169=DIRECTION('center_axis',(0.579517695132025,0.643568108591859,-0.499979330205122));
#122170=DIRECTION('ref_axis',(0.335267672838056,0.37091183139964,0.866036951219472));
#122171=DIRECTION('center_axis',(-0.334568754912014,-0.371576246276117,
0.866022425483298));
#122172=DIRECTION('ref_axis',(3.2863782672971E-15,-0.918982131463647,-0.394299178353865));
#122173=DIRECTION('center_axis',(-0.334568760917623,-0.37157625294595,0.8660224203014));
#122174=DIRECTION('ref_axis',(-0.743144825474898,0.66913060636163,2.13302690841267E-12));
#122175=DIRECTION('center_axis',(0.371576139135906,0.334568658442567,0.866022508721797));
#122176=DIRECTION('ref_axis',(0.669130606361539,-0.743144825474981,-2.06309160956524E-12));
#122177=DIRECTION('center_axis',(0.643556859037152,0.579501624400958,0.500012436348223));
#122178=DIRECTION('ref_axis',(-0.37224373150869,-0.333837986829168,0.866017784403031));
#122179=DIRECTION('center_axis',(-0.371576145565853,-0.334568664232085,
-0.866022503726308));
#122180=DIRECTION('ref_axis',(-0.918982183096513,7.65889573873005E-15,0.394299058014558));
#122181=DIRECTION('center_axis',(-0.743144825477406,-0.669130606358845,
-3.65592620896146E-14));
#122182=DIRECTION('ref_axis',(0.669130606358845,-0.743144825477406,1.03271697859918E-30));
#122183=DIRECTION('center_axis',(0.743144825477398,0.669130606358854,-1.04647355694969E-16));
#122184=DIRECTION('ref_axis',(-0.669130606358854,0.743144825477398,-9.32318254549198E-33));
#122185=DIRECTION('center_axis',(0.743144825477406,0.669130606358845,0.));
#122186=DIRECTION('ref_axis',(-0.669130606358845,0.743144825477406,0.));
#122187=DIRECTION('center_axis',(0.743144825477398,0.669130606358854,-1.04647355694969E-16));
#122188=DIRECTION('ref_axis',(-0.669130606358854,0.743144825477398,-9.32318254549198E-33));
#122189=DIRECTION('center_axis',(-0.743144825477382,-0.669130606358872,
0.));
#122190=DIRECTION('ref_axis',(0.669130606358872,-0.743144825477382,0.));
#122191=DIRECTION('center_axis',(0.393810436983641,0.354588510146757,-0.848045003637576));
#122192=DIRECTION('ref_axis',(-0.906978223357763,4.7283308664863E-15,-0.421177518814568));
#122193=DIRECTION('center_axis',(-0.371576246276136,-0.334568754912019,
0.866022425483288));
#122194=DIRECTION('ref_axis',(0.918982131463639,-1.04034049828032E-14,0.394299178353883));
#122195=DIRECTION('center_axis',(-0.393810430453513,-0.354588475163147,
0.848045021297509));
#122196=DIRECTION('ref_axis',(-0.633098037500157,-0.564245025062705,-0.529919264233181));
#122197=DIRECTION('center_axis',(0.393810395274834,0.354588472591979,-0.848045038708656));
#122198=DIRECTION('ref_axis',(-0.906978247051303,9.86594956512546E-15,-0.421177467792077));
#122199=DIRECTION('center_axis',(-0.371576263603857,-0.334568756369017,
0.866022417485764));
#122200=DIRECTION('ref_axis',(-0.646617000434433,-0.576095872879835,-0.499999999999998));
#122201=DIRECTION('center_axis',(-0.6435681085917,-0.579517695132229,0.49997933020509));
#122202=DIRECTION('ref_axis',(-0.370911831392187,-0.335267672846279,-0.866036951219482));
#122203=DIRECTION('center_axis',(-0.668950377172403,0.743307065001336,0.));
#122204=DIRECTION('ref_axis',(-0.743307065001336,-0.668950377172402,0.));
#122205=DIRECTION('center_axis',(0.743144825477398,0.669130606358854,-1.04647355694969E-16));
#122206=DIRECTION('ref_axis',(-0.669130606358854,0.743144825477398,-9.32318254549198E-33));
#122207=DIRECTION('center_axis',(-0.743144825477382,-0.669130606358872,
0.));
#122208=DIRECTION('ref_axis',(0.669130606358872,-0.743144825477382,0.));
#122209=DIRECTION('center_axis',(-2.4546426258488E-16,-9.42249022928242E-17,
-1.));
#122210=DIRECTION('ref_axis',(-1.,2.34879036376888E-33,2.25664243350207E-16));
#122211=DIRECTION('center_axis',(-0.669310796197597,0.742982542253409,0.));
#122212=DIRECTION('ref_axis',(-0.742982542253409,-0.669310796197597,0.));
#122213=DIRECTION('center_axis',(-0.393810781475716,-0.35458882032887,-0.848044713969297));
#122214=DIRECTION('ref_axis',(-0.906978027661832,-3.75249855275816E-15,
0.421177940232692));
#122215=DIRECTION('center_axis',(-0.393810395274935,-0.354588472592007,
0.848045038708598));
#122216=DIRECTION('ref_axis',(0.90697824705125,-1.0449597276298E-14,0.42117746779219));
#122217=DIRECTION('center_axis',(-0.393810788842373,-0.35458886088878,-0.848044693589285));
#122218=DIRECTION('ref_axis',(0.633246889661538,0.564077964583415,-0.529919264233165));
#122219=DIRECTION('center_axis',(-0.393810830024481,-0.354588864042382,
-0.848044673146741));
#122220=DIRECTION('ref_axis',(-0.906978000082665,-2.2872769161124E-15,0.421177999622545));
#122221=DIRECTION('center_axis',(0.393810430611346,0.354588475224443,-0.848045021198586));
#122222=DIRECTION('ref_axis',(-0.627330796759002,-0.570650194806061,-0.52991926423326));
#122223=DIRECTION('center_axis',(-0.393810436983659,-0.354588510146774,
0.848045003637561));
#122224=DIRECTION('ref_axis',(0.906978223357753,-5.41285892759898E-15,0.42117751881459));
#122225=DIRECTION('center_axis',(-0.668938718831589,0.743317556935091,0.));
#122226=DIRECTION('ref_axis',(-0.743317556935091,-0.668938718831589,0.));
#122227=DIRECTION('center_axis',(-0.743144825477406,-0.669130606358845,
0.));
#122228=DIRECTION('ref_axis',(0.669130606358845,-0.743144825477406,0.));
#122229=DIRECTION('center_axis',(-2.4546426258488E-16,-9.42249022928242E-17,
-1.));
#122230=DIRECTION('ref_axis',(-1.,1.04182536618998E-33,2.40228573745067E-16));
#122231=DIRECTION('center_axis',(-0.669322449283883,0.742972044483925,0.));
#122232=DIRECTION('ref_axis',(-0.742972044483925,-0.669322449283883,0.));
#122233=DIRECTION('center_axis',(-0.743144825477398,-0.669130606358854,
1.04647355694969E-16));
#122234=DIRECTION('ref_axis',(0.669130606358854,-0.743144825477398,-1.33231393542051E-30));
#122235=DIRECTION('center_axis',(-0.643597063368147,-0.579456972967606,
-0.500012436348454));
#122236=DIRECTION('ref_axis',(0.370919252632461,0.335308969645089,-0.86601778440291));
#122237=DIRECTION('center_axis',(0.393810830024549,0.354588864042318,0.848044673146736));
#122238=DIRECTION('ref_axis',(0.906978000082638,-3.66139072703648E-15,-0.421177999622604));
#122239=DIRECTION('center_axis',(0.371576128828018,0.334568662772985,0.866022511471544));
#122240=DIRECTION('ref_axis',(0.640578396533018,0.582802983773409,-0.499999999999999));
#122241=DIRECTION('center_axis',(-0.371576145565821,-0.334568664232056,
-0.866022503726332));
#122242=DIRECTION('ref_axis',(-0.918982183096527,-5.2693457410403E-15,0.394299058014525));
#122243=DIRECTION('center_axis',(0.393810788647791,0.354588860814735,0.848044693710605));
#122244=DIRECTION('ref_axis',(0.627180210739902,0.570815694117418,-0.529919264233244));
#122245=DIRECTION('center_axis',(0.39381078147571,0.354588820328817,0.848044713969322));
#122246=DIRECTION('ref_axis',(0.906978027661841,-6.75609972193682E-15,-0.421177940232673));
#122247=DIRECTION('center_axis',(-0.743144825477406,-0.669130606358845,
0.));
#122248=DIRECTION('ref_axis',(0.669130606358845,-0.743144825477406,0.));
#122249=DIRECTION('center_axis',(0.743144825477406,0.669130606358845,0.));
#122250=DIRECTION('ref_axis',(-0.669130606358845,0.743144825477406,0.));
#122251=DIRECTION('center_axis',(-0.743144825477398,-0.669130606358854,
1.04647355694969E-16));
#122252=DIRECTION('ref_axis',(0.669130606358854,-0.743144825477398,-1.33231393542051E-30));
#122253=DIRECTION('center_axis',(-0.743144825477406,-0.669130606358845,
0.));
#122254=DIRECTION('ref_axis',(0.669130606358845,-0.743144825477406,0.));
#122255=DIRECTION('center_axis',(-0.743144825477398,-0.669130606358854,
1.04647355694969E-16));
#122256=DIRECTION('ref_axis',(0.669130606358854,-0.743144825477398,-1.33231393542051E-30));
#122257=DIRECTION('center_axis',(0.643614221961228,0.579466481046758,-0.499979330205289));
#122258=DIRECTION('ref_axis',(0.372201885192673,0.33383492295096,0.866036951219373));
#122259=DIRECTION('center_axis',(-0.371576246276125,-0.334568754912021,
0.866022425483293));
#122260=DIRECTION('ref_axis',(0.918982131463643,-6.34168247799913E-15,0.394299178353873));
#122261=DIRECTION('center_axis',(-0.371576252946094,-0.334568760917662,
0.866022420301323));
#122262=DIRECTION('ref_axis',(-0.669130606357769,0.743144825478375,8.3922370166019E-13));
#122263=DIRECTION('center_axis',(0.404512553894235,0.293895573516223,0.866022508719914));
#122264=DIRECTION('ref_axis',(0.587785252291253,-0.809016994375834,8.74191359985202E-13));
#122265=DIRECTION('center_axis',(0.700605801485921,0.509057044367645,0.500012436349285));
#122266=DIRECTION('ref_axis',(-0.405100113149077,-0.293099122184537,0.86601778440241));
#122267=DIRECTION('center_axis',(-0.404512560891477,-0.293895578600006,
-0.86602250372631));
#122268=DIRECTION('ref_axis',(-0.906035256115479,9.01705582438248E-15,0.423202214875771));
#122269=DIRECTION('center_axis',(-0.80901699437495,-0.58778525229247,0.));
#122270=DIRECTION('ref_axis',(0.58778525229247,-0.80901699437495,0.));
#122271=DIRECTION('center_axis',(0.809016994374951,0.587785252292469,-1.13923270769253E-16));
#122272=DIRECTION('ref_axis',(-0.587785252292469,0.80901699437495,3.40207274335237E-32));
#122273=DIRECTION('center_axis',(0.80901699437495,0.58778525229247,0.));
#122274=DIRECTION('ref_axis',(-0.58778525229247,0.80901699437495,0.));
#122275=DIRECTION('center_axis',(0.809016994374951,0.587785252292469,-1.13923270769253E-16));
#122276=DIRECTION('ref_axis',(-0.587785252292469,0.80901699437495,3.40207274335237E-32));
#122277=DIRECTION('center_axis',(-0.809016994374976,-0.587785252292434,
0.));
#122278=DIRECTION('ref_axis',(0.587785252292434,-0.809016994374976,0.));
#122279=DIRECTION('center_axis',(0.428717694262762,0.311481637390294,-0.848045003637592));
#122280=DIRECTION('ref_axis',(-0.89244205802627,-6.91749752624164E-15,-0.451162025292284));
#122281=DIRECTION('center_axis',(-0.404512670528675,-0.293895658256101,
0.866022425483297));
#122282=DIRECTION('ref_axis',(0.906035197473499,-2.43383441813702E-15,0.423202340422591));
#122283=DIRECTION('center_axis',(-0.428717684114261,-0.311481603277307,
0.848045021297515));
#122284=DIRECTION('ref_axis',(-0.688609525582324,-0.494977266823274,-0.529919264233192));
#122285=DIRECTION('center_axis',(0.428717648856936,0.31148160440103,-0.848045038708641));
#122286=DIRECTION('ref_axis',(-0.892442084777727,-1.51672008863495E-15,
-0.451161972375314));
#122287=DIRECTION('center_axis',(-0.404512687916182,-0.293895657890621,
0.866022417485751));
#122288=DIRECTION('ref_axis',(-0.703293181145105,-0.505350078019966,-0.500000000000014));
#122289=DIRECTION('center_axis',(-0.700618669263857,-0.509071851162881,
0.4999793302053));
#122290=DIRECTION('ref_axis',(-0.403924952205241,-0.294660197700078,-0.866036951219372));
#122291=DIRECTION('center_axis',(-0.587589051772227,0.809159506053914,0.));
#122292=DIRECTION('ref_axis',(-0.809159506053914,-0.587589051772227,0.));
#122293=DIRECTION('center_axis',(0.809016994374951,0.587785252292469,-1.13923270769253E-16));
#122294=DIRECTION('ref_axis',(-0.587785252292469,0.80901699437495,3.40207274335237E-32));
#122295=DIRECTION('center_axis',(-0.80901699437495,-0.58778525229247,0.));
#122296=DIRECTION('ref_axis',(0.58778525229247,-0.80901699437495,0.));
#122297=DIRECTION('center_axis',(-2.54740177659163E-16,-8.27701011433311E-17,
-1.));
#122298=DIRECTION('ref_axis',(-1.,2.9359879547111E-33,2.25664243350207E-16));
#122299=DIRECTION('center_axis',(-0.587981418248456,0.808874435122371,0.));
#122300=DIRECTION('ref_axis',(-0.808874435122371,-0.587981418248456,0.));
#122301=DIRECTION('center_axis',(-0.428718069290576,-0.31148190986395,-0.848044713969298));
#122302=DIRECTION('ref_axis',(-0.892441837073373,-7.49535211974272E-15,
0.451162462358188));
#122303=DIRECTION('center_axis',(-0.428717648856939,-0.311481604401032,
0.848045038708639));
#122304=DIRECTION('ref_axis',(0.892442084777726,6.53865308856261E-16,0.451161972375317));
#122305=DIRECTION('center_axis',(-0.428718080852829,-0.3114819494368,-0.848044693589269));
#122306=DIRECTION('ref_axis',(0.688740099746409,0.4947955622233,-0.52991926423318));
#122307=DIRECTION('center_axis',(-0.428718122142682,-0.311481948263282,
-0.848044673146741));
#122308=DIRECTION('ref_axis',(-0.892441805934785,-7.52869580075203E-16,
0.451162523953242));
#122309=DIRECTION('center_axis',(0.428717684276781,0.311481603322996,-0.848045021198575));
#122310=DIRECTION('ref_axis',(-0.683543400925772,-0.501950189207415,-0.529919264233213));
#122311=DIRECTION('center_axis',(-0.428717694262774,-0.311481637390302,
0.848045003637583));
#122312=DIRECTION('ref_axis',(0.892442058026264,2.33582750500883E-15,0.451162025292297));
#122313=DIRECTION('center_axis',(-0.587576360591347,0.809168721883284,4.42105189882562E-14));
#122314=DIRECTION('ref_axis',(-0.809168721883284,-0.587576360591347,9.93302310845174E-28));
#122315=DIRECTION('center_axis',(-0.80901699437495,-0.58778525229247,4.42022290584717E-14));
#122316=DIRECTION('ref_axis',(0.58778525229247,-0.80901699437495,3.78613142600248E-30));
#122317=DIRECTION('center_axis',(-2.54740177659163E-16,-8.27701011433311E-17,
-1.));
#122318=DIRECTION('ref_axis',(-1.,1.66692058590397E-33,2.40228573745067E-16));
#122319=DIRECTION('center_axis',(-0.587994104813612,0.80886521293998,-1.20677258718682E-14));
#122320=DIRECTION('ref_axis',(-0.80886521293998,-0.587994104813612,1.51939136976245E-28));
#122321=DIRECTION('center_axis',(-0.809016994374951,-0.587785252292469,
1.13923270769253E-16));
#122322=DIRECTION('ref_axis',(0.587785252292469,-0.809016994374951,1.93507240347744E-30));
#122323=DIRECTION('center_axis',(-0.700641118228684,-0.509008435041272,
-0.500012436349432));
#122324=DIRECTION('ref_axis',(0.40393664947362,0.294700492552831,-0.866017784402344));
#122325=DIRECTION('center_axis',(0.428718122142701,0.311481948263287,0.848044673146729));
#122326=DIRECTION('ref_axis',(0.892441805934776,-6.12251068898412E-15,-0.45116252395326));
#122327=DIRECTION('center_axis',(0.40451254409338,0.293895578897687,0.866022511471553));
#122328=DIRECTION('ref_axis',(0.69798874133117,0.51265165265994,-0.499999999999961));
#122329=DIRECTION('center_axis',(-0.404512560891434,-0.293895578599982,
-0.866022503726338));
#122330=DIRECTION('ref_axis',(-0.9060352561155,-6.08383211411716E-15,0.423202214875727));
#122331=DIRECTION('center_axis',(0.428718080657259,0.311481949375618,0.848044693710609));
#122332=DIRECTION('ref_axis',(0.683410939236706,0.502130522400415,-0.529919264233232));
#122333=DIRECTION('center_axis',(0.42871806929053,0.311481909863937,0.848044713969325));
#122334=DIRECTION('ref_axis',(0.892441837073399,2.26869662838081E-15,-0.451162462358136));
#122335=DIRECTION('center_axis',(-0.80901699437495,-0.58778525229247,0.));
#122336=DIRECTION('ref_axis',(0.58778525229247,-0.80901699437495,0.));
#122337=DIRECTION('center_axis',(0.809016994374976,0.587785252292434,0.));
#122338=DIRECTION('ref_axis',(-0.587785252292434,0.809016994374976,0.));
#122339=DIRECTION('center_axis',(-0.809016994374951,-0.587785252292469,
1.13923270769253E-16));
#122340=DIRECTION('ref_axis',(0.587785252292469,-0.809016994374951,1.93507240347744E-30));
#122341=DIRECTION('center_axis',(-0.80901699437495,-0.58778525229247,-3.2114799243612E-14));
#122342=DIRECTION('ref_axis',(0.58778525229247,-0.80901699437495,-4.13565546558353E-30));
#122343=DIRECTION('center_axis',(-0.809016994374951,-0.587785252292469,
1.13923270769253E-16));
#122344=DIRECTION('ref_axis',(0.587785252292469,-0.809016994374951,1.93507240347744E-30));
#122345=DIRECTION('center_axis',(0.700659176689548,0.509016097474346,-0.499979330205472));
#122346=DIRECTION('ref_axis',(0.405058175792506,0.293100449243017,0.866036951219282));
#122347=DIRECTION('center_axis',(-0.404512670528692,-0.293895658256113,
0.866022425483285));
#122348=DIRECTION('ref_axis',(0.906035197473489,5.57797719073592E-15,0.423202340422612));
#122349=DIRECTION('center_axis',(-0.404512677787103,-0.29389566352967,0.866022420303287));
#122350=DIRECTION('ref_axis',(-0.587785252285307,0.809016994380154,5.10527751848768E-12));
#122351=DIRECTION('center_axis',(0.433017044457923,0.250002507181456,0.866022508721287));
#122352=DIRECTION('ref_axis',(0.500000000003501,-0.866025403782417,-2.34283284476153E-12));
#122353=DIRECTION('center_axis',(0.749978760162693,0.43303512882966,0.500012436349646));
#122354=DIRECTION('ref_axis',(-0.433518133171605,-0.249149002226608,0.866017784402198));
#122355=DIRECTION('center_axis',(-0.433017051950273,-0.250002511507195,
-0.866022503726312));
#122356=DIRECTION('ref_axis',(-0.894424794863786,-9.37039710670596E-16,
0.447218387740122));
#122357=DIRECTION('center_axis',(-0.86602540378444,-0.499999999999998,-6.09762352041363E-14));
#122358=DIRECTION('ref_axis',(0.499999999999998,-0.86602540378444,-8.28350179725319E-28));
#122359=DIRECTION('center_axis',(0.866025403784442,0.499999999999995,-1.21951018649011E-16));
#122360=DIRECTION('ref_axis',(-0.499999999999995,0.866025403784441,2.67488359253536E-33));
#122361=DIRECTION('center_axis',(0.866025403784433,0.50000000000001,1.36592399683214E-14));
#122362=DIRECTION('ref_axis',(-0.50000000000001,0.866025403784433,-1.33215113601878E-31));
#122363=DIRECTION('center_axis',(0.866025403784442,0.499999999999995,-1.21951018649011E-16));
#122364=DIRECTION('ref_axis',(-0.499999999999995,0.866025403784441,2.67488359253536E-33));
#122365=DIRECTION('center_axis',(-0.86602540378444,-0.499999999999998,0.));
#122366=DIRECTION('ref_axis',(0.499999999999998,-0.86602540378444,0.));
#122367=DIRECTION('center_axis',(0.45892783076861,0.264962106632875,-0.848045003637594));
#122368=DIRECTION('ref_axis',(-0.879478602053341,-1.44813680787485E-15,
-0.475938429348064));
#122369=DIRECTION('center_axis',(-0.43301716931323,-0.250002579266683,0.866022425483292));
#122370=DIRECTION('ref_axis',(0.894424730216411,5.21485729842101E-15,0.447218517033117));
#122371=DIRECTION('center_axis',(-0.458927817107387,-0.264962073772023,
0.8480450212975));
#122372=DIRECTION('ref_axis',(-0.736576463613238,-0.420286434048956,-0.529919264233174));
#122373=DIRECTION('center_axis',(0.45892778216319,0.264962078570523,-0.848045038708655));
#122374=DIRECTION('ref_axis',(-0.879478631391258,-5.23853710775596E-15,
-0.475938375135017));
#122375=DIRECTION('center_axis',(-0.433017186566647,-0.250002577086723,
0.866022417485773));
#122376=DIRECTION('ref_axis',(-0.752263934577883,-0.429067561968314,-0.49999999999997));
#122377=DIRECTION('center_axis',(-0.74999310518157,-0.433048509462502,0.499979330205172));
#122378=DIRECTION('ref_axis',(-0.43251258670403,-0.25082436377896,-0.866036951219444));
#122379=DIRECTION('center_axis',(-0.499789977759954,0.866146626230631,0.));
#122380=DIRECTION('ref_axis',(-0.866146626230631,-0.499789977759954,0.));
#122381=DIRECTION('center_axis',(0.866025403784442,0.499999999999995,-1.21951018649011E-16));
#122382=DIRECTION('ref_axis',(-0.499999999999995,0.866025403784441,2.67488359253536E-33));
#122383=DIRECTION('center_axis',(-0.866025403784457,-0.499999999999969,
0.));
#122384=DIRECTION('ref_axis',(0.499999999999969,-0.866025403784457,0.));
#122385=DIRECTION('center_axis',(-2.62767925538921E-16,-7.04084534449545E-17,
-1.));
#122386=DIRECTION('ref_axis',(-1.,2.9359879547111E-33,2.25664243350207E-16));
#122387=DIRECTION('center_axis',(-0.500209992837911,0.865904130412309,0.));
#122388=DIRECTION('ref_axis',(-0.865904130412309,-0.500209992837911,0.));
#122389=DIRECTION('center_axis',(-0.458928232223204,-0.264962338412793,
-0.848044713969322));
#122390=DIRECTION('ref_axis',(-0.879478359737744,-1.81174991810093E-15,
0.475938877118698));
#122391=DIRECTION('center_axis',(-0.45892778216322,-0.264962078570532,0.848045038708636));
#122392=DIRECTION('ref_axis',(0.879478631391242,-3.91934596708905E-15,0.475938375135046));
#122393=DIRECTION('center_axis',(-0.458928247862902,-0.264962376552842,
-0.848044693589292));
#122394=DIRECTION('ref_axis',(0.73668732915428,0.420092076166699,-0.529919264233228));
#122395=DIRECTION('center_axis',(-0.458928288799617,-0.264962371077283,
-0.848044673146739));
#122396=DIRECTION('ref_axis',(-0.879478325588526,-1.55521142283728E-15,
0.475938940222381));
#122397=DIRECTION('center_axis',(0.458927817276937,0.264962073795002,-0.848045021198567));
#122398=DIRECTION('ref_axis',(-0.732266960571272,-0.427750712273227,-0.529919264233202));
#122399=DIRECTION('center_axis',(-0.458927830768617,-0.264962106632871,
0.848045003637592));
#122400=DIRECTION('ref_axis',(0.879478602053337,-4.79936374009227E-16,0.47593842934807));
#122401=DIRECTION('center_axis',(-0.499776392786171,0.866154464985111,0.));
#122402=DIRECTION('ref_axis',(-0.86615446498511,-0.499776392786171,0.));
#122403=DIRECTION('center_axis',(-0.866025403784433,-0.50000000000001,-1.36592399683221E-14));
#122404=DIRECTION('ref_axis',(0.50000000000001,-0.866025403784433,1.85779939211817E-28));
#122405=DIRECTION('center_axis',(-2.62767925538921E-16,-7.04084534449545E-17,
-1.));
#122406=DIRECTION('ref_axis',(-1.,1.97946819576097E-33,2.40228573745067E-16));
#122407=DIRECTION('center_axis',(-0.500223573885299,0.865896284857153,3.67572504895883E-15));
#122408=DIRECTION('ref_axis',(-0.865896284857153,-0.500223573885299,4.46977350782273E-29));
#122409=DIRECTION('center_axis',(-0.866025403784442,-0.499999999999995,
1.21951018649011E-16));
#122410=DIRECTION('ref_axis',(0.499999999999995,-0.866025403784442,2.10506284754485E-30));
#122411=DIRECTION('center_axis',(-0.750008802379564,-0.432983094185751,
-0.500012436347842));
#122412=DIRECTION('ref_axis',(0.432528431882832,0.250863215139549,-0.866017784403315));
#122413=DIRECTION('center_axis',(0.458928288799688,0.264962371077179,0.848044673146733));
#122414=DIRECTION('ref_axis',(0.879478325588494,-3.39387948166673E-15,-0.475938940222439));
#122415=DIRECTION('center_axis',(0.433017035278663,0.250002513553368,0.866022511471541));
#122416=DIRECTION('ref_axis',(0.747751775424751,0.436883602746915,-0.500000000000008));
#122417=DIRECTION('center_axis',(-0.43301705195022,-0.250002511507164,-0.866022503726347));
#122418=DIRECTION('ref_axis',(-0.894424794863815,-4.94594594567521E-15,
0.447218387740065));
#122419=DIRECTION('center_axis',(0.458928247651838,0.264962376530043,0.848044693710635));
#122420=DIRECTION('ref_axis',(0.732154074451793,0.427943903634897,-0.529919264233113));
#122421=DIRECTION('center_axis',(0.458928232223194,0.264962338412787,0.848044713969329));
#122422=DIRECTION('ref_axis',(0.87947835973775,5.0288465242107E-15,-0.475938877118687));
#122423=DIRECTION('center_axis',(-0.866025403784433,-0.50000000000001,0.));
#122424=DIRECTION('ref_axis',(0.50000000000001,-0.866025403784433,0.));
#122425=DIRECTION('center_axis',(0.866025403784433,0.50000000000001,0.));
#122426=DIRECTION('ref_axis',(-0.50000000000001,0.866025403784433,0.));
#122427=DIRECTION('center_axis',(-0.866025403784442,-0.499999999999995,
1.21951018649011E-16));
#122428=DIRECTION('ref_axis',(0.499999999999995,-0.866025403784442,2.10506284754485E-30));
#122429=DIRECTION('center_axis',(-0.866025403784433,-0.50000000000001,0.));
#122430=DIRECTION('ref_axis',(0.50000000000001,-0.866025403784433,0.));
#122431=DIRECTION('center_axis',(-0.866025403784442,-0.499999999999995,
1.21951018649011E-16));
#122432=DIRECTION('ref_axis',(0.499999999999995,-0.866025403784442,2.10506284754485E-30));
#122433=DIRECTION('center_axis',(0.750027562855788,0.432988827019605,-0.499979330205554));
#122434=DIRECTION('ref_axis',(0.433476564278272,0.24915470564377,0.866036951219214));
#122435=DIRECTION('center_axis',(-0.433017169313196,-0.25000257926671,0.866022425483301));
#122436=DIRECTION('ref_axis',(0.894424730216427,1.90878151355965E-15,0.447218517033085));
#122437=DIRECTION('center_axis',(-0.433017177086037,-0.250002583754367,
0.866022420301334));
#122438=DIRECTION('ref_axis',(-0.500000000002471,0.866025403783012,-1.64347974908538E-12));
#122439=DIRECTION('center_axis',(0.456777309663355,0.203370361060154,0.866022508725362));
#122440=DIRECTION('ref_axis',(0.406736643069877,-0.913545457645238,3.70657136640272E-12));
#122441=DIRECTION('center_axis',(0.791134794599999,0.352268789802096,0.500012436349921));
#122442=DIRECTION('ref_axis',(0.457186437788949,0.202469153702906,-0.866017784402076));
#122443=DIRECTION('center_axis',(-0.456777317573304,-0.203370364581847,
-0.866022503726308));
#122444=DIRECTION('ref_axis',(-0.884507036382085,-1.36888255260538E-16,
0.466526850878469));
#122445=DIRECTION('center_axis',(-0.913545457642594,-0.406736643075817,
0.));
#122446=DIRECTION('ref_axis',(0.406736643075817,-0.913545457642593,0.));
#122447=DIRECTION('center_axis',(0.913545457642603,0.406736643075795,-1.28642645648559E-16));
#122448=DIRECTION('ref_axis',(-0.406736643075795,0.913545457642603,1.45091416765994E-32));
#122449=DIRECTION('center_axis',(0.913545457642598,0.406736643075807,0.));
#122450=DIRECTION('ref_axis',(-0.406736643075807,0.913545457642598,0.));
#122451=DIRECTION('center_axis',(0.913545457642603,0.406736643075795,-1.28642645648559E-16));
#122452=DIRECTION('ref_axis',(-0.406736643075795,0.913545457642603,1.45091416765994E-32));
#122453=DIRECTION('center_axis',(-0.913545457642603,-0.406736643075797,
0.));
#122454=DIRECTION('ref_axis',(0.406736643075797,-0.913545457642603,0.));
#122455=DIRECTION('center_axis',(0.484109857923767,0.215539595588305,-0.848045003637578));
#122456=DIRECTION('ref_axis',(-0.868458021515997,-1.32153558682304E-15,
-0.49576271024001));
#122457=DIRECTION('center_axis',(-0.456777441376074,-0.20337041970247,0.866022425483295));
#122458=DIRECTION('ref_axis',(0.884506966812058,2.53897267290044E-15,0.466526982779059));
#122459=DIRECTION('center_axis',(-0.484109840902121,-0.215539564336208,
0.848045021297502));
#122460=DIRECTION('ref_axis',(-0.776473315744763,-0.340990855201216,-0.52991926423322));
#122461=DIRECTION('center_axis',(0.484109806651284,0.215539572760325,-0.848045038708649));
#122462=DIRECTION('ref_axis',(-0.86845805294996,4.78172523366081E-17,-0.4957626551752));
#122463=DIRECTION('center_axis',(-0.456777458307931,-0.203370415729123,
0.866022417485777));
#122464=DIRECTION('ref_axis',(-0.792992726927602,-0.348084091908765,-0.499999999999977));
#122465=DIRECTION('center_axis',(-0.791150459692809,-0.352280597671166,
0.499979330205063));
#122466=DIRECTION('ref_axis',(0.456361522800706,0.204240445625793,0.866036951219518));
#122467=DIRECTION('center_axis',(-0.406515100163568,0.913644062717536,0.));
#122468=DIRECTION('ref_axis',(-0.913644062717536,-0.406515100163568,0.));
#122469=DIRECTION('center_axis',(0.913545457642603,0.406736643075795,-1.28642645648559E-16));
#122470=DIRECTION('ref_axis',(-0.406736643075795,0.913545457642603,1.45091416765994E-32));
#122471=DIRECTION('center_axis',(-0.913545457642603,-0.406736643075797,
0.));
#122472=DIRECTION('ref_axis',(0.406736643075797,-0.913545457642603,0.));
#122473=DIRECTION('center_axis',(-2.6945955253847E-16,-5.7275395996719E-17,
-1.));
#122474=DIRECTION('ref_axis',(-1.,2.74025542439703E-33,2.25664243350207E-16));
#122475=DIRECTION('center_axis',(-0.406958162070199,0.913446798847336,0.));
#122476=DIRECTION('ref_axis',(-0.913446798847336,-0.406958162070199,0.));
#122477=DIRECTION('center_axis',(-0.484110281406756,-0.215539784135086,
-0.8480447139693));
#122478=DIRECTION('ref_axis',(-0.868457761888263,-2.07453665764236E-15,
0.495763165045598));
#122479=DIRECTION('center_axis',(-0.484109806651301,-0.215539572760332,
0.848045038708637));
#122480=DIRECTION('ref_axis',(0.86845805294995,-4.51368237441253E-15,0.495762655175218));
#122481=DIRECTION('center_axis',(-0.484110300944432,-0.215539820438308,
-0.848044693589267));
#122482=DIRECTION('ref_axis',(0.776563258047416,0.340785973369427,-0.52991926423318));
#122483=DIRECTION('center_axis',(-0.484110341087582,-0.215539810706759,
-0.848044673146739));
#122484=DIRECTION('ref_axis',(-0.868457725299282,6.1582383090763E-16,0.495763229140682));
#122485=DIRECTION('center_axis',(0.484109841073423,0.215539564340702,-0.848045021198572));
#122486=DIRECTION('ref_axis',(-0.772967650153761,-0.348864709035361,-0.52991926423319));
#122487=DIRECTION('center_axis',(-0.484109857923745,-0.215539595588295,
0.848045003637594));
#122488=DIRECTION('ref_axis',(0.868458021516011,-2.89436985092629E-15,0.495762710239986));
#122489=DIRECTION('center_axis',(-0.406500770236713,0.913650438514074,0.));
#122490=DIRECTION('ref_axis',(-0.913650438514073,-0.406500770236713,0.));
#122491=DIRECTION('center_axis',(-0.913545457642598,-0.406736643075807,
0.));
#122492=DIRECTION('ref_axis',(0.406736643075807,-0.913545457642598,0.));
#122493=DIRECTION('center_axis',(-2.6945955253847E-16,-5.7275395996719E-17,
-1.));
#122494=DIRECTION('ref_axis',(-1.,1.97946819576097E-33,2.40228573745067E-16));
#122495=DIRECTION('center_axis',(-0.406972488803014,0.913440415876964,0.));
#122496=DIRECTION('ref_axis',(-0.913440415876964,-0.406972488803014,0.));
#122497=DIRECTION('center_axis',(-0.913545457642603,-0.406736643075795,
1.28642645648559E-16));
#122498=DIRECTION('ref_axis',(0.406736643075795,-0.913545457642603,1.67756362845828E-30));
#122499=DIRECTION('center_axis',(-0.791159233141683,-0.352213899942492,
-0.500012436347302));
#122500=DIRECTION('ref_axis',(0.456381342239291,0.204277427907535,-0.866017784403614));
#122501=DIRECTION('center_axis',(0.484110341087604,0.215539810706711,0.848044673146739));
#122502=DIRECTION('ref_axis',(0.868457725299272,5.31136787545075E-15,-0.4957632291407));
#122503=DIRECTION('center_axis',(0.456777301208103,0.203370368356831,0.866022511471525));
#122504=DIRECTION('ref_axis',(0.789322284583639,0.356328964665585,-0.500000000000017));
#122505=DIRECTION('center_axis',(-0.456777317573169,-0.203370364581866,
-0.866022503726375));
#122506=DIRECTION('ref_axis',(-0.884507036382156,-6.36152350155046E-15,
0.466526850878334));
#122507=DIRECTION('center_axis',(0.48411030073694,0.215539820426895,0.848044693710615));
#122508=DIRECTION('ref_axis',(0.77287557643918,0.349068641872047,-0.529919264233156));
#122509=DIRECTION('center_axis',(0.484110281406739,0.215539784135021,0.848044713969326));
#122510=DIRECTION('ref_axis',(0.868457761888278,-1.94242193778803E-15,-0.495763165045573));
#122511=DIRECTION('center_axis',(-0.913545457642598,-0.406736643075807,
0.));
#122512=DIRECTION('ref_axis',(0.406736643075807,-0.913545457642598,0.));
#122513=DIRECTION('center_axis',(0.913545457642598,0.406736643075807,0.));
#122514=DIRECTION('ref_axis',(-0.406736643075807,0.913545457642598,0.));
#122515=DIRECTION('center_axis',(-0.913545457642603,-0.406736643075795,
1.28642645648559E-16));
#122516=DIRECTION('ref_axis',(0.406736643075795,-0.913545457642603,1.67756362845828E-30));
#122517=DIRECTION('center_axis',(-0.913545457642598,-0.406736643075807,
1.11114268233636E-14));
#122518=DIRECTION('ref_axis',(0.406736643075807,-0.913545457642598,-1.92826049468501E-31));
#122519=DIRECTION('center_axis',(-0.913545457642603,-0.406736643075795,
1.28642645648559E-16));
#122520=DIRECTION('ref_axis',(0.406736643075795,-0.913545457642603,1.67756362845828E-30));
#122521=DIRECTION('center_axis',(0.791178490090852,0.352217640366497,-0.499979330204976));
#122522=DIRECTION('ref_axis',(0.457145692795309,0.202479170980695,0.866036951219558));
#122523=DIRECTION('center_axis',(-0.456777441376052,-0.203370419702461,
0.866022425483308));
#122524=DIRECTION('ref_axis',(0.884506966812071,-1.93472172084304E-15,0.466526982779036));
#122525=DIRECTION('center_axis',(-0.456777449576467,-0.203370423353516,
0.86602242030067));
#122526=DIRECTION('ref_axis',(-0.406736643078774,0.913545457641277,-1.88825332874541E-12));
#122527=DIRECTION('center_axis',(0.475533027092593,0.154510046711641,0.866022508719792));
#122528=DIRECTION('ref_axis',(0.309016994372452,-0.951056516295964,1.53857679358147E-12));
#122529=DIRECTION('center_axis',(0.823622990673448,0.267642920194726,0.500012436349103));
#122530=DIRECTION('ref_axis',(0.475845712132185,0.153571010753556,-0.866017784402575));
#122531=DIRECTION('center_axis',(-0.475533035318161,-0.154510049384248,
-0.866022503726303));
#122532=DIRECTION('ref_axis',(-0.876548788012425,-4.15617318960849E-15,
0.481313018974086));
#122533=DIRECTION('center_axis',(-0.951056516295146,-0.309016994374972,
0.));
#122534=DIRECTION('ref_axis',(0.309016994374972,-0.951056516295146,0.));
#122535=DIRECTION('center_axis',(0.951056516295156,0.309016994374942,-1.33924836902178E-16));
#122536=DIRECTION('ref_axis',(-0.309016994374942,0.951056516295155,-1.29861735441449E-32));
#122537=DIRECTION('center_axis',(0.951056516295148,0.309016994374964,-1.68837491218278E-14));
#122538=DIRECTION('ref_axis',(-0.309016994374964,0.951056516295148,-1.43380940262431E-28));
#122539=DIRECTION('center_axis',(0.951056516295156,0.309016994374942,-1.33924836902178E-16));
#122540=DIRECTION('ref_axis',(-0.309016994374942,0.951056516295155,5.50275392197254E-33));
#122541=DIRECTION('center_axis',(-0.951056516295146,-0.309016994374972,
0.));
#122542=DIRECTION('ref_axis',(0.309016994374972,-0.951056516295146,0.));
#122543=DIRECTION('center_axis',(0.503987876168977,0.163755587629901,-0.848045003637584));
#122544=DIRECTION('ref_axis',(-0.859649462041493,1.86435088897448E-15,-0.510884333691856));
#122545=DIRECTION('center_axis',(-0.475533164204401,-0.15451009126198,0.866022425483292));
#122546=DIRECTION('ref_axis',(0.876548714628841,-1.25657155782984E-15,0.481313152617426));
#122547=DIRECTION('center_axis',(-0.503987855974141,-0.163755558327407,
0.848045021297495));
#122548=DIRECTION('ref_axis',(-0.807862963766476,-0.257959309134166,-0.529919264233212));
#122549=DIRECTION('center_axis',(0.503987822791196,0.163755570286409,-0.848045038708654));
#122550=DIRECTION('ref_axis',(-0.859649495083708,-1.81880948564364E-15,
-0.510884278092727));
#122551=DIRECTION('center_axis',(-0.475533180627884,-0.154510085541378,
0.866022417485786));
#122552=DIRECTION('ref_axis',(-0.825033325010246,-0.263286939711361,-0.499999999999964));
#122553=DIRECTION('center_axis',(-0.823639804208727,-0.267653025932132,
0.499979330205143));
#122554=DIRECTION('ref_axis',(0.475210466540287,0.15541882644351,0.866036951219453));
#122555=DIRECTION('center_axis',(-0.308786358060986,0.951131423661017,0.));
#122556=DIRECTION('ref_axis',(-0.951131423661017,-0.308786358060986,0.));
#122557=DIRECTION('center_axis',(0.951056516295156,0.309016994374942,-1.33924836902178E-16));
#122558=DIRECTION('ref_axis',(-0.309016994374942,0.951056516295155,-1.29861735441449E-32));
#122559=DIRECTION('center_axis',(-0.951056516295162,-0.309016994374922,
0.));
#122560=DIRECTION('ref_axis',(0.309016994374922,-0.951056516295162,0.));
#122561=DIRECTION('center_axis',(-2.74741743792088E-16,-4.35148173242961E-17,
-1.));
#122562=DIRECTION('ref_axis',(-1.,2.34879036376888E-33,2.25664243350207E-16));
#122563=DIRECTION('center_axis',(-0.309247612517378,0.95098155300316,0.));
#122564=DIRECTION('ref_axis',(-0.95098155300316,-0.309247612517378,0.));
#122565=DIRECTION('center_axis',(-0.503988317040574,-0.163755730877723,
-0.848044713969324));
#122566=DIRECTION('ref_axis',(-0.859649189130472,-1.11108923047349E-15,
0.510884792910616));
#122567=DIRECTION('center_axis',(-0.503987822791213,-0.163755570286414,
0.848045038708643));
#122568=DIRECTION('ref_axis',(0.859649495083697,-1.4932809657743E-15,0.510884278092744));
#122569=DIRECTION('center_axis',(-0.503988340268045,-0.163755764933357,
-0.84804469358929));
#122570=DIRECTION('ref_axis',(0.80793099735763,0.257746148183087,-0.529919264233229));
#122571=DIRECTION('center_axis',(-0.503988379172003,-0.163755751065511,
-0.848044673146732));
#122572=DIRECTION('ref_axis',(-0.859649150669465,1.72876348210857E-15,0.510884857627693));
#122573=DIRECTION('center_axis',(0.503987856145422,0.163755558312599,-0.848045021198562));
#122574=DIRECTION('ref_axis',(-0.805199544416579,-0.266156471020048,-0.52991926423323));
#122575=DIRECTION('center_axis',(-0.503987876169011,-0.163755587629912,
0.848045003637562));
#122576=DIRECTION('ref_axis',(0.859649462041472,-9.84505827227631E-16,0.510884333691892));
#122577=DIRECTION('center_axis',(-0.308771440182777,0.951136266645034,0.));
#122578=DIRECTION('ref_axis',(-0.951136266645034,-0.308771440182777,0.));
#122579=DIRECTION('center_axis',(-0.951056516295148,-0.309016994374964,
5.19628367180465E-14));
#122580=DIRECTION('ref_axis',(0.309016994374964,-0.951056516295148,4.387849755876E-28));
#122581=DIRECTION('center_axis',(-2.74741743792088E-16,-4.35148173242961E-17,
-1.));
#122582=DIRECTION('ref_axis',(-1.,1.71901185421347E-33,2.40228573745067E-16));
#122583=DIRECTION('center_axis',(-0.309262527968948,0.950976702550728,-9.08207363789677E-15));
#122584=DIRECTION('ref_axis',(-0.950976702550728,-0.309262527968948,9.18332529948884E-29));
#122585=DIRECTION('center_axis',(-0.951056516295156,-0.309016994374942,
1.33924836902178E-16));
#122586=DIRECTION('ref_axis',(0.309016994374942,-0.951056516295156,3.08051195631577E-30));
#122587=DIRECTION('center_axis',(-0.823641557783683,-0.267585776505055,
-0.500012436349192));
#122588=DIRECTION('ref_axis',(0.475234043096222,0.15545353447593,-0.866017784402468));
#122589=DIRECTION('center_axis',(0.503988379172001,0.163755751065462,0.848044673146743));
#122590=DIRECTION('ref_axis',(0.859649150669468,-6.63213536595391E-16,-0.510884857627688));
#122591=DIRECTION('center_axis',(0.475533019435078,0.154510054855637,0.866022511471535));
#122592=DIRECTION('ref_axis',(0.822244813610695,0.271870311895752,-0.500000000000019));
#122593=DIRECTION('center_axis',(-0.475533035318099,-0.154510049384278,
-0.866022503726331));
#122594=DIRECTION('ref_axis',(-0.876548788012458,-3.21789385138784E-15,
0.481313018974027));
#122595=DIRECTION('center_axis',(0.503988340058086,0.163755764951276,0.848044693710607));
#122596=DIRECTION('ref_axis',(0.805129291880749,0.266368911005196,-0.529919264233251));
#122597=DIRECTION('center_axis',(0.503988317040564,0.16375573087773,0.848044713969329));
#122598=DIRECTION('ref_axis',(0.859649189130477,2.91164143962136E-15,-0.510884792910607));
#122599=DIRECTION('center_axis',(-0.951056516295148,-0.309016994374964,
5.19628367180465E-14));
#122600=DIRECTION('ref_axis',(0.309016994374964,-0.951056516295148,4.387849755876E-28));
#122601=DIRECTION('center_axis',(0.951056516295165,0.309016994374914,0.));
#122602=DIRECTION('ref_axis',(-0.309016994374914,0.951056516295164,0.));
#122603=DIRECTION('center_axis',(-0.951056516295156,-0.309016994374942,
1.33924836902178E-16));
#122604=DIRECTION('ref_axis',(0.309016994374942,-0.951056516295156,3.08051195631577E-30));
#122605=DIRECTION('center_axis',(-0.951056516295148,-0.309016994374964,
5.19628367180436E-14));
#122606=DIRECTION('ref_axis',(0.309016994374964,-0.951056516295148,4.43497354731716E-28));
#122607=DIRECTION('center_axis',(-0.951056516295156,-0.309016994374942,
1.33924836902178E-16));
#122608=DIRECTION('ref_axis',(0.309016994374942,-0.951056516295156,3.08051195631577E-30));
#122609=DIRECTION('center_axis',(0.823661100222813,0.267587483540049,-0.499979330205209));
#122610=DIRECTION('ref_axis',(0.475806237445136,0.153585232137957,0.866036951219423));
#122611=DIRECTION('center_axis',(-0.475533164204424,-0.154510091261983,
0.866022425483279));
#122612=DIRECTION('ref_axis',(0.876548714628828,1.92992104204874E-15,0.48131315261745));
#122613=DIRECTION('center_axis',(-0.475533172739555,-0.154510094035192,
0.866022420301858));
#122614=DIRECTION('ref_axis',(-0.30901699437591,0.951056516294841,-5.94450122003489E-13));
#122615=DIRECTION('center_axis',(0.489078705152277,0.103956887953192,0.866022508722296));
#122616=DIRECTION('ref_axis',(0.207911690817373,-0.978147600733888,2.09805926398475E-13));
#122617=DIRECTION('center_axis',(0.847087400905789,0.180084698747132,0.500012436349167));
#122618=DIRECTION('ref_axis',(0.489291521299429,0.102990311598153,-0.866017784402495));
#122619=DIRECTION('center_axis',(-0.48907871361637,-0.103956889752269,-0.866022503726313));
#122620=DIRECTION('ref_axis',(-0.870740345484703,-1.90004769966601E-15,
0.491743073916837));
#122621=DIRECTION('center_axis',(-0.978147600733807,-0.207911690817751,
0.));
#122622=DIRECTION('ref_axis',(0.207911690817752,-0.978147600733807,0.));
#122623=DIRECTION('center_axis',(0.978147600733807,0.207911690817753,-1.37739719617122E-16));
#122624=DIRECTION('ref_axis',(-0.207911690817753,0.978147600733807,6.2795738784361E-33));
#122625=DIRECTION('center_axis',(0.978147600733806,0.207911690817757,2.83991567709912E-15));
#122626=DIRECTION('ref_axis',(-0.207911690817757,0.978147600733806,-3.75217731718872E-32));
#122627=DIRECTION('center_axis',(0.978147600733807,0.207911690817753,-1.37739719617122E-16));
#122628=DIRECTION('ref_axis',(-0.207911690817753,0.978147600733807,1.15415498391972E-33));
#122629=DIRECTION('center_axis',(-0.978147600733807,-0.207911690817751,
0.));
#122630=DIRECTION('ref_axis',(0.207911690817752,-0.978147600733807,0.));
#122631=DIRECTION('center_axis',(0.518344097776653,0.110177439185354,-0.848045003637581));
#122632=DIRECTION('ref_axis',(-0.853239582811869,3.05350236707336E-15,-0.521519140898039));
#122633=DIRECTION('center_axis',(-0.489078846173993,-0.103956917928312,
0.866022425483291));
#122634=DIRECTION('ref_axis',(0.87074026939378,2.35244089688217E-16,0.491743208652694));
#122635=DIRECTION('center_axis',(-0.518344074628207,-0.110177412160433,
0.848045021297489));
#122636=DIRECTION('ref_axis',(-0.830401496086228,-0.172101506943537,-0.529919264233258));
#122637=DIRECTION('center_axis',(0.518344042878396,0.110177427516369,-0.848045038708649));
#122638=DIRECTION('ref_axis',(-0.853239616987304,-1.56305751275697E-15,
-0.521519084984776));
#122639=DIRECTION('center_axis',(-0.489078861910133,-0.103956910519561,
0.866022417485781));
#122640=DIRECTION('ref_axis',(-0.848034685338687,-0.175605160694559,-0.499999999999952));
#122641=DIRECTION('center_axis',(-0.847105178671993,-0.180092991630926,
0.499979330205273));
#122642=DIRECTION('ref_axis',(0.488852904973924,0.104894406052942,0.866036951219379));
#122643=DIRECTION('center_axis',(-0.207674488001825,0.978197989689807,-1.33614410777024E-14));
#122644=DIRECTION('ref_axis',(-0.978197989689807,-0.207674488001825,-1.57019667026149E-28));
#122645=DIRECTION('center_axis',(0.978147600733807,0.207911690817753,-1.37739719617122E-16));
#122646=DIRECTION('ref_axis',(-0.207911690817753,0.978147600733807,6.2795738784361E-33));
#122647=DIRECTION('center_axis',(-0.978147600733807,-0.207911690817751,
0.));
#122648=DIRECTION('ref_axis',(0.207911690817751,-0.978147600733807,0.));
#122649=DIRECTION('center_axis',(-2.78556626507032E-16,-2.92774812072074E-17,
-1.));
#122650=DIRECTION('ref_axis',(-1.,-1.56586024251259E-33,2.25664243350207E-16));
#122651=DIRECTION('center_axis',(-0.208148881407613,0.978097154258594,0.));
#122652=DIRECTION('ref_axis',(-0.978097154258594,-0.208148881407613,0.));
#122653=DIRECTION('center_axis',(-0.518344551206596,-0.110177535564893,
-0.848044713969304));
#122654=DIRECTION('ref_axis',(-0.853239300541031,-1.51561929168402E-15,
0.521519602711396));
#122655=DIRECTION('center_axis',(-0.518344042878388,-0.110177427516367,
0.848045038708654));
#122656=DIRECTION('ref_axis',(0.85323961698731,-2.50985335815255E-15,0.521519084984768));
#122657=DIRECTION('center_axis',(-0.518344577867011,-0.110177567003933,
-0.848044693589297));
#122658=DIRECTION('ref_axis',(0.830446875604274,0.171882402222111,-0.5299192642332));
#122659=DIRECTION('center_axis',(-0.51834461510783,-0.110177549147536,-0.848044673146738));
#122660=DIRECTION('ref_axis',(-0.853239260760977,2.64094694942535E-15,0.521519667794094));
#122661=DIRECTION('center_axis',(0.518344074797617,0.110177412124785,-0.848045021198573));
#122662=DIRECTION('ref_axis',(-0.828609503967038,-0.180532167023046,-0.529919264233206));
#122663=DIRECTION('center_axis',(-0.518344097776682,-0.11017743918536,0.848045003637563));
#122664=DIRECTION('ref_axis',(0.85323958281185,1.36926545915298E-15,0.521519140898069));
#122665=DIRECTION('center_axis',(-0.207659145615642,0.978201246800566,-2.01562116103747E-15));
#122666=DIRECTION('ref_axis',(-0.978201246800566,-0.207659145615642,1.35421654966406E-29));
#122667=DIRECTION('center_axis',(-0.978147600733806,-0.207911690817757,
-2.83991567709928E-15));
#122668=DIRECTION('ref_axis',(0.207911690817757,-0.978147600733806,-6.5334247463116E-32));
#122669=DIRECTION('center_axis',(-2.78556626507032E-16,-2.92774812072074E-17,
-1.));
#122670=DIRECTION('ref_axis',(-1.,1.27623607358273E-33,2.40228573745067E-16));
#122671=DIRECTION('center_axis',(-0.208164222161104,0.978093889466682,0.));
#122672=DIRECTION('ref_axis',(-0.978093889466682,-0.208164222161104,0.));
#122673=DIRECTION('center_axis',(-0.978147600733807,-0.207911690817753,
1.37739719617122E-16));
#122674=DIRECTION('ref_axis',(0.207911690817753,-0.978147600733807,5.37037489645435E-31));
#122675=DIRECTION('center_axis',(-0.847099893161371,-0.180025927303929,
-0.500012436349692));
#122676=DIRECTION('ref_axis',(0.488879980359381,0.104926459498552,-0.866017784402208));
#122677=DIRECTION('center_axis',(0.518344615107833,0.110177549147492,0.848044673146742));
#122678=DIRECTION('ref_axis',(0.853239260760976,-2.77194105736839E-15,-0.521519667794094));
#122679=DIRECTION('center_axis',(0.489078698392183,0.103956896853947,0.866022511471559));
#122680=DIRECTION('ref_axis',(0.846158656399947,0.184432991082058,-0.499999999999962));
#122681=DIRECTION('center_axis',(-0.489078713616272,-0.103956889752271,
-0.866022503726368));
#122682=DIRECTION('ref_axis',(-0.870740345484759,-1.01855317828021E-15,
0.491743073916738));
#122683=DIRECTION('center_axis',(0.518344577661094,0.110177567039033,0.848044693710597));
#122684=DIRECTION('ref_axis',(0.828561842309643,0.180750786617714,-0.529919264233268));
#122685=DIRECTION('center_axis',(0.518344551206575,0.110177535564859,0.848044713969322));
#122686=DIRECTION('ref_axis',(0.853239300541045,-5.67982937678162E-16,-0.521519602711372));
#122687=DIRECTION('center_axis',(-0.978147600733806,-0.207911690817757,
0.));
#122688=DIRECTION('ref_axis',(0.207911690817757,-0.978147600733806,0.));
#122689=DIRECTION('center_axis',(0.978147600733806,0.20791169081776,0.));
#122690=DIRECTION('ref_axis',(-0.20791169081776,0.978147600733805,0.));
#122691=DIRECTION('center_axis',(-0.978147600733807,-0.207911690817753,
1.37739719617122E-16));
#122692=DIRECTION('ref_axis',(0.207911690817753,-0.978147600733807,5.37037489645435E-31));
#122693=DIRECTION('center_axis',(-0.978147600733806,-0.207911690817757,
0.));
#122694=DIRECTION('ref_axis',(0.207911690817757,-0.978147600733806,0.));
#122695=DIRECTION('center_axis',(-0.978147600733807,-0.207911690817753,
1.37739719617122E-16));
#122696=DIRECTION('ref_axis',(0.207911690817753,-0.978147600733807,5.37037489645435E-31));
#122697=DIRECTION('center_axis',(0.847119506978269,0.180025582247972,-0.499979330205933));
#122698=DIRECTION('ref_axis',(0.489253749394679,0.103008581324964,0.866036951218981));
#122699=DIRECTION('center_axis',(-0.489078846173999,-0.103956917928286,
0.866022425483291));
#122700=DIRECTION('ref_axis',(0.870740269393778,-3.33045470606309E-16,0.491743208652698));
#122701=DIRECTION('center_axis',(-0.489078854957332,-0.103956919795235,
0.866022420298869));
#122702=DIRECTION('ref_axis',(-0.207911690817491,0.978147600733863,1.39870616944244E-13));
#122703=DIRECTION('center_axis',(0.497265934579216,0.0522647557776183,0.866022508720509));
#122704=DIRECTION('ref_axis',(0.10452846327069,-0.994521895367954,-1.74838271998628E-12));
#122705=DIRECTION('center_axis',(0.861270944309505,0.0905534316547599,0.500012436349098));
#122706=DIRECTION('ref_axis',(0.497376550150645,0.0512812291070752,-0.866017784402555));
#122707=DIRECTION('center_axis',(-0.497265943181917,-0.0522647566818157,
-0.866022503726311));
#122708=DIRECTION('ref_axis',(-0.867207748104378,1.34059683546342E-16,0.497946504785137));
#122709=DIRECTION('center_axis',(-0.994521895368276,-0.104528463267628,
0.));
#122710=DIRECTION('ref_axis',(0.104528463267628,-0.994521895368276,0.));
#122711=DIRECTION('center_axis',(0.994521895368274,0.104528463267647,-1.40045497140052E-16));
#122712=DIRECTION('ref_axis',(-0.104528463267647,0.994521895368274,4.46085091676035E-33));
#122713=DIRECTION('center_axis',(0.994521895368276,0.104528463267629,1.42777936329246E-15));
#122714=DIRECTION('ref_axis',(-0.104528463267629,0.994521895368276,-1.01175703524978E-30));
#122715=DIRECTION('center_axis',(0.994521895368274,0.104528463267647,-1.40045497140052E-16));
#122716=DIRECTION('ref_axis',(-0.104528463267647,0.994521895368274,4.46085091676035E-33));
#122717=DIRECTION('center_axis',(-0.994521895368276,-0.104528463267627,
0.));
#122718=DIRECTION('ref_axis',(0.104528463267627,-0.994521895368276,0.));
#122719=DIRECTION('center_axis',(0.527021232978628,0.0553921636609795,-0.848045003637568));
#122720=DIRECTION('ref_axis',(-0.849349030019368,-9.93784749494393E-16,
-0.527831625809934));
#122721=DIRECTION('center_axis',(-0.497266077958573,-0.0522647708473854,
0.866022425483295));
#122722=DIRECTION('ref_axis',(0.867207670398082,4.13270435684635E-16,0.497946640115918));
#122723=DIRECTION('center_axis',(-0.527021207132258,-0.0553921392020563,
0.8480450212975));
#122724=DIRECTION('ref_axis',(-0.843841975852909,-0.0843581245832878,-0.529919264233193));
#122725=DIRECTION('center_axis',(0.527021177161346,0.0553921577943468,-0.84804503870865));
#122726=DIRECTION('ref_axis',(-0.84934906486752,-5.14909852082013E-16,-0.527831569734768));
#122727=DIRECTION('center_axis',(-0.497266092833646,-0.0522647618386464,
0.866022417485777));
#122728=DIRECTION('ref_axis',(-0.861744800189479,-0.0859994148029189,-0.49999999999995));
#122729=DIRECTION('center_axis',(-0.861289491529659,-0.0905598208268723,
0.499979330205146));
#122730=DIRECTION('ref_axis',(0.497139368681318,0.0532207405966013,0.866036951219455));
#122731=DIRECTION('center_axis',(-0.104287292793437,0.994547213842468,-6.79237952684971E-15));
#122732=DIRECTION('ref_axis',(-0.994547213842468,-0.104287292793437,-5.43295081962893E-30));
#122733=DIRECTION('center_axis',(0.994521895368274,0.104528463267647,-1.40045497140052E-16));
#122734=DIRECTION('ref_axis',(-0.104528463267647,0.994521895368274,4.46085091676035E-33));
#122735=DIRECTION('center_axis',(-0.994521895368276,-0.104528463267628,
0.));
#122736=DIRECTION('ref_axis',(0.104528463267628,-0.994521895368276,0.));
#122737=DIRECTION('center_axis',(-2.80862404029962E-16,-1.47193748793057E-17,
-1.));
#122738=DIRECTION('ref_axis',(-1.,-7.33996988677776E-34,2.25664243350207E-16));
#122739=DIRECTION('center_axis',(-0.104769627595152,0.994496518411992,0.));
#122740=DIRECTION('ref_axis',(-0.994496518411992,-0.104769627595152,0.));
#122741=DIRECTION('center_axis',(-0.527021693998977,-0.0553922121162173,
-0.848044713969329));
#122742=DIRECTION('ref_axis',(-0.849348742192414,-1.83506661866328E-16,
0.527832088960271));
#122743=DIRECTION('center_axis',(-0.527021177161337,-0.0553921577943458,
0.848045038708656));
#122744=DIRECTION('ref_axis',(0.849349064867525,1.12341132698979E-15,0.527831569734759));
#122745=DIRECTION('center_axis',(-0.527021723799615,-0.0553922405967594,
-0.84804469358929));
#122746=DIRECTION('ref_axis',(0.843864204095484,0.0841354767076637,-0.529919264233213));
#122747=DIRECTION('center_axis',(-0.527021758969971,-0.0553922189449439,
-0.848044673146736));
#122748=DIRECTION('ref_axis',(-0.849348701629311,-1.08810580052108E-15,
0.527832154231441));
#122749=DIRECTION('center_axis',(0.527021207297265,0.0553921391468907,-0.848045021198559));
#122750=DIRECTION('ref_axis',(-0.842941044393171,-0.0929299148386683,-0.529919264233174));
#122751=DIRECTION('center_axis',(-0.527021232978637,-0.0553921636609804,
0.848045003637562));
#122752=DIRECTION('ref_axis',(0.849349030019363,3.97632889144078E-16,0.527831625809943));
#122753=DIRECTION('center_axis',(-0.104271693993661,0.994548849394384,-1.09530233639679E-15));
#122754=DIRECTION('ref_axis',(-0.994548849394384,-0.104271693993661,-4.95157661577672E-30));
#122755=DIRECTION('center_axis',(-0.994521895368276,-0.104528463267629,
0.));
#122756=DIRECTION('ref_axis',(0.104528463267629,-0.994521895368276,0.));
#122757=DIRECTION('center_axis',(-2.80862404029962E-16,-1.47193748793057E-17,
-1.));
#122758=DIRECTION('ref_axis',(-1.,6.7718648802349E-34,2.40228573745067E-16));
#122759=DIRECTION('center_axis',(-0.104785225574079,0.994494875050339,5.72514616500429E-15));
#122760=DIRECTION('ref_axis',(-0.994494875050339,-0.104785225574079,-6.43259793743591E-30));
#122761=DIRECTION('center_axis',(-0.994521895368274,-0.104528463267647,
1.40045497140052E-16));
#122762=DIRECTION('ref_axis',(0.104528463267647,-0.994521895368274,-2.54421857963839E-30));
#122763=DIRECTION('center_axis',(-0.861277224843639,-0.090493676373255,
-0.50001243634743));
#122764=DIRECTION('ref_axis',(0.497169646238253,0.0532497883205307,-0.866017784403501));
#122765=DIRECTION('center_axis',(0.527021758969985,0.0553922189448812,0.848044673146731));
#122766=DIRECTION('ref_axis',(0.849348701629303,2.79217958474986E-16,-0.527832154231454));
#122767=DIRECTION('center_axis',(0.497265928783528,0.0522647653353818,0.866022511471551));
#122768=DIRECTION('ref_axis',(0.860801807879636,0.0949749838176848,-0.499999999999981));
#122769=DIRECTION('center_axis',(-0.497265943181819,-0.0522647566817781,
-0.86602250372637));
#122770=DIRECTION('ref_axis',(-0.867207748104435,5.13864830604783E-16,0.497946504785037));
#122771=DIRECTION('center_axis',(0.527021723598022,0.0553922406572584,0.84804469371062));
#122772=DIRECTION('ref_axis',(0.842916495800095,0.0931523188259858,-0.529919264233176));
#122773=DIRECTION('center_axis',(0.527021693998996,0.0553922121161724,0.84804471396932));
#122774=DIRECTION('ref_axis',(0.849348742192403,5.99585543773934E-16,-0.527832088960289));
#122775=DIRECTION('center_axis',(-0.994521895368276,-0.104528463267629,
0.));
#122776=DIRECTION('ref_axis',(0.104528463267629,-0.994521895368276,0.));
#122777=DIRECTION('center_axis',(0.994521895368276,0.104528463267628,0.));
#122778=DIRECTION('ref_axis',(-0.104528463267628,0.994521895368276,0.));
#122779=DIRECTION('center_axis',(-0.994521895368274,-0.104528463267647,
1.40045497140052E-16));
#122780=DIRECTION('ref_axis',(0.104528463267647,-0.994521895368274,-2.54421857963839E-30));
#122781=DIRECTION('center_axis',(-0.994521895368276,-0.104528463267629,
-5.43376528903392E-14));
#122782=DIRECTION('ref_axis',(0.104528463267629,-0.994521895368276,3.90011821701468E-29));
#122783=DIRECTION('center_axis',(-0.994521895368274,-0.104528463267647,
1.40045497140052E-16));
#122784=DIRECTION('ref_axis',(0.104528463267647,-0.994521895368274,-2.54421857963839E-30));
#122785=DIRECTION('center_axis',(0.861296695145304,0.090491283002778,-0.499979330205048));
#122786=DIRECTION('ref_axis',(0.497340894868902,0.0513033469999677,0.86603695121952));
#122787=DIRECTION('center_axis',(-0.497266077958585,-0.052264770847387,
0.866022425483288));
#122788=DIRECTION('ref_axis',(0.867207670398075,-3.34654605919539E-16,0.497946640115931));
#122789=DIRECTION('center_axis',(-0.497266086882775,-0.0522647717853675,
0.866022420302451));
#122790=DIRECTION('ref_axis',(-0.104528463267235,0.994521895368317,2.09805925415276E-13));
#122791=DIRECTION('center_axis',(0.500005014359855,-5.28472542476178E-25,
0.866022508723071));
#122792=DIRECTION('ref_axis',(0.,-1.,0.));
#122793=DIRECTION('center_axis',(0.866018223015981,3.00422146885054E-5,
0.500012436347045));
#122794=DIRECTION('ref_axis',(0.50001221743854,-0.000989701280687953,-0.866017784403744));
#122795=DIRECTION('center_axis',(-0.500005023014372,1.99980824065794E-14,
-0.866022503726316));
#122796=DIRECTION('ref_axis',(-0.866022503726316,2.47318747560494E-28,0.500005023014372));
#122797=DIRECTION('center_axis',(-1.,0.,0.));
#122798=DIRECTION('ref_axis',(0.,0.,1.));
#122799=DIRECTION('center_axis',(1.,0.,-1.4081690688991E-16));
#122800=DIRECTION('ref_axis',(-1.40816906889911E-16,0.,-1.));
#122801=DIRECTION('center_axis',(1.,0.,0.));
#122802=DIRECTION('ref_axis',(0.,0.,-1.));
#122803=DIRECTION('center_axis',(1.,0.,-1.4081690688991E-16));
#122804=DIRECTION('ref_axis',(-1.40816906889911E-16,0.,-1.));
#122805=DIRECTION('center_axis',(-1.,0.,0.));
#122806=DIRECTION('ref_axis',(0.,0.,1.));
#122807=DIRECTION('center_axis',(0.52992421326579,0.,-0.848045003637563));
#122808=DIRECTION('ref_axis',(-0.848045003637563,0.,-0.52992421326579));
#122809=DIRECTION('center_axis',(-0.500005158533422,0.,0.866022425483294));
#122810=DIRECTION('ref_axis',(0.866022425483294,0.,0.500005158533421));
#122811=DIRECTION('center_axis',(-0.529924185004363,2.16250770144206E-8,
0.848045021297491));
#122812=DIRECTION('ref_axis',(-0.848037146343328,0.00430950303294841,-0.529919264233217));
#122813=DIRECTION('center_axis',(0.529924157141051,0.,-0.848045038708645));
#122814=DIRECTION('ref_axis',(-0.848045038708645,0.,-0.529924157141051));
#122815=DIRECTION('center_axis',(-0.500005172385336,1.05228546522468E-8,
0.866022417485778));
#122816=DIRECTION('ref_axis',(-0.866013458679382,0.00454855869519104,-0.499999999999971));
#122817=DIRECTION('center_axis',(-0.866037336481608,-3.44576746081222E-5,
0.499979330205271));
#122818=DIRECTION('ref_axis',(0.499979069431786,0.000963977571833242,0.866036951219384));
#122819=DIRECTION('center_axis',(1.,0.,-1.4081690688991E-16));
#122820=DIRECTION('ref_axis',(-1.40816906889911E-16,0.,-1.));
#122821=DIRECTION('center_axis',(-1.,0.,0.));
#122822=DIRECTION('ref_axis',(0.,0.,1.));
#122823=DIRECTION('center_axis',(-0.529924676825566,4.63345850078939E-14,
-0.848044713969328));
#122824=DIRECTION('ref_axis',(-0.848044713969328,6.28460543516088E-28,0.529924676825566));
#122825=DIRECTION('center_axis',(-0.529924157141051,0.,0.848045038708645));
#122826=DIRECTION('ref_axis',(0.848045038708645,0.,0.529924157141051));
#122827=DIRECTION('center_axis',(-0.529924709439991,-2.52115190754827E-8,
-0.848044693589283));
#122828=DIRECTION('ref_axis',(0.848035979777046,-0.004533254694808,-0.529919264233201));
#122829=DIRECTION('center_axis',(-0.529924742154432,-7.52880596504244E-14,
-0.848044673146739));
#122830=DIRECTION('ref_axis',(-0.848044673146739,-1.67508848323945E-27,
0.529924742154432));
#122831=DIRECTION('center_axis',(0.529924185162666,-2.16955825930106E-8,
-0.84804502119857));
#122832=DIRECTION('ref_axis',(-0.848037146343333,-0.00430950303298729,-0.529919264233208));
#122833=DIRECTION('center_axis',(-0.52992421326579,0.,0.848045003637563));
#122834=DIRECTION('ref_axis',(0.848045003637563,0.,0.52992421326579));
#122835=DIRECTION('center_axis',(-1.,0.,0.));
#122836=DIRECTION('ref_axis',(0.,0.,1.));
#122837=DIRECTION('center_axis',(-1.,0.,1.4081690688991E-16));
#122838=DIRECTION('ref_axis',(1.40816906889911E-16,0.,1.));
#122839=DIRECTION('center_axis',(-0.866018223014584,3.00422160359115E-5,
-0.500012436349465));
#122840=DIRECTION('ref_axis',(0.500012217440937,0.000989701331542005,-0.866017784402302));
#122841=DIRECTION('center_axis',(0.529924742154432,0.,0.848044673146739));
#122842=DIRECTION('ref_axis',(0.848044673146739,0.,-0.529924742154432));
#122843=DIRECTION('center_axis',(0.500005009599436,1.01138510236107E-8,
0.866022511471537));
#122844=DIRECTION('ref_axis',(0.866013834616156,0.00447641077665378,-0.49999999999998));
#122845=DIRECTION('center_axis',(-0.50000502301429,0.,-0.866022503726363));
#122846=DIRECTION('ref_axis',(-0.866022503726363,0.,0.50000502301429));
#122847=DIRECTION('center_axis',(0.529924709245824,2.5290276851337E-8,0.848044693710614));
#122848=DIRECTION('ref_axis',(0.84803597977705,0.00453325469478472,-0.529919264233196));
#122849=DIRECTION('center_axis',(0.529924676825566,-2.89534733035821E-14,
0.848044713969328));
#122850=DIRECTION('ref_axis',(0.848044713969328,-3.88919656581317E-28,-0.529924676825566));
#122851=DIRECTION('center_axis',(-1.,0.,0.));
#122852=DIRECTION('ref_axis',(0.,0.,1.));
#122853=DIRECTION('center_axis',(1.,0.,0.));
#122854=DIRECTION('ref_axis',(0.,0.,-1.));
#122855=DIRECTION('center_axis',(-1.,0.,1.4081690688991E-16));
#122856=DIRECTION('ref_axis',(1.40816906889911E-16,0.,1.));
#122857=DIRECTION('center_axis',(-1.,0.,-5.46369598732844E-14));
#122858=DIRECTION('ref_axis',(-5.46369598732844E-14,0.,1.));
#122859=DIRECTION('center_axis',(-1.,0.,1.4081690688991E-16));
#122860=DIRECTION('ref_axis',(1.40816906889911E-16,0.,1.));
#122861=DIRECTION('center_axis',(0.866037336481682,-3.44576746592244E-5,
-0.499979330205142));
#122862=DIRECTION('ref_axis',(0.499979069431655,-0.0009639775757032,0.866036951219455));
#122863=DIRECTION('center_axis',(-0.500005158533445,0.,0.866022425483281));
#122864=DIRECTION('ref_axis',(0.866022425483281,0.,0.500005158533445));
#122865=DIRECTION('center_axis',(-0.500005167507542,-1.62899615243472E-20,
0.866022420302012));
#122866=DIRECTION('ref_axis',(2.517671104983E-12,1.,1.43367382367087E-12));
#122867=DIRECTION('center_axis',(0.497265934578437,-0.0522647557775339,
0.866022508720962));
#122868=DIRECTION('ref_axis',(-0.104528463269674,-0.994521895368061,1.15393259518051E-12));
#122869=DIRECTION('center_axis',(0.861277224842471,-0.0904936763714831,
0.500012436349763));
#122870=DIRECTION('ref_axis',(0.497169646236513,-0.0532497883592382,-0.86601778440212));
#122871=DIRECTION('center_axis',(-0.497265943181921,0.0522647566818165,
-0.866022503726309));
#122872=DIRECTION('ref_axis',(-0.867207748104375,1.06823760381825E-15,0.497946504785141));
#122873=DIRECTION('center_axis',(-0.99452189536827,0.104528463267684,0.));
#122874=DIRECTION('ref_axis',(-0.104528463267684,-0.99452189536827,0.));
#122875=DIRECTION('center_axis',(0.994521895368273,-0.104528463267661,-1.40045497140051E-16));
#122876=DIRECTION('ref_axis',(0.104528463267661,0.994521895368273,1.30294696027314E-33));
#122877=DIRECTION('center_axis',(0.99452189536827,-0.104528463267683,7.13889681646599E-16));
#122878=DIRECTION('ref_axis',(0.104528463267683,0.99452189536827,1.34079853327121E-32));
#122879=DIRECTION('center_axis',(0.994521895368273,-0.104528463267661,-1.40045497140051E-16));
#122880=DIRECTION('ref_axis',(0.104528463267661,0.994521895368273,1.30294696027314E-33));
#122881=DIRECTION('center_axis',(-0.99452189536827,0.104528463267684,0.));
#122882=DIRECTION('ref_axis',(-0.104528463267684,-0.99452189536827,0.));
#122883=DIRECTION('center_axis',(0.527021232978633,-0.055392163661009,-0.848045003637563));
#122884=DIRECTION('ref_axis',(-0.849349030019364,5.85867664728134E-16,-0.52783162580994));
#122885=DIRECTION('center_axis',(-0.497266077958558,0.0522647708474108,
0.866022425483302));
#122886=DIRECTION('ref_axis',(0.86720767039809,-1.24823614703178E-15,0.497946640115905));
#122887=DIRECTION('center_axis',(-0.527021202611211,0.0553921822166726,
0.848045021297518));
#122888=DIRECTION('ref_axis',(-0.842941044394674,0.0929299148248866,-0.529919264233199));
#122889=DIRECTION('center_axis',(0.527021177161334,-0.0553921577943745,
-0.848045038708656));
#122890=DIRECTION('ref_axis',(-0.849349064867527,1.26627050092037E-15,-0.527831569734757));
#122891=DIRECTION('center_axis',(-0.497266090635456,0.052264782753286,0.866022417485762));
#122892=DIRECTION('ref_axis',(-0.860793892491048,0.0950466972078587,-0.499999999999987));
#122893=DIRECTION('center_axis',(-0.861296695145158,0.090491283003084,0.499979330205244));
#122894=DIRECTION('ref_axis',(0.497340894869869,-0.0513033469926123,0.8660369512194));
#122895=DIRECTION('center_axis',(0.104769627595185,0.994496518411988,6.7920332963246E-15));
#122896=DIRECTION('ref_axis',(-0.994496518411988,0.104769627595185,1.05324867106884E-29));
#122897=DIRECTION('center_axis',(0.994521895368273,-0.104528463267661,-1.40045497140051E-16));
#122898=DIRECTION('ref_axis',(0.104528463267661,0.994521895368273,1.30294696027314E-33));
#122899=DIRECTION('center_axis',(-0.99452189536827,0.104528463267682,0.));
#122900=DIRECTION('ref_axis',(-0.104528463267682,-0.99452189536827,0.));
#122901=DIRECTION('center_axis',(-2.80862404029962E-16,1.47193748793076E-17,
-1.));
#122902=DIRECTION('ref_axis',(-1.,7.33996988677776E-34,2.25664243350207E-16));
#122903=DIRECTION('center_axis',(0.104287292793436,0.994547213842468,0.));
#122904=DIRECTION('ref_axis',(-0.994547213842468,0.104287292793436,0.));
#122905=DIRECTION('center_axis',(-0.527021693998993,0.0553922121162014,
-0.84804471396932));
#122906=DIRECTION('ref_axis',(-0.849348742192405,7.73172637784552E-16,0.527832088960287));
#122907=DIRECTION('center_axis',(-0.527021177161343,0.0553921577943754,
0.84804503870865));
#122908=DIRECTION('ref_axis',(0.849349064867521,-6.73775658095366E-16,0.527831569734766));
#122909=DIRECTION('center_axis',(-0.527021729070407,0.0553921904487129,
-0.848044693589277));
#122910=DIRECTION('ref_axis',(0.842916495800679,-0.0931523188207521,-0.529919264233166));
#122911=DIRECTION('center_axis',(-0.527021758969984,0.0553922189448815,
-0.848044673146731));
#122912=DIRECTION('ref_axis',(-0.849348701629303,3.24436902378634E-16,0.527832154231453));
#122913=DIRECTION('center_axis',(0.527021202762083,-0.0553921822962672,
-0.848045021198559));
#122914=DIRECTION('ref_axis',(-0.843841975854018,0.0843581245720705,-0.529919264233212));
#122915=DIRECTION('center_axis',(-0.527021232978546,0.0553921636609998,
0.848045003637618));
#122916=DIRECTION('ref_axis',(0.849349030019419,4.23856781191178E-16,0.527831625809852));
#122917=DIRECTION('center_axis',(0.104785225574091,0.994494875050338,1.06687590778439E-15));
#122918=DIRECTION('ref_axis',(-0.994494875050338,0.104785225574091,-2.00184842661233E-31));
#122919=DIRECTION('center_axis',(-0.99452189536827,0.104528463267683,0.));
#122920=DIRECTION('ref_axis',(-0.104528463267683,-0.99452189536827,0.));
#122921=DIRECTION('center_axis',(-2.80862404029962E-16,1.47193748793076E-17,
-1.));
#122922=DIRECTION('ref_axis',(-1.,-6.7718648802349E-34,2.40228573745067E-16));
#122923=DIRECTION('center_axis',(0.104271693993677,0.994548849394382,1.0953023363959E-15));
#122924=DIRECTION('ref_axis',(-0.994548849394382,0.104271693993677,-2.24841715580815E-30));
#122925=DIRECTION('center_axis',(-0.994521895368273,0.104528463267661,1.40045497140051E-16));
#122926=DIRECTION('ref_axis',(-0.104528463267661,-0.994521895368273,-3.17226103509723E-30));
#122927=DIRECTION('center_axis',(-0.86127094430936,0.0905534316549058,-0.500012436349321));
#122928=DIRECTION('ref_axis',(0.497376550151829,-0.0512812290979085,-0.866017784402418));
#122929=DIRECTION('center_axis',(0.527021758969972,-0.0553922189449264,
0.848044673146736));
#122930=DIRECTION('ref_axis',(0.84934870162931,-1.04254574140673E-15,-0.527832154231442));
#122931=DIRECTION('center_axis',(0.497265930897757,-0.0522647452198303,
0.866022511471551));
#122932=DIRECTION('ref_axis',(0.861737632556863,-0.0860712067727678,-0.499999999999973));
#122933=DIRECTION('center_axis',(-0.497265943181812,0.0522647566818046,
-0.866022503726373));
#122934=DIRECTION('ref_axis',(-0.867207748104439,-1.05899293295569E-16,
0.497946504785031));
#122935=DIRECTION('center_axis',(0.52702172888492,-0.0553921903558326,0.848044693710617));
#122936=DIRECTION('ref_axis',(0.843864204094707,-0.0841354767155294,-0.529919264233202));
#122937=DIRECTION('center_axis',(0.527021693998975,-0.0553922121162288,
0.848044713969329));
#122938=DIRECTION('ref_axis',(0.849348742192415,-2.80634281047211E-16,-0.52783208896027));
#122939=DIRECTION('center_axis',(-0.99452189536827,0.104528463267683,-7.13889681646599E-16));
#122940=DIRECTION('ref_axis',(-0.104528463267683,-0.99452189536827,-1.34079853327121E-32));
#122941=DIRECTION('center_axis',(0.99452189536827,-0.104528463267683,0.));
#122942=DIRECTION('ref_axis',(0.104528463267683,0.99452189536827,0.));
#122943=DIRECTION('center_axis',(-0.994521895368273,0.104528463267661,1.40045497140051E-16));
#122944=DIRECTION('ref_axis',(-0.104528463267661,-0.994521895368273,-3.17226103509723E-30));
#122945=DIRECTION('center_axis',(-0.99452189536827,0.104528463267683,0.));
#122946=DIRECTION('ref_axis',(-0.104528463267683,-0.99452189536827,0.));
#122947=DIRECTION('center_axis',(-0.994521895368273,0.104528463267661,1.40045497140051E-16));
#122948=DIRECTION('ref_axis',(-0.104528463267661,-0.994521895368273,-3.17226103509723E-30));
#122949=DIRECTION('center_axis',(0.861289491529929,-0.0905598208278999,
-0.499979330204495));
#122950=DIRECTION('ref_axis',(0.497139368682485,-0.0532207405793518,0.866036951219846));
#122951=DIRECTION('center_axis',(-0.497266077958593,0.0522647708474152,
0.866022425483281));
#122952=DIRECTION('ref_axis',(0.86720767039807,8.55165079355547E-16,0.497946640115939));
#122953=DIRECTION('center_axis',(-0.497266086886414,0.0522647717857493,
0.866022420300339));
#122954=DIRECTION('ref_axis',(0.104528463264132,0.994521895368643,-2.02812394566828E-12));
#122955=DIRECTION('center_axis',(0.489078705152892,-0.103956887953326,0.866022508721933));
#122956=DIRECTION('ref_axis',(-0.207911690816164,-0.978147600734145,-9.44126668779075E-13));
#122957=DIRECTION('center_axis',(0.847099893161435,-0.180025927304715,0.5000124363493));
#122958=DIRECTION('ref_axis',(0.488879980346119,-0.104926459558925,-0.866017784402381));
#122959=DIRECTION('center_axis',(-0.489078713616374,0.103956889752291,-0.866022503726308));
#122960=DIRECTION('ref_axis',(-0.8707403454847,1.34673219974783E-15,0.491743073916842));
#122961=DIRECTION('center_axis',(-0.978147600733806,0.207911690817757,0.));
#122962=DIRECTION('ref_axis',(-0.207911690817757,-0.978147600733806,0.));
#122963=DIRECTION('center_axis',(0.978147600733804,-0.207911690817766,-1.37739719617121E-16));
#122964=DIRECTION('ref_axis',(0.207911690817766,0.978147600733804,1.60446558522523E-32));
#122965=DIRECTION('center_axis',(0.978147600733806,-0.207911690817757,2.83991567709912E-15));
#122966=DIRECTION('ref_axis',(0.207911690817757,0.978147600733806,3.75217731718872E-32));
#122967=DIRECTION('center_axis',(0.978147600733804,-0.207911690817766,-1.37739719617121E-16));
#122968=DIRECTION('ref_axis',(0.207911690817766,0.978147600733804,3.71870420817402E-33));
#122969=DIRECTION('center_axis',(-0.978147600733806,0.207911690817757,0.));
#122970=DIRECTION('ref_axis',(-0.207911690817757,-0.978147600733806,0.));
#122971=DIRECTION('center_axis',(0.518344097776651,-0.110177439185353,-0.848045003637583));
#122972=DIRECTION('ref_axis',(-0.85323958281187,-2.80350702506811E-15,-0.521519140898037));
#122973=DIRECTION('center_axis',(-0.489078846174,0.103956917928285,0.86602242548329));
#122974=DIRECTION('ref_axis',(0.870740269393777,4.88633091176988E-16,0.4917432086527));
#122975=DIRECTION('center_axis',(-0.518344065636028,0.110177454465083,0.848045021297518));
#122976=DIRECTION('ref_axis',(-0.828609503964381,0.180532167035406,-0.52991926423315));
#122977=DIRECTION('center_axis',(0.518344042878403,-0.110177427516371,-0.848045038708645));
#122978=DIRECTION('ref_axis',(-0.8532396169873,6.46440564947912E-16,-0.521519084984783));
#122979=DIRECTION('center_axis',(-0.489078857536097,0.103956931097731,0.866022417485788));
#122980=DIRECTION('ref_axis',(-0.846143288282855,0.18450348423242,-0.499999999999975));
#122981=DIRECTION('center_axis',(-0.847119506978905,0.180025582247166,0.499979330205145));
#122982=DIRECTION('ref_axis',(0.489253749388084,-0.103008581352267,0.866036951219459));
#122983=DIRECTION('center_axis',(0.208148881407623,0.978097154258592,-1.33600637423501E-14));
#122984=DIRECTION('ref_axis',(-0.978097154258592,0.208148881407623,6.0960315452562E-29));
#122985=DIRECTION('center_axis',(0.978147600733804,-0.207911690817766,-1.37739719617121E-16));
#122986=DIRECTION('ref_axis',(0.207911690817766,0.978147600733804,1.60446558522523E-32));
#122987=DIRECTION('center_axis',(-0.978147600733806,0.20791169081776,0.));
#122988=DIRECTION('ref_axis',(-0.20791169081776,-0.978147600733805,0.));
#122989=DIRECTION('center_axis',(-2.78556626507032E-16,2.92774812072093E-17,
-1.));
#122990=DIRECTION('ref_axis',(-1.,1.56586024251259E-33,2.25664243350207E-16));
#122991=DIRECTION('center_axis',(0.20767448800183,0.978197989689806,0.));
#122992=DIRECTION('ref_axis',(-0.978197989689806,0.20767448800183,0.));
#122993=DIRECTION('center_axis',(-0.518344551206579,0.11017753556484,-0.848044713969322));
#122994=DIRECTION('ref_axis',(-0.853239300541044,-9.36522703165552E-16,
0.521519602711375));
#122995=DIRECTION('center_axis',(-0.518344042878406,0.110177427516371,0.848045038708643));
#122996=DIRECTION('ref_axis',(0.853239616987298,-2.86146343343731E-16,0.521519084984786));
#122997=DIRECTION('center_axis',(-0.518344588350167,0.110177517684659,-0.848044693589284));
#122998=DIRECTION('ref_axis',(0.828561842306931,-0.180750786630268,-0.529919264233226));
#122999=DIRECTION('center_axis',(-0.518344615107843,0.110177549147442,-0.848044673146742));
#123000=DIRECTION('ref_axis',(-0.853239260760972,-3.62990359272678E-15,
0.521519667794101));
#123001=DIRECTION('center_axis',(0.51834406577791,-0.110177454559223,-0.848045021198566));
#123002=DIRECTION('ref_axis',(-0.830401496089648,0.172101506927106,-0.529919264233236));
#123003=DIRECTION('center_axis',(-0.518344097776628,0.110177439185349,0.848045003637597));
#123004=DIRECTION('ref_axis',(0.853239582811884,-1.82149902462599E-16,0.521519140898014));
#123005=DIRECTION('center_axis',(0.208164222161113,0.978093889466681,-1.13734602532708E-14));
#123006=DIRECTION('ref_axis',(-0.978093889466681,0.208164222161113,-1.1232129081755E-29));
#123007=DIRECTION('center_axis',(-0.978147600733806,0.207911690817757,-5.67983135419856E-15));
#123008=DIRECTION('ref_axis',(-0.207911690817757,-0.978147600733806,1.30668494926232E-31));
#123009=DIRECTION('center_axis',(-2.78556626507032E-16,2.92774812072093E-17,
-1.));
#123010=DIRECTION('ref_axis',(-1.,-1.27623607358273E-33,2.40228573745067E-16));
#123011=DIRECTION('center_axis',(0.207659145615657,0.978201246800563,2.0156211610367E-15));
#123012=DIRECTION('ref_axis',(-0.978201246800563,0.207659145615657,-8.6231864451917E-30));
#123013=DIRECTION('center_axis',(-0.978147600733804,0.207911690817766,1.37739719617121E-16));
#123014=DIRECTION('ref_axis',(-0.207911690817766,-0.978147600733804,1.32119636604405E-30));
#123015=DIRECTION('center_axis',(-0.847087400905852,0.180084698747157,-0.500012436349051));
#123016=DIRECTION('ref_axis',(0.489291521294912,-0.102990311618894,-0.86601778440258));
#123017=DIRECTION('center_axis',(0.518344615107832,-0.110177549147519,0.848044673146739));
#123018=DIRECTION('ref_axis',(0.853239260760976,2.80072453551802E-15,-0.521519667794095));
#123019=DIRECTION('center_axis',(0.489078702597842,-0.103956877068183,0.866022511471522));
#123020=DIRECTION('ref_axis',(0.848020052665161,-0.175675810166694,-0.500000000000054));
#123021=DIRECTION('center_axis',(-0.489078713616299,0.103956889752277,-0.866022503726352));
#123022=DIRECTION('ref_axis',(-0.870740345484743,-2.29938292486793E-15,
0.491743073916766));
#123023=DIRECTION('center_axis',(0.518344588177269,-0.110177517564182,0.848044693710616));
#123024=DIRECTION('ref_axis',(0.830446875605224,-0.171882402217535,-0.529919264233195));
#123025=DIRECTION('center_axis',(0.518344551206566,-0.110177535564839,0.84804471396933));
#123026=DIRECTION('ref_axis',(0.853239300541052,2.40506994729313E-15,-0.521519602711362));
#123027=DIRECTION('center_axis',(-0.978147600733806,0.207911690817757,-2.83991567709928E-15));
#123028=DIRECTION('ref_axis',(-0.207911690817757,-0.978147600733806,6.5334247463116E-32));
#123029=DIRECTION('center_axis',(0.978147600733807,-0.207911690817751,0.));
#123030=DIRECTION('ref_axis',(0.207911690817751,0.978147600733807,0.));
#123031=DIRECTION('center_axis',(-0.978147600733804,0.207911690817766,1.37739719617121E-16));
#123032=DIRECTION('ref_axis',(-0.207911690817766,-0.978147600733804,1.32119636604405E-30));
#123033=DIRECTION('center_axis',(-0.978147600733806,0.207911690817757,-5.91228425656406E-14));
#123034=DIRECTION('ref_axis',(-0.207911690817757,-0.978147600733806,-1.10389829321544E-30));
#123035=DIRECTION('center_axis',(-0.978147600733804,0.207911690817766,1.37739719617121E-16));
#123036=DIRECTION('ref_axis',(-0.207911690817766,-0.978147600733804,1.32119636604405E-30));
#123037=DIRECTION('center_axis',(0.847105178672255,-0.180092991631758,-0.499979330204529));
#123038=DIRECTION('ref_axis',(0.488852904980983,-0.104894406016243,0.866036951219839));
#123039=DIRECTION('center_axis',(-0.489078846174022,0.103956917928291,0.866022425483277));
#123040=DIRECTION('ref_axis',(0.870740269393764,-1.77516479390848E-15,0.491743208652722));
#123041=DIRECTION('center_axis',(-0.489078854950438,0.103956919793789,0.866022420302937));
#123042=DIRECTION('ref_axis',(0.207911690821673,0.978147600732974,2.30786517957212E-12));
#123043=DIRECTION('center_axis',(0.475533027088914,-0.154510046710454,0.866022508722024));
#123044=DIRECTION('ref_axis',(-0.309016994376972,-0.951056516294496,1.18890024960415E-12));
#123045=DIRECTION('center_axis',(0.823641557784546,-0.267585776505932,0.500012436347302));
#123046=DIRECTION('ref_axis',(0.475234043107506,-0.155453534435146,-0.866017784403596));
#123047=DIRECTION('center_axis',(-0.47553303531813,0.154510049384315,-0.866022503726308));
#123048=DIRECTION('ref_axis',(-0.876548788012439,-2.73579469640639E-15,
0.48131301897406));
#123049=DIRECTION('center_axis',(-0.951056516295146,0.309016994374972,0.));
#123050=DIRECTION('ref_axis',(-0.309016994374972,-0.951056516295146,0.));
#123051=DIRECTION('center_axis',(0.951056516295151,-0.309016994374955,-1.33924836902177E-16));
#123052=DIRECTION('ref_axis',(0.309016994374955,0.951056516295151,-1.26216548479895E-32));
#123053=DIRECTION('center_axis',(0.951056516295148,-0.309016994374964,0.));
#123054=DIRECTION('ref_axis',(0.309016994374964,0.951056516295148,0.));
#123055=DIRECTION('center_axis',(0.951056516295151,-0.309016994374955,-1.33924836902177E-16));
#123056=DIRECTION('ref_axis',(0.309016994374955,0.951056516295151,-2.95703203911168E-34));
#123057=DIRECTION('center_axis',(-0.951056516295151,0.309016994374956,0.));
#123058=DIRECTION('ref_axis',(-0.309016994374956,-0.951056516295151,0.));
#123059=DIRECTION('center_axis',(0.503987876168974,-0.1637555876299,-0.848045003637586));
#123060=DIRECTION('ref_axis',(-0.859649462041495,-1.25677763959017E-15,
-0.510884333691853));
#123061=DIRECTION('center_axis',(-0.475533164204393,0.154510091261982,0.866022425483296));
#123062=DIRECTION('ref_axis',(0.876548714628846,-1.09074871697088E-16,0.481313152617419));
#123063=DIRECTION('center_axis',(-0.503987842609045,0.163755599460945,0.848045021297494));
#123064=DIRECTION('ref_axis',(-0.805199544418188,0.266156471015187,-0.529919264233227));
#123065=DIRECTION('center_axis',(0.503987822791202,-0.163755570286411,-0.848045038708651));
#123066=DIRECTION('ref_axis',(-0.859649495083704,7.85201449699707E-16,-0.510884278092732));
#123067=DIRECTION('center_axis',(-0.475533174127523,0.154510105547485,0.866022417485776));
#123068=DIRECTION('ref_axis',(-0.822222161142181,0.271938812468327,-0.499999999999997));
#123069=DIRECTION('center_axis',(-0.823661100222764,0.267587483540024,0.499979330205303));
#123070=DIRECTION('ref_axis',(0.475806237442976,-0.153585232144924,0.866036951219374));
#123071=DIRECTION('center_axis',(0.309247612517411,0.950981553003149,2.59793704758334E-14));
#123072=DIRECTION('ref_axis',(-0.950981553003149,0.309247612517411,-2.01038495813744E-28));
#123073=DIRECTION('center_axis',(0.951056516295151,-0.309016994374955,-1.33924836902177E-16));
#123074=DIRECTION('ref_axis',(0.309016994374955,0.951056516295151,-1.26216548479895E-32));
#123075=DIRECTION('center_axis',(-0.951056516295151,0.309016994374956,0.));
#123076=DIRECTION('ref_axis',(-0.309016994374956,-0.951056516295151,0.));
#123077=DIRECTION('center_axis',(-2.74741743792087E-16,4.3514817324298E-17,
-1.));
#123078=DIRECTION('ref_axis',(-1.,-2.34879036376888E-33,2.25664243350207E-16));
#123079=DIRECTION('center_axis',(0.308786358060997,0.951131423661013,0.));
#123080=DIRECTION('ref_axis',(-0.951131423661013,0.308786358060997,0.));
#123081=DIRECTION('center_axis',(-0.503988317040562,0.163755730877734,-0.848044713969329));
#123082=DIRECTION('ref_axis',(-0.859649189130478,3.14369996253285E-15,0.510884792910605));
#123083=DIRECTION('center_axis',(-0.503987822791237,0.163755570286422,0.848045038708627));
#123084=DIRECTION('ref_axis',(0.859649495083682,-1.36481806660529E-15,0.510884278092769));
#123085=DIRECTION('center_axis',(-0.503988355851142,0.163755716973661,-0.848044693589262));
#123086=DIRECTION('ref_axis',(0.805129291876029,-0.266368911019599,-0.529919264233182));
#123087=DIRECTION('center_axis',(-0.503988379172014,0.163755751065422,-0.848044673146743));
#123088=DIRECTION('ref_axis',(-0.859649150669462,5.07104693475844E-15,0.510884857627698));
#123089=DIRECTION('center_axis',(0.50398784273828,-0.163755599575522,-0.848045021198566));
#123090=DIRECTION('ref_axis',(-0.807862963766318,0.257959309134735,-0.529919264233177));
#123091=DIRECTION('center_axis',(-0.503987876168969,0.163755587629899,0.848045003637589));
#123092=DIRECTION('ref_axis',(0.859649462041497,4.5006472016428E-16,0.510884333691849));
#123093=DIRECTION('center_axis',(0.309262527968972,0.95097670255072,0.));
#123094=DIRECTION('ref_axis',(-0.95097670255072,0.309262527968972,0.));
#123095=DIRECTION('center_axis',(-0.951056516295148,0.309016994374964,0.));
#123096=DIRECTION('ref_axis',(-0.309016994374964,-0.951056516295148,0.));
#123097=DIRECTION('center_axis',(-2.74741743792087E-16,4.3514817324298E-17,
-1.));
#123098=DIRECTION('ref_axis',(-1.,-1.71901185421347E-33,2.40228573745067E-16));
#123099=DIRECTION('center_axis',(0.308771440182806,0.951136266645025,0.));
#123100=DIRECTION('ref_axis',(-0.951136266645025,0.308771440182806,0.));
#123101=DIRECTION('center_axis',(-0.951056516295151,0.309016994374955,1.33924836902177E-16));
#123102=DIRECTION('ref_axis',(-0.309016994374955,-0.951056516295151,-1.27877458305741E-30));
#123103=DIRECTION('center_axis',(-0.823622990672807,0.267642920195442,-0.500012436349775));
#123104=DIRECTION('ref_axis',(0.475845712143356,-0.153571010721301,-0.866017784402157));
#123105=DIRECTION('center_axis',(0.503988379171984,-0.163755751065568,0.848044673146732));
#123106=DIRECTION('ref_axis',(0.859649150669473,3.71306128357102E-15,-0.510884857627679));
#123107=DIRECTION('center_axis',(0.475533025685365,-0.154510035619035,0.86602251147157));
#123108=DIRECTION('ref_axis',(0.825011387614939,-0.263355672628674,-0.499999999999972));
#123109=DIRECTION('center_axis',(-0.475533035318107,0.15451004938428,-0.866022503726327));
#123110=DIRECTION('ref_axis',(-0.876548788012453,1.8240586479188E-15,0.481313018974034));
#123111=DIRECTION('center_axis',(0.503988355690598,-0.163755716839192,0.848044693710638));
#123112=DIRECTION('ref_axis',(0.80793099735983,-0.257746148176285,-0.529919264233183));
#123113=DIRECTION('center_axis',(0.503988317040544,-0.163755730877805,0.848044713969326));
#123114=DIRECTION('ref_axis',(0.859649189130486,1.98206584939501E-15,-0.510884792910592));
#123115=DIRECTION('center_axis',(-0.951056516295148,0.309016994374964,0.));
#123116=DIRECTION('ref_axis',(-0.309016994374964,-0.951056516295148,0.));
#123117=DIRECTION('center_axis',(0.951056516295148,-0.309016994374964,0.));
#123118=DIRECTION('ref_axis',(0.309016994374964,0.951056516295148,0.));
#123119=DIRECTION('center_axis',(-0.951056516295151,0.309016994374955,1.33924836902177E-16));
#123120=DIRECTION('ref_axis',(-0.309016994374955,-0.951056516295151,-1.27877458305741E-30));
#123121=DIRECTION('center_axis',(-0.951056516295148,0.309016994374964,-8.44187456091391E-15));
#123122=DIRECTION('ref_axis',(-0.309016994374964,-0.951056516295148,7.16904701312154E-29));
#123123=DIRECTION('center_axis',(-0.951056516295151,0.309016994374955,1.33924836902177E-16));
#123124=DIRECTION('ref_axis',(-0.309016994374955,-0.951056516295151,-1.27877458305741E-30));
#123125=DIRECTION('center_axis',(0.823639804208732,-0.26765302593154,-0.499979330205452));
#123126=DIRECTION('ref_axis',(0.475210466541805,-0.155418826439845,0.866036951219277));
#123127=DIRECTION('center_axis',(-0.47553316420442,0.154510091261982,0.866022425483281));
#123128=DIRECTION('ref_axis',(0.876548714628831,4.67206082329057E-15,0.481313152617445));
#123129=DIRECTION('center_axis',(-0.475533172734512,0.154510094033577,0.866022420304916));
#123130=DIRECTION('ref_axis',(0.309016994377262,0.951056516294402,1.39870616943622E-12));
#123131=DIRECTION('center_axis',(0.456777309663209,-0.203370361060108,0.86602250872545));
#123132=DIRECTION('ref_axis',(-0.406736643086926,-0.913545457637647,7.02849853442907E-12));
#123133=DIRECTION('center_axis',(0.79115923314091,-0.352213899940629,0.500012436349837));
#123134=DIRECTION('ref_axis',(0.456381342241232,-0.204277427909412,-0.866017784402149));
#123135=DIRECTION('center_axis',(-0.456777317573273,0.203370364581912,-0.86602250372631));
#123136=DIRECTION('ref_axis',(-0.884507036382098,5.88362210846088E-15,0.466526850878444));
#123137=DIRECTION('center_axis',(-0.913545457642594,0.406736643075817,0.));
#123138=DIRECTION('ref_axis',(-0.406736643075817,-0.913545457642593,0.));
#123139=DIRECTION('center_axis',(0.913545457642598,-0.406736643075807,-1.28642645648558E-16));
#123140=DIRECTION('ref_axis',(0.406736643075807,0.913545457642598,-3.77717422672452E-33));
#123141=DIRECTION('center_axis',(0.913545457642598,-0.406736643075807,0.));
#123142=DIRECTION('ref_axis',(0.406736643075807,0.913545457642598,0.));
#123143=DIRECTION('center_axis',(0.913545457642598,-0.406736643075807,-1.28642645648558E-16));
#123144=DIRECTION('ref_axis',(0.406736643075807,0.913545457642598,-3.77717422672452E-33));
#123145=DIRECTION('center_axis',(-0.913545457642594,0.406736643075817,0.));
#123146=DIRECTION('ref_axis',(-0.406736643075817,-0.913545457642593,0.));
#123147=DIRECTION('center_axis',(0.484109857923749,-0.215539595588297,-0.84804500363759));
#123148=DIRECTION('ref_axis',(-0.868458021516007,5.90166044795577E-15,-0.495762710239992));
#123149=DIRECTION('center_axis',(-0.456777441376078,0.203370419702503,0.866022425483285));
#123150=DIRECTION('ref_axis',(0.884506966812054,-7.65140401810272E-16,0.466526982779067));
#123151=DIRECTION('center_axis',(-0.484109823308551,0.215539603851996,0.848045021297506));
#123152=DIRECTION('ref_axis',(-0.772967650156497,0.348864709029283,-0.529919264233201));
#123153=DIRECTION('center_axis',(0.484109806651292,-0.215539572760328,-0.848045038708643));
#123154=DIRECTION('ref_axis',(-0.868458052949955,-2.13353959478262E-15,
-0.495762655175209));
#123155=DIRECTION('center_axis',(-0.456777449755519,0.203370434938186,0.86602241748577));
#123156=DIRECTION('ref_axis',(-0.789292595945392,0.356394722163228,-0.499999999999979));
#123157=DIRECTION('center_axis',(-0.791178490090539,0.352217640366771,0.499979330205279));
#123158=DIRECTION('ref_axis',(0.457145692798399,-0.202479170974491,0.866036951219378));
#123159=DIRECTION('center_axis',(0.406958162070226,0.913446798847324,0.));
#123160=DIRECTION('ref_axis',(-0.913446798847324,0.406958162070226,0.));
#123161=DIRECTION('center_axis',(0.913545457642598,-0.406736643075807,-1.28642645648558E-16));
#123162=DIRECTION('ref_axis',(0.406736643075807,0.913545457642598,-3.77717422672452E-33));
#123163=DIRECTION('center_axis',(-0.913545457642603,0.406736643075797,0.));
#123164=DIRECTION('ref_axis',(-0.406736643075797,-0.913545457642603,0.));
#123165=DIRECTION('center_axis',(-2.69459552538469E-16,5.72753959967207E-17,
-1.));
#123166=DIRECTION('ref_axis',(-1.,-2.74025542439703E-33,2.25664243350207E-16));
#123167=DIRECTION('center_axis',(0.406515100163544,0.913644062717546,0.));
#123168=DIRECTION('ref_axis',(-0.913644062717546,0.406515100163544,0.));
#123169=DIRECTION('center_axis',(-0.484110281406756,0.21553978413508,-0.848044713969302));
#123170=DIRECTION('ref_axis',(-0.868457761888264,2.25907686083393E-15,0.495763165045597));
#123171=DIRECTION('center_axis',(-0.48410980665131,0.215539572760337,0.84804503870863));
#123172=DIRECTION('ref_axis',(0.868458052949943,-2.95523665556292E-15,0.49576265517523));
#123173=DIRECTION('center_axis',(-0.484110321457893,0.215539774364283,-0.848044693589277));
#123174=DIRECTION('ref_axis',(0.772875576437821,-0.349068641875063,-0.529919264233152));
#123175=DIRECTION('center_axis',(-0.484110341087621,0.215539810706662,-0.848044673146742));
#123176=DIRECTION('ref_axis',(-0.868457725299266,2.47979274693718E-15,0.495763229140711));
#123177=DIRECTION('center_axis',(0.484109823426302,-0.215539603976822,-0.848045021198562));
#123178=DIRECTION('ref_axis',(-0.776473315751079,0.340990855186838,-0.529919264233217));
#123179=DIRECTION('center_axis',(-0.484109857923765,0.215539595588304,0.84804500363758));
#123180=DIRECTION('ref_axis',(0.868458021515998,-1.76836178502353E-15,0.495762710240009));
#123181=DIRECTION('center_axis',(0.406972488803041,0.913440415876952,0.));
#123182=DIRECTION('ref_axis',(-0.913440415876952,0.406972488803041,0.));
#123183=DIRECTION('center_axis',(-0.913545457642598,0.406736643075807,0.));
#123184=DIRECTION('ref_axis',(-0.406736643075807,-0.913545457642598,0.));
#123185=DIRECTION('center_axis',(-2.69459552538469E-16,5.72753959967207E-17,
-1.));
#123186=DIRECTION('ref_axis',(-1.,-1.97946819576097E-33,2.40228573745067E-16));
#123187=DIRECTION('center_axis',(0.40650077023674,0.913650438514062,0.));
#123188=DIRECTION('ref_axis',(-0.913650438514062,0.40650077023674,0.));
#123189=DIRECTION('center_axis',(-0.913545457642598,0.406736643075807,1.28642645648558E-16));
#123190=DIRECTION('ref_axis',(-0.406736643075807,-0.913545457642598,5.69448373698529E-32));
#123191=DIRECTION('center_axis',(-0.791134794599912,0.352268789802041,-0.500012436350098));
#123192=DIRECTION('ref_axis',(0.45718643779245,-0.202469153695468,-0.866017784401967));
#123193=DIRECTION('center_axis',(0.484110341087585,-0.215539810706754,0.848044673146739));
#123194=DIRECTION('ref_axis',(0.868457725299281,1.08514503248968E-15,-0.495763229140683));
#123195=DIRECTION('center_axis',(0.456777309429512,-0.203370349891223,0.866022511471531));
#123196=DIRECTION('ref_axis',(0.792963725156405,-0.348150155229116,-0.50000000000002));
#123197=DIRECTION('center_axis',(-0.456777317573209,0.203370364581883,-0.86602250372635));
#123198=DIRECTION('ref_axis',(-0.884507036382135,-3.12434821125521E-15,
0.466526850878375));
#123199=DIRECTION('center_axis',(0.484110321310578,-0.215539774217795,0.848044693710603));
#123200=DIRECTION('ref_axis',(0.776563258038879,-0.340785973388812,-0.529919264233223));
#123201=DIRECTION('center_axis',(0.484110281406699,-0.215539784135105,0.848044713969328));
#123202=DIRECTION('ref_axis',(0.868457761888295,1.70886789336824E-17,-0.495763165045542));
#123203=DIRECTION('center_axis',(-0.913545457642598,0.406736643075807,0.));
#123204=DIRECTION('ref_axis',(-0.406736643075807,-0.913545457642598,0.));
#123205=DIRECTION('center_axis',(0.913545457642598,-0.406736643075807,0.));
#123206=DIRECTION('ref_axis',(0.406736643075807,0.913545457642598,0.));
#123207=DIRECTION('center_axis',(-0.913545457642598,0.406736643075807,1.28642645648558E-16));
#123208=DIRECTION('ref_axis',(-0.406736643075807,-0.913545457642598,5.69448373698529E-32));
#123209=DIRECTION('center_axis',(-0.913545457642598,0.406736643075807,-4.99133465116398E-14));
#123210=DIRECTION('ref_axis',(-0.406736643075807,-0.913545457642598,-2.82923979546378E-31));
#123211=DIRECTION('center_axis',(-0.913545457642598,0.406736643075807,1.28642645648558E-16));
#123212=DIRECTION('ref_axis',(-0.406736643075807,-0.913545457642598,5.69448373698529E-32));
#123213=DIRECTION('center_axis',(0.791150459692854,-0.352280597671101,-0.499979330205038));
#123214=DIRECTION('ref_axis',(0.456361522796786,-0.204240445634527,0.866036951219524));
#123215=DIRECTION('center_axis',(-0.456777441376069,0.203370419702468,0.866022425483298));
#123216=DIRECTION('ref_axis',(0.884506966812062,6.03592299906791E-15,0.466526982779053));
#123217=DIRECTION('center_axis',(-0.45677744957756,0.203370423354032,0.866022420299972));
#123218=DIRECTION('ref_axis',(0.406736643068276,0.913545457645951,-4.75560097597516E-12));
#123219=DIRECTION('center_axis',(0.433017044454879,-0.250002507179727,0.866022508723308));
#123220=DIRECTION('ref_axis',(-0.499999999994351,-0.8660254037877,-3.77650667513754E-12));
#123221=DIRECTION('center_axis',(0.750008802379408,-0.432983094185632,0.50001243634818));
#123222=DIRECTION('ref_axis',(0.432528431864326,-0.250863215172243,-0.866017784403087));
#123223=DIRECTION('center_axis',(-0.433017051950279,0.250002511507198,-0.866022503726308));
#123224=DIRECTION('ref_axis',(-0.894424794863783,-6.20270810435665E-16,
0.447218387740127));
#123225=DIRECTION('center_axis',(-0.86602540378444,0.499999999999998,0.));
#123226=DIRECTION('ref_axis',(-0.499999999999998,-0.86602540378444,0.));
#123227=DIRECTION('center_axis',(0.866025403784435,-0.500000000000007,-1.2195101864901E-16));
#123228=DIRECTION('ref_axis',(0.500000000000007,0.866025403784434,1.37857749616202E-32));
#123229=DIRECTION('center_axis',(0.866025403784433,-0.50000000000001,-1.36592399683214E-14));
#123230=DIRECTION('ref_axis',(0.50000000000001,0.866025403784433,-1.33215113601878E-31));
#123231=DIRECTION('center_axis',(0.866025403784435,-0.500000000000007,-1.2195101864901E-16));
#123232=DIRECTION('ref_axis',(0.500000000000007,0.866025403784434,1.37857749616202E-32));
#123233=DIRECTION('center_axis',(-0.866025403784433,0.50000000000001,0.));
#123234=DIRECTION('ref_axis',(-0.50000000000001,-0.866025403784433,0.));
#123235=DIRECTION('center_axis',(0.458927830768604,-0.264962106632863,-0.848045003637601));
#123236=DIRECTION('ref_axis',(-0.879478602053344,3.64727084574667E-15,-0.475938429348057));
#123237=DIRECTION('center_axis',(-0.433017169313214,0.25000257926672,0.866022425483289));
#123238=DIRECTION('ref_axis',(0.894424730216418,3.37693802438162E-15,0.447218517033103));
#123239=DIRECTION('center_axis',(-0.45892779548191,0.264962111228503,0.848045021297483));
#123240=DIRECTION('ref_axis',(-0.732266960577926,0.427750712261754,-0.529919264233269));
#123241=DIRECTION('center_axis',(0.45892778216323,-0.264962078570538,-0.848045038708628));
#123242=DIRECTION('ref_axis',(-0.879478631391236,-7.35193596082728E-15,
-0.475938375135057));
#123243=DIRECTION('center_axis',(-0.433017176051311,0.250002595299908,0.866022417485747));
#123244=DIRECTION('ref_axis',(-0.747715375893068,0.436945896711557,-0.500000000000021));
#123245=DIRECTION('center_axis',(-0.750027562856218,0.432988827019233,0.499979330205231));
#123246=DIRECTION('ref_axis',(0.433476564272144,-0.249154705653748,0.866036951219411));
#123247=DIRECTION('center_axis',(0.500209992837911,0.865904130412309,0.));
#123248=DIRECTION('ref_axis',(-0.865904130412309,0.500209992837911,0.));
#123249=DIRECTION('center_axis',(0.866025403784435,-0.500000000000007,-1.2195101864901E-16));
#123250=DIRECTION('ref_axis',(0.500000000000007,0.866025403784434,1.37857749616202E-32));
#123251=DIRECTION('center_axis',(-0.86602540378444,0.499999999999998,0.));
#123252=DIRECTION('ref_axis',(-0.499999999999998,-0.86602540378444,0.));
#123253=DIRECTION('center_axis',(-2.6276792553892E-16,7.04084534449562E-17,
-1.));
#123254=DIRECTION('ref_axis',(-1.,-2.9359879547111E-33,2.25664243350207E-16));
#123255=DIRECTION('center_axis',(0.499789977759954,0.866146626230631,0.));
#123256=DIRECTION('ref_axis',(-0.866146626230631,0.499789977759954,0.));
#123257=DIRECTION('center_axis',(-0.458928232223265,0.264962338412774,-0.848044713969295));
#123258=DIRECTION('ref_axis',(-0.879478359737711,3.22745562485081E-15,0.475938877118758));
#123259=DIRECTION('center_axis',(-0.458927782163224,0.264962078570543,0.84804503870863));
#123260=DIRECTION('ref_axis',(0.879478631391239,5.78561883712524E-15,0.475938375135052));
#123261=DIRECTION('center_axis',(-0.458928273071634,0.264962332890014,-0.8480446935893));
#123262=DIRECTION('ref_axis',(0.732154074467011,-0.427943903608719,-0.529919264233229));
#123263=DIRECTION('center_axis',(-0.458928288799681,0.264962371077192,-0.848044673146733));
#123264=DIRECTION('ref_axis',(-0.879478325588497,-1.70584345960497E-15,
0.475938940222434));
#123265=DIRECTION('center_axis',(0.458927795584395,-0.264962111367593,-0.848045021198565));
#123266=DIRECTION('ref_axis',(-0.736576463592187,0.420286434085738,-0.529919264233262));
#123267=DIRECTION('center_axis',(-0.458927830768623,0.264962106632883,0.848045003637585));
#123268=DIRECTION('ref_axis',(0.879478602053333,2.80327366676551E-15,0.475938429348078));
#123269=DIRECTION('center_axis',(0.500223573885336,0.865896284857131,1.99792452361211E-14));
#123270=DIRECTION('ref_axis',(-0.865896284857131,0.500223573885336,1.39216074893221E-28));
#123271=DIRECTION('center_axis',(-0.866025403784433,0.50000000000001,0.));
#123272=DIRECTION('ref_axis',(-0.50000000000001,-0.866025403784433,0.));
#123273=DIRECTION('center_axis',(-2.6276792553892E-16,7.04084534449562E-17,
-1.));
#123274=DIRECTION('ref_axis',(-1.,-1.97946819576097E-33,2.40228573745067E-16));
#123275=DIRECTION('center_axis',(0.499776392786197,0.866154464985095,-3.64423934454608E-15));
#123276=DIRECTION('ref_axis',(-0.866154464985095,0.499776392786197,-1.32824799399631E-29));
#123277=DIRECTION('center_axis',(-0.866025403784435,0.500000000000007,1.2195101864901E-16));
#123278=DIRECTION('ref_axis',(-0.500000000000007,-0.866025403784435,-3.8972730010601E-31));
#123279=DIRECTION('center_axis',(-0.749978760164197,0.433035128829165,-0.50001243634782));
#123280=DIRECTION('ref_axis',(-0.433518133165547,0.249149002233455,0.866017784403261));
#123281=DIRECTION('center_axis',(0.458928288799652,-0.264962371077221,0.848044673146739));
#123282=DIRECTION('ref_axis',(0.87947832558851,-5.62014896054226E-15,-0.475938940222411));
#123283=DIRECTION('center_axis',(0.433017045388115,-0.250002496043341,0.866022511471524));
#123284=DIRECTION('ref_axis',(0.752228186189541,-0.429130231866715,-0.500000000000012));
#123285=DIRECTION('center_axis',(-0.433017051950174,0.250002511507138,-0.866022503726378));
#123286=DIRECTION('ref_axis',(-0.894424794863841,8.78579593512627E-16,0.447218387740013));
#123287=DIRECTION('center_axis',(0.458928272946657,-0.264962332718179,0.848044693710621));
#123288=DIRECTION('ref_axis',(0.736687329165484,-0.420092076147145,-0.529919264233155));
#123289=DIRECTION('center_axis',(0.458928232223185,-0.264962338412827,0.848044713969322));
#123290=DIRECTION('ref_axis',(0.879478359737754,5.93852501903154E-15,-0.47593887711868));
#123291=DIRECTION('center_axis',(-0.866025403784433,0.50000000000001,0.));
#123292=DIRECTION('ref_axis',(-0.50000000000001,-0.866025403784433,0.));
#123293=DIRECTION('center_axis',(0.866025403784433,-0.50000000000001,0.));
#123294=DIRECTION('ref_axis',(0.50000000000001,0.866025403784433,0.));
#123295=DIRECTION('center_axis',(-0.866025403784435,0.500000000000007,1.2195101864901E-16));
#123296=DIRECTION('ref_axis',(-0.500000000000007,-0.866025403784435,-3.8972730010601E-31));
#123297=DIRECTION('center_axis',(-0.866025403784433,0.50000000000001,-4.09777199049641E-14));
#123298=DIRECTION('ref_axis',(-0.50000000000001,-0.866025403784433,-3.99645340805632E-31));
#123299=DIRECTION('center_axis',(-0.866025403784435,0.500000000000007,1.2195101864901E-16));
#123300=DIRECTION('ref_axis',(-0.500000000000007,-0.866025403784435,-3.8972730010601E-31));
#123301=DIRECTION('center_axis',(0.749993105181602,-0.433048509462509,-0.499979330205118));
#123302=DIRECTION('ref_axis',(-0.43251258669988,0.250824363786029,-0.866036951219469));
#123303=DIRECTION('center_axis',(-0.433017169313192,0.250002579266708,0.866022425483304));
#123304=DIRECTION('ref_axis',(0.894424730216429,-3.15083324732399E-15,0.44721851703308));
#123305=DIRECTION('center_axis',(-0.433017177084066,0.250002583753203,0.866022420302656));
#123306=DIRECTION('ref_axis',(0.5000000000025,0.866025403782995,1.71341505755983E-12));
#123307=DIRECTION('center_axis',(0.404512553894632,-0.293895573516493,0.866022508719637));
#123308=DIRECTION('ref_axis',(-0.587785252288474,-0.809016994377853,-2.8323800063508E-12));
#123309=DIRECTION('center_axis',(0.700641118228508,-0.509008435042022,0.500012436348915));
#123310=DIRECTION('ref_axis',(0.403936649436713,-0.294700492602699,-0.866017784402589));
#123311=DIRECTION('center_axis',(-0.404512560891457,0.293895578600019,-0.866022503726315));
#123312=DIRECTION('ref_axis',(-0.906035256115487,-3.15407140147818E-15,
0.423202214875754));
#123313=DIRECTION('center_axis',(-0.80901699437495,0.58778525229247,-3.2114799243612E-14));
#123314=DIRECTION('ref_axis',(-0.58778525229247,-0.80901699437495,4.13565546558353E-30));
#123315=DIRECTION('center_axis',(0.809016994374943,-0.58778525229248,-1.13923270769252E-16));
#123316=DIRECTION('ref_axis',(0.58778525229248,0.809016994374943,4.71515639841956E-33));
#123317=DIRECTION('center_axis',(0.809016994374931,-0.587785252292496,-4.42022290584682E-14));
#123318=DIRECTION('ref_axis',(0.587785252292496,0.809016994374931,4.35974171970421E-30));
#123319=DIRECTION('center_axis',(0.809016994374943,-0.58778525229248,-1.13923270769252E-16));
#123320=DIRECTION('ref_axis',(0.58778525229248,0.809016994374943,4.71515639841956E-33));
#123321=DIRECTION('center_axis',(-0.80901699437495,0.58778525229247,0.));
#123322=DIRECTION('ref_axis',(-0.58778525229247,-0.80901699437495,0.));
#123323=DIRECTION('center_axis',(0.428717694262752,-0.311481637390307,-0.848045003637591));
#123324=DIRECTION('ref_axis',(-0.892442058026276,-4.81426696315707E-15,
-0.451162025292273));
#123325=DIRECTION('center_axis',(-0.404512670528681,0.293895658256105,0.866022425483293));
#123326=DIRECTION('ref_axis',(0.906035197473496,4.3386129689956E-15,0.423202340422596));
#123327=DIRECTION('center_axis',(-0.428717658685243,0.311481638277357,0.848045021297512));
#123328=DIRECTION('ref_axis',(-0.683543400921194,0.501950189213663,-0.529919264233199));
#123329=DIRECTION('center_axis',(0.428717648856917,-0.311481604401037,-0.848045038708649));
#123330=DIRECTION('ref_axis',(-0.892442084777736,7.94801068170717E-15,-0.451161972375297));
#123331=DIRECTION('center_axis',(-0.404512675558581,0.293895674899355,0.866022417485766));
#123332=DIRECTION('ref_axis',(-0.69794602972004,0.512709800567571,-0.499999999999995));
#123333=DIRECTION('center_axis',(-0.70065917669006,0.509016097474051,0.499979330205054));
#123334=DIRECTION('ref_axis',(0.405058175799853,-0.29310044923218,0.866036951219513));
#123335=DIRECTION('center_axis',(0.587981418248444,0.808874435122379,0.));
#123336=DIRECTION('ref_axis',(-0.808874435122379,0.587981418248444,0.));
#123337=DIRECTION('center_axis',(0.809016994374943,-0.58778525229248,-1.13923270769252E-16));
#123338=DIRECTION('ref_axis',(0.58778525229248,0.809016994374943,4.71515639841956E-33));
#123339=DIRECTION('center_axis',(-0.809016994374912,0.587785252292522,0.));
#123340=DIRECTION('ref_axis',(-0.587785252292522,-0.809016994374912,0.));
#123341=DIRECTION('center_axis',(-2.54740177659162E-16,8.27701011433327E-17,
-1.));
#123342=DIRECTION('ref_axis',(-1.,-2.9359879547111E-33,2.25664243350207E-16));
#123343=DIRECTION('center_axis',(0.587589051772227,0.809159506053914,0.));
#123344=DIRECTION('ref_axis',(-0.809159506053914,0.587589051772227,0.));
#123345=DIRECTION('center_axis',(-0.428718069290599,0.31148190986391,-0.8480447139693));
#123346=DIRECTION('ref_axis',(-0.892441837073364,1.28712475779731E-15,0.451162462358205));
#123347=DIRECTION('center_axis',(-0.428717648856922,0.311481604401041,0.848045038708645));
#123348=DIRECTION('ref_axis',(0.892442084777733,-5.99017820001791E-15,0.451161972375302));
#123349=DIRECTION('center_axis',(-0.428718110499122,0.311481908632163,-0.848044693589275));
#123350=DIRECTION('ref_axis',(0.683410939224596,-0.502130522416956,-0.529919264233175));
#123351=DIRECTION('center_axis',(-0.428718122142699,0.311481948263265,-0.848044673146738));
#123352=DIRECTION('ref_axis',(-0.892441805934778,-4.37991823100416E-15,
0.451162523953256));
#123353=DIRECTION('center_axis',(0.428717658777127,-0.311481638420274,-0.848045021198569));
#123354=DIRECTION('ref_axis',(-0.688609525582563,0.494977266822919,-0.529919264233214));
#123355=DIRECTION('center_axis',(-0.428717694262775,0.311481637390324,0.848045003637574));
#123356=DIRECTION('ref_axis',(0.892442058026261,-6.4705373892766E-16,0.451162025292301));
#123357=DIRECTION('center_axis',(0.587994104813606,0.808865212939984,0.));
#123358=DIRECTION('ref_axis',(-0.808865212939984,0.587994104813606,0.));
#123359=DIRECTION('center_axis',(-0.809016994374931,0.587785252292496,0.));
#123360=DIRECTION('ref_axis',(-0.587785252292496,-0.809016994374931,0.));
#123361=DIRECTION('center_axis',(-2.54740177659162E-16,8.27701011433327E-17,
-1.));
#123362=DIRECTION('ref_axis',(-1.,-1.66692058590397E-33,2.40228573745067E-16));
#123363=DIRECTION('center_axis',(0.587576360591375,0.809168721883263,1.21071329521312E-14));
#123364=DIRECTION('ref_axis',(-0.809168721883263,0.587576360591375,1.5253418562395E-28));
#123365=DIRECTION('center_axis',(-0.809016994374943,0.58778525229248,1.13923270769252E-16));
#123366=DIRECTION('ref_axis',(-0.58778525229248,-0.809016994374943,-4.00133343489574E-31));
#123367=DIRECTION('center_axis',(-0.700605801485339,0.509057044367988,-0.500012436349751));
#123368=DIRECTION('ref_axis',(-0.405100113147179,0.293099122187947,0.866017784402143));
#123369=DIRECTION('center_axis',(0.428718122142675,-0.311481948263326,0.848044673146728));
#123370=DIRECTION('ref_axis',(0.892441805934786,-1.00097613656477E-15,-0.451162523953241));
#123371=DIRECTION('center_axis',(0.404512555982611,-0.293895562533576,0.866022511471548));
#123372=DIRECTION('ref_axis',(0.703251077796155,-0.505408667890181,-0.50000000000002));
#123373=DIRECTION('center_axis',(-0.404512560891349,0.293895578599941,-0.866022503726392));
#123374=DIRECTION('ref_axis',(-0.906035256115544,9.31541476348494E-16,0.423202214875631));
#123375=DIRECTION('center_axis',(0.428718110386438,-0.31148190845687,0.848044693710625));
#123376=DIRECTION('ref_axis',(0.688740099743675,-0.494795562227121,-0.529919264233166));
#123377=DIRECTION('center_axis',(0.428718069290549,-0.311481909863894,0.848044713969331));
#123378=DIRECTION('ref_axis',(0.892441837073392,-5.0994373414288E-15,-0.451162462358151));
#123379=DIRECTION('center_axis',(-0.809016994374931,0.587785252292496,0.));
#123380=DIRECTION('ref_axis',(-0.587785252292496,-0.809016994374931,0.));
#123381=DIRECTION('center_axis',(0.809016994374931,-0.587785252292496,0.));
#123382=DIRECTION('ref_axis',(0.587785252292496,0.809016994374931,0.));
#123383=DIRECTION('center_axis',(-0.809016994374943,0.58778525229248,1.13923270769252E-16));
#123384=DIRECTION('ref_axis',(-0.58778525229248,-0.809016994374943,-4.00133343489574E-31));
#123385=DIRECTION('center_axis',(-0.809016994374931,0.587785252292496,-1.08431827545695E-13));
#123386=DIRECTION('ref_axis',(-0.587785252292496,-0.809016994374931,-1.14793899448837E-30));
#123387=DIRECTION('center_axis',(-0.809016994374943,0.58778525229248,1.13923270769252E-16));
#123388=DIRECTION('ref_axis',(-0.58778525229248,-0.809016994374943,-4.00133343489574E-31));
#123389=DIRECTION('center_axis',(0.700618669263855,-0.509071851162735,-0.499979330205451));
#123390=DIRECTION('ref_axis',(-0.403924952201757,0.294660197705125,-0.86603695121928));
#123391=DIRECTION('center_axis',(-0.404512670528659,0.293895658256109,0.866022425483302));
#123392=DIRECTION('ref_axis',(0.906035197473505,-2.34802397371862E-15,0.423202340422577));
#123393=DIRECTION('center_axis',(-0.404512677789108,0.29389566353111,0.866022420301861));
#123394=DIRECTION('ref_axis',(0.587785252293696,0.809016994374059,8.74191355908437E-13));
#123395=DIRECTION('center_axis',(0.37157613913616,-0.334568658442753,0.866022508721616));
#123396=DIRECTION('ref_axis',(-0.669130606364157,-0.743144825472624,4.12618321919621E-12));
#123397=DIRECTION('center_axis',(0.643597063368368,-0.579456972966938,0.500012436348944));
#123398=DIRECTION('ref_axis',(0.37091925268088,-0.335308969592096,-0.86601778440269));
#123399=DIRECTION('center_axis',(-0.37157614556582,0.334568664232119,-0.866022503726309));
#123400=DIRECTION('ref_axis',(-0.918982183096524,2.56545002401075E-15,0.394299058014532));
#123401=DIRECTION('center_axis',(-0.743144825477379,0.669130606358875,0.));
#123402=DIRECTION('ref_axis',(-0.669130606358875,-0.743144825477379,0.));
#123403=DIRECTION('center_axis',(0.743144825477389,-0.669130606358864,-1.04647355694968E-16));
#123404=DIRECTION('ref_axis',(0.669130606358864,0.743144825477389,-1.94545925652658E-32));
#123405=DIRECTION('center_axis',(0.743144825477406,-0.669130606358845,4.06031740096479E-14));
#123406=DIRECTION('ref_axis',(0.669130606358845,0.743144825477406,-5.14555379104688E-31));
#123407=DIRECTION('center_axis',(0.743144825477389,-0.669130606358864,-1.04647355694968E-16));
#123408=DIRECTION('ref_axis',(0.669130606358864,0.743144825477389,-1.94545925652658E-32));
#123409=DIRECTION('center_axis',(-0.743144825477382,0.669130606358872,0.));
#123410=DIRECTION('ref_axis',(-0.669130606358872,-0.743144825477382,0.));
#123411=DIRECTION('center_axis',(0.393810436983645,-0.354588510146761,-0.848045003637573));
#123412=DIRECTION('ref_axis',(-0.90697822335776,9.40871057169973E-16,-0.421177518814575));
#123413=DIRECTION('center_axis',(-0.371576246276111,0.334568754912036,0.866022425483293));
#123414=DIRECTION('ref_axis',(0.918982131463648,2.13361091916559E-15,0.394299178353862));
#123415=DIRECTION('center_axis',(-0.393810401510386,0.354588507307772,0.848045021297498));
#123416=DIRECTION('ref_axis',(-0.627330796731871,0.570650194835957,-0.529919264233185));
#123417=DIRECTION('center_axis',(0.393810395274833,-0.354588472591978,-0.848045038708657));
#123418=DIRECTION('ref_axis',(-0.906978247051303,-9.32548843552878E-15,
-0.421177467792076));
#123419=DIRECTION('center_axis',(-0.37157624953287,0.334568771996355,0.866022417485793));
#123420=DIRECTION('ref_axis',(-0.640529840771603,0.582856348580999,-0.49999999999993));
#123421=DIRECTION('center_axis',(-0.64361422196112,0.579466481046826,0.499979330205351));
#123422=DIRECTION('ref_axis',(0.372201885186834,-0.333834922957544,0.866036951219345));
#123423=DIRECTION('center_axis',(0.669310796197597,0.742982542253409,0.));
#123424=DIRECTION('ref_axis',(-0.742982542253409,0.669310796197597,0.));
#123425=DIRECTION('center_axis',(0.743144825477389,-0.669130606358864,-1.04647355694968E-16));
#123426=DIRECTION('ref_axis',(0.669130606358864,0.743144825477389,-1.94545925652658E-32));
#123427=DIRECTION('center_axis',(-0.743144825477379,0.669130606358875,0.));
#123428=DIRECTION('ref_axis',(-0.669130606358875,-0.743144825477379,0.));
#123429=DIRECTION('center_axis',(-2.45464262584879E-16,9.42249022928256E-17,
-1.));
#123430=DIRECTION('ref_axis',(-1.,-2.34879036376888E-33,2.25664243350207E-16));
#123431=DIRECTION('center_axis',(0.668950377172438,0.743307065001304,0.));
#123432=DIRECTION('ref_axis',(-0.743307065001304,0.668950377172438,0.));
#123433=DIRECTION('center_axis',(-0.39381078147567,0.354588820328836,-0.848044713969332));
#123434=DIRECTION('ref_axis',(-0.906978027661857,7.54218793329778E-15,0.421177940232638));
#123435=DIRECTION('center_axis',(-0.393810395274846,0.35458847259199,0.848045038708646));
#123436=DIRECTION('ref_axis',(0.906978247051292,-8.75481591077838E-15,0.421177467792099));
#123437=DIRECTION('center_axis',(-0.39381082258445,0.354588823414425,-0.848044693589278));
#123438=DIRECTION('ref_axis',(0.627180210724977,-0.570815694133858,-0.529919264233199));
#123439=DIRECTION('center_axis',(-0.393810830024562,0.354588864042303,-0.848044673146736));
#123440=DIRECTION('ref_axis',(-0.906978000082633,-7.8483346287888E-15,0.421177999622614));
#123441=DIRECTION('center_axis',(0.393810401583025,-0.35458850746372,-0.848045021198561));
#123442=DIRECTION('ref_axis',(-0.633098037506084,0.56424502505606,-0.529919264233177));
#123443=DIRECTION('center_axis',(-0.393810436983627,0.354588510146745,0.848045003637588));
#123444=DIRECTION('ref_axis',(0.90697822335777,-1.33133695181472E-15,0.421177518814553));
#123445=DIRECTION('center_axis',(0.669322449283885,0.742972044483923,4.02398997762812E-15));
#123446=DIRECTION('ref_axis',(-0.742972044483923,0.669322449283885,8.69613941656436E-29));
#123447=DIRECTION('center_axis',(-0.743144825477406,0.669130606358845,0.));
#123448=DIRECTION('ref_axis',(-0.669130606358845,-0.743144825477406,0.));
#123449=DIRECTION('center_axis',(-2.45464262584879E-16,9.42249022928256E-17,
-1.));
#123450=DIRECTION('ref_axis',(-1.,-1.04182536618998E-33,2.40228573745067E-16));
#123451=DIRECTION('center_axis',(0.668938718831625,0.743317556935059,0.));
#123452=DIRECTION('ref_axis',(-0.743317556935059,0.668938718831625,0.));
#123453=DIRECTION('center_axis',(-0.743144825477389,0.669130606358864,1.04647355694968E-16));
#123454=DIRECTION('ref_axis',(-0.669130606358865,-0.743144825477389,8.32249373466419E-31));
#123455=DIRECTION('center_axis',(-0.643556859037426,0.579501624401081,-0.500012436347728));
#123456=DIRECTION('ref_axis',(-0.37224373150931,0.333837986827737,0.866017784403316));
#123457=DIRECTION('center_axis',(0.393810830024499,-0.354588864042362,0.848044673146741));
#123458=DIRECTION('ref_axis',(0.906978000082659,3.44782577783986E-15,-0.421177999622559));
#123459=DIRECTION('center_axis',(0.371576142361039,-0.334568647743098,0.866022511471523));
#123460=DIRECTION('ref_axis',(0.646569003432252,-0.576149740779758,-0.500000000000042));
#123461=DIRECTION('center_axis',(-0.371576145565792,0.33456866423203,-0.866022503726355));
#123462=DIRECTION('ref_axis',(-0.918982183096543,1.46372471911345E-15,0.394299058014488));
#123463=DIRECTION('center_axis',(0.393810822490023,-0.354588823229131,0.848044693710604));
#123464=DIRECTION('ref_axis',(0.633246889648164,-0.564077964598377,-0.529919264233221));
#123465=DIRECTION('center_axis',(0.393810781475714,-0.354588820328813,0.848044713969321));
#123466=DIRECTION('ref_axis',(0.906978027661839,8.40177352928018E-15,-0.421177940232677));
#123467=DIRECTION('center_axis',(-0.743144825477406,0.669130606358845,4.06031740096479E-14));
#123468=DIRECTION('ref_axis',(-0.669130606358845,-0.743144825477406,-5.14555379104688E-31));
#123469=DIRECTION('center_axis',(0.743144825477379,-0.669130606358875,0.));
#123470=DIRECTION('ref_axis',(0.669130606358875,0.743144825477379,0.));
#123471=DIRECTION('center_axis',(-0.743144825477389,0.669130606358864,1.04647355694968E-16));
#123472=DIRECTION('ref_axis',(-0.669130606358865,-0.743144825477389,8.32249373466419E-31));
#123473=DIRECTION('center_axis',(-0.743144825477406,0.669130606358845,4.06031740096457E-14));
#123474=DIRECTION('ref_axis',(-0.669130606358845,-0.743144825477406,2.80523855531594E-30));
#123475=DIRECTION('center_axis',(-0.743144825477389,0.669130606358864,1.04647355694968E-16));
#123476=DIRECTION('ref_axis',(-0.669130606358865,-0.743144825477389,8.32249373466419E-31));
#123477=DIRECTION('center_axis',(0.643568108591973,-0.579517695131666,-0.499979330205392));
#123478=DIRECTION('ref_axis',(-0.370911831395904,0.335267672842607,-0.866036951219311));
#123479=DIRECTION('center_axis',(-0.37157624627613,0.334568754912026,0.866022425483288));
#123480=DIRECTION('ref_axis',(0.918982131463641,8.64235197177631E-15,0.394299178353879));
#123481=DIRECTION('center_axis',(-0.37157625294445,0.334568760916253,0.866022420302572));
#123482=DIRECTION('ref_axis',(0.669130606362073,0.743144825474499,2.48270345075888E-12));
#123483=DIRECTION('center_axis',(0.33456865844238,-0.371576139135717,0.866022508721951));
#123484=DIRECTION('ref_axis',(-0.743144825474233,-0.669130606362369,-2.72747704315771E-12));
#123485=DIRECTION('center_axis',(0.579501624401054,-0.643556859037126,0.500012436348146));
#123486=DIRECTION('ref_axis',(0.333837986837391,-0.372243731501189,-0.866017784403085));
#123487=DIRECTION('center_axis',(-0.3345686642321,0.371576145565839,-0.866022503726308));
#123488=DIRECTION('ref_axis',(3.52929994070592E-15,0.918982183096517,0.394299058014547));
#123489=DIRECTION('center_axis',(-0.669130606358875,0.743144825477379,0.));
#123490=DIRECTION('ref_axis',(-0.743144825477379,-0.669130606358875,0.));
#123491=DIRECTION('center_axis',(0.669130606358852,-0.7431448254774,-9.42249022928238E-17));
#123492=DIRECTION('ref_axis',(0.7431448254774,0.669130606358852,-9.95814315644137E-34));
#123493=DIRECTION('center_axis',(0.669130606358845,-0.743144825477406,-3.65592620896146E-14));
#123494=DIRECTION('ref_axis',(0.743144825477406,0.669130606358845,9.99649599890217E-31));
#123495=DIRECTION('center_axis',(0.669130606358852,-0.7431448254774,-9.42249022928238E-17));
#123496=DIRECTION('ref_axis',(0.7431448254774,0.669130606358852,-9.95814315644137E-34));
#123497=DIRECTION('center_axis',(-0.669130606358845,0.743144825477406,0.));
#123498=DIRECTION('ref_axis',(-0.743144825477406,-0.669130606358845,0.));
#123499=DIRECTION('center_axis',(0.354588510146745,-0.393810436983627,-0.848045003637588));
#123500=DIRECTION('ref_axis',(-1.32348946953629E-15,0.90697822335777,-0.421177518814553));
#123501=DIRECTION('center_axis',(-0.334568754912041,0.371576246276148,0.866022425483275));
#123502=DIRECTION('ref_axis',(6.8466508941702E-15,-0.91898213146363,0.394299178353905));
#123503=DIRECTION('center_axis',(-0.354588475158959,0.393810430457258,0.848045021297521));
#123504=DIRECTION('ref_axis',(-0.564245025055314,0.633098037506755,-0.529919264233169));
#123505=DIRECTION('center_axis',(0.354588472592002,-0.39381039527486,-0.848045038708635));
#123506=DIRECTION('ref_axis',(-2.66687128082441E-15,0.906978247051286,-0.421177467792113));
#123507=DIRECTION('center_axis',(-0.334568756370059,0.371576263602952,0.866022417485749));
#123508=DIRECTION('ref_axis',(-0.576095872880217,0.646617000434065,-0.500000000000033));
#123509=DIRECTION('center_axis',(-0.579517695131992,0.643568108591923,0.499979330205078));
#123510=DIRECTION('ref_axis',(0.335267672822139,-0.370911831413928,0.866036951219515));
#123511=DIRECTION('center_axis',(0.743307065001336,0.668950377172403,0.));
#123512=DIRECTION('ref_axis',(-0.668950377172402,0.743307065001336,0.));
#123513=DIRECTION('center_axis',(0.669130606358852,-0.7431448254774,-9.42249022928238E-17));
#123514=DIRECTION('ref_axis',(0.7431448254774,0.669130606358852,-9.95814315644137E-34));
#123515=DIRECTION('center_axis',(-0.669130606358872,0.743144825477382,0.));
#123516=DIRECTION('ref_axis',(-0.743144825477382,-0.669130606358872,0.));
#123517=DIRECTION('center_axis',(-2.35041809182734E-16,1.0464735569497E-16,
-1.));
#123518=DIRECTION('ref_axis',(-1.,-1.56586024251259E-33,2.25664243350207E-16));
#123519=DIRECTION('center_axis',(0.742982542253406,0.669310796197601,0.));
#123520=DIRECTION('ref_axis',(-0.669310796197601,0.742982542253406,0.));
#123521=DIRECTION('center_axis',(-0.35458882032884,0.393810781475744,-0.848044713969297));
#123522=DIRECTION('ref_axis',(-2.60913257636008E-15,0.906978027661821,0.421177940232716));
#123523=DIRECTION('center_axis',(-0.354588472592004,0.393810395274862,0.848045038708633));
#123524=DIRECTION('ref_axis',(1.64363307278047E-15,-0.906978247051285,0.421177467792116));
#123525=DIRECTION('center_axis',(-0.35458886088619,0.393810788844712,-0.848044693589282));
#123526=DIRECTION('ref_axis',(0.564077964590569,-0.633246889655141,-0.529919264233195));
#123527=DIRECTION('center_axis',(-0.354588864042363,0.393810830024498,-0.848044673146741));
#123528=DIRECTION('ref_axis',(3.00368387037336E-15,0.90697800008266,0.421177999622557));
#123529=DIRECTION('center_axis',(0.354588475222375,-0.393810430613248,-0.848045021198568));
#123530=DIRECTION('ref_axis',(-0.570650194825298,0.627330796741533,-0.529919264233225));
#123531=DIRECTION('center_axis',(-0.354588510146774,0.393810436983659,0.848045003637561));
#123532=DIRECTION('ref_axis',(-5.40566344552556E-15,-0.906978223357753,
0.42117751881459));
#123533=DIRECTION('center_axis',(0.743317556935089,0.668938718831591,-4.06383359288233E-15));
#123534=DIRECTION('ref_axis',(-0.668938718831591,0.743317556935089,4.57642320323792E-30));
#123535=DIRECTION('center_axis',(-0.669130606358845,0.743144825477406,0.));
#123536=DIRECTION('ref_axis',(-0.743144825477406,-0.669130606358845,0.));
#123537=DIRECTION('center_axis',(-2.35041809182734E-16,1.0464735569497E-16,
-1.));
#123538=DIRECTION('ref_axis',(-1.,0.,2.40228573745067E-16));
#123539=DIRECTION('center_axis',(0.742972044483923,0.669322449283885,-4.02398997762833E-15));
#123540=DIRECTION('ref_axis',(-0.669322449283885,0.742972044483923,8.70403636810736E-29));
#123541=DIRECTION('center_axis',(-0.669130606358852,0.7431448254774,9.42249022928238E-17));
#123542=DIRECTION('ref_axis',(-0.7431448254774,-0.669130606358852,-8.60592964647315E-31));
#123543=DIRECTION('center_axis',(-0.579456972966213,0.643597063368616,-0.500012436349466));
#123544=DIRECTION('ref_axis',(-0.335308969664714,0.370919252616137,0.866017784402304));
#123545=DIRECTION('center_axis',(0.354588864042318,-0.393810830024549,0.848044673146736));
#123546=DIRECTION('ref_axis',(-3.66609196403161E-15,-0.906978000082638,
-0.421177999622604));
#123547=DIRECTION('center_axis',(0.334568662771634,-0.371576128829216,0.866022511471552));
#123548=DIRECTION('ref_axis',(0.582802983770213,-0.640578396535943,-0.499999999999977));
#123549=DIRECTION('center_axis',(-0.334568664232029,0.371576145565791,-0.866022503726356));
#123550=DIRECTION('ref_axis',(4.84407888932722E-15,0.918982183096544,0.394299058014485));
#123551=DIRECTION('center_axis',(0.354588860819346,-0.393810788643603,0.848044693710622));
#123552=DIRECTION('ref_axis',(0.570815694137047,-0.627180210722105,-0.529919264233163));
#123553=DIRECTION('center_axis',(0.354588820328778,-0.393810781475744,0.848044713969322));
#123554=DIRECTION('ref_axis',(6.08911365345571E-15,-0.906978027661825,-0.421177940232708));
#123555=DIRECTION('center_axis',(-0.669130606358845,0.743144825477406,-4.06031740096479E-14));
#123556=DIRECTION('ref_axis',(-0.743144825477406,-0.669130606358845,-1.17388982313054E-30));
#123557=DIRECTION('center_axis',(0.669130606358872,-0.743144825477382,0.));
#123558=DIRECTION('ref_axis',(0.743144825477382,0.669130606358872,0.));
#123559=DIRECTION('center_axis',(-0.669130606358852,0.7431448254774,9.42249022928238E-17));
#123560=DIRECTION('ref_axis',(-0.7431448254774,-0.669130606358852,-8.60592964647315E-31));
#123561=DIRECTION('center_axis',(-0.669130606358845,0.743144825477406,-3.65592620896146E-14));
#123562=DIRECTION('ref_axis',(-0.743144825477406,-0.669130606358845,9.99649599890217E-31));
#123563=DIRECTION('center_axis',(-0.669130606358852,0.7431448254774,9.42249022928238E-17));
#123564=DIRECTION('ref_axis',(-0.7431448254774,-0.669130606358852,-8.60592964647315E-31));
#123565=DIRECTION('center_axis',(0.579466481046707,-0.643614221961464,-0.499979330205044));
#123566=DIRECTION('ref_axis',(-0.333834922946263,0.372201885196569,-0.86603695121951));
#123567=DIRECTION('center_axis',(-0.334568754912033,0.371576246276138,0.866022425483283));
#123568=DIRECTION('ref_axis',(4.15067265588782E-15,-0.918982131463635,0.394299178353892));
#123569=DIRECTION('center_axis',(-0.334568760918544,0.37157625294706,0.866022420300568));
#123570=DIRECTION('ref_axis',(0.74314482547537,0.669130606361107,-1.78335036602841E-12));
#123571=DIRECTION('center_axis',(0.293895573515143,-0.404512553892808,0.866022508720948));
#123572=DIRECTION('ref_axis',(-0.809016994373897,-0.587785252293919,-1.08399728638205E-12));
#123573=DIRECTION('center_axis',(0.509057044367757,-0.700605801485709,0.500012436349469));
#123574=DIRECTION('ref_axis',(0.293099122173842,-0.405100113157068,-0.866017784402292));
#123575=DIRECTION('center_axis',(-0.293895578600024,0.404512560891464,-0.86602250372631));
#123576=DIRECTION('ref_axis',(5.57115822586198E-15,0.906035256115484,0.423202214875761));
#123577=DIRECTION('center_axis',(-0.58778525229247,0.80901699437495,0.));
#123578=DIRECTION('ref_axis',(-0.80901699437495,-0.58778525229247,0.));
#123579=DIRECTION('center_axis',(0.587785252292466,-0.809016994374953,-8.27701011433307E-17));
#123580=DIRECTION('ref_axis',(0.809016994374953,0.587785252292466,-1.11448779222234E-32));
#123581=DIRECTION('center_axis',(0.58778525229247,-0.80901699437495,0.));
#123582=DIRECTION('ref_axis',(0.80901699437495,0.58778525229247,0.));
#123583=DIRECTION('center_axis',(0.587785252292466,-0.809016994374953,-8.27701011433307E-17));
#123584=DIRECTION('ref_axis',(0.809016994374953,0.587785252292466,3.81297860563151E-33));
#123585=DIRECTION('center_axis',(-0.58778525229247,0.80901699437495,0.));
#123586=DIRECTION('ref_axis',(-0.80901699437495,-0.58778525229247,0.));
#123587=DIRECTION('center_axis',(0.311481637390299,-0.428717694262769,-0.848045003637586));
#123588=DIRECTION('ref_axis',(-4.11382121094243E-15,0.892442058026266,-0.451162025292292));
#123589=DIRECTION('center_axis',(-0.293895658256123,0.404512670528733,0.866022425483262));
#123590=DIRECTION('ref_axis',(-8.25691251523047E-15,-0.90603519747347,0.423202340422653));
#123591=DIRECTION('center_axis',(-0.311481603280472,0.428717684111969,0.848045021297511));
#123592=DIRECTION('ref_axis',(-0.494977266816266,0.688609525587369,-0.529919264233183));
#123593=DIRECTION('center_axis',(0.311481604401019,-0.428717648856921,-0.848045038708653));
#123594=DIRECTION('ref_axis',(-7.59295483192656E-15,0.892442084777736,-0.451161972375298));
#123595=DIRECTION('center_axis',(-0.293895657887586,0.404512687918341,0.866022417485773));
#123596=DIRECTION('ref_axis',(-0.505350078017002,0.703293181147248,-0.499999999999994));
#123597=DIRECTION('center_axis',(-0.509071851162815,0.700618669263933,0.49997933020526));
#123598=DIRECTION('ref_axis',(0.294660197713809,-0.403924952195204,0.866036951219381));
#123599=DIRECTION('center_axis',(0.809159506053914,0.587589051772227,0.));
#123600=DIRECTION('ref_axis',(-0.587589051772227,0.809159506053914,0.));
#123601=DIRECTION('center_axis',(0.587785252292466,-0.809016994374953,-8.27701011433307E-17));
#123602=DIRECTION('ref_axis',(0.809016994374953,0.587785252292466,-1.11448779222234E-32));
#123603=DIRECTION('center_axis',(-0.58778525229247,0.80901699437495,0.));
#123604=DIRECTION('ref_axis',(-0.80901699437495,-0.58778525229247,0.));
#123605=DIRECTION('center_axis',(-2.23587008033241E-16,1.13923270769253E-16,
-1.));
#123606=DIRECTION('ref_axis',(-1.,-3.91465060628147E-34,2.25664243350207E-16));
#123607=DIRECTION('center_axis',(0.808874435122379,0.587981418248444,0.));
#123608=DIRECTION('ref_axis',(-0.587981418248444,0.808874435122379,0.));
#123609=DIRECTION('center_axis',(-0.311481909863932,0.428718069290522,-0.848044713969331));
#123610=DIRECTION('ref_axis',(9.11251128025232E-15,0.892441837073405,0.451162462358124));
#123611=DIRECTION('center_axis',(-0.311481604401018,0.428717648856998,0.848045038708615));
#123612=DIRECTION('ref_axis',(2.45085461175841E-15,-0.892442084777695,0.451161972375377));
#123613=DIRECTION('center_axis',(-0.311481949435979,0.428718080853434,-0.848044693589265));
#123614=DIRECTION('ref_axis',(0.494795562220743,-0.688740099748264,-0.529919264233157));
#123615=DIRECTION('center_axis',(-0.311481948263276,0.428718122142686,-0.848044673146741));
#123616=DIRECTION('ref_axis',(2.81035723410834E-16,0.892441805934784,0.451162523953244));
#123617=DIRECTION('center_axis',(0.311481603324408,-0.428717684275746,-0.848045021198579));
#123618=DIRECTION('ref_axis',(-0.501950189202811,0.683543400929142,-0.529919264233227));
#123619=DIRECTION('center_axis',(-0.311481637390294,0.428717694262762,0.848045003637591));
#123620=DIRECTION('ref_axis',(6.8200989747602E-15,-0.89244205802627,0.451162025292285));
#123621=DIRECTION('center_axis',(0.809168721883286,0.587576360591345,-1.21071329521341E-14));
#123622=DIRECTION('ref_axis',(-0.587576360591345,0.809168721883286,-3.03871162902842E-28));
#123623=DIRECTION('center_axis',(-0.58778525229247,0.80901699437495,0.));
#123624=DIRECTION('ref_axis',(-0.80901699437495,-0.58778525229247,0.));
#123625=DIRECTION('center_axis',(-2.23587008033241E-16,1.13923270769253E-16,
-1.));
#123626=DIRECTION('ref_axis',(-1.,1.25019043942798E-33,2.40228573745067E-16));
#123627=DIRECTION('center_axis',(0.808865212939984,0.587994104813606,0.));
#123628=DIRECTION('ref_axis',(-0.587994104813606,0.808865212939984,0.));
#123629=DIRECTION('center_axis',(-0.587785252292466,0.809016994374953,8.27701011433307E-17));
#123630=DIRECTION('ref_axis',(-0.809016994374953,-0.587785252292466,-1.27906067821219E-31));
#123631=DIRECTION('center_axis',(-0.509008435042523,0.70064111822839,-0.500012436348571));
#123632=DIRECTION('ref_axis',(-0.294700492564884,0.403936649463788,0.866017784402828));
#123633=DIRECTION('center_axis',(0.31148194826325,-0.428718122142728,0.848044673146729));
#123634=DIRECTION('ref_axis',(7.04633136982833E-16,-0.892441805934763,-0.451162523953285));
#123635=DIRECTION('center_axis',(0.293895578900055,-0.40451254409162,0.866022511471571));
#123636=DIRECTION('ref_axis',(0.512651652657614,-0.697988741332897,-0.499999999999935));
#123637=DIRECTION('center_axis',(-0.293895578599974,0.404512560891423,-0.866022503726346));
#123638=DIRECTION('ref_axis',(3.81388142168972E-15,0.906035256115507,0.423202214875711));
#123639=DIRECTION('center_axis',(0.311481949380144,-0.428718080653948,0.848044693710621));
#123640=DIRECTION('ref_axis',(0.502130522403619,-0.683410939234349,-0.529919264233236));
#123641=DIRECTION('center_axis',(0.311481909863867,-0.428718069290581,0.848044713969325));
#123642=DIRECTION('ref_axis',(-4.71143346943765E-15,-0.892441837073378,
-0.451162462358177));
#123643=DIRECTION('center_axis',(-0.58778525229247,0.80901699437495,0.));
#123644=DIRECTION('ref_axis',(-0.80901699437495,-0.58778525229247,0.));
#123645=DIRECTION('center_axis',(0.587785252292496,-0.809016994374931,0.));
#123646=DIRECTION('ref_axis',(0.809016994374931,0.587785252292496,0.));
#123647=DIRECTION('center_axis',(-0.587785252292466,0.809016994374953,8.27701011433307E-17));
#123648=DIRECTION('ref_axis',(-0.809016994374953,-0.587785252292466,-1.27906067821219E-31));
#123649=DIRECTION('center_axis',(-0.58778525229247,0.80901699437495,1.20874298148573E-14));
#123650=DIRECTION('ref_axis',(-0.80901699437495,-0.58778525229247,-1.84071433653408E-31));
#123651=DIRECTION('center_axis',(-0.587785252292466,0.809016994374953,8.27701011433307E-17));
#123652=DIRECTION('ref_axis',(-0.809016994374953,-0.587785252292466,-1.27906067821219E-31));
#123653=DIRECTION('center_axis',(0.509016097474312,-0.700659176689658,-0.499979330205352));
#123654=DIRECTION('ref_axis',(-0.293100449226779,0.405058175804142,-0.866036951219335));
#123655=DIRECTION('center_axis',(-0.293895658256093,0.404512670528665,0.866022425483304));
#123656=DIRECTION('ref_axis',(1.1317083799287E-15,-0.906035197473503,0.42320234042258));
#123657=DIRECTION('center_axis',(-0.293895663531789,0.404512677790057,0.866022420301188));
#123658=DIRECTION('ref_axis',(0.809016994371241,0.587785252297575,-3.67160369476059E-12));
#123659=DIRECTION('center_axis',(0.250002507181632,-0.433017044458199,0.866022508721098));
#123660=DIRECTION('ref_axis',(-0.866025403784408,-0.500000000000054,-3.49676543996346E-14));
#123661=DIRECTION('center_axis',(0.433035128829457,-0.749978760163043,0.500012436349297));
#123662=DIRECTION('ref_axis',(0.249149002268627,-0.433518133146968,-0.866017784402443));
#123663=DIRECTION('center_axis',(-0.25000251150716,0.433017051950293,-0.866022503726312));
#123664=DIRECTION('ref_axis',(3.51864076615538E-15,0.894424794863778,0.447218387740138));
#123665=DIRECTION('center_axis',(-0.500000000000022,0.866025403784426,0.));
#123666=DIRECTION('ref_axis',(-0.866025403784426,-0.500000000000022,0.));
#123667=DIRECTION('center_axis',(0.499999999999992,-0.866025403784443,-7.04084534449541E-17));
#123668=DIRECTION('ref_axis',(0.866025403784443,0.499999999999992,-1.7712134304101E-32));
#123669=DIRECTION('center_axis',(0.50000000000001,-0.866025403784433,1.36592399683214E-14));
#123670=DIRECTION('ref_axis',(0.866025403784433,0.50000000000001,3.78074180857848E-32));
#123671=DIRECTION('center_axis',(0.499999999999992,-0.866025403784443,-7.04084534449541E-17));
#123672=DIRECTION('ref_axis',(0.866025403784443,0.499999999999992,-1.7712134304101E-32));
#123673=DIRECTION('center_axis',(-0.50000000000001,0.866025403784433,0.));
#123674=DIRECTION('ref_axis',(-0.866025403784433,-0.50000000000001,0.));
#123675=DIRECTION('center_axis',(0.264962106632875,-0.45892783076861,-0.848045003637594));
#123676=DIRECTION('ref_axis',(-1.43964512713556E-15,0.879478602053341,-0.475938429348064));
#123677=DIRECTION('center_axis',(-0.25000257926675,0.433017169313245,0.866022425483265));
#123678=DIRECTION('ref_axis',(-1.3082911094407E-15,-0.8944247302164,0.44721851703314));
#123679=DIRECTION('center_axis',(-0.264962073769681,0.458927817108741,0.848045021297499));
#123680=DIRECTION('ref_axis',(-0.42028643404606,0.736576463614905,-0.529919264233154));
#123681=DIRECTION('center_axis',(0.264962078570529,-0.458927782163201,-0.848045038708647));
#123682=DIRECTION('ref_axis',(-1.89361858943742E-15,0.879478631391252,-0.475938375135028));
#123683=DIRECTION('center_axis',(-0.250002577084016,0.433017186568188,0.866022417485784));
#123684=DIRECTION('ref_axis',(-0.429067561962739,0.752263934581071,-0.499999999999957));
#123685=DIRECTION('center_axis',(-0.433048509462457,0.749993105181608,0.499979330205154));
#123686=DIRECTION('ref_axis',(0.250824363778504,-0.432512586704271,0.866036951219455));
#123687=DIRECTION('center_axis',(0.866146626230631,0.499789977759954,0.));
#123688=DIRECTION('ref_axis',(-0.499789977759954,0.866146626230631,0.));
#123689=DIRECTION('center_axis',(0.499999999999992,-0.866025403784443,-7.04084534449541E-17));
#123690=DIRECTION('ref_axis',(0.866025403784443,0.499999999999992,-1.7712134304101E-32));
#123691=DIRECTION('center_axis',(-0.499999999999998,0.86602540378444,0.));
#123692=DIRECTION('ref_axis',(-0.86602540378444,-0.499999999999998,0.));
#123693=DIRECTION('center_axis',(-2.11225360334865E-16,1.21951018649011E-16,
-1.));
#123694=DIRECTION('ref_axis',(-1.,1.17439518188444E-33,2.25664243350207E-16));
#123695=DIRECTION('center_axis',(0.865904130412297,0.500209992837931,0.));
#123696=DIRECTION('ref_axis',(-0.500209992837931,0.865904130412297,0.));
#123697=DIRECTION('center_axis',(-0.264962338412774,0.458928232223215,-0.848044713969322));
#123698=DIRECTION('ref_axis',(6.42968295905551E-16,0.87947835973774,0.475938877118706));
#123699=DIRECTION('center_axis',(-0.264962078570521,0.458927782163201,0.848045038708649));
#123700=DIRECTION('ref_axis',(2.043795734415E-15,-0.879478631391252,0.475938375135027));
#123701=DIRECTION('center_axis',(-0.264962376552941,0.45892824786285,-0.84804469358929));
#123702=DIRECTION('ref_axis',(0.420092076162084,-0.736687329156922,-0.529919264233213));
#123703=DIRECTION('center_axis',(-0.264962371077221,0.458928288799652,-0.848044673146739));
#123704=DIRECTION('ref_axis',(-5.61404975480703E-15,0.87947832558851,0.475938940222411));
#123705=DIRECTION('center_axis',(0.264962073787568,-0.458927817281253,-0.848045021198554));
#123706=DIRECTION('ref_axis',(-0.427750712267922,0.732266960574363,-0.529919264233213));
#123707=DIRECTION('center_axis',(-0.264962106632886,0.458927830768643,0.848045003637573));
#123708=DIRECTION('ref_axis',(3.30353726242757E-15,-0.879478602053321,0.4759384293481));
#123709=DIRECTION('center_axis',(0.86615446498511,0.499776392786171,0.));
#123710=DIRECTION('ref_axis',(-0.499776392786171,0.86615446498511,0.));
#123711=DIRECTION('center_axis',(-0.50000000000001,0.866025403784433,0.));
#123712=DIRECTION('ref_axis',(-0.866025403784433,-0.50000000000001,0.));
#123713=DIRECTION('center_axis',(-2.11225360334865E-16,1.21951018649011E-16,
-1.));
#123714=DIRECTION('ref_axis',(-1.,2.81292848871296E-33,2.40228573745067E-16));
#123715=DIRECTION('center_axis',(0.865896284857143,0.500223573885315,-2.73306953340429E-14));
#123716=DIRECTION('ref_axis',(-0.500223573885315,0.865896284857143,-4.47025834271801E-28));
#123717=DIRECTION('center_axis',(-0.499999999999992,0.866025403784443,7.04084534449541E-17));
#123718=DIRECTION('ref_axis',(-0.866025403784443,-0.499999999999992,-6.94743527014557E-31));
#123719=DIRECTION('center_axis',(-0.432983094185233,0.750008802378944,-0.500012436349222));
#123720=DIRECTION('ref_axis',(-0.250863215139369,0.43252843188453,0.866017784402519));
#123721=DIRECTION('center_axis',(0.264962371077185,-0.458928288799684,0.848044673146733));
#123722=DIRECTION('ref_axis',(-2.53116482579111E-15,-0.879478325588496,
-0.475938940222437));
#123723=DIRECTION('center_axis',(0.250002513560361,-0.433017035274593,0.866022511471557));
#123724=DIRECTION('ref_axis',(0.436883602752815,-0.747751775421316,-0.499999999999991));
#123725=DIRECTION('center_axis',(-0.250002511507164,0.43301705195022,-0.866022503726347));
#123726=DIRECTION('ref_axis',(-4.94285822981357E-15,0.894424794863815,0.447218387740065));
#123727=DIRECTION('center_axis',(0.264962376523978,-0.458928247655394,0.848044693710606));
#123728=DIRECTION('ref_axis',(0.427943903610924,-0.732154074465734,-0.529919264233212));
#123729=DIRECTION('center_axis',(0.264962338412787,-0.458928232223194,0.848044713969329));
#123730=DIRECTION('ref_axis',(5.019182273909E-15,-0.87947835973775,-0.475938877118687));
#123731=DIRECTION('center_axis',(-0.50000000000001,0.866025403784433,6.09762352041363E-14));
#123732=DIRECTION('ref_axis',(-0.866025403784433,-0.50000000000001,2.00105264687255E-32));
#123733=DIRECTION('center_axis',(0.499999999999998,-0.86602540378444,0.));
#123734=DIRECTION('ref_axis',(0.86602540378444,0.499999999999998,0.));
#123735=DIRECTION('center_axis',(-0.499999999999992,0.866025403784443,7.04084534449541E-17));
#123736=DIRECTION('ref_axis',(-0.866025403784443,-0.499999999999992,-6.94743527014557E-31));
#123737=DIRECTION('center_axis',(-0.50000000000001,0.866025403784433,-2.73184799366427E-14));
#123738=DIRECTION('ref_axis',(-0.866025403784433,-0.50000000000001,-7.56148361715697E-32));
#123739=DIRECTION('center_axis',(-0.499999999999992,0.866025403784443,7.04084534449541E-17));
#123740=DIRECTION('ref_axis',(-0.866025403784443,-0.499999999999992,-6.94743527014557E-31));
#123741=DIRECTION('center_axis',(0.432988827019321,-0.750027562856135,-0.499979330205279));
#123742=DIRECTION('ref_axis',(-0.249154705643646,0.433476564278025,-0.866036951219373));
#123743=DIRECTION('center_axis',(-0.250002579266693,0.433017169313166,0.866022425483321));
#123744=DIRECTION('ref_axis',(-6.80109926771202E-15,-0.894424730216445,
0.447218517033049));
#123745=DIRECTION('center_axis',(-0.250002583755051,0.433017177087239,0.866022420300536));
#123746=DIRECTION('ref_axis',(0.866025403785887,0.499999999997491,1.67844740332471E-12));
#123747=DIRECTION('center_axis',(0.203370361064481,-0.456777309673029,0.866022508719244));
#123748=DIRECTION('ref_axis',(-0.913545457641425,-0.406736643078441,-1.67844741116904E-12));
#123749=DIRECTION('center_axis',(0.352268789800274,-0.791134794601849,0.500012436348278));
#123750=DIRECTION('ref_axis',(0.202469153659259,-0.457186437806557,-0.866017784402985));
#123751=DIRECTION('center_axis',(-0.203370364581913,0.456777317573275,-0.866022503726308));
#123752=DIRECTION('ref_axis',(-5.36134519175288E-15,0.884507036382097,0.466526850878446));
#123753=DIRECTION('center_axis',(-0.406736643075807,0.913545457642598,0.));
#123754=DIRECTION('ref_axis',(-0.913545457642598,-0.406736643075807,0.));
#123755=DIRECTION('center_axis',(0.406736643075792,-0.913545457642605,-5.72753959967185E-17));
#123756=DIRECTION('ref_axis',(0.913545457642605,0.406736643075792,-7.24473849677094E-34));
#123757=DIRECTION('center_axis',(0.406736643075807,-0.913545457642598,0.));
#123758=DIRECTION('ref_axis',(0.913545457642598,0.406736643075807,0.));
#123759=DIRECTION('center_axis',(0.406736643075792,-0.913545457642605,-5.72753959967185E-17));
#123760=DIRECTION('ref_axis',(0.913545457642605,0.406736643075792,-7.24473849677094E-34));
#123761=DIRECTION('center_axis',(-0.406736643075751,0.913545457642623,0.));
#123762=DIRECTION('ref_axis',(-0.913545457642623,-0.406736643075751,0.));
#123763=DIRECTION('center_axis',(0.215539595588322,-0.484109857923806,-0.848045003637552));
#123764=DIRECTION('ref_axis',(-1.22051060460069E-15,0.868458021515973,-0.495762710240052));
#123765=DIRECTION('center_axis',(-0.20337041970245,0.456777441376077,0.866022425483297));
#123766=DIRECTION('ref_axis',(2.19291865361494E-15,-0.884506966812057,0.466526982779061));
#123767=DIRECTION('center_axis',(-0.215539564334464,0.484109840902905,0.848045021297498));
#123768=DIRECTION('ref_axis',(-0.340990855184624,0.776473315752058,-0.529919264233207));
#123769=DIRECTION('center_axis',(0.215539572760323,-0.484109806651279,-0.848045038708652));
#123770=DIRECTION('ref_axis',(-1.14521404331846E-15,0.868458052949962,-0.495762655175196));
#123771=DIRECTION('center_axis',(-0.203370415731982,0.456777458306689,0.866022417485761));
#123772=DIRECTION('ref_axis',(-0.348084091918818,0.792992726923176,-0.499999999999997));
#123773=DIRECTION('center_axis',(-0.352280597671314,0.791150459692796,0.499979330204979));
#123774=DIRECTION('ref_axis',(0.204240445642938,-0.456361522792971,0.866036951219551));
#123775=DIRECTION('center_axis',(0.913644062717554,0.406515100163527,-2.49593669965817E-14));
#123776=DIRECTION('ref_axis',(-0.406515100163527,0.913644062717554,2.93346074380205E-28));
#123777=DIRECTION('center_axis',(0.406736643075792,-0.913545457642605,-5.72753959967185E-17));
#123778=DIRECTION('ref_axis',(0.913545457642605,0.406736643075792,-7.24473849677094E-34));
#123779=DIRECTION('center_axis',(-0.406736643075807,0.913545457642598,0.));
#123780=DIRECTION('ref_axis',(-0.913545457642598,-0.406736643075807,0.));
#123781=DIRECTION('center_axis',(-1.98092302886629E-16,1.28642645648559E-16,
-1.));
#123782=DIRECTION('ref_axis',(-1.,2.74025542439703E-33,2.25664243350207E-16));
#123783=DIRECTION('center_axis',(0.913446798847323,0.406958162070229,0.));
#123784=DIRECTION('ref_axis',(-0.406958162070229,0.913446798847323,0.));
#123785=DIRECTION('center_axis',(-0.215539784135063,0.484110281406767,-0.8480447139693));
#123786=DIRECTION('ref_axis',(-1.11523192825129E-16,0.868457761888259,0.495763165045606));
#123787=DIRECTION('center_axis',(-0.215539572760323,0.484109806651281,0.848045038708651));
#123788=DIRECTION('ref_axis',(6.78208419898497E-16,-0.868458052949962,0.495762655175198));
#123789=DIRECTION('center_axis',(-0.215539820430813,0.484110300947715,-0.848044693589297));
#123790=DIRECTION('ref_axis',(0.340785973389205,-0.776563258038715,-0.529919264233212));
#123791=DIRECTION('center_axis',(-0.215539810706713,0.484110341087608,-0.848044673146736));
#123792=DIRECTION('ref_axis',(-4.23381048949575E-15,0.86845772529927,0.495763229140704));
#123793=DIRECTION('center_axis',(0.215539564338691,-0.484109841074344,-0.848045021198557));
#123794=DIRECTION('ref_axis',(-0.348864709029164,0.772967650156545,-0.529919264233209));
#123795=DIRECTION('center_axis',(-0.215539595588306,0.48410985792377,0.848045003637576));
#123796=DIRECTION('ref_axis',(5.65310087418454E-16,-0.868458021515995,0.495762710240013));
#123797=DIRECTION('center_axis',(0.913650438514074,0.406500770236713,0.));
#123798=DIRECTION('ref_axis',(-0.406500770236713,0.913650438514073,0.));
#123799=DIRECTION('center_axis',(-0.406736643075807,0.913545457642598,3.88019196882762E-14));
#123800=DIRECTION('ref_axis',(-0.913545457642598,-0.406736643075807,-7.82081982317031E-31));
#123801=DIRECTION('center_axis',(-1.98092302886629E-16,1.28642645648559E-16,
-1.));
#123802=DIRECTION('ref_axis',(-1.,4.68821414785493E-33,2.40228573745067E-16));
#123803=DIRECTION('center_axis',(0.913440415876957,0.406972488803028,-2.49538036744541E-14));
#123804=DIRECTION('ref_axis',(-0.406972488803028,0.913440415876957,1.34873736753699E-28));
#123805=DIRECTION('center_axis',(-0.406736643075792,0.913545457642605,5.72753959967185E-17));
#123806=DIRECTION('ref_axis',(-0.913545457642605,-0.406736643075792,-5.10634159526644E-31));
#123807=DIRECTION('center_axis',(-0.352213899942141,0.7911592331408,-0.500012436348947));
#123808=DIRECTION('ref_axis',(-0.204277427990782,0.456381342203981,0.866017784402586));
#123809=DIRECTION('center_axis',(0.215539810706706,-0.484110341087606,0.848044673146739));
#123810=DIRECTION('ref_axis',(4.86428769523775E-15,-0.868457725299271,-0.495763229140701));
#123811=DIRECTION('center_axis',(0.203370368362508,-0.456777301205554,0.866022511471537));
#123812=DIRECTION('ref_axis',(0.35632896466816,-0.789322284582468,-0.500000000000031));
#123813=DIRECTION('center_axis',(-0.203370364581893,0.456777317573231,-0.866022503726336));
#123814=DIRECTION('ref_axis',(-1.22569712450493E-15,0.884507036382122,0.466526850878399));
#123815=DIRECTION('center_axis',(0.215539820427113,-0.484110300736857,0.848044693710607));
#123816=DIRECTION('ref_axis',(0.349068641869984,-0.772875576440095,-0.529919264233181));
#123817=DIRECTION('center_axis',(0.215539784134997,-0.48411028140675,0.848044713969326));
#123818=DIRECTION('ref_axis',(-3.99144860726419E-15,-0.868457761888273,
-0.495763165045581));
#123819=DIRECTION('center_axis',(-0.406736643075807,0.913545457642598,1.11114268233636E-14));
#123820=DIRECTION('ref_axis',(-0.913545457642598,-0.406736643075807,-1.88066567154315E-32));
#123821=DIRECTION('center_axis',(0.406736643075751,-0.913545457642623,0.));
#123822=DIRECTION('ref_axis',(0.913545457642623,0.406736643075751,0.));
#123823=DIRECTION('center_axis',(-0.406736643075792,0.913545457642605,5.72753959967185E-17));
#123824=DIRECTION('ref_axis',(-0.913545457642605,-0.406736643075792,-5.10634159526644E-31));
#123825=DIRECTION('center_axis',(-0.406736643075807,0.913545457642598,2.76904928649126E-14));
#123826=DIRECTION('ref_axis',(-0.913545457642598,-0.406736643075807,1.39870556442785E-30));
#123827=DIRECTION('center_axis',(-0.406736643075792,0.913545457642605,5.72753959967185E-17));
#123828=DIRECTION('ref_axis',(-0.913545457642605,-0.406736643075792,-5.10634159526644E-31));
#123829=DIRECTION('center_axis',(0.352217640366456,-0.791178490090896,-0.499979330204935));
#123830=DIRECTION('ref_axis',(-0.202479170974534,0.457145692798004,-0.866036951219576));
#123831=DIRECTION('center_axis',(-0.203370419702469,0.45677744137607,0.866022425483297));
#123832=DIRECTION('ref_axis',(-6.1956980622853E-15,-0.884506966812061,0.466526982779054));
#123833=DIRECTION('center_axis',(-0.203370423351418,0.456777449571772,0.866022420303639));
#123834=DIRECTION('ref_axis',(0.913545457643787,0.406736643073135,1.67844740332474E-12));
#123835=DIRECTION('center_axis',(0.154510046710178,-0.475533027088194,0.866022508722469));
#123836=DIRECTION('ref_axis',(-0.951056516294165,-0.309016994377989,-1.85328568317356E-12));
#123837=DIRECTION('center_axis',(0.267642920194485,-0.823622990674322,0.500012436347791));
#123838=DIRECTION('ref_axis',(0.153571010689768,-0.475845712151499,-0.866017784403274));
#123839=DIRECTION('center_axis',(-0.154510049384264,0.475533035318155,-0.866022503726303));
#123840=DIRECTION('ref_axis',(-4.8539766534288E-15,0.876548788012427,0.481313018974082));
#123841=DIRECTION('center_axis',(-0.309016994374914,0.951056516295165,0.));
#123842=DIRECTION('ref_axis',(-0.951056516295164,-0.309016994374914,0.));
#123843=DIRECTION('center_axis',(0.309016994374938,-0.951056516295157,-4.35148173242957E-17));
#123844=DIRECTION('ref_axis',(0.951056516295157,0.309016994374938,-2.85097203607405E-33));
#123845=DIRECTION('center_axis',(0.309016994374914,-0.951056516295164,-6.04047112789604E-14));
#123846=DIRECTION('ref_axis',(0.951056516295164,0.309016994374914,2.74316558509634E-30));
#123847=DIRECTION('center_axis',(0.309016994374938,-0.951056516295157,-4.35148173242957E-17));
#123848=DIRECTION('ref_axis',(0.951056516295157,0.309016994374938,-2.85097203607405E-33));
#123849=DIRECTION('center_axis',(-0.30901699437498,0.951056516295143,0.));
#123850=DIRECTION('ref_axis',(-0.951056516295143,-0.30901699437498,0.));
#123851=DIRECTION('center_axis',(0.163755587629875,-0.503987876168985,-0.848045003637584));
#123852=DIRECTION('ref_axis',(3.02936709568593E-15,0.859649462041489,-0.510884333691862));
#123853=DIRECTION('center_axis',(-0.154510091261946,0.475533164204408,0.866022425483295));
#123854=DIRECTION('ref_axis',(-2.02831240586475E-15,-0.876548714628839,
0.481313152617431));
#123855=DIRECTION('center_axis',(-0.163755558330189,0.50398785597322,0.848045021297505));
#123856=DIRECTION('ref_axis',(-0.25795930913709,0.807862963765557,-0.52991926423319));
#123857=DIRECTION('center_axis',(0.163755570286389,-0.503987822791223,-0.848045038708642));
#123858=DIRECTION('ref_axis',(-4.55251793567526E-15,0.859649495083692,-0.510884278092753));
#123859=DIRECTION('center_axis',(-0.154510085538992,0.475533180628678,0.866022417485775));
#123860=DIRECTION('ref_axis',(-0.263286939707607,0.825033325011428,-0.49999999999999));
#123861=DIRECTION('center_axis',(-0.267653025932399,0.823639804208775,0.49997933020492));
#123862=DIRECTION('ref_axis',(0.155418826433078,-0.475210466543448,0.86603695121959));
#123863=DIRECTION('center_axis',(0.951131423661017,0.308786358060986,0.));
#123864=DIRECTION('ref_axis',(-0.308786358060986,0.951131423661017,0.));
#123865=DIRECTION('center_axis',(0.309016994374938,-0.951056516295157,-4.35148173242957E-17));
#123866=DIRECTION('ref_axis',(0.951056516295157,0.309016994374938,-2.85097203607405E-33));
#123867=DIRECTION('center_axis',(-0.309016994374914,0.951056516295165,0.));
#123868=DIRECTION('ref_axis',(-0.951056516295164,-0.309016994374914,0.));
#123869=DIRECTION('center_axis',(-1.84331724214206E-16,1.33924836902178E-16,
-1.));
#123870=DIRECTION('ref_axis',(-1.,4.69758072753777E-33,2.25664243350207E-16));
#123871=DIRECTION('center_axis',(0.95098155300316,0.309247612517378,0.));
#123872=DIRECTION('ref_axis',(-0.309247612517378,0.95098155300316,0.));
#123873=DIRECTION('center_axis',(-0.163755730877748,0.503988317040607,-0.848044713969299));
#123874=DIRECTION('ref_axis',(5.60887131859091E-15,0.859649189130451,0.510884792910651));
#123875=DIRECTION('center_axis',(-0.163755570286382,0.503987822791203,0.848045038708655));
#123876=DIRECTION('ref_axis',(9.71142862414541E-16,-0.859649495083705,0.510884278092731));
#123877=DIRECTION('center_axis',(-0.163755764938156,0.503988340266509,-0.848044693589276));
#123878=DIRECTION('ref_axis',(0.257746148170087,-0.8079309973618,-0.529919264233195));
#123879=DIRECTION('center_axis',(-0.163755751065481,0.503988379172012,-0.848044673146732));
#123880=DIRECTION('ref_axis',(-4.45972261711213E-15,0.85964915066946,0.510884857627701));
#123881=DIRECTION('center_axis',(0.163755558314818,-0.503987856144707,-0.848045021198559));
#123882=DIRECTION('ref_axis',(-0.266156471020442,0.805199544416449,-0.52991926423323));
#123883=DIRECTION('center_axis',(-0.163755587629886,0.50398787616902,0.848045003637562));
#123884=DIRECTION('ref_axis',(-2.19355421648303E-15,-0.859649462041468,
0.510884333691899));
#123885=DIRECTION('center_axis',(0.951136266645031,0.308771440182787,-1.68703327872841E-14));
#123886=DIRECTION('ref_axis',(-0.308771440182787,0.951136266645031,1.33674482860247E-28));
#123887=DIRECTION('center_axis',(-0.309016994374914,0.951056516295165,0.));
#123888=DIRECTION('ref_axis',(-0.951056516295164,-0.309016994374914,0.));
#123889=DIRECTION('center_axis',(-1.84331724214206E-16,1.33924836902178E-16,
-1.));
#123890=DIRECTION('ref_axis',(-1.,6.6676823436159E-33,2.40228573745067E-16));
#123891=DIRECTION('center_axis',(0.950976702550726,0.309262527968953,-1.68971643309511E-14));
#123892=DIRECTION('ref_axis',(-0.309262527968953,0.950976702550726,2.53399383097093E-28));
#123893=DIRECTION('center_axis',(-0.309016994374938,0.951056516295157,4.35148173242957E-17));
#123894=DIRECTION('ref_axis',(-0.951056516295156,-0.309016994374938,1.19291088153759E-31));
#123895=DIRECTION('center_axis',(-0.267585776504812,0.823641557783688,-0.500012436349313));
#123896=DIRECTION('ref_axis',(-0.15545353440973,0.475234043117894,0.866017784402458));
#123897=DIRECTION('center_axis',(0.163755751065396,-0.503988379172023,0.848044673146743));
#123898=DIRECTION('ref_axis',(3.85968722528993E-15,-0.859649150669458,-0.510884857627704));
#123899=DIRECTION('center_axis',(0.154510054856149,-0.475533019434887,0.866022511471549));
#123900=DIRECTION('ref_axis',(0.271870311899548,-0.822244813609475,-0.499999999999963));
#123901=DIRECTION('center_axis',(-0.154510049384232,0.475533035318044,-0.86602250372637));
#123902=DIRECTION('ref_axis',(5.01558990523659E-15,0.876548788012491,0.481313018973966));
#123903=DIRECTION('center_axis',(0.163755764945469,-0.503988340060009,0.848044693710586));
#123904=DIRECTION('ref_axis',(0.266368911006386,-0.805129291880355,-0.52991926423325));
#123905=DIRECTION('center_axis',(0.163755730877703,-0.503988317040573,0.848044713969329));
#123906=DIRECTION('ref_axis',(1.7121350261526E-15,-0.859649189130473,-0.510884792910613));
#123907=DIRECTION('center_axis',(-0.309016994374914,0.951056516295164,8.44187456091302E-15));
#123908=DIRECTION('ref_axis',(-0.951056516295164,-0.309016994374914,-8.17628747588762E-32));
#123909=DIRECTION('center_axis',(0.309016994374914,-0.951056516295165,0.));
#123910=DIRECTION('ref_axis',(0.951056516295164,0.309016994374914,0.));
#123911=DIRECTION('center_axis',(-0.309016994374938,0.951056516295157,4.35148173242957E-17));
#123912=DIRECTION('ref_axis',(-0.951056516295156,-0.309016994374938,1.19291088153759E-31));
#123913=DIRECTION('center_axis',(-0.309016994374914,0.951056516295164,-8.44187456091302E-15));
#123914=DIRECTION('ref_axis',(-0.951056516295164,-0.309016994374914,8.17628747588762E-32));
#123915=DIRECTION('center_axis',(-0.309016994374938,0.951056516295157,4.35148173242957E-17));
#123916=DIRECTION('ref_axis',(-0.951056516295156,-0.309016994374938,1.19291088153759E-31));
#123917=DIRECTION('center_axis',(0.267587483540081,-0.823661100222712,-0.499979330205359));
#123918=DIRECTION('ref_axis',(-0.153585232144589,0.475806237443143,-0.866036951219342));
#123919=DIRECTION('center_axis',(-0.154510091261949,0.475533164204404,0.866022425483296));
#123920=DIRECTION('ref_axis',(-1.35777311912048E-15,-0.876548714628841,
0.481313152617427));
#123921=DIRECTION('center_axis',(-0.154510094035502,0.475533172740419,0.866022420301328));
#123922=DIRECTION('ref_axis',(0.951056516294199,0.309016994377886,-1.78335036603156E-12));
#123923=DIRECTION('center_axis',(0.103956887954197,-0.489078705157028,0.866022508719493));
#123924=DIRECTION('ref_axis',(-0.978147600733613,-0.207911690818664,-5.24514815992741E-13));
#123925=DIRECTION('center_axis',(0.180084698745668,-0.847087400906779,0.500012436348017));
#123926=DIRECTION('ref_axis',(0.102990311633872,-0.489291521290677,-0.866017784403192));
#123927=DIRECTION('center_axis',(-0.103956889752271,0.48907871361637,-0.866022503726313));
#123928=DIRECTION('ref_axis',(-1.92726867033915E-15,0.870740345484703,0.491743073916837));
#123929=DIRECTION('center_axis',(-0.207911690817757,0.978147600733806,0.));
#123930=DIRECTION('ref_axis',(-0.978147600733806,-0.207911690817757,0.));
#123931=DIRECTION('center_axis',(0.207911690817749,-0.978147600733808,-2.92774812072069E-17));
#123932=DIRECTION('ref_axis',(0.978147600733808,0.207911690817749,-8.19440684934305E-34));
#123933=DIRECTION('center_axis',(0.207911690817754,-0.978147600733807,0.));
#123934=DIRECTION('ref_axis',(0.978147600733807,0.207911690817754,0.));
#123935=DIRECTION('center_axis',(0.207911690817749,-0.978147600733808,-2.92774812072069E-17));
#123936=DIRECTION('ref_axis',(0.978147600733808,0.207911690817749,-3.83359069178834E-33));
#123937=DIRECTION('center_axis',(-0.207911690817754,0.978147600733807,0.));
#123938=DIRECTION('ref_axis',(-0.978147600733807,-0.207911690817754,0.));
#123939=DIRECTION('center_axis',(0.110177439185349,-0.518344097776638,-0.848045003637591));
#123940=DIRECTION('ref_axis',(1.11828009136564E-15,0.853239582811878,-0.521519140898024));
#123941=DIRECTION('center_axis',(-0.103956917928284,0.489078846173999,0.866022425483291));
#123942=DIRECTION('ref_axis',(-2.88334954178905E-16,-0.870740269393778,
0.491743208652698));
#123943=DIRECTION('center_axis',(-0.110177412160068,0.518344074628259,0.848045021297504));
#123944=DIRECTION('ref_axis',(-0.172101506936992,0.830401496087603,-0.52991926423323));
#123945=DIRECTION('center_axis',(0.110177427516376,-0.518344042878435,-0.848045038708625));
#123946=DIRECTION('ref_axis',(3.87763046936564E-16,0.85323961698728,-0.521519084984815));
#123947=DIRECTION('center_axis',(-0.103956910521019,0.489078861909796,0.866022417485797));
#123948=DIRECTION('ref_axis',(-0.175605160695512,0.848034685338496,-0.499999999999942));
#123949=DIRECTION('center_axis',(-0.180092991631446,0.84710517867207,0.499979330204955));
#123950=DIRECTION('ref_axis',(0.104894406043488,-0.488852904975612,0.86603695121957));
#123951=DIRECTION('center_axis',(0.978197989689811,0.207674488001809,-1.33614410777024E-14));
#123952=DIRECTION('ref_axis',(-0.207674488001809,0.97819798968981,1.40420698398036E-28));
#123953=DIRECTION('center_axis',(0.207911690817749,-0.978147600733808,-2.92774812072069E-17));
#123954=DIRECTION('ref_axis',(0.978147600733808,0.207911690817749,-8.19440684934305E-34));
#123955=DIRECTION('center_axis',(-0.207911690817754,0.978147600733807,0.));
#123956=DIRECTION('ref_axis',(-0.978147600733807,-0.207911690817754,0.));
#123957=DIRECTION('center_axis',(-1.70094388097117E-16,1.37739719617122E-16,
-1.));
#123958=DIRECTION('ref_axis',(-1.,7.04637109130665E-33,2.25664243350207E-16));
#123959=DIRECTION('center_axis',(0.978097154258596,0.208148881407602,0.));
#123960=DIRECTION('ref_axis',(-0.208148881407602,0.978097154258596,0.));
#123961=DIRECTION('center_axis',(-0.110177535564893,0.518344551206598,-0.848044713969303));
#123962=DIRECTION('ref_axis',(-1.36566886276548E-15,0.85323930054103,0.521519602711397));
#123963=DIRECTION('center_axis',(-0.11017742751637,0.518344042878406,0.848045038708643));
#123964=DIRECTION('ref_axis',(2.91791121664691E-16,-0.853239616987298,0.521519084984786));
#123965=DIRECTION('center_axis',(-0.110177567008161,0.518344577866136,-0.848044693589282));
#123966=DIRECTION('ref_axis',(0.171882402214125,-0.830446875605937,-0.529919264233185));
#123967=DIRECTION('center_axis',(-0.110177549147491,0.518344615107839,-0.848044673146738));
#123968=DIRECTION('ref_axis',(3.5353103468128E-15,0.853239260760973,0.5215196677941));
#123969=DIRECTION('center_axis',(0.110177412122302,-0.518344074798144,-0.848045021198573));
#123970=DIRECTION('ref_axis',(-0.180532167034328,0.828609503964605,-0.529919264233167));
#123971=DIRECTION('center_axis',(-0.110177439185351,0.518344097776645,0.848045003637586));
#123972=DIRECTION('ref_axis',(-2.03810354964487E-15,-0.853239582811873,
0.521519140898031));
#123973=DIRECTION('center_axis',(0.978201246800566,0.207659145615641,0.));
#123974=DIRECTION('ref_axis',(-0.207659145615641,0.978201246800566,0.));
#123975=DIRECTION('center_axis',(-0.207911690817754,0.978147600733807,-2.83991567709924E-15));
#123976=DIRECTION('ref_axis',(-0.978147600733807,-0.207911690817754,-8.15748401032363E-30));
#123977=DIRECTION('center_axis',(-1.70094388097117E-16,1.37739719617122E-16,
-1.));
#123978=DIRECTION('ref_axis',(-1.,-7.29277756332989E-33,1.20114286872534E-16));
#123979=DIRECTION('center_axis',(0.978093889466684,0.208164222161096,1.3360019147774E-14));
#123980=DIRECTION('ref_axis',(-0.208164222161096,0.978093889466684,3.50631737784726E-29));
#123981=DIRECTION('center_axis',(-0.207911690817749,0.978147600733808,2.92774812072069E-17));
#123982=DIRECTION('ref_axis',(-0.978147600733808,-0.207911690817749,1.87865085870298E-31));
#123983=DIRECTION('center_axis',(-0.180025927304454,0.84709989316138,-0.500012436349487));
#123984=DIRECTION('ref_axis',(-0.104926459513297,0.48887998035603,0.866017784402314));
#123985=DIRECTION('center_axis',(0.110177549147416,-0.51834461510785,0.848044673146742));
#123986=DIRECTION('ref_axis',(3.90302724780887E-15,-0.853239260760969,-0.521519667794107));
#123987=DIRECTION('center_axis',(0.103956896855725,-0.489078698391826,0.866022511471547));
#123988=DIRECTION('ref_axis',(0.184432991083765,-0.846158656399562,-0.499999999999985));
#123989=DIRECTION('center_axis',(-0.103956889752269,0.489078713616271,-0.866022503726369));
#123990=DIRECTION('ref_axis',(-1.13722082929134E-15,0.87074034548476,0.491743073916737));
#123991=DIRECTION('center_axis',(0.110177567041805,-0.518344577660503,0.848044693710599));
#123992=DIRECTION('ref_axis',(0.18075078662755,-0.828561842307535,-0.529919264233209));
#123993=DIRECTION('center_axis',(0.110177535564769,-0.518344551206596,0.848044713969321));
#123994=DIRECTION('ref_axis',(2.49956668273804E-15,-0.853239300541035,-0.521519602711388));
#123995=DIRECTION('center_axis',(-0.207911690817754,0.978147600733807,0.));
#123996=DIRECTION('ref_axis',(-0.978147600733807,-0.207911690817754,0.));
#123997=DIRECTION('center_axis',(0.207911690817757,-0.978147600733806,0.));
#123998=DIRECTION('ref_axis',(0.978147600733806,0.207911690817757,0.));
#123999=DIRECTION('center_axis',(-0.207911690817749,0.978147600733808,2.92774812072069E-17));
#124000=DIRECTION('ref_axis',(-0.978147600733808,-0.207911690817749,1.87865085870298E-31));
#124001=DIRECTION('center_axis',(-0.207911690817754,0.978147600733807,-5.67983135419817E-15));
#124002=DIRECTION('ref_axis',(-0.978147600733807,-0.207911690817754,-1.62169121129155E-29));
#124003=DIRECTION('center_axis',(-0.207911690817749,0.978147600733808,2.92774812072069E-17));
#124004=DIRECTION('ref_axis',(-0.978147600733808,-0.207911690817749,1.87865085870298E-31));
#124005=DIRECTION('center_axis',(0.180025582247342,-0.847119506978929,-0.499979330205042));
#124006=DIRECTION('ref_axis',(-0.103008581347892,0.489253749388906,-0.866036951219515));
#124007=DIRECTION('center_axis',(-0.103956917928285,0.489078846174002,0.866022425483289));
#124008=DIRECTION('ref_axis',(-6.4647814085365E-16,-0.870740269393776,0.491743208652701));
#124009=DIRECTION('center_axis',(-0.103956919795632,0.489078854959153,0.866022420297794));
#124010=DIRECTION('ref_axis',(0.978147600733986,0.207911690816909,5.24514813542623E-13));
#124011=DIRECTION('center_axis',(0.0522647557775586,-0.49726593457861,0.866022508720861));
#124012=DIRECTION('ref_axis',(-0.994521895368301,-0.10452846326739,1.39870617599167E-13));
#124013=DIRECTION('center_axis',(0.0905534316548002,-0.861270944309356,
0.500012436349347));
#124014=DIRECTION('ref_axis',(0.0512812291256691,-0.49737655014895,-0.866017784402428));
#124015=DIRECTION('center_axis',(-0.052264756681742,0.497265943181925,-0.866022503726311));
#124016=DIRECTION('ref_axis',(-9.31368434701196E-16,0.867207748104374,0.497946504785143));
#124017=DIRECTION('center_axis',(-0.104528463267628,0.994521895368276,0.));
#124018=DIRECTION('ref_axis',(-0.994521895368276,-0.104528463267628,0.));
#124019=DIRECTION('center_axis',(0.104528463267644,-0.994521895368274,-1.47193748793052E-17));
#124020=DIRECTION('ref_axis',(0.994521895368274,0.104528463267644,-6.04857834754731E-34));
#124021=DIRECTION('center_axis',(0.104528463267629,-0.994521895368276,-7.13889681646191E-16));
#124022=DIRECTION('ref_axis',(0.994521895368276,0.104528463267629,5.1828952049124E-31));
#124023=DIRECTION('center_axis',(0.104528463267644,-0.994521895368274,-1.47193748793052E-17));
#124024=DIRECTION('ref_axis',(0.994521895368274,0.104528463267644,-3.02439851631779E-35));
#124025=DIRECTION('center_axis',(-0.10452846326763,0.994521895368276,0.));
#124026=DIRECTION('ref_axis',(-0.994521895368276,-0.10452846326763,0.));
#124027=DIRECTION('center_axis',(0.0553921636609794,-0.527021232978627,
-0.848045003637568));
#124028=DIRECTION('ref_axis',(-1.03878386976432E-15,0.849349030019369,-0.527831625809933));
#124029=DIRECTION('center_axis',(-0.0522647708473857,0.497266077958573,
0.866022425483295));
#124030=DIRECTION('ref_axis',(4.0027550172051E-16,-0.867207670398082,0.497946640115919));
#124031=DIRECTION('center_axis',(-0.0553921391978153,0.52702120713269,0.848045021297509));
#124032=DIRECTION('ref_axis',(-0.084358124572687,0.843841975853974,-0.529919264233185));
#124033=DIRECTION('center_axis',(0.0553921577943494,-0.527021177161371,
-0.848045038708634));
#124034=DIRECTION('ref_axis',(1.11869826565349E-15,0.849349064867504,-0.527831569734793));
#124035=DIRECTION('center_axis',(-0.052264761841082,0.497266092833372,0.866022417485788));
#124036=DIRECTION('ref_axis',(-0.0859994148082359,0.861744800188948,-0.499999999999951));
#124037=DIRECTION('center_axis',(-0.0905598208270846,0.861289491529776,
0.499979330204906));
#124038=DIRECTION('ref_axis',(0.0532207405856546,-0.497139368682233,0.866036951219603));
#124039=DIRECTION('center_axis',(0.994547213842469,0.104287292793425,-1.35847590536994E-14));
#124040=DIRECTION('ref_axis',(-0.104287292793425,0.994547213842469,7.25153974882784E-30));
#124041=DIRECTION('center_axis',(0.104528463267644,-0.994521895368274,-1.47193748793052E-17));
#124042=DIRECTION('ref_axis',(0.994521895368274,0.104528463267644,-6.04857834754731E-34));
#124043=DIRECTION('center_axis',(-0.104528463267628,0.994521895368276,0.));
#124044=DIRECTION('ref_axis',(-0.994521895368276,-0.104528463267628,0.));
#124045=DIRECTION('center_axis',(-1.55536281769216E-16,1.40045497140052E-16,
-1.));
#124046=DIRECTION('ref_axis',(-1.,-6.26344097005036E-33,1.12832121675104E-16));
#124047=DIRECTION('center_axis',(0.994496518411992,0.104769627595152,0.));
#124048=DIRECTION('ref_axis',(-0.104769627595152,0.994496518411992,0.));
#124049=DIRECTION('center_axis',(-0.055392212116204,0.527021693999018,-0.848044713969304));
#124050=DIRECTION('ref_axis',(8.65376607539225E-16,0.849348742192389,0.527832088960312));
#124051=DIRECTION('center_axis',(-0.0553921577943474,0.527021177161352,
0.848045038708646));
#124052=DIRECTION('ref_axis',(1.30911556478354E-16,-0.849349064867516,0.527831569734774));
#124053=DIRECTION('center_axis',(-0.0553922406001646,0.527021723799264,
-0.848044693589286));
#124054=DIRECTION('ref_axis',(0.0841354767040651,-0.843864204095861,-0.529919264233183));
#124055=DIRECTION('center_axis',(-0.0553922189449436,0.527021758969971,
-0.848044673146736));
#124056=DIRECTION('ref_axis',(-1.08455201048859E-15,0.849348701629311,0.527832154231441));
#124057=DIRECTION('center_axis',(0.0553921391498299,-0.527021207296933,
-0.848045021198574));
#124058=DIRECTION('ref_axis',(-0.0929299148210875,0.842941044395081,-0.529919264233218));
#124059=DIRECTION('center_axis',(-0.0553921636609763,0.527021232978597,
0.848045003637587));
#124060=DIRECTION('ref_axis',(-1.18714675169444E-15,-0.849349030019387,
0.527831625809904));
#124061=DIRECTION('center_axis',(0.994548849394384,0.104271693993661,-1.09530233639679E-15));
#124062=DIRECTION('ref_axis',(-0.104271693993661,0.994548849394384,-4.94221831143587E-30));
#124063=DIRECTION('center_axis',(-0.104528463267629,0.994521895368276,0.));
#124064=DIRECTION('ref_axis',(-0.994521895368276,-0.104528463267629,0.));
#124065=DIRECTION('center_axis',(-1.55536281769216E-16,1.40045497140052E-16,
-1.));
#124066=DIRECTION('ref_axis',(-1.,-5.41749190418792E-33,1.20114286872534E-16));
#124067=DIRECTION('center_axis',(0.99449487505034,0.104785225574074,0.));
#124068=DIRECTION('ref_axis',(-0.104785225574074,0.994494875050339,0.));
#124069=DIRECTION('center_axis',(-0.104528463267644,0.994521895368274,1.47193748793052E-17));
#124070=DIRECTION('ref_axis',(-0.994521895368274,-0.104528463267644,-2.00812407505412E-32));
#124071=DIRECTION('center_axis',(-0.090493676371101,0.861277224842662,-0.500012436349501));
#124072=DIRECTION('ref_axis',(-0.0532497883198399,0.49716964624041,0.866017784402305));
#124073=DIRECTION('center_axis',(0.0553922189448982,-0.527021758969983,
0.848044673146731));
#124074=DIRECTION('ref_axis',(3.68113899431711E-16,-0.849348701629304,-0.527832154231452));
#124075=DIRECTION('center_axis',(0.0522647653332842,-0.497265928783765,
0.866022511471541));
#124076=DIRECTION('ref_axis',(0.0949749838225286,-0.860801807879101,-0.499999999999982));
#124077=DIRECTION('center_axis',(-0.0522647566817781,0.49726594318182,-0.86602250372637));
#124078=DIRECTION('ref_axis',(5.50301678318796E-16,0.867207748104434,0.497946504785038));
#124079=DIRECTION('center_axis',(0.0553922406592559,-0.527021723597822,
0.848044693710613));
#124080=DIRECTION('ref_axis',(0.0931523188204474,-0.842916495800706,-0.529919264233177));
#124081=DIRECTION('center_axis',(0.0553922121161434,-0.527021693999,0.848044713969319));
#124082=DIRECTION('ref_axis',(4.25528683943419E-16,-0.849348742192401,-0.527832088960292));
#124083=DIRECTION('center_axis',(-0.104528463267629,0.994521895368276,-7.1388968164623E-16));
#124084=DIRECTION('ref_axis',(-0.994521895368276,-0.104528463267629,5.0770299838595E-31));
#124085=DIRECTION('center_axis',(0.104528463267629,-0.994521895368276,0.));
#124086=DIRECTION('ref_axis',(0.994521895368276,0.104528463267629,0.));
#124087=DIRECTION('center_axis',(-0.104528463267644,0.994521895368274,1.47193748793052E-17));
#124088=DIRECTION('ref_axis',(-0.994521895368274,-0.104528463267644,-2.00812407505412E-32));
#124089=DIRECTION('center_axis',(-0.104528463267629,0.994521895368276,0.));
#124090=DIRECTION('ref_axis',(-0.994521895368276,-0.104528463267629,0.));
#124091=DIRECTION('center_axis',(-0.104528463267644,0.994521895368274,1.47193748793052E-17));
#124092=DIRECTION('ref_axis',(-0.994521895368274,-0.104528463267644,-2.00812407505412E-32));
#124093=DIRECTION('center_axis',(0.0904912830029371,-0.861296695145102,
-0.499979330205368));
#124094=DIRECTION('ref_axis',(-0.0513033469792888,0.497340894871386,-0.866036951219318));
#124095=DIRECTION('center_axis',(-0.0522647708473827,0.497266077958545,
0.866022425483311));
#124096=DIRECTION('ref_axis',(-3.47519388666402E-16,-0.867207670398098,
0.49794664011589));
#124097=DIRECTION('center_axis',(-0.0522647717850455,0.497266086879728,
0.86602242030422));
#124098=DIRECTION('ref_axis',(0.99452189536868,0.104528463263786,2.23792987110329E-12));
#124099=DIRECTION('center_axis',(-5.08727263162943E-15,-0.500005014362422,
0.866022508721589));
#124100=DIRECTION('ref_axis',(-1.,-7.55301335024474E-12,-4.33598914551087E-12));
#124101=DIRECTION('center_axis',(3.00422138958798E-5,-0.866018223016285,
0.500012436346518));
#124102=DIRECTION('ref_axis',(-0.00098970131624398,-0.500012217437995,-0.866017784404017));
#124103=DIRECTION('center_axis',(-2.73187543788774E-14,0.500005023014372,
-0.866022503726316));
#124104=DIRECTION('ref_axis',(-3.29182907633956E-28,0.866022503726316,0.500005023014372));
#124105=DIRECTION('center_axis',(0.,1.,0.));
#124106=DIRECTION('ref_axis',(0.,0.,1.));
#124107=DIRECTION('center_axis',(-1.04744440165294E-14,-1.,1.4749788077992E-30));
#124108=DIRECTION('ref_axis',(1.,-1.04744440165294E-14,-2.48920611114446E-60));
#124109=DIRECTION('center_axis',(0.,-1.,0.));
#124110=DIRECTION('ref_axis',(0.,0.,-1.));
#124111=DIRECTION('center_axis',(-1.04744440165294E-14,-1.,1.4749788077992E-30));
#124112=DIRECTION('ref_axis',(1.,-1.04744440165294E-14,-2.48920611114446E-60));
#124113=DIRECTION('center_axis',(0.,1.,0.));
#124114=DIRECTION('ref_axis',(0.,0.,1.));
#124115=DIRECTION('center_axis',(0.,-0.52992421326579,-0.848045003637563));
#124116=DIRECTION('ref_axis',(0.,0.848045003637563,-0.52992421326579));
#124117=DIRECTION('center_axis',(0.,0.500005158533422,0.866022425483294));
#124118=DIRECTION('ref_axis',(0.,-0.866022425483294,0.500005158533421));
#124119=DIRECTION('center_axis',(2.16240926169255E-8,0.529924185004365,
0.84804502129749));
#124120=DIRECTION('ref_axis',(0.00430950301662301,0.848037146343398,-0.529919264233237));
#124121=DIRECTION('center_axis',(0.,-0.529924157141051,-0.848045038708645));
#124122=DIRECTION('ref_axis',(0.,0.848045038708645,-0.529924157141051));
#124123=DIRECTION('center_axis',(1.05144329133207E-8,0.500005172385368,
0.866022417485759));
#124124=DIRECTION('ref_axis',(0.00454855868433578,0.866013458679421,-0.500000000000001));
#124125=DIRECTION('center_axis',(-3.44576744524761E-5,0.866037336481559,
0.499979330205355));
#124126=DIRECTION('ref_axis',(0.000963977578947313,-0.499979069431867,0.866036951219329));
#124127=DIRECTION('center_axis',(-1.04744440165294E-14,-1.,1.4749788077992E-30));
#124128=DIRECTION('ref_axis',(1.,-1.04744440165294E-14,-2.48920611114446E-60));
#124129=DIRECTION('center_axis',(0.,1.,0.));
#124130=DIRECTION('ref_axis',(0.,0.,1.));
#124131=DIRECTION('center_axis',(-2.89534733035821E-14,0.529924676825566,
-0.848044713969328));
#124132=DIRECTION('ref_axis',(-3.84874727475395E-28,0.848044713969328,0.529924676825566));
#124133=DIRECTION('center_axis',(0.,0.529924157141041,0.848045038708651));
#124134=DIRECTION('ref_axis',(0.,-0.848045038708651,0.529924157141041));
#124135=DIRECTION('center_axis',(-2.52137135654268E-8,0.529924709439987,
-0.848044693589285));
#124136=DIRECTION('ref_axis',(-0.00453325468848542,-0.848035979777079,-0.529919264233202));
#124137=DIRECTION('center_axis',(-4.63345827774717E-14,0.529924742154432,
-0.848044673146739));
#124138=DIRECTION('ref_axis',(-1.03401629657842E-27,0.848044673146739,0.529924742154432));
#124139=DIRECTION('center_axis',(-2.16959060264487E-8,-0.529924185162668,
-0.848045021198569));
#124140=DIRECTION('ref_axis',(-0.00430950303050303,0.848037146343343,-0.529919264233213));
#124141=DIRECTION('center_axis',(0.,0.52992421326579,0.848045003637563));
#124142=DIRECTION('ref_axis',(0.,-0.848045003637563,0.52992421326579));
#124143=DIRECTION('center_axis',(0.,1.,0.));
#124144=DIRECTION('ref_axis',(0.,0.,1.));
#124145=DIRECTION('center_axis',(1.04744440165294E-14,1.,-1.4749788077992E-30));
#124146=DIRECTION('ref_axis',(-1.,1.04744440165294E-14,-2.83769496670468E-58));
#124147=DIRECTION('center_axis',(3.00422154286595E-5,0.866018223015636,
-0.500012436347643));
#124148=DIRECTION('ref_axis',(-0.000989701290563527,0.500012217439134,0.86601778440339));
#124149=DIRECTION('center_axis',(0.,-0.529924742154432,0.848044673146739));
#124150=DIRECTION('ref_axis',(0.,-0.848044673146739,-0.529924742154432));
#124151=DIRECTION('center_axis',(1.01107237965894E-8,-0.500005009599421,
0.866022511471545));
#124152=DIRECTION('ref_axis',(0.00447641076555513,-0.866013834616201,-0.500000000000002));
#124153=DIRECTION('center_axis',(0.,0.500005023014355,-0.866022503726326));
#124154=DIRECTION('ref_axis',(0.,0.866022503726326,0.500005023014355));
#124155=DIRECTION('center_axis',(2.52897127115498E-8,-0.529924709245837,
0.848044693710606));
#124156=DIRECTION('ref_axis',(0.00453325469237332,-0.848035979777063,-0.529919264233195));
#124157=DIRECTION('center_axis',(-2.89534733035821E-14,-0.529924676825566,
0.848044713969328));
#124158=DIRECTION('ref_axis',(-3.89468630110175E-28,-0.848044713969328,
-0.529924676825566));
#124159=DIRECTION('center_axis',(0.,1.,0.));
#124160=DIRECTION('ref_axis',(0.,0.,1.));
#124161=DIRECTION('center_axis',(0.,-1.,0.));
#124162=DIRECTION('ref_axis',(0.,0.,-1.));
#124163=DIRECTION('center_axis',(1.04744440165294E-14,1.,-1.4749788077992E-30));
#124164=DIRECTION('ref_axis',(-1.,1.04744440165294E-14,-2.83769496670468E-58));
#124165=DIRECTION('center_axis',(0.,1.,0.));
#124166=DIRECTION('ref_axis',(0.,0.,1.));
#124167=DIRECTION('center_axis',(1.04744440165294E-14,1.,-1.4749788077992E-30));
#124168=DIRECTION('ref_axis',(-1.,1.04744440165294E-14,-2.83769496670468E-58));
#124169=DIRECTION('center_axis',(-3.44576745143992E-5,-0.866037336481586,
-0.499979330205309));
#124170=DIRECTION('ref_axis',(0.000963977574060321,0.499979069431824,-0.86603695121936));
#124171=DIRECTION('center_axis',(0.,0.500005158533422,0.866022425483294));
#124172=DIRECTION('ref_axis',(0.,-0.866022425483294,0.500005158533422));
#124173=DIRECTION('center_axis',(5.43769792106264E-15,0.500005167509914,
0.866022420300643));
#124174=DIRECTION('ref_axis',(1.,-1.67844740333718E-12,9.44126664377163E-13));
#124175=DIRECTION('center_axis',(-0.0522647557773824,-0.497265934576869,
0.866022508721871));
#124176=DIRECTION('ref_axis',(-0.994521895368246,0.104528463267908,1.39870617597895E-13));
#124177=DIRECTION('center_axis',(-0.0904936763721428,-0.861277224842625,
0.500012436349377));
#124178=DIRECTION('ref_axis',(-0.0532497883297758,-0.497169646239235,-0.866017784402369));
#124179=DIRECTION('center_axis',(0.0522647566817887,0.497265943181924,-0.866022503726309));
#124180=DIRECTION('ref_axis',(9.3445928215498E-16,0.867207748104374,0.497946504785143));
#124181=DIRECTION('center_axis',(0.104528463267683,0.99452189536827,0.));
#124182=DIRECTION('ref_axis',(-0.99452189536827,0.104528463267683,0.));
#124183=DIRECTION('center_axis',(-0.104528463267664,-0.994521895368272,
1.4719374879308E-17));
#124184=DIRECTION('ref_axis',(0.994521895368272,-0.104528463267664,7.55090158384622E-35));
#124185=DIRECTION('center_axis',(-0.104528463267683,-0.99452189536827,0.));
#124186=DIRECTION('ref_axis',(0.99452189536827,-0.104528463267683,0.));
#124187=DIRECTION('center_axis',(-0.104528463267664,-0.994521895368272,
1.4719374879308E-17));
#124188=DIRECTION('ref_axis',(0.994521895368272,-0.104528463267664,-4.99104833753089E-34));
#124189=DIRECTION('center_axis',(0.104528463267682,0.994521895368271,0.));
#124190=DIRECTION('ref_axis',(-0.994521895368271,0.104528463267682,0.));
#124191=DIRECTION('center_axis',(-0.055392163661009,-0.527021232978633,
-0.848045003637563));
#124192=DIRECTION('ref_axis',(5.85670520831155E-16,0.849349030019364,-0.52783162580994));
#124193=DIRECTION('center_axis',(0.052264770847414,0.497266077958582,0.866022425483288));
#124194=DIRECTION('ref_axis',(1.6088847247092E-16,-0.867207670398076,0.497946640115928));
#124195=DIRECTION('center_axis',(0.0553921822216235,0.527021202610695,0.848045021297516));
#124196=DIRECTION('ref_axis',(0.0929299148295972,0.842941044394173,-0.52991926423317));
#124197=DIRECTION('center_axis',(-0.0553921577943759,-0.527021177161348,
-0.848045038708647));
#124198=DIRECTION('ref_axis',(3.66225041260374E-16,0.849349064867518,-0.527831569734771));
#124199=DIRECTION('center_axis',(0.0522647827539146,0.497266090635403,0.866022417485754));
#124200=DIRECTION('ref_axis',(0.0950466972136718,0.860793892490397,-0.500000000000004));
#124201=DIRECTION('center_axis',(0.0904912830033326,0.861296695144991,0.499979330205487));
#124202=DIRECTION('ref_axis',(-0.0513033469766535,-0.497340894871782,0.866036951219247));
#124203=DIRECTION('center_axis',(0.994496518411991,-0.104769627595163,6.79203329632462E-15));
#124204=DIRECTION('ref_axis',(0.104769627595163,0.994496518411991,2.96919234963523E-30));
#124205=DIRECTION('center_axis',(-0.104528463267664,-0.994521895368272,
1.4719374879308E-17));
#124206=DIRECTION('ref_axis',(0.994521895368272,-0.104528463267664,7.55090158384622E-35));
#124207=DIRECTION('center_axis',(0.104528463267628,0.994521895368276,0.));
#124208=DIRECTION('ref_axis',(-0.994521895368276,0.104528463267628,0.));
#124209=DIRECTION('center_axis',(-1.26097532010602E-16,1.40045497140051E-16,
-1.));
#124210=DIRECTION('ref_axis',(0.,1.,1.12832121675104E-16));
#124211=DIRECTION('center_axis',(0.994547213842467,-0.104287292793444,0.));
#124212=DIRECTION('ref_axis',(0.104287292793444,0.994547213842467,0.));
#124213=DIRECTION('center_axis',(0.0553922121162013,0.527021693998993,-0.84804471396932));
#124214=DIRECTION('ref_axis',(7.93731044687634E-16,0.849348742192405,0.527832088960286));
#124215=DIRECTION('center_axis',(0.0553921577943754,0.527021177161343,0.84804503870865));
#124216=DIRECTION('ref_axis',(-6.93579166402575E-16,-0.849349064867522,
0.527831569734766));
#124217=DIRECTION('center_axis',(0.0553921904558474,0.52702172906962,-0.848044693589301));
#124218=DIRECTION('ref_axis',(-0.0931523188100742,-0.842916495801844,-0.529919264233191));
#124219=DIRECTION('center_axis',(0.0553922189449272,0.527021758969979,-0.848044673146731));
#124220=DIRECTION('ref_axis',(5.64549624567747E-16,0.849348701629306,0.527832154231449));
#124221=DIRECTION('center_axis',(-0.0553921822949527,-0.527021202762207,
-0.848045021198568));
#124222=DIRECTION('ref_axis',(0.0843581245765446,0.843841975853581,-0.529919264233197));
#124223=DIRECTION('center_axis',(0.0553921636610064,0.527021232978609,0.848045003637578));
#124224=DIRECTION('ref_axis',(-5.90605431002811E-16,-0.84934903001938,0.527831625809916));
#124225=DIRECTION('center_axis',(0.994494875050337,-0.104785225574097,-1.06687590778408E-15));
#124226=DIRECTION('ref_axis',(0.104785225574097,0.994494875050337,3.46902153471063E-31));
#124227=DIRECTION('center_axis',(0.104528463267683,0.99452189536827,7.1388968164656E-16));
#124228=DIRECTION('ref_axis',(-0.99452189536827,0.104528463267683,2.13048964590254E-33));
#124229=DIRECTION('center_axis',(-1.26097532010602E-16,1.40045497140051E-16,
-1.));
#124230=DIRECTION('ref_axis',(0.,1.,1.20114286872534E-16));
#124231=DIRECTION('center_axis',(0.994548849394382,-0.104271693993677,1.0953023363959E-15));
#124232=DIRECTION('ref_axis',(0.104271693993677,0.994548849394382,-2.25165513859667E-30));
#124233=DIRECTION('center_axis',(0.104528463267664,0.994521895368272,-1.4719374879308E-17));
#124234=DIRECTION('ref_axis',(-0.994521895368272,0.104528463267664,-1.2142399857261E-32));
#124235=DIRECTION('center_axis',(0.0905534316547619,0.861270944309424,-0.500012436349237));
#124236=DIRECTION('ref_axis',(0.0512812291215075,0.497376550149274,0.866017784402488));
#124237=DIRECTION('center_axis',(-0.0553922189449268,-0.527021758969972,
0.848044673146736));
#124238=DIRECTION('ref_axis',(-1.04823533788178E-15,-0.84934870162931,-0.527832154231442));
#124239=DIRECTION('center_axis',(-0.0522647452196774,-0.49726593089775,
0.866022511471565));
#124240=DIRECTION('ref_axis',(-0.0860712067697641,-0.861737632557173,-0.499999999999955));
#124241=DIRECTION('center_axis',(0.0522647566818046,0.497265943181812,-0.866022503726373));
#124242=DIRECTION('ref_axis',(-1.28065569756335E-16,0.867207748104438,0.497946504785031));
#124243=DIRECTION('center_axis',(-0.055392190356225,-0.527021728884907,
0.848044693710599));
#124244=DIRECTION('ref_axis',(-0.0841354767102596,-0.843864204095235,-0.529919264233197));
#124245=DIRECTION('center_axis',(-0.0553922121162459,-0.527021693998973,
0.848044713969329));
#124246=DIRECTION('ref_axis',(-3.6090586595327E-16,-0.849348742192416,-0.527832088960269));
#124247=DIRECTION('center_axis',(0.104528463267683,0.99452189536827,-5.36237632086923E-14));
#124248=DIRECTION('ref_axis',(-0.99452189536827,0.104528463267683,5.67004406102361E-31));
#124249=DIRECTION('center_axis',(-0.104528463267684,-0.99452189536827,0.));
#124250=DIRECTION('ref_axis',(0.99452189536827,-0.104528463267684,0.));
#124251=DIRECTION('center_axis',(0.104528463267664,0.994521895368272,-1.4719374879308E-17));
#124252=DIRECTION('ref_axis',(-0.994521895368272,0.104528463267664,-1.2142399857261E-32));
#124253=DIRECTION('center_axis',(0.104528463267683,0.99452189536827,9.28056586140528E-15));
#124254=DIRECTION('ref_axis',(-0.99452189536827,0.104528463267683,2.74937968383573E-32));
#124255=DIRECTION('center_axis',(0.104528463267664,0.994521895368272,-1.4719374879308E-17));
#124256=DIRECTION('ref_axis',(-0.994521895368272,0.104528463267664,-1.2142399857261E-32));
#124257=DIRECTION('center_axis',(-0.0905598208270262,-0.861289491529606,
-0.49997933020521));
#124258=DIRECTION('ref_axis',(0.0532207406056314,0.497139368680429,-0.866036951219411));
#124259=DIRECTION('center_axis',(0.0522647708474102,0.497266077958546,0.866022425483309));
#124260=DIRECTION('ref_axis',(4.84777660203887E-16,-0.867207670398097,0.497946640115892));
#124261=DIRECTION('center_axis',(0.0522647717852642,0.497266086881686,0.866022420303083));
#124262=DIRECTION('ref_axis',(0.994521895367867,-0.104528463271519,2.23792987111612E-12));
#124263=DIRECTION('center_axis',(-0.103956887952481,-0.489078705148897,
0.86602250872429));
#124264=DIRECTION('ref_axis',(-0.978147600733677,0.207911690818365,3.49676543997127E-13));
#124265=DIRECTION('center_axis',(-0.180025927304388,-0.847099893162094,
0.500012436348302));
#124266=DIRECTION('ref_axis',(-0.104926459550624,-0.488879980346867,-0.866017784402964));
#124267=DIRECTION('center_axis',(0.103956889752339,0.489078713616364,-0.866022503726308));
#124268=DIRECTION('ref_axis',(2.29104531904658E-15,0.870740345484705,0.491743073916834));
#124269=DIRECTION('center_axis',(0.207911690817757,0.978147600733806,5.62829268885415E-14));
#124270=DIRECTION('ref_axis',(-0.978147600733806,0.207911690817757,-6.75602897704988E-32));
#124271=DIRECTION('center_axis',(-0.20791169081777,-0.978147600733803,2.92774812072098E-17));
#124272=DIRECTION('ref_axis',(0.978147600733803,-0.20791169081777,9.03770998686543E-34));
#124273=DIRECTION('center_axis',(-0.207911690817757,-0.978147600733806,
-2.83991567709912E-15));
#124274=DIRECTION('ref_axis',(0.978147600733806,-0.207911690817757,-1.96908327204163E-32));
#124275=DIRECTION('center_axis',(-0.20791169081777,-0.978147600733803,2.92774812072098E-17));
#124276=DIRECTION('ref_axis',(0.978147600733803,-0.20791169081777,-1.35684150645397E-33));
#124277=DIRECTION('center_axis',(0.207911690817754,0.978147600733807,0.));
#124278=DIRECTION('ref_axis',(-0.978147600733807,0.207911690817754,0.));
#124279=DIRECTION('center_axis',(-0.110177439185351,-0.518344097776641,
-0.848045003637589));
#124280=DIRECTION('ref_axis',(-1.51970787343667E-15,0.853239582811876,-0.521519140898027));
#124281=DIRECTION('center_axis',(0.103956917928287,0.489078846173999,0.866022425483291));
#124282=DIRECTION('ref_axis',(2.96906041204586E-16,-0.870740269393778,0.491743208652698));
#124283=DIRECTION('center_axis',(0.110177454466897,0.518344065635659,0.848045021297508));
#124284=DIRECTION('ref_axis',(0.180532167028516,0.828609503965844,-0.52991926423321));
#124285=DIRECTION('center_axis',(-0.110177427516368,-0.51834404287839,-0.848045038708654));
#124286=DIRECTION('ref_axis',(-2.67094448372999E-15,0.853239616987309,-0.521519084984769));
#124287=DIRECTION('center_axis',(0.103956931095903,0.489078857536534,0.86602241748576));
#124288=DIRECTION('ref_axis',(0.18450348422679,0.846143288284058,-0.500000000000016));
#124289=DIRECTION('center_axis',(0.18002558224756,0.847119506978716,0.499979330205324));
#124290=DIRECTION('ref_axis',(-0.103008581357447,-0.489253749387169,0.86603695121936));
#124291=DIRECTION('center_axis',(0.978097154258593,-0.208148881407615,0.));
#124292=DIRECTION('ref_axis',(0.208148881407615,0.978097154258593,0.));
#124293=DIRECTION('center_axis',(-0.20791169081777,-0.978147600733803,2.92774812072098E-17));
#124294=DIRECTION('ref_axis',(0.978147600733803,-0.20791169081777,9.03770998686543E-34));
#124295=DIRECTION('center_axis',(0.207911690817809,0.978147600733795,0.));
#124296=DIRECTION('ref_axis',(-0.978147600733795,0.207911690817809,0.));
#124297=DIRECTION('center_axis',(-1.11539425682701E-16,1.37739719617121E-16,
-1.));
#124298=DIRECTION('ref_axis',(0.,1.,1.12832121675104E-16));
#124299=DIRECTION('center_axis',(0.978197989689803,-0.207674488001846,0.));
#124300=DIRECTION('ref_axis',(0.207674488001846,0.978197989689803,0.));
#124301=DIRECTION('center_axis',(0.110177535564859,0.518344551206574,-0.848044713969323));
#124302=DIRECTION('ref_axis',(-4.00339603515207E-16,0.853239300541046,0.521519602711371));
#124303=DIRECTION('center_axis',(0.110177427516366,0.518344042878381,0.848045038708659));
#124304=DIRECTION('ref_axis',(1.58984749529623E-15,-0.853239616987314,0.521519084984761));
#124305=DIRECTION('center_axis',(0.110177517684597,0.518344588350194,-0.848044693589276));
#124306=DIRECTION('ref_axis',(-0.18075078663936,-0.828561842304951,-0.529919264233221));
#124307=DIRECTION('center_axis',(0.110177549147491,0.518344615107832,-0.848044673146743));
#124308=DIRECTION('ref_axis',(-2.64002787776822E-15,0.853239260760977,0.521519667794094));
#124309=DIRECTION('center_axis',(-0.110177454555387,-0.518344065778716,
-0.848045021198572));
#124310=DIRECTION('ref_axis',(0.172101506935008,0.830401496088012,-0.529919264233233));
#124311=DIRECTION('center_axis',(0.110177439185354,0.518344097776652,0.848045003637582));
#124312=DIRECTION('ref_axis',(2.89201529937556E-15,-0.853239582811869,0.521519140898038));
#124313=DIRECTION('center_axis',(0.978093889466681,-0.20816422216111,-1.53465780422786E-14));
#124314=DIRECTION('ref_axis',(0.20816422216111,0.978093889466681,2.32253611591275E-29));
#124315=DIRECTION('center_axis',(0.207911690817757,0.978147600733806,5.34430112114423E-14));
#124316=DIRECTION('ref_axis',(-0.978147600733806,0.207911690817757,1.19680266142653E-30));
#124317=DIRECTION('center_axis',(-1.11539425682701E-16,1.37739719617121E-16,
-1.));
#124318=DIRECTION('ref_axis',(0.,1.,1.20114286872534E-16));
#124319=DIRECTION('center_axis',(0.978201246800563,-0.207659145615657,2.0156211610367E-15));
#124320=DIRECTION('ref_axis',(0.207659145615657,0.978201246800563,-8.63903528825318E-30));
#124321=DIRECTION('center_axis',(0.20791169081777,0.978147600733803,-2.92774812072098E-17));
#124322=DIRECTION('ref_axis',(-0.978147600733803,0.20791169081777,-1.37139085278161E-32));
#124323=DIRECTION('center_axis',(0.180084698748564,0.847087400905278,-0.500012436349517));
#124324=DIRECTION('ref_axis',(0.102990311599707,0.489291521299458,0.866017784402293));
#124325=DIRECTION('center_axis',(-0.110177549147563,-0.518344615107823,
0.848044673146739));
#124326=DIRECTION('ref_axis',(1.94829734210075E-15,-0.85323926076098,-0.521519667794088));
#124327=DIRECTION('center_axis',(-0.103956877077249,-0.489078702595896,
0.866022511471533));
#124328=DIRECTION('ref_axis',(-0.175675810178078,-0.84802005266283,-0.500000000000007));
#124329=DIRECTION('center_axis',(0.103956889752269,0.489078713616261,-0.866022503726375));
#124330=DIRECTION('ref_axis',(2.38114632574082E-15,0.870740345484765,0.491743073916727));
#124331=DIRECTION('center_axis',(-0.110177517568077,-0.51834458817644,0.848044693710616));
#124332=DIRECTION('ref_axis',(-0.171882402228799,-0.830446875602875,-0.529919264233223));
#124333=DIRECTION('center_axis',(-0.110177535564811,-0.518344551206572,
0.84804471396933));
#124334=DIRECTION('ref_axis',(-1.96158023811665E-16,-0.853239300541049,
-0.521519602711367));
#124335=DIRECTION('center_axis',(0.207911690817757,0.978147600733806,5.34430112114423E-14));
#124336=DIRECTION('ref_axis',(-0.978147600733806,0.207911690817757,1.19680266142653E-30));
#124337=DIRECTION('center_axis',(-0.207911690817757,-0.978147600733806,
0.));
#124338=DIRECTION('ref_axis',(0.978147600733806,-0.207911690817757,0.));
#124339=DIRECTION('center_axis',(0.20791169081777,0.978147600733803,-2.92774812072098E-17));
#124340=DIRECTION('ref_axis',(-0.978147600733803,0.20791169081777,-1.37139085278161E-32));
#124341=DIRECTION('center_axis',(0.207911690817757,0.978147600733806,-7.33224209511362E-14));
#124342=DIRECTION('ref_axis',(-0.978147600733806,0.207911690817757,-2.34871055257466E-31));
#124343=DIRECTION('center_axis',(0.20791169081777,0.978147600733803,-2.92774812072098E-17));
#124344=DIRECTION('ref_axis',(-0.978147600733803,0.20791169081777,-1.37139085278161E-32));
#124345=DIRECTION('center_axis',(-0.180092991631147,-0.847105178672085,
-0.499979330205039));
#124346=DIRECTION('ref_axis',(0.104894406044029,0.488852904975583,-0.866036951219522));
#124347=DIRECTION('center_axis',(0.103956917928286,0.489078846173998,0.866022425483291));
#124348=DIRECTION('ref_axis',(2.529180872252E-16,-0.870740269393778,0.491743208652698));
#124349=DIRECTION('center_axis',(0.10395691979444,0.489078854953561,0.866022420301095));
#124350=DIRECTION('ref_axis',(0.978147600733799,-0.207911690817788,3.49676542358288E-14));
#124351=DIRECTION('center_axis',(-0.154510046710454,-0.475533027088933,
0.866022508722013));
#124352=DIRECTION('ref_axis',(-0.9510565162939,0.309016994378807,2.34283284479982E-12));
#124353=DIRECTION('center_axis',(-0.267585776504412,-0.823641557783639,
0.500012436349609));
#124354=DIRECTION('ref_axis',(-0.155453534429849,-0.475234043111657,-0.866017784402269));
#124355=DIRECTION('center_axis',(0.154510049384266,0.475533035318147,-0.866022503726308));
#124356=DIRECTION('ref_axis',(-4.94155540489305E-15,0.876548788012433,0.481313018974072));
#124357=DIRECTION('center_axis',(0.309016994374964,0.951056516295148,0.));
#124358=DIRECTION('ref_axis',(-0.951056516295148,0.309016994374964,0.));
#124359=DIRECTION('center_axis',(-0.309016994374957,-0.95105651629515,4.35148173242984E-17));
#124360=DIRECTION('ref_axis',(0.95105651629515,-0.309016994374957,3.82078699478083E-35));
#124361=DIRECTION('center_axis',(-0.309016994374964,-0.951056516295148,
0.));
#124362=DIRECTION('ref_axis',(0.951056516295148,-0.309016994374964,0.));
#124363=DIRECTION('center_axis',(-0.309016994374957,-0.95105651629515,4.35148173242984E-17));
#124364=DIRECTION('ref_axis',(0.95105651629515,-0.309016994374957,3.82078699478083E-35));
#124365=DIRECTION('center_axis',(0.309016994374914,0.951056516295165,0.));
#124366=DIRECTION('ref_axis',(-0.951056516295164,0.309016994374914,0.));
#124367=DIRECTION('center_axis',(-0.163755587629897,-0.503987876168966,
-0.848045003637591));
#124368=DIRECTION('ref_axis',(2.74983269065662E-16,0.8596494620415,-0.510884333691845));
#124369=DIRECTION('center_axis',(0.154510091262001,0.47553316420445,0.866022425483262));
#124370=DIRECTION('ref_axis',(-1.17478566960452E-15,-0.876548714628813,
0.481313152617478));
#124371=DIRECTION('center_axis',(0.163755599457083,0.503987842610314,0.848045021297486));
#124372=DIRECTION('ref_axis',(0.26615647102241,0.805199544415818,-0.5299192642332));
#124373=DIRECTION('center_axis',(-0.163755570286403,-0.503987822791179,
-0.848045038708665));
#124374=DIRECTION('ref_axis',(6.13898415849569E-16,0.859649495083718,-0.510884278092709));
#124375=DIRECTION('center_axis',(0.154510105546379,0.475533174127907,0.866022417485762));
#124376=DIRECTION('ref_axis',(0.271938812471266,0.822222161141207,-0.5));
#124377=DIRECTION('center_axis',(0.267587483540056,0.823661100222809,0.499979330205211));
#124378=DIRECTION('ref_axis',(-0.153585232141186,-0.475806237444091,0.866036951219424));
#124379=DIRECTION('center_axis',(0.950981553003154,-0.309247612517397,0.));
#124380=DIRECTION('ref_axis',(0.309247612517397,0.950981553003154,0.));
#124381=DIRECTION('center_axis',(-0.309016994374957,-0.95105651629515,4.35148173242984E-17));
#124382=DIRECTION('ref_axis',(0.95105651629515,-0.309016994374957,3.82078699478083E-35));
#124383=DIRECTION('center_axis',(0.309016994374964,0.951056516295148,0.));
#124384=DIRECTION('ref_axis',(-0.951056516295148,0.309016994374964,0.));
#124385=DIRECTION('center_axis',(-9.73020895656121E-17,1.33924836902177E-16,
-1.));
#124386=DIRECTION('ref_axis',(0.,1.,1.12832121675104E-16));
#124387=DIRECTION('center_axis',(0.951131423661011,-0.308786358061005,0.));
#124388=DIRECTION('ref_axis',(0.308786358061005,0.95113142366101,0.));
#124389=DIRECTION('center_axis',(0.16375573087775,0.503988317040599,-0.848044713969304));
#124390=DIRECTION('ref_axis',(-3.99459261142949E-15,0.859649189130456,0.510884792910642));
#124391=DIRECTION('center_axis',(0.163755570286399,0.503987822791167,0.848045038708674));
#124392=DIRECTION('ref_axis',(4.51011726205046E-15,-0.859649495083727,0.510884278092695));
#124393=DIRECTION('center_axis',(0.163755716974444,0.503988355850892,-0.848044693589259));
#124394=DIRECTION('ref_axis',(-0.266368911007828,-0.80512929187988,-0.529919264233247));
#124395=DIRECTION('center_axis',(0.163755751065492,0.503988379171991,-0.848044673146743));
#124396=DIRECTION('ref_axis',(-3.74794587153715E-15,0.859649150669473,0.510884857627679));
#124397=DIRECTION('center_axis',(-0.163755599580069,-0.50398784273681,-0.848045021198562));
#124398=DIRECTION('ref_axis',(0.257959309136819,0.807862963765655,-0.529919264233172));
#124399=DIRECTION('center_axis',(0.1637555876299,0.503987876168973,0.848045003637587));
#124400=DIRECTION('ref_axis',(1.15652631111913E-15,-0.859649462041495,0.510884333691853));
#124401=DIRECTION('center_axis',(0.95097670255072,-0.309262527968972,0.));
#124402=DIRECTION('ref_axis',(0.309262527968972,0.95097670255072,0.));
#124403=DIRECTION('center_axis',(0.309016994374964,0.951056516295148,8.44187456091391E-15));
#124404=DIRECTION('ref_axis',(-0.951056516295148,0.309016994374964,-7.18667850250016E-29));
#124405=DIRECTION('center_axis',(-9.73020895656121E-17,1.33924836902177E-16,
-1.));
#124406=DIRECTION('ref_axis',(0.,1.,1.20114286872534E-16));
#124407=DIRECTION('center_axis',(0.951136266645023,-0.308771440182812,9.1132642300708E-15));
#124408=DIRECTION('ref_axis',(0.308771440182812,0.951136266645023,7.06407243348961E-29));
#124409=DIRECTION('center_axis',(0.309016994374957,0.95105651629515,-4.35148173242984E-17));
#124410=DIRECTION('ref_axis',(-0.95105651629515,0.309016994374957,4.68049650745012E-31));
#124411=DIRECTION('center_axis',(0.267642920194536,0.823622990674872,-0.500012436346858));
#124412=DIRECTION('ref_axis',(0.153571010754701,0.475845712129453,0.866017784403873));
#124413=DIRECTION('center_axis',(-0.163755751065471,-0.503988379172015,
0.848044673146733));
#124414=DIRECTION('ref_axis',(-4.07962663151818E-15,-0.859649150669459,
-0.510884857627703));
#124415=DIRECTION('center_axis',(-0.154510035624795,-0.475533025683541,
0.866022511471545));
#124416=DIRECTION('ref_axis',(-0.263355672637406,-0.825011387612138,-0.499999999999994));
#124417=DIRECTION('center_axis',(0.154510049384271,0.475533035318079,-0.866022503726344));
#124418=DIRECTION('ref_axis',(-3.78698134078517E-16,0.87654878801247,0.481313018974005));
#124419=DIRECTION('center_axis',(-0.163755716848899,-0.503988355687507,
0.8480446937106));
#124420=DIRECTION('ref_axis',(-0.257746148182604,-0.807930997357781,-0.529919264233234));
#124421=DIRECTION('center_axis',(-0.163755730877757,-0.503988317040559,
0.848044713969326));
#124422=DIRECTION('ref_axis',(-3.38818205240043E-15,-0.859649189130478,
-0.510884792910604));
#124423=DIRECTION('center_axis',(0.309016994374964,0.951056516295148,0.));
#124424=DIRECTION('ref_axis',(-0.951056516295148,0.309016994374964,0.));
#124425=DIRECTION('center_axis',(-0.309016994374964,-0.951056516295148,
0.));
#124426=DIRECTION('ref_axis',(0.951056516295148,-0.309016994374964,0.));
#124427=DIRECTION('center_axis',(0.309016994374957,0.95105651629515,-4.35148173242984E-17));
#124428=DIRECTION('ref_axis',(-0.95105651629515,0.309016994374957,4.68049650745012E-31));
#124429=DIRECTION('center_axis',(0.309016994374964,0.951056516295148,1.68837491218278E-14));
#124430=DIRECTION('ref_axis',(-0.951056516295148,0.309016994374964,-1.43733570050003E-28));
#124431=DIRECTION('center_axis',(0.309016994374957,0.95105651629515,-4.35148173242984E-17));
#124432=DIRECTION('ref_axis',(-0.95105651629515,0.309016994374957,4.68049650745012E-31));
#124433=DIRECTION('center_axis',(-0.26765302593251,-0.823639804208764,-0.499979330204879));
#124434=DIRECTION('ref_axis',(0.155418826437838,0.475210466541855,-0.86603695121961));
#124435=DIRECTION('center_axis',(0.154510091261982,0.47553316420442,0.866022425483281));
#124436=DIRECTION('ref_axis',(4.67804569173509E-15,-0.876548714628831,0.481313152617445));
#124437=DIRECTION('center_axis',(0.154510094034566,0.475533172737486,0.866022420303106));
#124438=DIRECTION('ref_axis',(0.951056516295455,-0.309016994374019,-5.94450122008058E-13));
#124439=DIRECTION('center_axis',(-0.203370361063959,-0.456777309671768,
0.866022508720031));
#124440=DIRECTION('ref_axis',(-0.913545457642825,0.406736643075296,-3.49676543997941E-13));
#124441=DIRECTION('center_axis',(-0.352213899943218,-0.791159233140749,
0.500012436348268));
#124442=DIRECTION('ref_axis',(-0.20427742790161,-0.456381342242989,-0.866017784403063));
#124443=DIRECTION('center_axis',(0.203370364581912,0.456777317573273,-0.86602250372631));
#124444=DIRECTION('ref_axis',(5.88898682911472E-15,0.884507036382098,0.466526850878444));
#124445=DIRECTION('center_axis',(0.406736643075807,0.913545457642598,0.));
#124446=DIRECTION('ref_axis',(-0.913545457642598,0.406736643075807,0.));
#124447=DIRECTION('center_axis',(-0.40673664307581,-0.913545457642596,5.72753959967211E-17));
#124448=DIRECTION('ref_axis',(0.913545457642596,-0.40673664307581,-6.16988091840288E-33));
#124449=DIRECTION('center_axis',(-0.406736643075807,-0.913545457642598,
0.));
#124450=DIRECTION('ref_axis',(0.913545457642598,-0.406736643075807,0.));
#124451=DIRECTION('center_axis',(-0.40673664307581,-0.913545457642596,5.72753959967211E-17));
#124452=DIRECTION('ref_axis',(0.913545457642596,-0.40673664307581,-6.16988091840288E-33));
#124453=DIRECTION('center_axis',(0.406736643075817,0.913545457642594,0.));
#124454=DIRECTION('ref_axis',(-0.913545457642593,0.406736643075817,0.));
#124455=DIRECTION('center_axis',(-0.215539595588313,-0.484109857923785,
-0.848045003637566));
#124456=DIRECTION('ref_axis',(-3.45358436037744E-15,0.868458021515986,-0.495762710240029));
#124457=DIRECTION('center_axis',(0.20337041970248,0.456777441376083,0.866022425483287));
#124458=DIRECTION('ref_axis',(-1.65090401241273E-16,-0.884506966812053,
0.46652698277907));
#124459=DIRECTION('center_axis',(0.215539603856733,0.48410982330642,0.848045021297519));
#124460=DIRECTION('ref_axis',(0.34886470904002,0.772967650151669,-0.529919264233175));
#124461=DIRECTION('center_axis',(-0.21553957276031,-0.484109806651251,-0.848045038708671));
#124462=DIRECTION('ref_axis',(-1.58448265001912E-15,0.86845805294998,-0.495762655175165));
#124463=DIRECTION('center_axis',(0.20337043494579,0.456777449752126,0.866022417485774));
#124464=DIRECTION('ref_axis',(0.356394722167848,0.789292595943303,-0.499999999999984));
#124465=DIRECTION('center_axis',(0.352217640366796,0.79117849009036,0.499979330205544));
#124466=DIRECTION('ref_axis',(-0.202479170978949,-0.457145692796707,0.866036951219228));
#124467=DIRECTION('center_axis',(0.913446798847318,-0.406958162070241,-2.49539780475005E-14));
#124468=DIRECTION('ref_axis',(0.406958162070241,0.913446798847317,-4.8143736717754E-28));
#124469=DIRECTION('center_axis',(-0.40673664307581,-0.913545457642596,5.72753959967211E-17));
#124470=DIRECTION('ref_axis',(0.913545457642596,-0.40673664307581,-6.16988091840288E-33));
#124471=DIRECTION('center_axis',(0.406736643075817,0.913545457642594,0.));
#124472=DIRECTION('ref_axis',(-0.913545457642593,0.406736643075817,0.));
#124473=DIRECTION('center_axis',(-8.35415108931894E-17,1.28642645648558E-16,
-1.));
#124474=DIRECTION('ref_axis',(0.,1.,1.12832121675104E-16));
#124475=DIRECTION('center_axis',(0.913644062717548,-0.406515100163541,0.));
#124476=DIRECTION('ref_axis',(0.406515100163541,0.913644062717548,0.));
#124477=DIRECTION('center_axis',(0.215539784135082,0.484110281406712,-0.848044713969326));
#124478=DIRECTION('ref_axis',(3.15501118393508E-15,0.868457761888289,0.495763165045553));
#124479=DIRECTION('center_axis',(0.215539572760321,0.484109806651275,0.848045038708655));
#124480=DIRECTION('ref_axis',(-2.32320804316489E-15,-0.868458052949965,
0.495762655175191));
#124481=DIRECTION('center_axis',(0.215539774369014,0.48411032145577,-0.848044693589286));
#124482=DIRECTION('ref_axis',(-0.349068641855651,-0.772875576446536,-0.529919264233229));
#124483=DIRECTION('center_axis',(0.215539810706709,0.484110341087599,-0.848044673146742));
#124484=DIRECTION('ref_axis',(-3.47902836708183E-15,0.868457725299276,0.495763229140693));
#124485=DIRECTION('center_axis',(-0.215539603978092,-0.484109823425721,
-0.848045021198571));
#124486=DIRECTION('ref_axis',(0.340990855174584,0.77647331575649,-0.529919264233173));
#124487=DIRECTION('center_axis',(0.215539595588318,0.484109857923797,0.848045003637558));
#124488=DIRECTION('ref_axis',(6.38857881715217E-15,-0.86845802151598,0.49576271024004));
#124489=DIRECTION('center_axis',(0.913440415876953,-0.406972488803039,-2.71806413419043E-15));
#124490=DIRECTION('ref_axis',(0.406972488803039,0.913440415876953,-4.73617210527067E-29));
#124491=DIRECTION('center_axis',(0.406736643075807,0.913545457642598,1.11114268233636E-14));
#124492=DIRECTION('ref_axis',(-0.913545457642598,0.406736643075807,1.88066567154315E-32));
#124493=DIRECTION('center_axis',(-8.35415108931894E-17,1.28642645648558E-16,
-1.));
#124494=DIRECTION('ref_axis',(0.,1.,1.20114286872534E-16));
#124495=DIRECTION('center_axis',(0.913650438514062,-0.40650077023674,0.));
#124496=DIRECTION('ref_axis',(0.40650077023674,0.913650438514061,0.));
#124497=DIRECTION('center_axis',(0.40673664307581,0.913545457642596,-5.72753959967211E-17));
#124498=DIRECTION('ref_axis',(-0.913545457642596,0.40673664307581,8.86064060326668E-32));
#124499=DIRECTION('center_axis',(0.352268789801539,0.791134794600438,-0.500012436349619));
#124500=DIRECTION('ref_axis',(0.202469153665814,0.457186437805111,0.866017784402215));
#124501=DIRECTION('center_axis',(-0.215539810706676,-0.484110341087619,
0.848044673146739));
#124502=DIRECTION('ref_axis',(-2.55985226452489E-15,-0.868457725299266,
-0.49576322914071));
#124503=DIRECTION('center_axis',(-0.203370349888124,-0.456777309430842,
0.866022511471557));
#124504=DIRECTION('ref_axis',(-0.348150155229772,-0.792963725156138,-0.499999999999987));
#124505=DIRECTION('center_axis',(0.203370364581896,0.456777317573237,-0.866022503726332));
#124506=DIRECTION('ref_axis',(-3.435979432868E-16,0.884507036382118,0.466526850878406));
#124507=DIRECTION('center_axis',(-0.215539774216652,-0.48411032131109,0.848044693710602));
#124508=DIRECTION('ref_axis',(-0.340785973383132,-0.776563258041383,-0.529919264233207));
#124509=DIRECTION('center_axis',(-0.215539784135111,-0.484110281406697,
0.848044713969328));
#124510=DIRECTION('ref_axis',(-4.1843617536873E-16,-0.868457761888296,-0.49576316504554));
#124511=DIRECTION('center_axis',(0.406736643075807,0.913545457642598,0.));
#124512=DIRECTION('ref_axis',(-0.913545457642598,0.406736643075807,0.));
#124513=DIRECTION('center_axis',(-0.406736643075817,-0.913545457642594,
0.));
#124514=DIRECTION('ref_axis',(0.913545457642593,-0.406736643075817,0.));
#124515=DIRECTION('center_axis',(0.40673664307581,0.913545457642596,-5.72753959967211E-17));
#124516=DIRECTION('ref_axis',(-0.913545457642596,0.40673664307581,8.86064060326668E-32));
#124517=DIRECTION('center_axis',(0.406736643075807,0.913545457642598,-1.11114268233636E-14));
#124518=DIRECTION('ref_axis',(-0.913545457642598,0.406736643075807,-1.88066567154315E-32));
#124519=DIRECTION('center_axis',(0.40673664307581,0.913545457642596,-5.72753959967211E-17));
#124520=DIRECTION('ref_axis',(-0.913545457642596,0.40673664307581,8.86064060326668E-32));
#124521=DIRECTION('center_axis',(-0.352280597670949,-0.791150459692801,
-0.499979330205227));
#124522=DIRECTION('ref_axis',(0.204240445640436,0.456361522794359,-0.86603695121941));
#124523=DIRECTION('center_axis',(0.203370419702468,0.456777441376069,0.866022425483298));
#124524=DIRECTION('ref_axis',(6.03968553444511E-15,-0.884506966812061,0.466526982779053));
#124525=DIRECTION('center_axis',(0.203370423353836,0.456777449577125,0.866022420300248));
#124526=DIRECTION('ref_axis',(0.91354545764332,-0.406736643074185,-1.04902962708698E-12));
#124527=DIRECTION('center_axis',(-0.250002507181426,-0.433017044457782,
0.866022508721366));
#124528=DIRECTION('ref_axis',(-0.866025403785938,0.499999999997404,-1.74838271999619E-12));
#124529=DIRECTION('center_axis',(-0.43298309418575,-0.750008802379122,0.500012436348507));
#124530=DIRECTION('ref_axis',(-0.250863215204664,-0.432528431845965,-0.866017784402866));
#124531=DIRECTION('center_axis',(0.250002511507219,0.433017051950267,-0.866022503726308));
#124532=DIRECTION('ref_axis',(2.04174131109056E-15,0.894424794863788,0.447218387740118));
#124533=DIRECTION('center_axis',(0.499999999999998,0.86602540378444,0.));
#124534=DIRECTION('ref_axis',(-0.86602540378444,0.499999999999998,0.));
#124535=DIRECTION('center_axis',(-0.50000000000001,-0.866025403784433,7.04084534449567E-17));
#124536=DIRECTION('ref_axis',(0.866025403784433,-0.50000000000001,-1.10642434862234E-32));
#124537=DIRECTION('center_axis',(-0.50000000000001,-0.866025403784433,0.));
#124538=DIRECTION('ref_axis',(0.866025403784433,-0.50000000000001,0.));
#124539=DIRECTION('center_axis',(-0.50000000000001,-0.866025403784433,7.04084534449567E-17));
#124540=DIRECTION('ref_axis',(0.866025403784433,-0.50000000000001,-1.10642434862234E-32));
#124541=DIRECTION('center_axis',(0.499999999999998,0.86602540378444,0.));
#124542=DIRECTION('ref_axis',(-0.86602540378444,0.499999999999998,0.));
#124543=DIRECTION('center_axis',(-0.264962106632877,-0.458927830768628,
-0.848045003637584));
#124544=DIRECTION('ref_axis',(-3.91597869182367E-15,0.879478602053331,-0.475938429348081));
#124545=DIRECTION('center_axis',(0.250002579266714,0.433017169313217,0.866022425483289));
#124546=DIRECTION('ref_axis',(4.16344728135109E-15,-0.894424730216417,0.447218517033106));
#124547=DIRECTION('center_axis',(0.264962111231692,0.458927795480013,0.848045021297513));
#124548=DIRECTION('ref_axis',(0.427750712286238,0.732266960563717,-0.52991926423314));
#124549=DIRECTION('center_axis',(-0.264962078570518,-0.458927782163196,
-0.848045038708653));
#124550=DIRECTION('ref_axis',(3.68379810748961E-15,0.879478631391255,-0.475938375135022));
#124551=DIRECTION('center_axis',(0.250002595294356,0.433017176054468,0.866022417485772));
#124552=DIRECTION('ref_axis',(0.436945896706248,0.747715375896206,-0.499999999999968));
#124553=DIRECTION('center_axis',(0.432988827019129,0.750027562856271,0.499979330205241));
#124554=DIRECTION('ref_axis',(-0.249154705657373,-0.433476564270065,0.866036951219408));
#124555=DIRECTION('center_axis',(0.865904130412325,-0.500209992837883,0.));
#124556=DIRECTION('ref_axis',(0.500209992837883,0.865904130412325,0.));
#124557=DIRECTION('center_axis',(-0.50000000000001,-0.866025403784433,7.04084534449567E-17));
#124558=DIRECTION('ref_axis',(0.866025403784433,-0.50000000000001,-1.10642434862234E-32));
#124559=DIRECTION('center_axis',(0.50000000000001,0.866025403784433,0.));
#124560=DIRECTION('ref_axis',(-0.866025403784433,0.50000000000001,0.));
#124561=DIRECTION('center_axis',(-7.04084534449538E-17,1.2195101864901E-16,
-1.));
#124562=DIRECTION('ref_axis',(0.,1.,1.12832121675104E-16));
#124563=DIRECTION('center_axis',(0.866146626230604,-0.499789977760002,0.));
#124564=DIRECTION('ref_axis',(0.499789977760002,0.866146626230603,0.));
#124565=DIRECTION('center_axis',(0.264962338412816,0.458928232223194,-0.84804471396932));
#124566=DIRECTION('ref_axis',(3.75627101917228E-15,0.879478359737748,0.475938877118692));
#124567=DIRECTION('center_axis',(0.264962078570517,0.45892778216318,0.848045038708662));
#124568=DIRECTION('ref_axis',(3.56607010359993E-15,-0.879478631391266,0.475938375135003));
#124569=DIRECTION('center_axis',(0.264962332885149,0.458928273074468,-0.848044693589286));
#124570=DIRECTION('ref_axis',(-0.427943903622742,-0.732154074458846,-0.529919264233185));
#124571=DIRECTION('center_axis',(0.264962371077225,0.458928288799661,-0.848044673146733));
#124572=DIRECTION('ref_axis',(2.91201203045915E-15,0.879478325588505,0.475938940222419));
#124573=DIRECTION('center_axis',(-0.264962111366864,-0.458927795584814,
-0.848045021198567));
#124574=DIRECTION('ref_axis',(0.42028643407695,0.736576463597214,-0.529919264233245));
#124575=DIRECTION('center_axis',(0.264962106632849,0.458927830768566,0.848045003637626));
#124576=DIRECTION('ref_axis',(3.02991594379835E-15,-0.879478602053368,0.475938429348013));
#124577=DIRECTION('center_axis',(0.86589628485713,-0.500223573885338,2.36549702850838E-14));
#124578=DIRECTION('ref_axis',(0.500223573885338,0.86589628485713,2.17961681937253E-28));
#124579=DIRECTION('center_axis',(0.50000000000001,0.866025403784433,0.));
#124580=DIRECTION('ref_axis',(-0.866025403784433,0.50000000000001,0.));
#124581=DIRECTION('center_axis',(-7.04084534449538E-17,1.2195101864901E-16,
-1.));
#124582=DIRECTION('ref_axis',(0.,1.,1.20114286872534E-16));
#124583=DIRECTION('center_axis',(0.866154464985094,-0.499776392786199,0.));
#124584=DIRECTION('ref_axis',(0.499776392786199,0.866154464985094,0.));
#124585=DIRECTION('center_axis',(0.50000000000001,0.866025403784433,-7.04084534449567E-17));
#124586=DIRECTION('ref_axis',(-0.866025403784433,0.50000000000001,-2.26108826570355E-32));
#124587=DIRECTION('center_axis',(0.433035128829351,0.749978760163112,-0.500012436349286));
#124588=DIRECTION('ref_axis',(0.249149002230563,0.433518133168907,0.866017784402411));
#124589=DIRECTION('center_axis',(-0.264962371077261,-0.458928288799629,
0.848044673146739));
#124590=DIRECTION('ref_axis',(1.3237123733169E-15,-0.879478325588521,-0.475938940222391));
#124591=DIRECTION('center_axis',(-0.250002496042324,-0.433017045388671,
0.86602251147154));
#124592=DIRECTION('ref_axis',(-0.429130231858343,-0.752228186194332,-0.49999999999999));
#124593=DIRECTION('center_axis',(0.250002511507148,0.433017051950192,-0.866022503726366));
#124594=DIRECTION('ref_axis',(-4.43899159512102E-15,0.894424794863831,0.447218387740031));
#124595=DIRECTION('center_axis',(-0.26496233272356,-0.458928272943599,0.848044693710594));
#124596=DIRECTION('ref_axis',(-0.420092076171116,-0.73668732915174,-0.529919264233257));
#124597=DIRECTION('center_axis',(-0.264962338412833,-0.458928232223181,
0.848044713969322));
#124598=DIRECTION('ref_axis',(5.09612267090991E-15,-0.879478359737755,-0.475938877118678));
#124599=DIRECTION('center_axis',(0.50000000000001,0.866025403784433,1.36592399683221E-14));
#124600=DIRECTION('ref_axis',(-0.866025403784433,0.50000000000001,1.17750412048402E-31));
#124601=DIRECTION('center_axis',(-0.500000000000034,-0.866025403784419,
0.));
#124602=DIRECTION('ref_axis',(0.866025403784419,-0.500000000000034,0.));
#124603=DIRECTION('center_axis',(0.50000000000001,0.866025403784433,-7.04084534449567E-17));
#124604=DIRECTION('ref_axis',(-0.866025403784433,0.50000000000001,-2.26108826570355E-32));
#124605=DIRECTION('center_axis',(0.50000000000001,0.866025403784433,3.36577552674936E-14));
#124606=DIRECTION('ref_axis',(-0.866025403784433,0.50000000000001,4.78353594691771E-31));
#124607=DIRECTION('center_axis',(0.50000000000001,0.866025403784433,-7.04084534449567E-17));
#124608=DIRECTION('ref_axis',(-0.866025403784433,0.50000000000001,-2.26108826570355E-32));
#124609=DIRECTION('center_axis',(-0.433048509462144,-0.74999310518159,-0.499979330205452));
#124610=DIRECTION('ref_axis',(0.250824363787036,0.432512586699685,-0.866036951219275));
#124611=DIRECTION('center_axis',(0.250002579266705,0.433017169313187,0.866022425483307));
#124612=DIRECTION('ref_axis',(-4.67813616211968E-15,-0.894424730216432,
0.447218517033075));
#124613=DIRECTION('center_axis',(0.250002583754379,0.433017177086056,0.866022420301321));
#124614=DIRECTION('ref_axis',(0.866025403784735,-0.499999999999487,-3.84644196594952E-13));
#124615=DIRECTION('center_axis',(-0.293895573516442,-0.404512553894514,
0.86602250871971));
#124616=DIRECTION('ref_axis',(-0.809016994376793,0.587785252289932,-1.81831802877876E-12));
#124617=DIRECTION('center_axis',(-0.509008435041602,-0.700641118228716,
0.500012436349051));
#124618=DIRECTION('ref_axis',(-0.294700492590666,-0.403936649445632,-0.866017784402523));
#124619=DIRECTION('center_axis',(0.293895578599988,0.40451256089148,-0.866022503726315));
#124620=DIRECTION('ref_axis',(4.72353162256085E-15,0.906035256115477,0.423202214875775));
#124621=DIRECTION('center_axis',(0.587785252292496,0.809016994374931,0.));
#124622=DIRECTION('ref_axis',(-0.809016994374931,0.587785252292496,0.));
#124623=DIRECTION('center_axis',(-0.587785252292482,-0.809016994374941,
8.2770101143333E-17));
#124624=DIRECTION('ref_axis',(0.809016994374941,-0.587785252292482,1.04582204444099E-33));
#124625=DIRECTION('center_axis',(-0.587785252292496,-0.809016994374931,
-3.21147992436152E-14));
#124626=DIRECTION('ref_axis',(0.809016994374931,-0.587785252292496,2.30136499084345E-30));
#124627=DIRECTION('center_axis',(-0.587785252292482,-0.809016994374941,
8.2770101143333E-17));
#124628=DIRECTION('ref_axis',(0.809016994374941,-0.587785252292482,1.04582204444099E-33));
#124629=DIRECTION('center_axis',(0.58778525229247,0.80901699437495,0.));
#124630=DIRECTION('ref_axis',(-0.80901699437495,0.58778525229247,0.));
#124631=DIRECTION('center_axis',(-0.31148163739031,-0.428717694262756,-0.848045003637588));
#124632=DIRECTION('ref_axis',(-6.37487263847381E-15,0.892442058026274,-0.451162025292277));
#124633=DIRECTION('center_axis',(0.293895658256118,0.404512670528671,0.866022425483293));
#124634=DIRECTION('ref_axis',(1.8194066783722E-15,-0.906035197473499,0.423202340422589));
#124635=DIRECTION('center_axis',(0.311481638274036,0.428717658687681,0.848045021297499));
#124636=DIRECTION('ref_axis',(0.50195018920892,0.683543400924673,-0.529919264233204));
#124637=DIRECTION('center_axis',(-0.311481604401037,-0.428717648856917,
-0.848045038708649));
#124638=DIRECTION('ref_axis',(7.95334372440912E-15,0.892442084777736,-0.451161972375297));
#124639=DIRECTION('center_axis',(0.293895674898826,0.404512675558928,0.866022417485784));
#124640=DIRECTION('ref_axis',(0.51270980056614,0.697946029721123,-0.49999999999995));
#124641=DIRECTION('center_axis',(0.509016097474113,0.700659176689997,0.499979330205079));
#124642=DIRECTION('ref_axis',(-0.293100449236466,-0.405058175796775,0.866036951219503));
#124643=DIRECTION('center_axis',(0.808874435122379,-0.587981418248444,0.));
#124644=DIRECTION('ref_axis',(0.587981418248444,0.808874435122379,0.));
#124645=DIRECTION('center_axis',(-0.587785252292482,-0.809016994374941,
8.2770101143333E-17));
#124646=DIRECTION('ref_axis',(0.809016994374941,-0.587785252292482,1.04582204444099E-33));
#124647=DIRECTION('center_axis',(0.58778525229247,0.80901699437495,0.));
#124648=DIRECTION('ref_axis',(-0.80901699437495,0.58778525229247,0.));
#124649=DIRECTION('center_axis',(-5.80468057465775E-17,1.13923270769251E-16,
-1.));
#124650=DIRECTION('ref_axis',(0.,1.,1.12832121675104E-16));
#124651=DIRECTION('center_axis',(0.809159506053906,-0.587589051772239,0.));
#124652=DIRECTION('ref_axis',(0.587589051772239,0.809159506053906,0.));
#124653=DIRECTION('center_axis',(0.3114819098639,0.428718069290558,-0.848044713969325));
#124654=DIRECTION('ref_axis',(1.92114153099776E-15,0.892441837073387,0.451162462358159));
#124655=DIRECTION('center_axis',(0.311481604401026,0.428717648856902,0.84804503870866));
#124656=DIRECTION('ref_axis',(6.88023766601185E-16,-0.892442084777746,0.451161972375277));
#124657=DIRECTION('center_axis',(0.311481908636186,0.428718110496172,-0.848044693589289));
#124658=DIRECTION('ref_axis',(-0.502130522426461,-0.683410939217635,-0.529919264233147));
#124659=DIRECTION('center_axis',(0.311481948263223,0.428718122142731,-0.848044673146738));
#124660=DIRECTION('ref_axis',(1.34798612095186E-15,0.892441805934764,0.451162523953283));
#124661=DIRECTION('center_axis',(-0.311481638423146,-0.428717658775068,
-0.848045021198555));
#124662=DIRECTION('ref_axis',(0.494977266815938,0.688609525587588,-0.529919264233205));
#124663=DIRECTION('center_axis',(0.311481637390356,0.428717694262819,0.84804500363754));
#124664=DIRECTION('ref_axis',(-5.56364179183466E-15,-0.892442058026235,
0.451162025292353));
#124665=DIRECTION('center_axis',(0.808865212939996,-0.58799410481359,-3.21262103104279E-14));
#124666=DIRECTION('ref_axis',(0.58799410481359,0.808865212939996,4.78933061976136E-28));
#124667=DIRECTION('center_axis',(0.587785252292496,0.809016994374931,-3.21147992436152E-14));
#124668=DIRECTION('ref_axis',(-0.809016994374931,0.587785252292496,2.30136499084345E-30));
#124669=DIRECTION('center_axis',(-5.80468057465775E-17,1.13923270769251E-16,
-1.));
#124670=DIRECTION('ref_axis',(0.,1.,1.20114286872534E-16));
#124671=DIRECTION('center_axis',(0.80916872188328,-0.587576360591353,-3.21033860361202E-14));
#124672=DIRECTION('ref_axis',(0.587576360591353,0.80916872188328,4.80261672572901E-28));
#124673=DIRECTION('center_axis',(0.587785252292482,0.809016994374941,-8.2770101143333E-17));
#124674=DIRECTION('ref_axis',(-0.809016994374941,0.587785252292482,4.73588184773858E-32));
#124675=DIRECTION('center_axis',(0.509057044368194,0.700605801485152,-0.500012436349803));
#124676=DIRECTION('ref_axis',(0.293099122184562,0.405100113149701,0.86601778440211));
#124677=DIRECTION('center_axis',(-0.311481948263288,-0.428718122142702,
0.848044673146728));
#124678=DIRECTION('ref_axis',(6.50740225724504E-15,-0.892441805934775,-0.451162523953261));
#124679=DIRECTION('center_axis',(-0.293895562534375,-0.40451255598208,0.866022511471525));
#124680=DIRECTION('ref_axis',(-0.505408667883912,-0.70325107780065,-0.500000000000034));
#124681=DIRECTION('center_axis',(0.293895578599968,0.404512560891387,-0.866022503726365));
#124682=DIRECTION('ref_axis',(1.55256022332075E-15,0.906035256115524,0.423202214875674));
#124683=DIRECTION('center_axis',(-0.311481908459053,-0.42871811038485,0.848044693710626));
#124684=DIRECTION('ref_axis',(-0.494795562234247,-0.688740099738556,-0.529919264233166));
#124685=DIRECTION('center_axis',(-0.311481909863969,-0.428718069290495,
0.848044713969331));
#124686=DIRECTION('ref_axis',(1.5898874044363E-15,-0.892441837073416,-0.451162462358103));
#124687=DIRECTION('center_axis',(0.587785252292496,0.809016994374931,0.));
#124688=DIRECTION('ref_axis',(-0.809016994374931,0.587785252292496,0.));
#124689=DIRECTION('center_axis',(-0.587785252292496,-0.809016994374931,
0.));
#124690=DIRECTION('ref_axis',(0.809016994374931,-0.587785252292496,0.));
#124691=DIRECTION('center_axis',(0.587785252292482,0.809016994374941,-8.2770101143333E-17));
#124692=DIRECTION('ref_axis',(-0.809016994374941,0.587785252292482,4.73588184773858E-32));
#124693=DIRECTION('center_axis',(0.587785252292496,0.809016994374931,-4.42022290584682E-14));
#124694=DIRECTION('ref_axis',(-0.809016994374931,0.587785252292496,1.69177565650547E-30));
#124695=DIRECTION('center_axis',(0.587785252292482,0.809016994374941,-8.2770101143333E-17));
#124696=DIRECTION('ref_axis',(-0.809016994374941,0.587785252292482,4.73588184773858E-32));
#124697=DIRECTION('center_axis',(-0.50907185116306,-0.700618669263837,-0.499979330205146));
#124698=DIRECTION('ref_axis',(0.294660197696144,0.403924952207911,-0.866036951219465));
#124699=DIRECTION('center_axis',(0.293895658256114,0.404512670528666,0.866022425483297));
#124700=DIRECTION('ref_axis',(-6.85542257558146E-17,-0.906035197473502,
0.423202340422583));
#124701=DIRECTION('center_axis',(0.293895663530901,0.404512677788762,0.866022420302094));
#124702=DIRECTION('ref_axis',(0.809016994373366,-0.58778525229465,1.53857678639347E-12));
#124703=DIRECTION('center_axis',(-0.334568658443799,-0.371576139137306,
0.866022508720721));
#124704=DIRECTION('ref_axis',(-0.743144825476915,0.66913060635939,4.19611852791889E-13));
#124705=DIRECTION('center_axis',(-0.579456972966298,-0.643597063368579,
0.500012436349413));
#124706=DIRECTION('ref_axis',(-0.335308969655448,-0.370919252624417,-0.866017784402345));
#124707=DIRECTION('center_axis',(0.334568664232119,0.37157614556582,-0.866022503726309));
#124708=DIRECTION('ref_axis',(2.56241420419672E-15,0.918982183096524,0.394299058014532));
#124709=DIRECTION('center_axis',(0.669130606358875,0.743144825477379,0.));
#124710=DIRECTION('ref_axis',(-0.743144825477379,0.669130606358875,0.));
#124711=DIRECTION('center_axis',(-0.669130606358867,-0.743144825477386,
9.42249022928259E-17));
#124712=DIRECTION('ref_axis',(0.743144825477386,-0.669130606358867,1.14423954767457E-32));
#124713=DIRECTION('center_axis',(-0.669130606358845,-0.743144825477406,
4.06031740096479E-14));
#124714=DIRECTION('ref_axis',(0.743144825477406,-0.669130606358845,-1.17388982313054E-30));
#124715=DIRECTION('center_axis',(-0.669130606358867,-0.743144825477386,
9.42249022928259E-17));
#124716=DIRECTION('ref_axis',(0.743144825477386,-0.669130606358867,-3.88054752867469E-33));
#124717=DIRECTION('center_axis',(0.669130606358845,0.743144825477406,0.));
#124718=DIRECTION('ref_axis',(-0.743144825477406,0.669130606358845,0.));
#124719=DIRECTION('center_axis',(-0.354588510146749,-0.393810436983632,
-0.848045003637584));
#124720=DIRECTION('ref_axis',(-5.89688827602511E-16,0.906978223357768,-0.421177518814558));
#124721=DIRECTION('center_axis',(0.334568754912034,0.371576246276112,0.866022425483293));
#124722=DIRECTION('ref_axis',(2.56170689995423E-15,-0.918982131463647,0.394299178353863));
#124723=DIRECTION('center_axis',(0.354588507310876,0.39381040150757,0.848045021297508));
#124724=DIRECTION('ref_axis',(0.570650194839117,0.627330796729033,-0.529919264233142));
#124725=DIRECTION('center_axis',(-0.354588472592004,-0.393810395274862,
-0.848045038708633));
#124726=DIRECTION('ref_axis',(1.64363307278047E-15,0.906978247051285,-0.421177467792116));
#124727=DIRECTION('center_axis',(0.334568771994895,0.37157624953427,0.866022417485757));
#124728=DIRECTION('ref_axis',(0.582856348565578,0.640529840785569,-0.500000000000016));
#124729=DIRECTION('center_axis',(0.579466481046627,0.643614221961416,0.4999793302052));
#124730=DIRECTION('ref_axis',(-0.333834922962011,-0.372201885182612,0.866036951219437));
#124731=DIRECTION('center_axis',(0.742982542253377,-0.669310796197633,-7.71634144622546E-14));
#124732=DIRECTION('ref_axis',(0.669310796197633,0.742982542253377,-3.15085687395575E-28));
#124733=DIRECTION('center_axis',(-0.669130606358867,-0.743144825477386,
9.42249022928259E-17));
#124734=DIRECTION('ref_axis',(0.743144825477386,-0.669130606358867,1.14423954767457E-32));
#124735=DIRECTION('center_axis',(0.669130606358845,0.743144825477406,0.));
#124736=DIRECTION('ref_axis',(-0.743144825477406,0.669130606358845,0.));
#124737=DIRECTION('center_axis',(-4.65920045970846E-17,1.04647355694968E-16,
-1.));
#124738=DIRECTION('ref_axis',(0.,1.,1.12832121675104E-16));
#124739=DIRECTION('center_axis',(0.743307065001304,-0.668950377172438,0.));
#124740=DIRECTION('ref_axis',(0.668950377172438,0.743307065001304,0.));
#124741=DIRECTION('center_axis',(0.354588820328836,0.39381078147567,-0.848044713969332));
#124742=DIRECTION('ref_axis',(7.54048452976697E-15,0.906978027661857,0.421177940232638));
#124743=DIRECTION('center_axis',(0.354588472592016,0.393810395274875,0.848045038708621));
#124744=DIRECTION('ref_axis',(4.30002933985616E-15,-0.906978247051278,0.42117746779213));
#124745=DIRECTION('center_axis',(0.354588823409533,0.393810822588869,-0.848044693589271));
#124746=DIRECTION('ref_axis',(-0.570815694142538,-0.62718021071711,-0.52991926423316));
#124747=DIRECTION('center_axis',(0.354588864042302,0.393810830024563,-0.848044673146736));
#124748=DIRECTION('ref_axis',(-8.30756835896895E-15,0.906978000082633,0.421177999622615));
#124749=DIRECTION('center_axis',(-0.354588507465445,-0.393810401581466,
-0.848045021198564));
#124750=DIRECTION('ref_axis',(0.564245025076819,0.633098037487535,-0.529919264233234));
#124751=DIRECTION('center_axis',(0.354588510146734,0.393810436983615,0.848045003637598));
#124752=DIRECTION('ref_axis',(9.67156497587423E-15,-0.906978223357779,0.421177518814534));
#124753=DIRECTION('center_axis',(0.742972044483923,-0.669322449283885,4.02398997762811E-15));
#124754=DIRECTION('ref_axis',(0.669322449283885,0.742972044483923,8.70636259521657E-29));
#124755=DIRECTION('center_axis',(0.669130606358845,0.743144825477406,4.06031740096502E-14));
#124756=DIRECTION('ref_axis',(-0.743144825477406,0.669130606358845,-2.91235641449386E-31));
#124757=DIRECTION('center_axis',(-4.65920045970846E-17,1.04647355694968E-16,
-1.));
#124758=DIRECTION('ref_axis',(0.,1.,1.20114286872534E-16));
#124759=DIRECTION('center_axis',(0.743317556935059,-0.668938718831625,0.));
#124760=DIRECTION('ref_axis',(0.668938718831625,0.743317556935059,0.));
#124761=DIRECTION('center_axis',(0.669130606358867,0.743144825477386,-9.42249022928259E-17));
#124762=DIRECTION('ref_axis',(-0.743144825477386,0.669130606358867,8.40817423203469E-31));
#124763=DIRECTION('center_axis',(0.579501624401492,0.643556859034944,-0.500012436350447));
#124764=DIRECTION('ref_axis',(0.333837986828513,0.372243731512272,0.866017784401743));
#124765=DIRECTION('center_axis',(-0.354588864042398,-0.393810830024467,
0.848044673146741));
#124766=DIRECTION('ref_axis',(-6.88772073415207E-15,-0.906978000082671,
-0.421177999622534));
#124767=DIRECTION('center_axis',(-0.334568647742382,-0.371576142361624,
0.866022511471549));
#124768=DIRECTION('ref_axis',(-0.576149740778052,-0.646569003433809,-0.499999999999994));
#124769=DIRECTION('center_axis',(0.334568664232095,0.371576145565864,-0.866022503726299));
#124770=DIRECTION('ref_axis',(3.33579067942304E-15,0.918982183096505,0.394299058014576));
#124771=DIRECTION('center_axis',(-0.354588823227312,-0.393810822491673,
0.848044693710598));
#124772=DIRECTION('ref_axis',(-0.564077964592822,-0.633246889653118,-0.529919264233215));
#124773=DIRECTION('center_axis',(-0.354588820328848,-0.393810781475683,
0.848044713969321));
#124774=DIRECTION('ref_axis',(-1.51628995831101E-15,-0.90697802766185,-0.421177940232653));
#124775=DIRECTION('center_axis',(0.669130606358845,0.743144825477406,3.65592620896146E-14));
#124776=DIRECTION('ref_axis',(-0.743144825477406,0.669130606358845,9.99649599890217E-31));
#124777=DIRECTION('center_axis',(-0.669130606358872,-0.743144825477382,
0.));
#124778=DIRECTION('ref_axis',(0.743144825477382,-0.669130606358872,0.));
#124779=DIRECTION('center_axis',(0.669130606358867,0.743144825477386,-9.42249022928259E-17));
#124780=DIRECTION('ref_axis',(-0.743144825477386,0.669130606358867,8.40817423203469E-31));
#124781=DIRECTION('center_axis',(0.669130606358845,0.743144825477406,3.65592620896126E-14));
#124782=DIRECTION('ref_axis',(-0.743144825477406,0.669130606358845,-2.40072602627987E-31));
#124783=DIRECTION('center_axis',(0.669130606358867,0.743144825477386,-9.42249022928259E-17));
#124784=DIRECTION('ref_axis',(-0.743144825477386,0.669130606358867,8.40817423203469E-31));
#124785=DIRECTION('center_axis',(-0.579517695131705,-0.643568108591948,
-0.499979330205379));
#124786=DIRECTION('ref_axis',(0.335267672852102,0.370911831387327,-0.866036951219309));
#124787=DIRECTION('center_axis',(0.33456875491201,0.371576246276113,0.866022425483302));
#124788=DIRECTION('ref_axis',(1.51465199069959E-15,-0.918982131463649,0.394299178353861));
#124789=DIRECTION('center_axis',(0.334568760918561,0.37157625294704,0.866022420300569));
#124790=DIRECTION('ref_axis',(0.743144825473852,-0.669130606362792,3.04218591854262E-12));
#124791=DIRECTION('center_axis',(-0.371576139134505,-0.334568658441323,
0.866022508722879));
#124792=DIRECTION('ref_axis',(-0.669130606356846,0.743144825479206,1.57354444798169E-12));
#124793=DIRECTION('center_axis',(-0.643556859036478,-0.579501624401258,
0.500012436348744));
#124794=DIRECTION('ref_axis',(-0.372243731475059,-0.333837986867333,-0.866017784402775));
#124795=DIRECTION('center_axis',(0.371576145565853,0.334568664232085,-0.866022503726308));
#124796=DIRECTION('ref_axis',(-0.918982183096513,7.65889573873005E-15,-0.394299058014558));
#124797=DIRECTION('center_axis',(0.743144825477379,0.669130606358875,0.));
#124798=DIRECTION('ref_axis',(-0.669130606358875,0.743144825477379,0.));
#124799=DIRECTION('center_axis',(-0.743144825477402,-0.66913060635885,1.0464735569497E-16));
#124800=DIRECTION('ref_axis',(0.66913060635885,-0.743144825477402,-1.36521113930368E-32));
#124801=DIRECTION('center_axis',(-0.743144825477406,-0.669130606358845,
0.));
#124802=DIRECTION('ref_axis',(0.669130606358845,-0.743144825477406,0.));
#124803=DIRECTION('center_axis',(-0.743144825477402,-0.66913060635885,1.0464735569497E-16));
#124804=DIRECTION('ref_axis',(0.66913060635885,-0.743144825477402,-1.36521113930368E-32));
#124805=DIRECTION('center_axis',(0.743144825477382,0.669130606358872,0.));
#124806=DIRECTION('ref_axis',(-0.669130606358872,0.743144825477382,0.));
#124807=DIRECTION('center_axis',(-0.393810436983627,-0.354588510146745,
-0.848045003637588));
#124808=DIRECTION('ref_axis',(-0.90697822335777,-1.33133695181472E-15,0.421177518814553));
#124809=DIRECTION('center_axis',(0.371576246276117,0.334568754912014,0.866022425483298));
#124810=DIRECTION('ref_axis',(0.918982131463646,-3.28768502367003E-15,-0.394299178353865));
#124811=DIRECTION('center_axis',(0.393810430452539,0.354588475164265,0.848045021297494));
#124812=DIRECTION('ref_axis',(0.633098037499372,0.564245025063572,-0.529919264233196));
#124813=DIRECTION('center_axis',(-0.393810395274859,-0.354588472592001,
-0.848045038708636));
#124814=DIRECTION('ref_axis',(-0.906978247051286,-3.29122279906641E-15,
0.421177467792112));
#124815=DIRECTION('center_axis',(0.37157626360525,0.334568756367432,0.866022417485778));
#124816=DIRECTION('ref_axis',(0.646617000437273,0.576095872876662,-0.49999999999998));
#124817=DIRECTION('center_axis',(0.643568108591639,0.579517695132388,0.499979330204985));
#124818=DIRECTION('ref_axis',(-0.370911831408801,-0.335267672827688,0.866036951219563));
#124819=DIRECTION('center_axis',(0.668950377172403,-0.743307065001336,0.));
#124820=DIRECTION('ref_axis',(0.743307065001336,0.668950377172402,0.));
#124821=DIRECTION('center_axis',(-0.743144825477402,-0.66913060635885,1.0464735569497E-16));
#124822=DIRECTION('ref_axis',(0.66913060635885,-0.743144825477402,-1.36521113930368E-32));
#124823=DIRECTION('center_axis',(0.743144825477409,0.669130606358842,0.));
#124824=DIRECTION('ref_axis',(-0.669130606358842,0.743144825477409,0.));
#124825=DIRECTION('center_axis',(-3.61695511949404E-17,9.42249022928235E-17,
-1.));
#124826=DIRECTION('ref_axis',(0.,1.,1.12832121675104E-16));
#124827=DIRECTION('center_axis',(0.669310796197601,-0.742982542253406,0.));
#124828=DIRECTION('ref_axis',(0.742982542253406,0.669310796197601,0.));
#124829=DIRECTION('center_axis',(0.393810781475729,0.354588820328856,-0.848044713969297));
#124830=DIRECTION('ref_axis',(-0.906978027661826,-7.21760554452843E-15,
-0.421177940232705));
#124831=DIRECTION('center_axis',(0.393810395274862,0.354588472592004,0.848045038708633));
#124832=DIRECTION('ref_axis',(0.906978247051285,1.62635303421704E-15,-0.421177467792116));
#124833=DIRECTION('center_axis',(0.393810788839631,0.354588860891869,-0.848044693589267));
#124834=DIRECTION('ref_axis',(-0.633246889667058,-0.564077964577223,-0.52991926423316));
#124835=DIRECTION('center_axis',(0.393810830024499,0.354588864042362,-0.848044673146741));
#124836=DIRECTION('ref_axis',(-0.906978000082659,3.44782577783986E-15,-0.421177999622559));
#124837=DIRECTION('center_axis',(-0.393810430614147,-0.354588475221364,
-0.848045021198573));
#124838=DIRECTION('ref_axis',(0.627330796753185,0.570650194812477,-0.529919264233238));
#124839=DIRECTION('center_axis',(0.39381043698369,0.354588510146801,0.848045003637535));
#124840=DIRECTION('ref_axis',(0.906978223357735,-2.65352984180235E-15,-0.421177518814628));
#124841=DIRECTION('center_axis',(0.668938718831589,-0.743317556935091,0.));
#124842=DIRECTION('ref_axis',(0.743317556935091,0.668938718831589,0.));
#124843=DIRECTION('center_axis',(0.743144825477406,0.669130606358845,0.));
#124844=DIRECTION('ref_axis',(-0.669130606358845,0.743144825477406,0.));
#124845=DIRECTION('center_axis',(-3.61695511949404E-17,9.42249022928235E-17,
-1.));
#124846=DIRECTION('ref_axis',(0.,1.,1.20114286872534E-16));
#124847=DIRECTION('center_axis',(0.669322449283883,-0.742972044483925,0.));
#124848=DIRECTION('ref_axis',(0.742972044483925,0.669322449283883,0.));
#124849=DIRECTION('center_axis',(0.743144825477402,0.66913060635885,-1.0464735569497E-16));
#124850=DIRECTION('ref_axis',(-0.66913060635885,0.743144825477402,-1.26626413714807E-30));
#124851=DIRECTION('center_axis',(0.643597063368661,0.579456972966462,-0.500012436349118));
#124852=DIRECTION('ref_axis',(0.370919252629949,0.335308969648868,0.866017784402523));
#124853=DIRECTION('center_axis',(-0.393810830024549,-0.354588864042318,
0.848044673146736));
#124854=DIRECTION('ref_axis',(0.906978000082638,-3.66139072703648E-15,0.421177999622604));
#124855=DIRECTION('center_axis',(-0.371576128832128,-0.334568662768395,
0.866022511471554));
#124856=DIRECTION('ref_axis',(-0.640578396537439,-0.582802983768563,-0.499999999999984));
#124857=DIRECTION('center_axis',(0.371576145565796,0.334568664232034,-0.866022503726352));
#124858=DIRECTION('ref_axis',(-0.91898218309654,3.67733214476396E-16,-0.394299058014493));
#124859=DIRECTION('center_axis',(-0.393810788646935,-0.354588860815713,
0.848044693710593));
#124860=DIRECTION('ref_axis',(-0.627180210735122,-0.570815694122663,-0.529919264233251));
#124861=DIRECTION('center_axis',(-0.393810781475744,-0.354588820328778,
0.848044713969322));
#124862=DIRECTION('ref_axis',(0.906978027661825,6.0864701038141E-15,0.421177940232708));
#124863=DIRECTION('center_axis',(0.743144825477406,0.669130606358845,4.0439119200333E-15));
#124864=DIRECTION('ref_axis',(-0.669130606358845,0.743144825477406,3.55234324240431E-31));
#124865=DIRECTION('center_axis',(-0.743144825477406,-0.669130606358845,
0.));
#124866=DIRECTION('ref_axis',(0.669130606358845,-0.743144825477406,0.));
#124867=DIRECTION('center_axis',(0.743144825477402,0.66913060635885,-1.0464735569497E-16));
#124868=DIRECTION('ref_axis',(-0.66913060635885,0.743144825477402,6.45362564166036E-31));
#124869=DIRECTION('center_axis',(0.743144825477406,0.669130606358845,4.04391192003308E-15));
#124870=DIRECTION('ref_axis',(-0.669130606358845,0.743144825477406,1.02141021320469E-31));
#124871=DIRECTION('center_axis',(0.743144825477402,0.66913060635885,-1.0464735569497E-16));
#124872=DIRECTION('ref_axis',(-0.66913060635885,0.743144825477402,6.45362564166036E-31));
#124873=DIRECTION('center_axis',(-0.643614221961378,-0.57946648104669,-0.499979330205176));
#124874=DIRECTION('ref_axis',(0.372201885190803,0.333834922952869,-0.866036951219441));
#124875=DIRECTION('center_axis',(0.371576246276125,0.334568754912021,0.866022425483293));
#124876=DIRECTION('ref_axis',(0.918982131463643,-6.34168247799913E-15,-0.394299178353873));
#124877=DIRECTION('center_axis',(0.371576252947737,0.334568760919143,0.866022420300046));
#124878=DIRECTION('ref_axis',(0.669130606360272,-0.743144825476121,-1.11896493554479E-12));
#124879=DIRECTION('center_axis',(-0.404512553894778,-0.29389557351658,0.866022508719539));
#124880=DIRECTION('ref_axis',(-0.587785252299528,0.809016994369821,-5.07030988789205E-12));
#124881=DIRECTION('center_axis',(-0.700605801487114,-0.509057044366917,
0.500012436348355));
#124882=DIRECTION('ref_axis',(-0.405100113158709,-0.293099122169683,-0.866017784402932));
#124883=DIRECTION('center_axis',(0.404512560891477,0.293895578600006,-0.86602250372631));
#124884=DIRECTION('ref_axis',(-0.906035256115479,9.01705582438248E-15,-0.423202214875771));
#124885=DIRECTION('center_axis',(0.80901699437495,0.58778525229247,0.));
#124886=DIRECTION('ref_axis',(-0.58778525229247,0.80901699437495,0.));
#124887=DIRECTION('center_axis',(-0.809016994374955,-0.587785252292463,
1.13923270769253E-16));
#124888=DIRECTION('ref_axis',(0.587785252292463,-0.809016994374955,7.17089999548893E-33));
#124889=DIRECTION('center_axis',(-0.80901699437495,-0.58778525229247,0.));
#124890=DIRECTION('ref_axis',(0.58778525229247,-0.80901699437495,0.));
#124891=DIRECTION('center_axis',(-0.809016994374955,-0.587785252292463,
1.13923270769253E-16));
#124892=DIRECTION('ref_axis',(0.587785252292463,-0.809016994374955,7.17089999548893E-33));
#124893=DIRECTION('center_axis',(0.80901699437495,0.58778525229247,0.));
#124894=DIRECTION('ref_axis',(-0.58778525229247,0.80901699437495,0.));
#124895=DIRECTION('center_axis',(-0.428717694262757,-0.31148163739029,-0.848045003637595));
#124896=DIRECTION('ref_axis',(-0.892442058026274,5.80484162998979E-15,0.451162025292275));
#124897=DIRECTION('center_axis',(0.404512670528679,0.293895658256096,0.866022425483297));
#124898=DIRECTION('ref_axis',(0.906035197473497,-3.36511067292208E-15,-0.423202340422593));
#124899=DIRECTION('center_axis',(0.428717684113496,0.311481603278383,0.848045021297507));
#124900=DIRECTION('ref_axis',(0.68860952557487,0.494977266833581,-0.529919264233252));
#124901=DIRECTION('center_axis',(-0.428717648856936,-0.31148160440103,-0.848045038708641));
#124902=DIRECTION('ref_axis',(-0.892442084777727,-1.51672008863495E-15,
0.451161972375314));
#124903=DIRECTION('center_axis',(0.404512687914156,0.293895657893397,0.866022417485755));
#124904=DIRECTION('ref_axis',(0.703293181141416,0.505350078025127,-0.499999999999986));
#124905=DIRECTION('center_axis',(0.700618669263901,0.509071851162835,0.499979330205284));
#124906=DIRECTION('ref_axis',(-0.403924952198554,-0.294660197709245,0.866036951219372));
#124907=DIRECTION('center_axis',(0.587589051772177,-0.809159506053951,4.42100154633563E-14));
#124908=DIRECTION('ref_axis',(0.809159506053951,0.587589051772177,1.06274147446815E-27));
#124909=DIRECTION('center_axis',(-0.809016994374955,-0.587785252292463,
1.13923270769253E-16));
#124910=DIRECTION('ref_axis',(0.587785252292463,-0.809016994374955,7.17089999548893E-33));
#124911=DIRECTION('center_axis',(0.80901699437495,0.58778525229247,0.));
#124912=DIRECTION('ref_axis',(-0.58778525229247,0.80901699437495,0.));
#124913=DIRECTION('center_axis',(-2.68936361206573E-17,8.27701011433304E-17,
-1.));
#124914=DIRECTION('ref_axis',(0.,1.,1.12832121675104E-16));
#124915=DIRECTION('center_axis',(0.587981418248456,-0.808874435122371,0.));
#124916=DIRECTION('ref_axis',(0.808874435122371,0.587981418248456,0.));
#124917=DIRECTION('center_axis',(0.428718069290566,0.311481909863963,-0.848044713969297));
#124918=DIRECTION('ref_axis',(-0.892441837073379,4.20951290950153E-15,-0.451162462358176));
#124919=DIRECTION('center_axis',(0.428717648856939,0.311481604401032,0.848045038708639));
#124920=DIRECTION('ref_axis',(0.892442084777726,6.53865308856261E-16,-0.451161972375317));
#124921=DIRECTION('center_axis',(0.428718080852843,0.311481949436789,-0.848044693589266));
#124922=DIRECTION('ref_axis',(-0.688740099740917,-0.494795562230913,-0.52991926423321));
#124923=DIRECTION('center_axis',(0.428718122142669,0.3114819482633,-0.848044673146741));
#124924=DIRECTION('ref_axis',(-0.89244180593479,-4.45144579489326E-15,-0.451162523953232));
#124925=DIRECTION('center_axis',(-0.428717684279335,-0.311481603319502,
-0.848045021198567));
#124926=DIRECTION('ref_axis',(0.683543400919167,0.501950189216426,-0.529919264233197));
#124927=DIRECTION('center_axis',(0.42871769426279,0.311481637390314,0.84804500363757));
#124928=DIRECTION('ref_axis',(0.892442058026255,-3.92099685579204E-15,-0.451162025292314));
#124929=DIRECTION('center_axis',(0.587576360591332,-0.809168721883295,1.21071329521359E-14));
#124930=DIRECTION('ref_axis',(0.809168721883294,0.587576360591332,-4.66403124080741E-29));
#124931=DIRECTION('center_axis',(0.80901699437495,0.58778525229247,-3.21147992436137E-14));
#124932=DIRECTION('ref_axis',(-0.58778525229247,0.80901699437495,6.08123400109255E-31));
#124933=DIRECTION('center_axis',(-2.68936361206573E-17,8.27701011433304E-17,
-1.));
#124934=DIRECTION('ref_axis',(0.,1.,1.20114286872534E-16));
#124935=DIRECTION('center_axis',(0.587994104813612,-0.80886521293998,-1.20677258718689E-14));
#124936=DIRECTION('ref_axis',(0.80886521293998,0.587994104813612,1.52456665748993E-28));
#124937=DIRECTION('center_axis',(0.809016994374955,0.587785252292463,-1.13923270769253E-16));
#124938=DIRECTION('ref_axis',(-0.587785252292463,0.809016994374955,-2.72904051338169E-30));
#124939=DIRECTION('center_axis',(0.700641118228982,0.509008435040225,-0.50001243635008));
#124940=DIRECTION('ref_axis',(0.403936649504382,0.294700492511635,0.866017784402014));
#124941=DIRECTION('center_axis',(-0.428718122142697,-0.311481948263293,
0.848044673146729));
#124942=DIRECTION('ref_axis',(0.892441805934777,-5.0778461836944E-15,0.451162523953257));
#124943=DIRECTION('center_axis',(-0.404512544096507,-0.293895578893441,
0.866022511471532));
#124944=DIRECTION('ref_axis',(-0.697988741332449,-0.512651652658167,-0.499999999999993));
#124945=DIRECTION('center_axis',(0.404512560891374,0.293895578599939,-0.866022503726381));
#124946=DIRECTION('ref_axis',(-0.906035256115533,6.95641201217777E-15,-0.423202214875654));
#124947=DIRECTION('center_axis',(-0.428718080655422,-0.311481949378178,
0.848044693710597));
#124948=DIRECTION('ref_axis',(-0.683410939228684,-0.50213052241134,-0.529919264233225));
#124949=DIRECTION('center_axis',(-0.428718069290593,-0.311481909863876,
0.848044713969316));
#124950=DIRECTION('ref_axis',(0.89244183707337,5.21317305093966E-15,0.451162462358194));
#124951=DIRECTION('center_axis',(0.80901699437495,0.58778525229247,-3.2114799243612E-14));
#124952=DIRECTION('ref_axis',(-0.58778525229247,0.80901699437495,-4.13565546558353E-30));
#124953=DIRECTION('center_axis',(-0.809016994374976,-0.587785252292434,
0.));
#124954=DIRECTION('ref_axis',(0.587785252292434,-0.809016994374976,0.));
#124955=DIRECTION('center_axis',(0.809016994374955,0.587785252292463,-1.13923270769253E-16));
#124956=DIRECTION('ref_axis',(-0.587785252292463,0.809016994374955,-2.72904051338169E-30));
#124957=DIRECTION('center_axis',(0.80901699437495,0.58778525229247,0.));
#124958=DIRECTION('ref_axis',(-0.58778525229247,0.80901699437495,0.));
#124959=DIRECTION('center_axis',(0.809016994374955,0.587785252292463,-1.13923270769253E-16));
#124960=DIRECTION('ref_axis',(-0.587785252292463,0.809016994374955,-2.72904051338169E-30));
#124961=DIRECTION('center_axis',(-0.700659176689738,-0.50901609747425,-0.499979330205303));
#124962=DIRECTION('ref_axis',(0.405058175803442,0.293100449227661,-0.866036951219364));
#124963=DIRECTION('center_axis',(0.404512670528659,0.293895658256089,0.866022425483309));
#124964=DIRECTION('ref_axis',(0.906035197473507,3.41535267324782E-15,-0.423202340422573));
#124965=DIRECTION('center_axis',(0.4045126777905,0.293895663532146,0.86602242030086));
#124966=DIRECTION('ref_axis',(0.587785252291003,-0.809016994376015,1.04902962708232E-12));
#124967=DIRECTION('center_axis',(-0.433017044458743,-0.250002507181973,
0.866022508720728));
#124968=DIRECTION('ref_axis',(-0.500000000003119,0.866025403782638,-2.02812395516345E-12));
#124969=DIRECTION('center_axis',(-0.749978760163342,-0.433035128829169,
0.500012436349099));
#124970=DIRECTION('ref_axis',(-0.433518133182558,-0.24914900220652,-0.866017784402495));
#124971=DIRECTION('center_axis',(0.43301705195027,0.250002511507201,-0.866022503726312));
#124972=DIRECTION('ref_axis',(-0.894424794863788,-1.72347843759609E-15,
-0.447218387740119));
#124973=DIRECTION('center_axis',(0.866025403784433,0.50000000000001,0.));
#124974=DIRECTION('ref_axis',(-0.50000000000001,0.866025403784433,0.));
#124975=DIRECTION('center_axis',(-0.866025403784445,-0.499999999999989,
1.21951018649011E-16));
#124976=DIRECTION('ref_axis',(0.499999999999989,-0.866025403784445,7.73386177718291E-33));
#124977=DIRECTION('center_axis',(-0.86602540378444,-0.499999999999998,-1.3659239968321E-14));
#124978=DIRECTION('ref_axis',(0.499999999999998,-0.86602540378444,-1.8627714006626E-28));
#124979=DIRECTION('center_axis',(-0.866025403784445,-0.499999999999989,
1.21951018649011E-16));
#124980=DIRECTION('ref_axis',(0.499999999999989,-0.866025403784445,7.73386177718291E-33));
#124981=DIRECTION('center_axis',(0.866025403784463,0.499999999999957,0.));
#124982=DIRECTION('ref_axis',(-0.499999999999957,0.866025403784463,0.));
#124983=DIRECTION('center_axis',(-0.458927830768608,-0.264962106632866,
-0.848045003637598));
#124984=DIRECTION('ref_axis',(-0.879478602053342,-2.31870210175756E-15,
0.475938429348061));
#124985=DIRECTION('center_axis',(0.43301716931321,0.250002579266718,0.866022425483292));
#124986=DIRECTION('ref_axis',(0.89442473021642,-2.13116799657304E-15,-0.447218517033099));
#124987=DIRECTION('center_axis',(0.458927817109519,0.264962073768271,0.848045021297519));
#124988=DIRECTION('ref_axis',(0.736576463609069,0.42028643405628,-0.529919264233161));
#124989=DIRECTION('center_axis',(-0.458927782163189,-0.264962078570514,
-0.848045038708658));
#124990=DIRECTION('ref_axis',(-0.879478631391259,-6.14731538978695E-15,
0.475938375135014));
#124991=DIRECTION('center_axis',(0.433017186566327,0.250002577087191,0.866022417485798));
#124992=DIRECTION('ref_axis',(0.752263934579074,0.429067561966284,-0.49999999999992));
#124993=DIRECTION('center_axis',(0.749993105181526,0.433048509462592,0.49997933020516));
#124994=DIRECTION('ref_axis',(-0.432512586703677,-0.250824363779544,0.86603695121945));
#124995=DIRECTION('center_axis',(0.499789977759954,-0.866146626230631,0.));
#124996=DIRECTION('ref_axis',(0.866146626230631,0.499789977759954,0.));
#124997=DIRECTION('center_axis',(-0.866025403784445,-0.499999999999989,
1.21951018649011E-16));
#124998=DIRECTION('ref_axis',(0.499999999999989,-0.866025403784445,7.73386177718291E-33));
#124999=DIRECTION('center_axis',(0.86602540378444,0.499999999999998,0.));
#125000=DIRECTION('ref_axis',(-0.499999999999998,0.86602540378444,0.));
#125001=DIRECTION('center_axis',(-1.88658882408992E-17,7.04084534449537E-17,
-1.));
#125002=DIRECTION('ref_axis',(0.,1.,1.12832121675104E-16));
#125003=DIRECTION('center_axis',(0.500209992837931,-0.865904130412297,0.));
#125004=DIRECTION('ref_axis',(0.865904130412297,0.500209992837931,0.));
#125005=DIRECTION('center_axis',(0.458928232223227,0.264962338412753,-0.848044713969322));
#125006=DIRECTION('ref_axis',(-0.879478359737735,3.52718193142461E-15,-0.475938877118715));
#125007=DIRECTION('center_axis',(0.458927782163212,0.264962078570527,0.848045038708642));
#125008=DIRECTION('ref_axis',(0.879478631391246,-1.38546995367359E-15,-0.475938375135038));
#125009=DIRECTION('center_axis',(0.458928247861521,0.264962376555267,-0.848044693589282));
#125010=DIRECTION('ref_axis',(-0.736687329167645,-0.420092076143344,-0.529919264233163));
#125011=DIRECTION('center_axis',(0.458928288799633,0.264962371077255,-0.848044673146739));
#125012=DIRECTION('ref_axis',(-0.879478325588519,2.1428654450467E-15,-0.475938940222393));
#125013=DIRECTION('center_axis',(-0.458927817275468,-0.264962073797545,
-0.848045021198568));
#125014=DIRECTION('ref_axis',(0.732266960582963,0.427750712253125,-0.529919264233274));
#125015=DIRECTION('center_axis',(0.458927830768628,0.264962106632877,0.848045003637584));
#125016=DIRECTION('ref_axis',(0.879478602053331,-3.90796687788124E-15,-0.475938429348081));
#125017=DIRECTION('center_axis',(0.499776392786184,-0.866154464985103,-2.36620233737299E-14));
#125018=DIRECTION('ref_axis',(0.866154464985103,0.499776392786184,2.85780049921816E-28));
#125019=DIRECTION('center_axis',(0.86602540378444,0.499999999999998,0.));
#125020=DIRECTION('ref_axis',(-0.499999999999998,0.86602540378444,0.));
#125021=DIRECTION('center_axis',(-1.88658882408992E-17,7.04084534449537E-17,
-1.));
#125022=DIRECTION('ref_axis',(0.,1.,1.20114286872534E-16));
#125023=DIRECTION('center_axis',(0.500223573885301,-0.865896284857152,0.));
#125024=DIRECTION('ref_axis',(0.865896284857152,0.500223573885301,0.));
#125025=DIRECTION('center_axis',(0.866025403784445,0.499999999999989,-1.21951018649011E-16));
#125026=DIRECTION('ref_axis',(-0.499999999999989,0.866025403784445,-1.28346985693928E-30));
#125027=DIRECTION('center_axis',(0.75000880237976,0.432983094186958,-0.500012436346502));
#125028=DIRECTION('ref_axis',(0.432528431881907,0.250863215138471,0.866017784404089));
#125029=DIRECTION('center_axis',(-0.458928288799653,-0.26496237107725,0.84804467314673));
#125030=DIRECTION('ref_axis',(0.879478325588507,4.12607120826034E-15,0.475938940222415));
#125031=DIRECTION('center_axis',(-0.43301703527827,-0.250002513554088,0.866022511471529));
#125032=DIRECTION('ref_axis',(-0.747751775424576,-0.436883602747219,-0.500000000000005));
#125033=DIRECTION('center_axis',(0.433017051950193,0.250002511507141,-0.866022503726367));
#125034=DIRECTION('ref_axis',(-0.894424794863831,4.51772688567625E-15,-0.447218387740032));
#125035=DIRECTION('center_axis',(-0.458928247653241,-0.264962376527612,
0.848044693710636));
#125036=DIRECTION('ref_axis',(-0.732154074453982,-0.427943903631124,-0.529919264233136));
#125037=DIRECTION('center_axis',(-0.458928232223214,-0.264962338412753,
0.848044713969329));
#125038=DIRECTION('ref_axis',(0.879478359737742,3.73673734303752E-16,0.475938877118702));
#125039=DIRECTION('center_axis',(0.86602540378444,0.499999999999998,3.36577552674943E-14));
#125040=DIRECTION('ref_axis',(-0.499999999999998,0.86602540378444,4.57373621403242E-28));
#125041=DIRECTION('center_axis',(-0.866025403784433,-0.50000000000001,0.));
#125042=DIRECTION('ref_axis',(0.50000000000001,-0.866025403784433,0.));
#125043=DIRECTION('center_axis',(0.866025403784445,0.499999999999989,-1.21951018649011E-16));
#125044=DIRECTION('ref_axis',(-0.499999999999989,0.866025403784445,-1.28346985693928E-30));
#125045=DIRECTION('center_axis',(0.86602540378444,0.499999999999998,-2.73184799366421E-14));
#125046=DIRECTION('ref_axis',(-0.499999999999998,0.86602540378444,-3.72554280132519E-28));
#125047=DIRECTION('center_axis',(0.866025403784445,0.499999999999989,-1.21951018649011E-16));
#125048=DIRECTION('ref_axis',(-0.499999999999989,0.866025403784445,-1.28346985693928E-30));
#125049=DIRECTION('center_axis',(-0.750027562856474,-0.432988827019046,
-0.499979330205008));
#125050=DIRECTION('ref_axis',(0.433476564273207,0.249154705651457,-0.866036951219538));
#125051=DIRECTION('center_axis',(0.433017169313169,0.250002579266687,0.866022425483321));
#125052=DIRECTION('ref_axis',(0.894424730216444,-7.57227756159649E-15,-0.447218517033052));
#125053=DIRECTION('center_axis',(0.433017177087304,0.250002583755051,0.866022420300503));
#125054=DIRECTION('ref_axis',(0.499999999999399,-0.866025403784786,3.84644196595208E-13));
#125055=DIRECTION('center_axis',(-0.456777309670065,-0.203370361063163,
0.866022508721116));
#125056=DIRECTION('ref_axis',(-0.406736643075047,0.913545457642936,4.54579507195795E-13));
#125057=DIRECTION('center_axis',(-0.791134794601669,-0.352268789800729,
0.500012436348242));
#125058=DIRECTION('ref_axis',(0.457186437801428,0.202469153670706,0.866017784403016));
#125059=DIRECTION('center_axis',(0.456777317573273,0.203370364581918,-0.866022503726308));
#125060=DIRECTION('ref_axis',(-0.884507036382097,-5.7553372295389E-15,-0.466526850878445));
#125061=DIRECTION('center_axis',(0.913545457642598,0.406736643075807,0.));
#125062=DIRECTION('ref_axis',(-0.406736643075807,0.913545457642598,0.));
#125063=DIRECTION('center_axis',(-0.913545457642606,-0.406736643075789,
1.2864264564856E-16));
#125064=DIRECTION('ref_axis',(0.406736643075789,-0.913545457642606,1.48709352463992E-32));
#125065=DIRECTION('center_axis',(-0.913545457642598,-0.406736643075807,
-1.11114268233636E-14));
#125066=DIRECTION('ref_axis',(0.406736643075807,-0.913545457642598,1.92826049468501E-31));
#125067=DIRECTION('center_axis',(-0.913545457642606,-0.406736643075789,
1.2864264564856E-16));
#125068=DIRECTION('ref_axis',(0.406736643075789,-0.913545457642606,1.48709352463992E-32));
#125069=DIRECTION('center_axis',(0.913545457642598,0.406736643075807,0.));
#125070=DIRECTION('ref_axis',(-0.406736643075807,0.913545457642598,0.));
#125071=DIRECTION('center_axis',(-0.484109857923765,-0.215539595588304,
-0.84804500363758));
#125072=DIRECTION('ref_axis',(-0.868458021515998,-1.76836178502353E-15,
0.495762710240009));
#125073=DIRECTION('center_axis',(0.456777441376074,0.20337041970247,0.866022425483295));
#125074=DIRECTION('ref_axis',(0.884506966812058,2.53897267290044E-15,-0.466526982779059));
#125075=DIRECTION('center_axis',(0.484109840901723,0.215539564337118,0.848045021297498));
#125076=DIRECTION('ref_axis',(0.776473315749238,0.340990855191042,-0.52991926423321));
#125077=DIRECTION('center_axis',(-0.484109806651279,-0.215539572760323,
-0.848045038708652));
#125078=DIRECTION('ref_axis',(-0.868458052949962,-1.14722910183595E-15,
0.495762655175196));
#125079=DIRECTION('center_axis',(0.456777458308629,0.203370415727499,0.866022417485791));
#125080=DIRECTION('ref_axis',(0.792992726927746,0.348084091908492,-0.499999999999938));
#125081=DIRECTION('center_axis',(0.791150459692712,0.352280597671149,0.499979330205228));
#125082=DIRECTION('ref_axis',(0.456361522792999,0.204240445643489,-0.866036951219406));
#125083=DIRECTION('center_axis',(0.406515100163541,-0.913644062717548,0.));
#125084=DIRECTION('ref_axis',(0.913644062717548,0.406515100163541,0.));
#125085=DIRECTION('center_axis',(-0.913545457642606,-0.406736643075789,
1.2864264564856E-16));
#125086=DIRECTION('ref_axis',(0.406736643075789,-0.913545457642606,1.48709352463992E-32));
#125087=DIRECTION('center_axis',(0.913545457642618,0.406736643075761,0.));
#125088=DIRECTION('ref_axis',(-0.406736643075761,0.913545457642618,0.));
#125089=DIRECTION('center_axis',(-1.2174261241351E-17,5.72753959967181E-17,
-1.));
#125090=DIRECTION('ref_axis',(0.,1.,1.12832121675104E-16));
#125091=DIRECTION('center_axis',(0.406958162070199,-0.913446798847336,0.));
#125092=DIRECTION('ref_axis',(0.913446798847336,0.406958162070199,0.));
#125093=DIRECTION('center_axis',(0.484110281406754,0.215539784135092,-0.8480447139693));
#125094=DIRECTION('ref_axis',(-0.868457761888264,-2.53993026454612E-15,
-0.495763165045596));
#125095=DIRECTION('center_axis',(0.484109806651376,0.215539572760315,0.848045038708598));
#125096=DIRECTION('ref_axis',(0.868458052949906,2.93749497420107E-15,-0.495762655175295));
#125097=DIRECTION('center_axis',(0.484110300945566,0.215539820435717,-0.848044693589278));
#125098=DIRECTION('ref_axis',(-0.776563258037241,-0.340785973392545,-0.529919264233223));
#125099=DIRECTION('center_axis',(0.484110341087594,0.215539810706745,-0.848044673146736));
#125100=DIRECTION('ref_axis',(-0.868457725299277,3.13556863905275E-15,-0.495763229140692));
#125101=DIRECTION('center_axis',(-0.484109841074426,-0.215539564338561,
-0.848045021198543));
#125102=DIRECTION('ref_axis',(0.772967650152,0.348864709039245,-0.529919264233202));
#125103=DIRECTION('center_axis',(0.484109857923745,0.215539595588295,0.848045003637594));
#125104=DIRECTION('ref_axis',(0.868458021516011,-2.89436985092629E-15,-0.495762710239986));
#125105=DIRECTION('center_axis',(0.406500770236715,-0.913650438514073,-2.74957490176846E-15));
#125106=DIRECTION('ref_axis',(0.913650438514073,0.406500770236715,5.03959061829502E-30));
#125107=DIRECTION('center_axis',(0.913545457642598,0.406736643075807,4.99133465116398E-14));
#125108=DIRECTION('ref_axis',(-0.406736643075807,0.913545457642598,-2.82923979546378E-31));
#125109=DIRECTION('center_axis',(-1.2174261241351E-17,5.72753959967181E-17,
-1.));
#125110=DIRECTION('ref_axis',(0.,1.,0.));
#125111=DIRECTION('center_axis',(0.406972488803016,-0.913440415876963,-2.71806413419201E-15));
#125112=DIRECTION('ref_axis',(0.913440415876963,0.406972488803016,-2.33723455769851E-29));
#125113=DIRECTION('center_axis',(0.913545457642606,0.406736643075789,-1.2864264564856E-16));
#125114=DIRECTION('ref_axis',(-0.406736643075789,0.913545457642606,-2.52138284268272E-30));
#125115=DIRECTION('center_axis',(0.791159233140775,0.352213899940326,-0.500012436350263));
#125116=DIRECTION('ref_axis',(0.456381342221735,0.204277427954193,0.86601778440186));
#125117=DIRECTION('center_axis',(-0.484110341087625,-0.215539810706664,
0.848044673146739));
#125118=DIRECTION('ref_axis',(0.868457725299263,1.28125800661297E-15,0.495763229140715));
#125119=DIRECTION('center_axis',(-0.456777301206709,-0.203370368359864,
0.866022511471549));
#125120=DIRECTION('ref_axis',(-0.789322284582009,-0.356328964669238,-0.499999999999987));
#125121=DIRECTION('center_axis',(0.456777317573189,0.203370364581875,-0.866022503726362));
#125122=DIRECTION('ref_axis',(-0.884507036382145,-1.64379723448746E-15,
-0.466526850878354));
#125123=DIRECTION('center_axis',(-0.484110300736294,-0.215539820428334,
0.848044693710618));
#125124=DIRECTION('ref_axis',(-0.772875576443094,-0.349068641863358,-0.529919264233171));
#125125=DIRECTION('center_axis',(-0.484110281406742,-0.215539784135016,
0.848044713969326));
#125126=DIRECTION('ref_axis',(0.868457761888277,-2.39045094596213E-15,0.495763165045575));
#125127=DIRECTION('center_axis',(0.913545457642598,0.406736643075807,1.11114268233636E-14));
#125128=DIRECTION('ref_axis',(-0.406736643075807,0.913545457642598,-1.92826049468501E-31));
#125129=DIRECTION('center_axis',(-0.913545457642594,-0.406736643075817,
0.));
#125130=DIRECTION('ref_axis',(0.406736643075817,-0.913545457642593,0.));
#125131=DIRECTION('center_axis',(0.913545457642606,0.406736643075789,-1.2864264564856E-16));
#125132=DIRECTION('ref_axis',(-0.406736643075789,0.913545457642606,-2.52138284268272E-30));
#125133=DIRECTION('center_axis',(0.913545457642598,0.406736643075807,-6.10247733350034E-14));
#125134=DIRECTION('ref_axis',(-0.406736643075807,0.913545457642598,1.41175456657023E-30));
#125135=DIRECTION('center_axis',(0.913545457642606,0.406736643075789,-1.2864264564856E-16));
#125136=DIRECTION('ref_axis',(-0.406736643075789,0.913545457642606,-2.52138284268272E-30));
#125137=DIRECTION('center_axis',(-0.791178490090679,-0.352217640366629,
-0.499979330205157));
#125138=DIRECTION('ref_axis',(0.457145692795638,0.202479170980401,-0.866036951219453));
#125139=DIRECTION('center_axis',(0.45677744137607,0.203370419702469,0.866022425483297));
#125140=DIRECTION('ref_axis',(0.884506966812061,-6.18778487782607E-15,-0.466526982779054));
#125141=DIRECTION('center_axis',(0.456777449578343,0.203370423354363,0.866022420299481));
#125142=DIRECTION('ref_axis',(0.406736643083121,-0.913545457639341,-4.61573035911191E-12));
#125143=DIRECTION('center_axis',(-0.475533027090268,-0.154510046710891,
0.866022508721202));
#125144=DIRECTION('ref_axis',(-0.30901699437301,0.951056516295783,1.18890024959428E-12));
#125145=DIRECTION('center_axis',(-0.823622990673951,-0.267642920194547,
0.50001243634837));
#125146=DIRECTION('ref_axis',(0.475845712142861,0.153571010718269,0.866017784402967));
#125147=DIRECTION('center_axis',(0.475533035318122,0.154510049384294,-0.866022503726316));
#125148=DIRECTION('ref_axis',(-0.876548788012445,9.99951496082734E-16,-0.48131301897405));
#125149=DIRECTION('center_axis',(0.951056516295165,0.309016994374914,-6.04047112789571E-14));
#125150=DIRECTION('ref_axis',(-0.309016994374914,0.951056516295164,-2.46817372928747E-30));
#125151=DIRECTION('center_axis',(-0.951056516295158,-0.309016994374935,
1.33924836902178E-16));
#125152=DIRECTION('ref_axis',(0.309016994374935,-0.951056516295158,-9.27809067577952E-33));
#125153=DIRECTION('center_axis',(-0.951056516295165,-0.309016994374914,
-5.19628367180445E-14));
#125154=DIRECTION('ref_axis',(0.309016994374914,-0.951056516295164,-1.42492764277297E-30));
#125155=DIRECTION('center_axis',(-0.951056516295158,-0.309016994374935,
1.33924836902178E-16));
#125156=DIRECTION('ref_axis',(0.309016994374935,-0.951056516295158,3.04786096829879E-33));
#125157=DIRECTION('center_axis',(0.951056516295165,0.309016994374914,0.));
#125158=DIRECTION('ref_axis',(-0.309016994374914,0.951056516295164,0.));
#125159=DIRECTION('center_axis',(-0.503987876168997,-0.163755587629879,
-0.848045003637577));
#125160=DIRECTION('ref_axis',(-0.859649462041482,-2.31443907975747E-15,
0.510884333691875));
#125161=DIRECTION('center_axis',(0.475533164204451,0.15451009126196,0.866022425483269));
#125162=DIRECTION('ref_axis',(0.876548714628815,1.61550628132638E-15,-0.481313152617475));
#125163=DIRECTION('center_axis',(0.503987855974665,0.163755558325779,0.848045021297497));
#125164=DIRECTION('ref_axis',(0.807862963764707,0.257959309139721,-0.529919264233205));
#125165=DIRECTION('center_axis',(-0.503987822791223,-0.163755570286389,
-0.848045038708642));
#125166=DIRECTION('ref_axis',(-0.859649495083692,-4.55730791939964E-15,
0.510884278092753));
#125167=DIRECTION('center_axis',(0.475533180627103,0.154510085543892,0.866022417485766));
#125168=DIRECTION('ref_axis',(0.825033325009168,0.263286939714686,-0.499999999999991));
#125169=DIRECTION('center_axis',(0.82363980420873,0.267653025932129,0.499979330205139));
#125170=DIRECTION('ref_axis',(0.475210466543398,0.155418826433942,-0.866036951219463));
#125171=DIRECTION('center_axis',(0.308786358060973,-0.951131423661021,2.59834647143935E-14));
#125172=DIRECTION('ref_axis',(0.951131423661021,0.308786358060973,1.96167695623581E-28));
#125173=DIRECTION('center_axis',(-0.951056516295158,-0.309016994374935,
1.33924836902178E-16));
#125174=DIRECTION('ref_axis',(0.309016994374935,-0.951056516295158,-9.27809067577952E-33));
#125175=DIRECTION('center_axis',(0.951056516295165,0.309016994374914,0.));
#125176=DIRECTION('ref_axis',(-0.309016994374914,0.951056516295164,0.));
#125177=DIRECTION('center_axis',(-6.89206998773264E-18,4.35148173242952E-17,
-1.));
#125178=DIRECTION('ref_axis',(0.,1.,0.));
#125179=DIRECTION('center_axis',(0.309247612517378,-0.95098155300316,0.));
#125180=DIRECTION('ref_axis',(0.95098155300316,0.309247612517378,0.));
#125181=DIRECTION('center_axis',(0.503988317040571,0.163755730877732,-0.848044713969324));
#125182=DIRECTION('ref_axis',(-0.859649189130473,-1.51298268767331E-15,
-0.510884792910614));
#125183=DIRECTION('center_axis',(0.503987822791218,0.163755570286387,0.848045038708645));
#125184=DIRECTION('ref_axis',(0.859649495083696,-2.0335524798323E-15,-0.510884278092747));
#125185=DIRECTION('center_axis',(0.503988340265571,0.163755764941051,-0.848044693589274));
#125186=DIRECTION('ref_axis',(-0.807930997363437,-0.257746148165048,-0.52991926423315));
#125187=DIRECTION('center_axis',(0.503988379172015,0.163755751065486,-0.84804467314673));
#125188=DIRECTION('ref_axis',(-0.859649150669458,-3.94104971099401E-15,
-0.510884857627704));
#125189=DIRECTION('center_axis',(-0.503987856144593,-0.163755558315073,
-0.848045021198578));
#125190=DIRECTION('ref_axis',(0.805199544413242,0.266156471030219,-0.529919264233193));
#125191=DIRECTION('center_axis',(0.503987876168979,0.163755587629873,0.848045003637589));
#125192=DIRECTION('ref_axis',(0.859649462041493,-1.78492124839558E-15,-0.510884333691856));
#125193=DIRECTION('center_axis',(0.308771440182783,-0.951136266645033,-9.11326423007215E-15));
#125194=DIRECTION('ref_axis',(0.951136266645033,0.308771440182783,2.771149958367E-29));
#125195=DIRECTION('center_axis',(0.951056516295165,0.309016994374914,8.44187456091256E-15));
#125196=DIRECTION('ref_axis',(-0.309016994374914,0.951056516295164,1.39291926319097E-31));
#125197=DIRECTION('center_axis',(-6.89206998773264E-18,4.35148173242952E-17,
-1.));
#125198=DIRECTION('ref_axis',(0.,1.,0.));
#125199=DIRECTION('center_axis',(0.309262527968943,-0.95097670255073,0.));
#125200=DIRECTION('ref_axis',(0.950976702550729,0.309262527968943,0.));
#125201=DIRECTION('center_axis',(0.951056516295158,0.309016994374935,-1.33924836902178E-16));
#125202=DIRECTION('ref_axis',(-0.309016994374935,0.951056516295158,2.92272947789642E-30));
#125203=DIRECTION('center_axis',(0.823641557784016,0.267585776504269,-0.500012436349064));
#125204=DIRECTION('ref_axis',(0.475234043092174,0.155453534487958,0.86601778440253));
#125205=DIRECTION('center_axis',(-0.503988379172015,-0.163755751065433,
0.84804467314674));
#125206=DIRECTION('ref_axis',(0.859649150669461,4.80415871610856E-15,0.510884857627699));
#125207=DIRECTION('center_axis',(-0.475533019436127,-0.154510054852395,
0.866022511471538));
#125208=DIRECTION('ref_axis',(-0.822244813612915,-0.271870311889065,-0.500000000000005));
#125209=DIRECTION('center_axis',(0.475533035318005,0.15451004938422,-0.866022503726394));
#125210=DIRECTION('ref_axis',(-0.876548788012513,-2.02407478928591E-15,
-0.481313018973926));
#125211=DIRECTION('center_axis',(-0.503988340058875,-0.163755764948789,
0.848044693710618));
#125212=DIRECTION('ref_axis',(-0.805129291879029,-0.266368911010517,-0.529919264233189));
#125213=DIRECTION('center_axis',(-0.503988317040557,-0.163755730877752,
0.848044713969329));
#125214=DIRECTION('ref_axis',(0.85964918913048,3.98009309471949E-15,0.510884792910601));
#125215=DIRECTION('center_axis',(0.951056516295165,0.309016994374914,-6.04047112789571E-14));
#125216=DIRECTION('ref_axis',(-0.309016994374914,0.951056516295164,-2.46817372928747E-30));
#125217=DIRECTION('center_axis',(-0.951056516295165,-0.309016994374914,
0.));
#125218=DIRECTION('ref_axis',(0.309016994374914,-0.951056516295164,0.));
#125219=DIRECTION('center_axis',(0.951056516295158,0.309016994374935,-1.33924836902178E-16));
#125220=DIRECTION('ref_axis',(-0.309016994374935,0.951056516295158,2.92272947789642E-30));
#125221=DIRECTION('center_axis',(0.951056516295165,0.309016994374914,-4.3520962157132E-14));
#125222=DIRECTION('ref_axis',(-0.309016994374914,0.951056516295164,-1.2145041730042E-30));
#125223=DIRECTION('center_axis',(0.951056516295158,0.309016994374935,-1.33924836902178E-16));
#125224=DIRECTION('ref_axis',(-0.309016994374935,0.951056516295158,2.92272947789642E-30));
#125225=DIRECTION('center_axis',(-0.823661100222713,-0.267587483540128,
-0.499979330205332));
#125226=DIRECTION('ref_axis',(0.47580623744722,0.153585232131932,-0.866036951219346));
#125227=DIRECTION('center_axis',(0.475533164204429,0.154510091261957,0.866022425483281));
#125228=DIRECTION('ref_axis',(0.876548714628827,1.44586213632941E-15,-0.481313152617453));
#125229=DIRECTION('center_axis',(0.475533172742431,0.154510094036134,0.866022420300111));
#125230=DIRECTION('ref_axis',(0.309016994376992,-0.951056516294489,-1.25883555248922E-12));
#125231=DIRECTION('center_axis',(-0.48907870515122,-0.103956887952953,0.866022508722922));
#125232=DIRECTION('ref_axis',(-0.207911690817661,0.978147600733827,6.99353087993298E-14));
#125233=DIRECTION('center_axis',(-0.847087400905761,-0.180084698747582,
0.500012436349052));
#125234=DIRECTION('ref_axis',(0.489291521290444,0.102990311639969,0.866017784402598));
#125235=DIRECTION('center_axis',(0.489078713616366,0.103956889752291,-0.866022503726313));
#125236=DIRECTION('ref_axis',(-0.870740345484705,-2.30898284559697E-15,
-0.491743073916834));
#125237=DIRECTION('center_axis',(0.978147600733806,0.207911690817757,0.));
#125238=DIRECTION('ref_axis',(-0.207911690817757,0.978147600733806,0.));
#125239=DIRECTION('center_axis',(-0.978147600733808,-0.207911690817747,
1.37739719617122E-16));
#125240=DIRECTION('ref_axis',(0.207911690817747,-0.978147600733808,-5.77321332412281E-33));
#125241=DIRECTION('center_axis',(-0.978147600733807,-0.207911690817754,
-2.83991567709909E-15));
#125242=DIRECTION('ref_axis',(0.207911690817754,-0.978147600733807,-8.10663864458446E-30));
#125243=DIRECTION('center_axis',(-0.978147600733808,-0.207911690817747,
1.37739719617122E-16));
#125244=DIRECTION('ref_axis',(0.207911690817747,-0.978147600733808,1.27157141419947E-32));
#125245=DIRECTION('center_axis',(0.978147600733806,0.207911690817757,0.));
#125246=DIRECTION('ref_axis',(-0.207911690817757,0.978147600733806,0.));
#125247=DIRECTION('center_axis',(-0.518344097776651,-0.110177439185352,
-0.848045003637583));
#125248=DIRECTION('ref_axis',(-0.85323958281187,2.74380692439891E-15,0.521519140898036));
#125249=DIRECTION('center_axis',(0.489078846174035,0.103956917928313,0.866022425483267));
#125250=DIRECTION('ref_axis',(0.870740269393757,1.63311310360591E-16,-0.491743208652736));
#125251=DIRECTION('center_axis',(0.518344074628942,0.110177412156896,0.848045021297499));
#125252=DIRECTION('ref_axis',(0.830401496088695,0.172101506931704,-0.529919264233235));
#125253=DIRECTION('center_axis',(-0.518344042878405,-0.11017742751637,-0.848045038708644));
#125254=DIRECTION('ref_axis',(-0.853239616987299,-4.34819448574131E-16,
0.521519084984785));
#125255=DIRECTION('center_axis',(0.489078861909502,0.103956910522811,0.866022417485748));
#125256=DIRECTION('ref_axis',(0.84803468533791,0.1756051606982,-0.499999999999992));
#125257=DIRECTION('center_axis',(0.847105178672016,0.180092991630677,0.499979330205324));
#125258=DIRECTION('ref_axis',(0.488852904975635,0.104894406045156,-0.866036951219356));
#125259=DIRECTION('center_axis',(0.207674488001815,-0.978197989689809,0.));
#125260=DIRECTION('ref_axis',(0.978197989689809,0.207674488001815,0.));
#125261=DIRECTION('center_axis',(-0.978147600733808,-0.207911690817747,
1.37739719617122E-16));
#125262=DIRECTION('ref_axis',(0.207911690817747,-0.978147600733808,-5.77321332412281E-33));
#125263=DIRECTION('center_axis',(0.978147600733806,0.207911690817757,0.));
#125264=DIRECTION('ref_axis',(-0.207911690817757,0.978147600733806,0.));
#125265=DIRECTION('center_axis',(-3.07718727278846E-18,2.92774812072065E-17,
-1.));
#125266=DIRECTION('ref_axis',(0.,1.,0.));
#125267=DIRECTION('center_axis',(0.208148881407602,-0.978097154258596,0.));
#125268=DIRECTION('ref_axis',(0.978097154258596,0.208148881407602,0.));
#125269=DIRECTION('center_axis',(0.518344551206563,0.110177535564868,-0.848044713969328));
#125270=DIRECTION('ref_axis',(-0.853239300541053,2.15107083335551E-15,-0.52151960271136));
#125271=DIRECTION('center_axis',(0.51834404287839,0.110177427516366,0.848045038708654));
#125272=DIRECTION('ref_axis',(0.853239616987309,-2.70652115665923E-15,-0.521519084984769));
#125273=DIRECTION('center_axis',(0.518344577867921,0.110177566999581,-0.848044693589306));
#125274=DIRECTION('ref_axis',(-0.830446875599428,-0.171882402245342,-0.529919264233259));
#125275=DIRECTION('center_axis',(0.518344615107839,0.110177549147491,-0.848044673146738));
#125276=DIRECTION('ref_axis',(-0.853239260760973,3.52957760131147E-15,-0.5215196677941));
#125277=DIRECTION('center_axis',(-0.51834407479893,-0.110177412118683,-0.848045021198563));
#125278=DIRECTION('ref_axis',(0.828609503964271,0.180532167035843,-0.529919264233173));
#125279=DIRECTION('center_axis',(0.518344097776644,0.11017743918535,0.848045003637587));
#125280=DIRECTION('ref_axis',(0.853239582811874,-1.85602097405422E-15,-0.52151914089803));
#125281=DIRECTION('center_axis',(0.207659145615641,-0.978201246800566,0.));
#125282=DIRECTION('ref_axis',(0.978201246800566,0.207659145615641,0.));
#125283=DIRECTION('center_axis',(0.978147600733807,0.207911690817754,0.));
#125284=DIRECTION('ref_axis',(-0.207911690817754,0.978147600733807,0.));
#125285=DIRECTION('center_axis',(-3.07718727278846E-18,2.92774812072065E-17,
-1.));
#125286=DIRECTION('ref_axis',(0.,1.,0.));
#125287=DIRECTION('center_axis',(0.208164222161082,-0.978093889466687,1.13734602532685E-14));
#125288=DIRECTION('ref_axis',(0.978093889466687,0.208164222161082,4.2991390833162E-29));
#125289=DIRECTION('center_axis',(0.978147600733808,0.207911690817747,-1.37739719617122E-16));
#125290=DIRECTION('ref_axis',(-0.207911690817747,0.978147600733808,-1.05212114846847E-30));
#125291=DIRECTION('center_axis',(0.847099893161591,0.180025927304202,-0.500012436349221));
#125292=DIRECTION('ref_axis',(0.488879980351705,0.104926459532324,0.86601778440245));
#125293=DIRECTION('center_axis',(-0.518344615107841,-0.110177549147463,
0.848044673146741));
#125294=DIRECTION('ref_axis',(0.853239260760973,-3.53605500348288E-15,0.5215196677941));
#125295=DIRECTION('center_axis',(-0.489078698392428,-0.103956896852848,
0.866022511471552));
#125296=DIRECTION('ref_axis',(-0.846158656400491,-0.184432991079564,-0.499999999999962));
#125297=DIRECTION('center_axis',(0.489078713616248,0.103956889752265,-0.866022503726382));
#125298=DIRECTION('ref_axis',(-0.870740345484772,1.04734835562025E-15,-0.491743073916714));
#125299=DIRECTION('center_axis',(-0.51834457766095,-0.110177567039741,0.848044693710594));
#125300=DIRECTION('ref_axis',(-0.82856184230912,-0.180750786620166,-0.529919264233249));
#125301=DIRECTION('center_axis',(-0.518344551206586,-0.110177535564814,
0.848044713969321));
#125302=DIRECTION('ref_axis',(0.85323930054104,3.44800433278326E-15,0.521519602711381));
#125303=DIRECTION('center_axis',(0.978147600733807,0.207911690817754,0.));
#125304=DIRECTION('ref_axis',(-0.207911690817754,0.978147600733807,0.));
#125305=DIRECTION('center_axis',(-0.978147600733807,-0.207911690817754,
0.));
#125306=DIRECTION('ref_axis',(0.207911690817754,-0.978147600733807,0.));
#125307=DIRECTION('center_axis',(0.978147600733808,0.207911690817747,-1.37739719617122E-16));
#125308=DIRECTION('ref_axis',(-0.207911690817747,0.978147600733808,-1.05212114846847E-30));
#125309=DIRECTION('center_axis',(0.978147600733807,0.207911690817754,5.34430112114424E-14));
#125310=DIRECTION('ref_axis',(-0.207911690817754,0.978147600733807,1.52655727061559E-28));
#125311=DIRECTION('center_axis',(0.978147600733808,0.207911690817747,-1.37739719617122E-16));
#125312=DIRECTION('ref_axis',(-0.207911690817747,0.978147600733808,-1.05212114846847E-30));
#125313=DIRECTION('center_axis',(-0.847119506978902,-0.180025582247299,
-0.499979330205103));
#125314=DIRECTION('ref_axis',(0.489253749387821,0.103008581353307,-0.866036951219484));
#125315=DIRECTION('center_axis',(0.489078846174003,0.103956917928285,0.866022425483288));
#125316=DIRECTION('ref_axis',(0.870740269393775,-7.78986752012561E-16,-0.491743208652702));
#125317=DIRECTION('center_axis',(0.489078854943167,0.103956919792226,0.86602242030723));
#125318=DIRECTION('ref_axis',(0.207911690809382,-0.978147600735586,4.93043924728801E-12));
#125319=DIRECTION('center_axis',(-0.497265934578102,-0.0522647557774919,
0.866022508721157));
#125320=DIRECTION('ref_axis',(-0.104528463268414,0.994521895368193,-4.54579507199312E-13));
#125321=DIRECTION('center_axis',(-0.861270944309288,-0.0905534316550128,
0.500012436349425));
#125322=DIRECTION('ref_axis',(0.497376550150498,0.0512812291116259,0.86601778440237));
#125323=DIRECTION('center_axis',(0.497265943181925,0.0522647566817413,-0.866022503726311));
#125324=DIRECTION('ref_axis',(-0.867207748104374,-9.26225114799316E-16,
-0.497946504785143));
#125325=DIRECTION('center_axis',(0.994521895368276,0.104528463267629,0.));
#125326=DIRECTION('ref_axis',(-0.104528463267629,0.994521895368276,0.));
#125327=DIRECTION('center_axis',(-0.994521895368275,-0.10452846326764,1.40045497140052E-16));
#125328=DIRECTION('ref_axis',(0.10452846326764,-0.994521895368275,-1.79838028938001E-33));
#125329=DIRECTION('center_axis',(-0.994521895368276,-0.104528463267629,
0.));
#125330=DIRECTION('ref_axis',(0.104528463267629,-0.994521895368276,0.));
#125331=DIRECTION('center_axis',(-0.994521895368275,-0.10452846326764,1.40045497140052E-16));
#125332=DIRECTION('ref_axis',(0.10452846326764,-0.994521895368275,-1.79838028938001E-33));
#125333=DIRECTION('center_axis',(0.994521895368276,0.10452846326763,0.));
#125334=DIRECTION('ref_axis',(-0.10452846326763,0.994521895368276,0.));
#125335=DIRECTION('center_axis',(-0.527021232978627,-0.0553921636609794,
-0.848045003637568));
#125336=DIRECTION('ref_axis',(-0.849349030019368,-1.01561542645059E-15,
0.527831625809934));
#125337=DIRECTION('center_axis',(0.497266077958573,0.0522647708473857,0.866022425483295));
#125338=DIRECTION('ref_axis',(0.867207670398082,3.99694090177787E-16,-0.497946640115919));
#125339=DIRECTION('center_axis',(0.527021207132431,0.0553921392005086,0.848045021297494));
#125340=DIRECTION('ref_axis',(0.843841975852503,0.084358124587104,-0.529919264233232));
#125341=DIRECTION('center_axis',(-0.527021177161347,-0.0553921577943469,
-0.848045038708649));
#125342=DIRECTION('ref_axis',(-0.849349064867519,-4.73002354866103E-16,
0.527831569734769));
#125343=DIRECTION('center_axis',(0.49726609283361,0.0522647618391874,0.866022417485765));
#125344=DIRECTION('ref_axis',(0.861744800189585,0.0859994148015332,-0.500000000000005));
#125345=DIRECTION('center_axis',(0.861289491529721,0.090559820826828,0.499979330205046));
#125346=DIRECTION('ref_axis',(0.497139368682281,0.0532207405865388,-0.866036951219521));
#125347=DIRECTION('center_axis',(0.104287292793425,-0.994547213842469,0.));
#125348=DIRECTION('ref_axis',(0.994547213842469,0.104287292793425,0.));
#125349=DIRECTION('center_axis',(-0.994521895368275,-0.10452846326764,1.40045497140052E-16));
#125350=DIRECTION('ref_axis',(0.10452846326764,-0.994521895368275,-1.79838028938001E-33));
#125351=DIRECTION('center_axis',(0.994521895368276,0.10452846326763,0.));
#125352=DIRECTION('ref_axis',(-0.10452846326763,0.994521895368276,0.));
#125353=DIRECTION('center_axis',(-7.71409749858844E-19,1.47193748793047E-17,
-1.));
#125354=DIRECTION('ref_axis',(0.,1.,0.));
#125355=DIRECTION('center_axis',(0.104769627595152,-0.994496518411992,0.));
#125356=DIRECTION('ref_axis',(0.994496518411992,0.104769627595152,0.));
#125357=DIRECTION('center_axis',(0.527021693999021,0.0553922121161754,-0.848044713969304));
#125358=DIRECTION('ref_axis',(-0.849348742192388,1.01528730975471E-15,-0.527832088960314));
#125359=DIRECTION('center_axis',(0.527021177161445,0.0553921577943106,0.848045038708591));
#125360=DIRECTION('ref_axis',(0.849349064867459,8.87709183645612E-16,-0.527831569734866));
#125361=DIRECTION('center_axis',(0.527021723799587,0.0553922405971153,-0.848044693589284));
#125362=DIRECTION('ref_axis',(-0.843864204095477,-0.0841354767077662,-0.529919264233208));
#125363=DIRECTION('center_axis',(0.527021758969976,0.0553922189448975,-0.848044673146735));
#125364=DIRECTION('ref_axis',(-0.849348701629308,-8.38249277152437E-16,
-0.527832154231445));
#125365=DIRECTION('center_axis',(-0.527021207296642,-0.0553921391525556,
-0.848045021198577));
#125366=DIRECTION('ref_axis',(0.842941044396022,0.092929914812537,-0.529919264233221));
#125367=DIRECTION('center_axis',(0.527021232978636,0.0553921636609804,0.848045003637562));
#125368=DIRECTION('ref_axis',(0.849349030019363,4.17709715649168E-16,-0.527831625809943));
#125369=DIRECTION('center_axis',(0.10427169399366,-0.994548849394384,-1.24894790576994E-14));
#125370=DIRECTION('ref_axis',(0.994548849394384,0.10427169399366,-6.77001402833622E-29));
#125371=DIRECTION('center_axis',(0.994521895368276,0.104528463267629,0.));
#125372=DIRECTION('ref_axis',(-0.104528463267629,0.994521895368276,0.));
#125373=DIRECTION('center_axis',(-7.71409749858844E-19,1.47193748793047E-17,
-1.));
#125374=DIRECTION('ref_axis',(0.,1.,0.));
#125375=DIRECTION('center_axis',(0.104785225574074,-0.99449487505034,0.));
#125376=DIRECTION('ref_axis',(0.994494875050339,0.104785225574074,0.));
#125377=DIRECTION('center_axis',(0.994521895368275,0.10452846326764,-1.40045497140052E-16));
#125378=DIRECTION('ref_axis',(-0.10452846326764,0.994521895368275,1.56623842824886E-30));
#125379=DIRECTION('center_axis',(0.861277224843046,0.0904936763733016,-0.500012436348442));
#125380=DIRECTION('ref_axis',(0.497169646239973,0.0532497883138783,0.866017784402923));
#125381=DIRECTION('center_axis',(-0.527021758969983,-0.0553922189448987,
0.848044673146731));
#125382=DIRECTION('ref_axis',(0.849348701629304,3.53735120591045E-16,0.527832154231453));
#125383=DIRECTION('center_axis',(-0.497265928782812,-0.0522647653419817,
0.866022511471564));
#125384=DIRECTION('ref_axis',(-0.860801807878642,-0.0949749838266845,-0.499999999999982));
#125385=DIRECTION('center_axis',(0.497265943181779,0.0522647566817739,-0.866022503726393));
#125386=DIRECTION('ref_axis',(-0.867207748104458,5.79523975621388E-16,-0.497946504784997));
#125387=DIRECTION('center_axis',(-0.527021723597968,-0.055392240657868,
0.848044693710613));
#125388=DIRECTION('ref_axis',(-0.842916495800633,-0.0931523188209939,-0.529919264233198));
#125389=DIRECTION('center_axis',(-0.527021693999002,-0.0553922121161264,
0.848044713969319));
#125390=DIRECTION('ref_axis',(0.849348742192401,3.31432934842991E-16,0.527832088960293));
#125391=DIRECTION('center_axis',(0.994521895368276,0.104528463267629,1.42777936329238E-15));
#125392=DIRECTION('ref_axis',(-0.104528463267629,0.994521895368276,-1.03141617847887E-30));
#125393=DIRECTION('center_axis',(-0.994521895368276,-0.104528463267628,
0.));
#125394=DIRECTION('ref_axis',(0.104528463267628,-0.994521895368276,0.));
#125395=DIRECTION('center_axis',(0.994521895368275,0.10452846326764,-1.40045497140052E-16));
#125396=DIRECTION('ref_axis',(-0.10452846326764,0.994521895368275,1.56623842824886E-30));
#125397=DIRECTION('center_axis',(0.994521895368276,0.104528463267629,-7.13889681646191E-16));
#125398=DIRECTION('ref_axis',(-0.104528463267629,0.994521895368276,5.15708089239434E-31));
#125399=DIRECTION('center_axis',(0.994521895368275,0.10452846326764,-1.40045497140052E-16));
#125400=DIRECTION('ref_axis',(-0.10452846326764,0.994521895368275,1.56623842824886E-30));
#125401=DIRECTION('center_axis',(-0.861296695145335,-0.0904912830026736,
-0.499979330205014));
#125402=DIRECTION('ref_axis',(0.497340894868559,0.0513033470029239,-0.866036951219542));
#125403=DIRECTION('center_axis',(0.497266077958562,0.0522647708473845,0.866022425483301));
#125404=DIRECTION('ref_axis',(0.867207670398088,1.09710147407178E-15,-0.497946640115907));
#125405=DIRECTION('center_axis',(0.497266086887884,0.052264771785901,0.866022420299486));
#125406=DIRECTION('ref_axis',(0.104528463274216,-0.994521895367584,-3.84644196591536E-12));
#125407=DIRECTION('center_axis',(-1.40816906889909E-16,-7.12377958457618E-15,
1.));
#125408=DIRECTION('ref_axis',(0.,-1.,-7.12427864012715E-15));
#125409=DIRECTION('center_axis',(-1.40816906889909E-16,-7.12377958457618E-15,
1.));
#125410=DIRECTION('ref_axis',(-3.91292818132308E-34,-1.,-7.12377958457618E-15));
#125411=DIRECTION('center_axis',(0.99999996667151,-0.00025818012795372,
1.58266350846276E-16));
#125412=DIRECTION('ref_axis',(-0.00025818012795372,-0.99999996667151,-6.82961998416055E-15));
#125413=DIRECTION('center_axis',(1.4081690688991E-16,6.98296267768627E-15,
-1.));
#125414=DIRECTION('ref_axis',(-1.,4.05186995067197E-12,-1.40816906861616E-16));
#125415=DIRECTION('center_axis',(0.99999996667151,0.000258180127974661,
1.35193873067682E-16));
#125416=DIRECTION('ref_axis',(0.000258180127974661,-0.99999996667151,-6.82961998416055E-15));
#125417=DIRECTION('center_axis',(-1.40816906889909E-16,-7.12377958457618E-15,
1.));
#125418=DIRECTION('ref_axis',(0.,-1.,-7.12252768074091E-15));
#125419=DIRECTION('center_axis',(-1.4081690688991E-16,-6.98296267768627E-15,
1.));
#125420=DIRECTION('ref_axis',(1.,-4.31477076290321E-12,1.40816906859781E-16));
#125421=DIRECTION('center_axis',(0.999999970597889,-0.000242495818320685,
1.45036773284196E-16));
#125422=DIRECTION('ref_axis',(-0.000242495818320685,-0.999999970597889,
-6.82961998416057E-15));
#125423=DIRECTION('center_axis',(1.40816906889909E-16,7.12377958457618E-15,
-1.));
#125424=DIRECTION('ref_axis',(9.00435281891987E-12,-1.,-7.12377958457491E-15));
#125425=DIRECTION('center_axis',(0.999999970597889,0.000242495818341616,
1.7510165406073E-16));
#125426=DIRECTION('ref_axis',(0.000242495818341616,-0.999999970597889,-6.82961998416057E-15));
#125427=DIRECTION('center_axis',(-2.81633813779821E-16,-6.98296267768627E-15,
1.));
#125428=DIRECTION('ref_axis',(-1.,2.13365834995709E-30,-2.77764288392734E-16));
#125429=DIRECTION('center_axis',(-2.81633813779821E-16,-6.98296267768627E-15,
1.));
#125430=DIRECTION('ref_axis',(-1.,2.10523536799201E-30,-2.81633813779821E-16));
#125431=DIRECTION('center_axis',(-0.00025818012796419,-0.99999996667151,
-6.98372952115933E-15));
#125432=DIRECTION('ref_axis',(-0.99999996667151,0.00025818012796419,4.97610099109124E-32));
#125433=DIRECTION('center_axis',(1.4081690688991E-16,6.98296267768627E-15,
-1.));
#125434=DIRECTION('ref_axis',(-1.,3.98880928287326E-12,-1.40816906862057E-16));
#125435=DIRECTION('center_axis',(0.00025818012796419,-0.99999996667151,
-6.98219536875E-15));
#125436=DIRECTION('ref_axis',(-0.99999996667151,-0.00025818012796419,-4.98515713638296E-32));
#125437=DIRECTION('center_axis',(-2.81633813779821E-16,-6.98296267768627E-15,
1.));
#125438=DIRECTION('ref_axis',(-1.,2.00430111041611E-30,-2.82080304187759E-16));
#125439=DIRECTION('center_axis',(-1.4081690688991E-16,-6.98296267768627E-15,
1.));
#125440=DIRECTION('ref_axis',(1.,-1.19598452005484E-30,1.4081690688991E-16));
#125441=DIRECTION('center_axis',(-0.000242495818331158,-0.999999970597889,
-6.98296247237242E-15));
#125442=DIRECTION('ref_axis',(-0.999999970597889,0.000242495818331158,5.20911529687998E-32));
#125443=DIRECTION('center_axis',(2.81633813779821E-16,6.98296267768627E-15,
-1.));
#125444=DIRECTION('ref_axis',(-1.,9.2414964569798E-12,-2.81633813715288E-16));
#125445=DIRECTION('center_axis',(0.00024249581833115,-0.999999970597889,
-6.96962337123306E-15));
#125446=DIRECTION('ref_axis',(-0.999999970597889,-0.00024249581833115,-9.17267951536334E-32));
#125447=DIRECTION('center_axis',(-1.4081690688991E-16,-6.98296267768627E-15,
1.));
#125448=DIRECTION('ref_axis',(1.,-1.19598452005484E-30,1.4081690688991E-16));
#125449=DIRECTION('center_axis',(-1.4081690688991E-16,-6.98296267768627E-15,
1.));
#125450=DIRECTION('ref_axis',(-1.,8.57836796235549E-31,-1.35821020636094E-16));
#125451=DIRECTION('center_axis',(-1.4081690688991E-16,-6.98296267768627E-15,
1.));
#125452=DIRECTION('ref_axis',(-1.,8.41864228189078E-31,-1.4081690688991E-16));
#125453=DIRECTION('center_axis',(-1.22464679914736E-16,1.,6.98296267768627E-15));
#125454=DIRECTION('ref_axis',(1.,1.22464679914735E-16,1.41480229829265E-16));
#125455=DIRECTION('center_axis',(1.4081690688991E-16,6.98296267768627E-15,
-1.));
#125456=DIRECTION('ref_axis',(-1.,8.40543590285906E-31,-1.4081690688991E-16));
#125457=DIRECTION('center_axis',(1.4081690688991E-16,6.98296267768627E-15,
-1.));
#125458=DIRECTION('ref_axis',(-1.,8.40543590285906E-31,-1.4081690688991E-16));
#125459=DIRECTION('center_axis',(-1.4081690688991E-16,-6.98296267768627E-15,
1.));
#125460=DIRECTION('ref_axis',(-1.,8.5653263190156E-31,-1.3561453272173E-16));
#125461=DIRECTION('center_axis',(-1.4081690688991E-16,-6.98296267768627E-15,
1.));
#125462=DIRECTION('ref_axis',(1.,-8.43374090490393E-31,1.4081690688991E-16));
#125463=DIRECTION('center_axis',(-1.22464679914736E-16,1.,6.98296267768627E-15));
#125464=DIRECTION('ref_axis',(1.,1.22464679914735E-16,1.41265138251802E-16));
#125465=DIRECTION('center_axis',(1.4081690688991E-16,6.98296267768627E-15,
-1.));
#125466=DIRECTION('ref_axis',(-1.,8.42081623376257E-31,-1.40816906889911E-16));
#125467=DIRECTION('center_axis',(-1.4081690688991E-16,-6.98296267768627E-15,
1.));
#125468=DIRECTION('ref_axis',(-1.,1.17957896342593E-30,-1.38342483857788E-16));
#125469=DIRECTION('center_axis',(-1.4081690688991E-16,-6.98296267768627E-15,
1.));
#125470=DIRECTION('ref_axis',(-1.,1.14629496755776E-30,-1.4081690688991E-16));
#125471=DIRECTION('center_axis',(-1.22464679914735E-16,1.,6.98296267768627E-15));
#125472=DIRECTION('ref_axis',(1.,1.22464679914734E-16,1.38342483857788E-16));
#125473=DIRECTION('center_axis',(1.4081690688991E-16,6.98296267768627E-15,
-1.));
#125474=DIRECTION('ref_axis',(-1.,1.19573562666198E-30,-1.40816906889911E-16));
#125475=DIRECTION('center_axis',(1.4081690688991E-16,6.98296267768627E-15,
-1.));
#125476=DIRECTION('ref_axis',(-1.,1.19573562666198E-30,-1.40816906889911E-16));
#125477=DIRECTION('center_axis',(-1.4081690688991E-16,-6.98296267768627E-15,
1.));
#125478=DIRECTION('ref_axis',(-1.,1.17793481601532E-30,-1.38149656210243E-16));
#125479=DIRECTION('center_axis',(-1.4081690688991E-16,-6.98296267768627E-15,
1.));
#125480=DIRECTION('ref_axis',(1.,-1.14470030428736E-30,1.4081690688991E-16));
#125481=DIRECTION('center_axis',(-1.22464679914735E-16,1.,6.98296267768627E-15));
#125482=DIRECTION('ref_axis',(1.,1.22464679914734E-16,1.38149656210243E-16));
#125483=DIRECTION('center_axis',(1.4081690688991E-16,6.98296267768627E-15,
-1.));
#125484=DIRECTION('ref_axis',(-1.,1.14606553893984E-30,-1.40816906889911E-16));
#125485=DIRECTION('center_axis',(-1.4081690688991E-16,-6.98296267768627E-15,
1.));
#125486=DIRECTION('ref_axis',(-1.,1.1860226061992E-30,-1.4081690688991E-16));
#125487=DIRECTION('center_axis',(-1.4081690688991E-16,-6.98296267768627E-15,
1.));
#125488=DIRECTION('ref_axis',(-1.,1.09611010944228E-30,-1.4081690688991E-16));
#125489=DIRECTION('',(1.4081690688991E-16,6.98296267768627E-15,-1.));
#125490=DIRECTION('center_axis',(-1.4081690688991E-16,-6.98296267768627E-15,
1.));
#125491=DIRECTION('ref_axis',(-1.,1.14270052978402E-30,-1.4081690688991E-16));
#125492=DIRECTION('center_axis',(-1.4081690688991E-16,-6.98296267768627E-15,
1.));
#125493=DIRECTION('ref_axis',(-1.,1.14517058122326E-30,-1.4081690688991E-16));
#125494=DIRECTION('',(-0.529919264233199,5.85699181126827E-15,-0.84804809615643));
#125495=DIRECTION('center_axis',(1.4081690688991E-16,6.98296267768627E-15,
-1.));
#125496=DIRECTION('ref_axis',(1.,-8.0229549381324E-31,1.4081690688991E-16));
#125497=DIRECTION('center_axis',(-1.4081690688991E-16,-6.98296267768627E-15,
1.));
#125498=DIRECTION('ref_axis',(1.,-1.19598452005484E-30,1.4081690688991E-16));
#125499=DIRECTION('',(-0.529924202082878,4.64200439806007E-6,0.848045010612807));
#125500=DIRECTION('center_axis',(-1.4081690688991E-16,-6.98296267768627E-15,
1.));
#125501=DIRECTION('ref_axis',(1.,-8.02836526847902E-31,1.4081690688991E-16));
#125502=DIRECTION('',(0.527020736635427,0.0553967790670863,-0.848045010612788));
#125503=DIRECTION('center_axis',(-1.4081690688991E-16,-6.98296267768627E-15,
1.));
#125504=DIRECTION('ref_axis',(1.,-6.21724893790088E-15,1.40816906889867E-16));
#125505=DIRECTION('',(-0.527021707078575,-0.055387545917055,0.848045010612804));
#125506=DIRECTION('center_axis',(-1.4081690688991E-16,-6.98296267768627E-15,
1.));
#125507=DIRECTION('ref_axis',(1.,-8.02836526847902E-31,1.4081690688991E-16));
#125508=DIRECTION('',(0.518343121711171,0.110181977425787,-0.848045010612799));
#125509=DIRECTION('center_axis',(-1.4081690688991E-16,-6.98296267768627E-15,
1.));
#125510=DIRECTION('ref_axis',(1.,-1.24344978758018E-14,1.40816906889824E-16));
#125511=DIRECTION('',(-0.518345051965149,-0.110172896294845,0.848045010612793));
#125512=DIRECTION('center_axis',(-1.4081690688991E-16,-6.98296267768627E-15,
1.));
#125513=DIRECTION('ref_axis',(1.,-8.02836526847902E-31,1.4081690688991E-16));
#125514=DIRECTION('',(0.503986431075191,0.16375999898274,-0.8480450106128));
#125515=DIRECTION('center_axis',(-1.4081690688991E-16,-6.98296267768627E-15,
1.));
#125516=DIRECTION('ref_axis',(1.,-1.19598452005484E-30,1.4081690688991E-16));
#125517=DIRECTION('',(-0.503989299991689,-0.163751169365674,0.848045010612798));
#125518=DIRECTION('center_axis',(-1.4081690688991E-16,-6.98296267768627E-15,
1.));
#125519=DIRECTION('ref_axis',(1.,-8.02836526847902E-31,1.4081690688991E-16));
#125520=DIRECTION('',(0.484107959634417,0.215543831721869,-0.848045010612795));
#125521=DIRECTION('center_axis',(-1.4081690688991E-16,-6.98296267768627E-15,
1.));
#125522=DIRECTION('ref_axis',(1.,-4.79616346638068E-14,1.40816906889576E-16));
#125523=DIRECTION('',(-0.484111735780992,-0.215535350357788,0.848045010612797));
#125524=DIRECTION('center_axis',(-1.4081690688991E-16,-6.98296267768627E-15,
1.));
#125525=DIRECTION('ref_axis',(1.,-8.88178419700127E-16,1.40816906889904E-16));
#125526=DIRECTION('',(0.458925500081787,0.264966121135203,-0.848045010612789));
#125527=DIRECTION('center_axis',(-1.4081690688991E-16,-6.98296267768627E-15,
1.));
#125528=DIRECTION('ref_axis',(1.,-1.19598452005484E-30,1.4081690688991E-16));
#125529=DIRECTION('',(-0.458930142086182,-0.264958080947721,0.848045010612796));
#125530=DIRECTION('center_axis',(-1.4081690688991E-16,-6.98296267768627E-15,
1.));
#125531=DIRECTION('ref_axis',(1.,-8.88178419700127E-16,1.40816906889904E-16));
#125532=DIRECTION('',(0.428714956713912,0.31148538627764,-0.848045010612796));
#125533=DIRECTION('center_axis',(-1.4081690688991E-16,-6.98296267768627E-15,
1.));
#125534=DIRECTION('ref_axis',(1.,-1.19598452005484E-30,1.4081690688991E-16));
#125535=DIRECTION('',(-0.428720413717374,-0.311477875356759,0.848045010612788));
#125536=DIRECTION('center_axis',(-1.4081690688991E-16,-6.98296267768627E-15,
1.));
#125537=DIRECTION('ref_axis',(1.,-8.88178419700127E-16,1.40816906889904E-16));
#125538=DIRECTION('',(0.393807322565913,0.354591952345519,-0.848045010612797));
#125539=DIRECTION('center_axis',(-1.4081690688991E-16,-6.98296267768627E-15,
1.));
#125540=DIRECTION('ref_axis',(1.,-1.19598452005484E-30,1.4081690688991E-16));
#125541=DIRECTION('',(-0.393813534780367,-0.354585052982427,0.848045010612787));
#125542=DIRECTION('center_axis',(-1.4081690688991E-16,-6.98296267768627E-15,
1.));
#125543=DIRECTION('ref_axis',(1.,-8.88178419700127E-16,1.40816906889904E-16));
#125544=DIRECTION('',(0.354585052982402,0.393813534780382,-0.848045010612791));
#125545=DIRECTION('center_axis',(-1.4081690688991E-16,-6.98296267768627E-15,
1.));
#125546=DIRECTION('ref_axis',(1.,-1.19598452005484E-30,1.4081690688991E-16));
#125547=DIRECTION('',(-0.354591952345514,-0.393807322565934,0.84804501061279));
#125548=DIRECTION('center_axis',(-1.4081690688991E-16,-6.98296267768627E-15,
1.));
#125549=DIRECTION('ref_axis',(1.,-8.88178419700127E-16,1.40816906889904E-16));
#125550=DIRECTION('',(0.311477875356731,0.428720413717367,-0.848045010612801));
#125551=DIRECTION('center_axis',(-1.4081690688991E-16,-6.98296267768627E-15,
1.));
#125552=DIRECTION('ref_axis',(1.,-1.19598452005484E-30,1.4081690688991E-16));
#125553=DIRECTION('',(-0.311485386277638,-0.428714956713914,0.848045010612796));
#125554=DIRECTION('center_axis',(-1.4081690688991E-16,-6.98296267768627E-15,
1.));
#125555=DIRECTION('ref_axis',(1.,-8.02836526847902E-31,1.4081690688991E-16));
#125556=DIRECTION('',(0.264958080947702,0.458930142086184,-0.848045010612801));
#125557=DIRECTION('center_axis',(-1.4081690688991E-16,-6.98296267768627E-15,
1.));
#125558=DIRECTION('ref_axis',(1.,-1.19598452005484E-30,1.4081690688991E-16));
#125559=DIRECTION('',(-0.26496612113518,-0.458925500081782,0.8480450106128));
#125560=DIRECTION('center_axis',(-1.4081690688991E-16,-6.98296267768627E-15,
1.));
#125561=DIRECTION('ref_axis',(1.,-8.02836526847902E-31,1.4081690688991E-16));
#125562=DIRECTION('',(0.215535350357773,0.484111735781,-0.848045010612798));
#125563=DIRECTION('center_axis',(-1.4081690688991E-16,-6.98296267768627E-15,
1.));
#125564=DIRECTION('ref_axis',(1.,-1.19598452005484E-30,1.4081690688991E-16));
#125565=DIRECTION('',(-0.215543831721857,-0.484107959634406,0.848045010612805));
#125566=DIRECTION('center_axis',(-1.4081690688991E-16,-6.98296267768627E-15,
1.));
#125567=DIRECTION('ref_axis',(1.,-8.02836526847902E-31,1.4081690688991E-16));
#125568=DIRECTION('',(0.163751169365655,0.503989299991706,-0.848045010612792));
#125569=DIRECTION('center_axis',(-1.4081690688991E-16,-6.98296267768627E-15,
1.));
#125570=DIRECTION('ref_axis',(1.,-1.19598452005484E-30,1.4081690688991E-16));
#125571=DIRECTION('',(-0.163759998982739,-0.5039864310752,0.848045010612796));
#125572=DIRECTION('center_axis',(-1.4081690688991E-16,-6.98296267768627E-15,
1.));
#125573=DIRECTION('ref_axis',(1.,-8.02836526847902E-31,1.4081690688991E-16));
#125574=DIRECTION('',(0.110172896294836,0.518345051965155,-0.848045010612791));
#125575=DIRECTION('center_axis',(-1.4081690688991E-16,-6.98296267768627E-15,
1.));
#125576=DIRECTION('ref_axis',(1.,-1.19598452005484E-30,1.4081690688991E-16));
#125577=DIRECTION('',(-0.110181977425776,-0.518343121711191,0.848045010612788));
#125578=DIRECTION('center_axis',(-1.4081690688991E-16,-6.98296267768627E-15,
1.));
#125579=DIRECTION('ref_axis',(1.,-8.02836526847902E-31,1.4081690688991E-16));
#125580=DIRECTION('',(0.0553875459170424,0.527021707078595,-0.848045010612793));
#125581=DIRECTION('center_axis',(-1.4081690688991E-16,-6.98296267768627E-15,
1.));
#125582=DIRECTION('ref_axis',(1.,-1.19598452005484E-30,1.4081690688991E-16));
#125583=DIRECTION('',(-0.0553967790670788,-0.527020736635434,0.848045010612784));
#125584=DIRECTION('center_axis',(-1.4081690688991E-16,-6.98296267768627E-15,
1.));
#125585=DIRECTION('ref_axis',(1.,-8.02836526847902E-31,1.4081690688991E-16));
#125586=DIRECTION('',(-4.64200440569701E-6,0.529924202082914,-0.848045010612785));
#125587=DIRECTION('center_axis',(-1.4081690688991E-16,-6.98296267768627E-15,
1.));
#125588=DIRECTION('ref_axis',(1.,-1.19598452005484E-30,1.4081690688991E-16));
#125589=DIRECTION('',(-4.64200440229132E-6,-0.529924202082886,0.848045010612803));
#125590=DIRECTION('center_axis',(-1.4081690688991E-16,-6.98296267768627E-15,
1.));
#125591=DIRECTION('ref_axis',(1.,-8.02836526847902E-31,1.4081690688991E-16));
#125592=DIRECTION('',(-0.0553967790670825,0.527020736635425,-0.84804501061279));
#125593=DIRECTION('center_axis',(-1.4081690688991E-16,-6.98296267768627E-15,
1.));
#125594=DIRECTION('ref_axis',(1.,-1.19598452005484E-30,1.4081690688991E-16));
#125595=DIRECTION('',(0.0553875459170465,-0.527021707078599,0.848045010612789));
#125596=DIRECTION('center_axis',(-1.4081690688991E-16,-6.98296267768627E-15,
1.));
#125597=DIRECTION('ref_axis',(1.,-8.02836526847902E-31,1.4081690688991E-16));
#125598=DIRECTION('',(-0.110181977425775,0.518343121711176,-0.848045010612797));
#125599=DIRECTION('center_axis',(-1.4081690688991E-16,-6.98296267768627E-15,
1.));
#125600=DIRECTION('ref_axis',(1.,-1.19598452005484E-30,1.4081690688991E-16));
#125601=DIRECTION('',(0.110172896294839,-0.51834505196514,0.848045010612799));
#125602=DIRECTION('center_axis',(-1.4081690688991E-16,-6.98296267768627E-15,
1.));
#125603=DIRECTION('ref_axis',(1.,-8.02836526847902E-31,1.4081690688991E-16));
#125604=DIRECTION('',(-0.163759998982728,0.50398643107521,-0.848045010612791));
#125605=DIRECTION('center_axis',(-1.4081690688991E-16,-6.98296267768627E-15,
1.));
#125606=DIRECTION('ref_axis',(1.,-1.19598452005484E-30,1.4081690688991E-16));
#125607=DIRECTION('',(0.163751169365666,-0.503989299991696,0.848045010612796));
#125608=DIRECTION('center_axis',(-1.4081690688991E-16,-6.98296267768627E-15,
1.));
#125609=DIRECTION('ref_axis',(1.,-8.02836526847902E-31,1.4081690688991E-16));
#125610=DIRECTION('',(-0.215543831721853,0.484107959634437,-0.848045010612788));
#125611=DIRECTION('center_axis',(-1.4081690688991E-16,-6.98296267768627E-15,
1.));
#125612=DIRECTION('ref_axis',(1.,-1.19598452005484E-30,1.4081690688991E-16));
#125613=DIRECTION('',(0.215535350357773,-0.484111735781,0.848045010612798));
#125614=DIRECTION('center_axis',(-1.4081690688991E-16,-6.98296267768627E-15,
1.));
#125615=DIRECTION('ref_axis',(1.,4.44089209850063E-15,1.40816906889941E-16));
#125616=DIRECTION('',(-0.264966121135185,0.45892550008179,-0.848045010612794));
#125617=DIRECTION('center_axis',(-1.4081690688991E-16,-6.98296267768627E-15,
1.));
#125618=DIRECTION('ref_axis',(1.,-1.19598452005484E-30,1.4081690688991E-16));
#125619=DIRECTION('',(0.264958080947719,-0.458930142086191,0.848045010612792));
#125620=DIRECTION('center_axis',(-1.4081690688991E-16,-6.98296267768627E-15,
1.));
#125621=DIRECTION('ref_axis',(1.,-8.02836526847902E-31,1.4081690688991E-16));
#125622=DIRECTION('',(-0.31148538627764,0.428714956713912,-0.848045010612796));
#125623=DIRECTION('center_axis',(-1.4081690688991E-16,-6.98296267768627E-15,
1.));
#125624=DIRECTION('ref_axis',(1.,-2.01438865587988E-12,1.40816906875844E-16));
#125625=DIRECTION('',(0.31147787535674,-0.428720413717385,0.848045010612789));
#125626=DIRECTION('center_axis',(-1.4081690688991E-16,-6.98296267768627E-15,
1.));
#125627=DIRECTION('ref_axis',(1.,-8.02836526847902E-31,1.4081690688991E-16));
#125628=DIRECTION('',(-0.354591952345504,0.393807322565925,-0.848045010612798));
#125629=DIRECTION('center_axis',(-1.4081690688991E-16,-6.98296267768627E-15,
1.));
#125630=DIRECTION('ref_axis',(1.,-1.19598452005484E-30,1.4081690688991E-16));
#125631=DIRECTION('',(0.354585052982402,-0.393813534780382,0.848045010612791));
#125632=DIRECTION('center_axis',(-1.4081690688991E-16,-6.98296267768627E-15,
1.));
#125633=DIRECTION('ref_axis',(1.,-8.02836526847902E-31,1.4081690688991E-16));
#125634=DIRECTION('',(-0.393813534780341,0.354585052982428,-0.848045010612799));
#125635=DIRECTION('center_axis',(-1.4081690688991E-16,-6.98296267768627E-15,
1.));
#125636=DIRECTION('ref_axis',(1.,2.20534701611541E-12,1.4081690690531E-16));
#125637=DIRECTION('',(0.393807322565921,-0.354591952345514,0.848045010612796));
#125638=DIRECTION('center_axis',(-1.4081690688991E-16,-6.98296267768627E-15,
1.));
#125639=DIRECTION('ref_axis',(1.,-1.24344978758018E-14,1.40816906889824E-16));
#125640=DIRECTION('',(-0.428720413717363,0.311477875356744,-0.848045010612799));
#125641=DIRECTION('center_axis',(-1.4081690688991E-16,-6.98296267768627E-15,
1.));
#125642=DIRECTION('ref_axis',(1.,-1.19598452005484E-30,1.4081690688991E-16));
#125643=DIRECTION('',(0.428714956713901,-0.311485386277647,0.848045010612799));
#125644=DIRECTION('center_axis',(-1.4081690688991E-16,-6.98296267768627E-15,
1.));
#125645=DIRECTION('ref_axis',(1.,-8.02836526847902E-31,1.4081690688991E-16));
#125646=DIRECTION('',(-0.458930142086183,0.264958080947715,-0.848045010612797));
#125647=DIRECTION('center_axis',(-1.4081690688991E-16,-6.98296267768627E-15,
1.));
#125648=DIRECTION('ref_axis',(1.,-1.19598452005484E-30,1.4081690688991E-16));
#125649=DIRECTION('',(0.458925500081769,-0.264966121135201,0.8480450106128));
#125650=DIRECTION('center_axis',(-1.4081690688991E-16,-6.98296267768627E-15,
1.));
#125651=DIRECTION('ref_axis',(1.,-8.02836526847902E-31,1.4081690688991E-16));
#125652=DIRECTION('',(-0.484111735781003,0.215535350357781,-0.848045010612793));
#125653=DIRECTION('center_axis',(-1.4081690688991E-16,-6.98296267768627E-15,
1.));
#125654=DIRECTION('ref_axis',(1.,-1.19598452005484E-30,1.4081690688991E-16));
#125655=DIRECTION('',(0.4841079596344,-0.215543831721854,0.848045010612809));
#125656=DIRECTION('center_axis',(-1.4081690688991E-16,-6.98296267768627E-15,
1.));
#125657=DIRECTION('ref_axis',(1.,-8.02836526847902E-31,1.4081690688991E-16));
#125658=DIRECTION('',(-0.5039892999917,0.163751169365664,-0.848045010612794));
#125659=DIRECTION('center_axis',(-1.4081690688991E-16,-6.98296267768627E-15,
1.));
#125660=DIRECTION('ref_axis',(1.,-1.19598452005484E-30,1.4081690688991E-16));
#125661=DIRECTION('',(0.503986431075195,-0.163759998982748,0.848045010612796));
#125662=DIRECTION('center_axis',(-1.4081690688991E-16,-6.98296267768627E-15,
1.));
#125663=DIRECTION('ref_axis',(1.,-8.02836526847902E-31,1.4081690688991E-16));
#125664=DIRECTION('',(-0.518345051965131,0.11017289629484,-0.848045010612805));
#125665=DIRECTION('center_axis',(-1.4081690688991E-16,-6.98296267768627E-15,
1.));
#125666=DIRECTION('ref_axis',(1.,-1.19598452005484E-30,1.4081690688991E-16));
#125667=DIRECTION('',(0.518343121711172,-0.110181977425781,0.848045010612799));
#125668=DIRECTION('center_axis',(-1.4081690688991E-16,-6.98296267768627E-15,
1.));
#125669=DIRECTION('ref_axis',(1.,-8.02836526847902E-31,1.4081690688991E-16));
#125670=DIRECTION('',(-0.527021707078581,0.0553875459170459,-0.848045010612801));
#125671=DIRECTION('center_axis',(-1.4081690688991E-16,-6.98296267768627E-15,
1.));
#125672=DIRECTION('ref_axis',(1.,-1.19598452005484E-30,1.4081690688991E-16));
#125673=DIRECTION('',(0.527020736635404,-0.0553967790670833,0.848045010612803));
#125674=DIRECTION('center_axis',(-1.4081690688991E-16,-6.98296267768627E-15,
1.));
#125675=DIRECTION('ref_axis',(1.,-8.02836526847902E-31,1.4081690688991E-16));
#125676=DIRECTION('',(-0.529924202082893,-4.64200439816316E-6,-0.848045010612798));
#125677=DIRECTION('',(-0.529919264233196,5.98678459741823E-15,-0.848048096156432));
#125678=DIRECTION('',(0.529924202082893,-4.64200440982505E-6,0.848045010612798));
#125679=DIRECTION('center_axis',(-1.4081690688991E-16,-6.98296267768627E-15,
1.));
#125680=DIRECTION('ref_axis',(1.,-8.02836526847902E-31,1.4081690688991E-16));
#125681=DIRECTION('',(-0.527020736635413,-0.0553967790670796,-0.848045010612797));
#125682=DIRECTION('center_axis',(-1.4081690688991E-16,-6.98296267768627E-15,
1.));
#125683=DIRECTION('ref_axis',(1.,-1.19598452005484E-30,1.4081690688991E-16));
#125684=DIRECTION('',(0.527021707078571,0.0553875459170413,0.848045010612807));
#125685=DIRECTION('center_axis',(-1.4081690688991E-16,-6.98296267768627E-15,
1.));
#125686=DIRECTION('ref_axis',(1.,-8.02836526847902E-31,1.4081690688991E-16));
#125687=DIRECTION('',(-0.518343121711153,-0.110181977425773,-0.848045010612811));
#125688=DIRECTION('center_axis',(-1.4081690688991E-16,-6.98296267768627E-15,
1.));
#125689=DIRECTION('ref_axis',(1.,-1.19598452005484E-30,1.4081690688991E-16));
#125690=DIRECTION('',(0.518345051965141,0.110172896294833,0.848045010612799));
#125691=DIRECTION('center_axis',(-1.4081690688991E-16,-6.98296267768627E-15,
1.));
#125692=DIRECTION('ref_axis',(1.,-8.02836526847902E-31,1.4081690688991E-16));
#125693=DIRECTION('',(-0.503986431075192,-0.163759998982734,-0.848045010612801));
#125694=DIRECTION('center_axis',(-1.4081690688991E-16,-6.98296267768627E-15,
1.));
#125695=DIRECTION('ref_axis',(1.,-1.19598452005484E-30,1.4081690688991E-16));
#125696=DIRECTION('',(0.503989299991687,0.163751169365657,0.848045010612803));
#125697=DIRECTION('center_axis',(-1.4081690688991E-16,-6.98296267768627E-15,
1.));
#125698=DIRECTION('ref_axis',(1.,-8.02836526847902E-31,1.4081690688991E-16));
#125699=DIRECTION('',(-0.484107959634419,-0.21554383172185,-0.848045010612799));
#125700=DIRECTION('center_axis',(-1.4081690688991E-16,-6.98296267768627E-15,
1.));
#125701=DIRECTION('ref_axis',(1.,-1.19598452005484E-30,1.4081690688991E-16));
#125702=DIRECTION('',(0.484111735780995,0.21553535035777,0.848045010612801));
#125703=DIRECTION('center_axis',(-1.4081690688991E-16,-6.98296267768627E-15,
1.));
#125704=DIRECTION('ref_axis',(1.,-8.02836526847902E-31,1.4081690688991E-16));
#125705=DIRECTION('',(-0.458925500081788,-0.264966121135171,-0.8480450106128));
#125706=DIRECTION('center_axis',(-1.4081690688991E-16,-6.98296267768627E-15,
1.));
#125707=DIRECTION('ref_axis',(1.,-1.19598452005484E-30,1.4081690688991E-16));
#125708=DIRECTION('',(0.45893014208618,0.264958080947707,0.848045010612802));
#125709=DIRECTION('center_axis',(-1.4081690688991E-16,-6.98296267768627E-15,
1.));
#125710=DIRECTION('ref_axis',(1.,-8.02836526847902E-31,1.4081690688991E-16));
#125711=DIRECTION('',(-0.428714956713899,-0.311485386277633,-0.848045010612806));
#125712=DIRECTION('center_axis',(-1.4081690688991E-16,-6.98296267768627E-15,
1.));
#125713=DIRECTION('ref_axis',(1.,-1.19598452005484E-30,1.4081690688991E-16));
#125714=DIRECTION('',(0.42872041371736,0.311477875356735,0.848045010612803));
#125715=DIRECTION('center_axis',(-1.4081690688991E-16,-6.98296267768627E-15,
1.));
#125716=DIRECTION('ref_axis',(1.,-8.02836526847902E-31,1.4081690688991E-16));
#125717=DIRECTION('',(-0.393807322565921,-0.354591952345514,-0.848045010612796));
#125718=DIRECTION('center_axis',(-1.4081690688991E-16,-6.98296267768627E-15,
1.));
#125719=DIRECTION('ref_axis',(1.,-1.19598452005484E-30,1.4081690688991E-16));
#125720=DIRECTION('',(0.393813534780356,0.354585052982402,0.848045010612803));
#125721=DIRECTION('center_axis',(-1.4081690688991E-16,-6.98296267768627E-15,
1.));
#125722=DIRECTION('ref_axis',(1.,-8.02836526847902E-31,1.4081690688991E-16));
#125723=DIRECTION('',(-0.354585052982407,-0.393813534780348,-0.848045010612804));
#125724=DIRECTION('center_axis',(-1.4081690688991E-16,-6.98296267768627E-15,
1.));
#125725=DIRECTION('ref_axis',(1.,-1.19598452005484E-30,1.4081690688991E-16));
#125726=DIRECTION('',(0.354591952345508,0.393807322565902,0.848045010612807));
#125727=DIRECTION('center_axis',(-1.4081690688991E-16,-6.98296267768627E-15,
1.));
#125728=DIRECTION('ref_axis',(1.,-8.02836526847902E-31,1.4081690688991E-16));
#125729=DIRECTION('',(-0.311477875356729,-0.428720413717378,-0.848045010612797));
#125730=DIRECTION('center_axis',(-1.4081690688991E-16,-6.98296267768627E-15,
1.));
#125731=DIRECTION('ref_axis',(1.,-7.47846229387506E-12,1.40816906837689E-16));
#125732=DIRECTION('',(0.311485386277628,0.428714956713906,0.848045010612804));
#125733=DIRECTION('center_axis',(-1.4081690688991E-16,-6.98296267768627E-15,
1.));
#125734=DIRECTION('ref_axis',(1.,1.95399252334028E-14,1.40816906890047E-16));
#125735=DIRECTION('',(-0.264958080947707,-0.458930142086193,-0.848045010612795));
#125736=DIRECTION('center_axis',(-1.4081690688991E-16,-6.98296267768627E-15,
1.));
#125737=DIRECTION('ref_axis',(1.,-7.67208518936968E-12,1.40816906836337E-16));
#125738=DIRECTION('',(0.264966121135178,0.458925500081776,0.848045010612803));
#125739=DIRECTION('center_axis',(-1.4081690688991E-16,-6.98296267768627E-15,
1.));
#125740=DIRECTION('ref_axis',(1.,3.01980662698043E-14,1.40816906890121E-16));
#125741=DIRECTION('',(-0.215535350357775,-0.484111735780979,-0.848045010612808));
#125742=DIRECTION('center_axis',(-1.4081690688991E-16,-6.98296267768627E-15,
1.));
#125743=DIRECTION('ref_axis',(1.,5.89750470680883E-12,1.40816906931093E-16));
#125744=DIRECTION('',(0.21554383172186,0.484107959634412,0.848045010612801));
#125745=DIRECTION('center_axis',(-1.4081690688991E-16,-6.98296267768627E-15,
1.));
#125746=DIRECTION('ref_axis',(1.,-8.02836526847902E-31,1.4081690688991E-16));
#125747=DIRECTION('',(-0.163751169365654,-0.503989299991677,-0.848045010612809));
#125748=DIRECTION('center_axis',(-1.4081690688991E-16,-6.98296267768627E-15,
1.));
#125749=DIRECTION('ref_axis',(1.,6.04050143238055E-12,1.40816906932091E-16));
#125750=DIRECTION('',(0.163759998982731,0.503986431075181,0.848045010612808));
#125751=DIRECTION('center_axis',(-1.4081690688991E-16,-6.98296267768627E-15,
1.));
#125752=DIRECTION('ref_axis',(1.,-2.1316282072803E-14,1.40816906889762E-16));
#125753=DIRECTION('',(-0.110172896294832,-0.51834505196514,-0.8480450106128));
#125754=DIRECTION('center_axis',(-1.4081690688991E-16,-6.98296267768627E-15,
1.));
#125755=DIRECTION('ref_axis',(1.,6.18438633637197E-12,1.40816906933096E-16));
#125756=DIRECTION('',(0.11018197742577,0.518343121711167,0.848045010612803));
#125757=DIRECTION('center_axis',(-1.4081690688991E-16,-6.98296267768627E-15,
1.));
#125758=DIRECTION('ref_axis',(1.,-8.02836526847902E-31,1.4081690688991E-16));
#125759=DIRECTION('',(-0.0553875459170386,-0.52702170707859,-0.848045010612796));
#125760=DIRECTION('center_axis',(-1.4081690688991E-16,-6.98296267768627E-15,
1.));
#125761=DIRECTION('ref_axis',(1.,-2.1094237467878E-12,1.4081690687518E-16));
#125762=DIRECTION('',(0.0553967790670769,0.527020736635406,0.848045010612802));
#125763=DIRECTION('center_axis',(-1.4081690688991E-16,-6.98296267768627E-15,
1.));
#125764=DIRECTION('ref_axis',(1.,-8.02836526847902E-31,1.4081690688991E-16));
#125765=DIRECTION('',(4.64200440982511E-6,-0.5299242020829,-0.848045010612794));
#125766=DIRECTION('',(4.64200439836955E-6,0.52992420208289,0.8480450106128));
#125767=DIRECTION('center_axis',(-1.4081690688991E-16,-6.98296267768627E-15,
1.));
#125768=DIRECTION('ref_axis',(1.,3.37507799486048E-14,1.40816906890146E-16));
#125769=DIRECTION('',(0.0553967790670857,-0.527020736635411,-0.848045010612798));
#125770=DIRECTION('center_axis',(-1.4081690688991E-16,-6.98296267768627E-15,
1.));
#125771=DIRECTION('ref_axis',(1.,-1.19598452005484E-30,1.4081690688991E-16));
#125772=DIRECTION('',(-0.0553875459170506,0.52702170707858,0.848045010612801));
#125773=DIRECTION('center_axis',(-1.4081690688991E-16,-6.98296267768627E-15,
1.));
#125774=DIRECTION('ref_axis',(1.,-1.06581410364015E-14,1.40816906889836E-16));
#125775=DIRECTION('',(0.110181977425778,-0.518343121711171,-0.848045010612799));
#125776=DIRECTION('center_axis',(-1.4081690688991E-16,-6.98296267768627E-15,
1.));
#125777=DIRECTION('ref_axis',(1.,-1.19598452005484E-30,1.4081690688991E-16));
#125778=DIRECTION('',(-0.110172896294836,0.518345051965145,0.848045010612797));
#125779=DIRECTION('center_axis',(-1.4081690688991E-16,-6.98296267768627E-15,
1.));
#125780=DIRECTION('ref_axis',(1.,-1.24344978758018E-14,1.40816906889824E-16));
#125781=DIRECTION('',(0.163759998982748,-0.503986431075193,-0.848045010612797));
#125782=DIRECTION('center_axis',(-1.4081690688991E-16,-6.98296267768627E-15,
1.));
#125783=DIRECTION('ref_axis',(1.,-1.19598452005484E-30,1.4081690688991E-16));
#125784=DIRECTION('',(-0.163751169365665,0.503989299991695,0.848045010612797));
#125785=DIRECTION('center_axis',(-1.4081690688991E-16,-6.98296267768627E-15,
1.));
#125786=DIRECTION('ref_axis',(1.,3.5527136788005E-14,1.40816906890159E-16));
#125787=DIRECTION('',(0.215543831721856,-0.484107959634392,-0.848045010612813));
#125788=DIRECTION('center_axis',(-1.4081690688991E-16,-6.98296267768627E-15,
1.));
#125789=DIRECTION('ref_axis',(1.,-4.69846384021366E-12,1.40816906857101E-16));
#125790=DIRECTION('',(-0.215535350357786,0.484111735780988,0.848045010612801));
#125791=DIRECTION('center_axis',(-1.4081690688991E-16,-6.98296267768627E-15,
1.));
#125792=DIRECTION('ref_axis',(1.,3.5527136788005E-14,1.40816906890159E-16));
#125793=DIRECTION('',(0.264966121135192,-0.458925500081766,-0.848045010612805));
#125794=DIRECTION('center_axis',(-1.4081690688991E-16,-6.98296267768627E-15,
1.));
#125795=DIRECTION('ref_axis',(1.,-2.39719355477064E-12,1.40816906873171E-16));
#125796=DIRECTION('',(-0.264958080947705,0.458930142086164,0.848045010612811));
#125797=DIRECTION('center_axis',(-1.4081690688991E-16,-6.98296267768627E-15,
1.));
#125798=DIRECTION('ref_axis',(1.,4.2632564145606E-14,1.40816906890208E-16));
#125799=DIRECTION('',(0.311485386277635,-0.428714956713879,-0.848045010612815));
#125800=DIRECTION('center_axis',(-1.4081690688991E-16,-6.98296267768627E-15,
1.));
#125801=DIRECTION('ref_axis',(1.,-1.22213350550737E-12,1.40816906881376E-16));
#125802=DIRECTION('',(-0.311477875356741,0.428720413717359,0.848045010612802));
#125803=DIRECTION('center_axis',(-1.4081690688991E-16,-6.98296267768627E-15,
1.));
#125804=DIRECTION('ref_axis',(1.,3.10862446895044E-14,1.40816906890128E-16));
#125805=DIRECTION('',(0.354591952345524,-0.393807322565893,-0.848045010612805));
#125806=DIRECTION('center_axis',(-1.4081690688991E-16,-6.98296267768627E-15,
1.));
#125807=DIRECTION('ref_axis',(1.,4.9862336481965E-12,1.40816906924729E-16));
#125808=DIRECTION('',(-0.354585052982407,0.393813534780348,0.848045010612804));
#125809=DIRECTION('center_axis',(-1.4081690688991E-16,-6.98296267768627E-15,
1.));
#125810=DIRECTION('ref_axis',(1.,-8.02836526847902E-31,1.4081690688991E-16));
#125811=DIRECTION('',(0.393813534780361,-0.354585052982394,-0.848045010612804));
#125812=DIRECTION('center_axis',(-1.4081690688991E-16,-6.98296267768627E-15,
1.));
#125813=DIRECTION('ref_axis',(1.,-1.27009514017118E-12,1.40816906881041E-16));
#125814=DIRECTION('',(-0.393807322565913,0.354591952345492,0.848045010612809));
#125815=DIRECTION('center_axis',(-1.4081690688991E-16,-6.98296267768627E-15,
1.));
#125816=DIRECTION('ref_axis',(1.,3.90798504668055E-14,1.40816906890183E-16));
#125817=DIRECTION('',(0.428720413717362,-0.311477875356717,-0.848045010612809));
#125818=DIRECTION('center_axis',(-1.4081690688991E-16,-6.98296267768627E-15,
1.));
#125819=DIRECTION('ref_axis',(1.,-2.58904009342587E-12,1.40816906871831E-16));
#125820=DIRECTION('',(-0.428714956713912,0.311485386277613,0.848045010612806));
#125821=DIRECTION('center_axis',(-1.4081690688991E-16,-6.98296267768627E-15,
1.));
#125822=DIRECTION('ref_axis',(1.,3.99680288865056E-14,1.4081690689019E-16));
#125823=DIRECTION('',(0.458930142086181,-0.264958080947701,-0.848045010612803));
#125824=DIRECTION('center_axis',(-1.4081690688991E-16,-6.98296267768627E-15,
1.));
#125825=DIRECTION('ref_axis',(1.,-1.19598452005484E-30,1.4081690688991E-16));
#125826=DIRECTION('',(-0.458925500081773,0.26496612113517,0.848045010612808));
#125827=DIRECTION('center_axis',(-1.4081690688991E-16,-6.98296267768627E-15,
1.));
#125828=DIRECTION('ref_axis',(1.,-9.76996261670138E-15,1.40816906889842E-16));
#125829=DIRECTION('',(0.484111735780991,-0.215535350357761,-0.848045010612805));
#125830=DIRECTION('center_axis',(-1.4081690688991E-16,-6.98296267768627E-15,
1.));
#125831=DIRECTION('ref_axis',(1.,-2.01350047746018E-12,1.4081690687585E-16));
#125832=DIRECTION('',(-0.484107959634416,0.215543831721835,0.848045010612804));
#125833=DIRECTION('center_axis',(-1.4081690688991E-16,-6.98296267768627E-15,
1.));
#125834=DIRECTION('ref_axis',(1.,-1.4210854715202E-14,1.40816906889811E-16));
#125835=DIRECTION('',(0.503989299991706,-0.163751169365648,-0.848045010612793));
#125836=DIRECTION('center_axis',(-1.4081690688991E-16,-6.98296267768627E-15,
1.));
#125837=DIRECTION('ref_axis',(1.,-1.36601840949879E-12,1.40816906880372E-16));
#125838=DIRECTION('',(-0.503986431075204,0.16375999898272,0.848045010612797));
#125839=DIRECTION('center_axis',(-1.4081690688991E-16,-6.98296267768627E-15,
1.));
#125840=DIRECTION('ref_axis',(1.,-1.24344978758018E-14,1.40816906889824E-16));
#125841=DIRECTION('',(0.518345051965146,-0.110172896294824,-0.848045010612797));
#125842=DIRECTION('center_axis',(-1.4081690688991E-16,-6.98296267768627E-15,
1.));
#125843=DIRECTION('ref_axis',(1.,-2.78088663208109E-12,1.40816906870492E-16));
#125844=DIRECTION('',(-0.518343121711178,0.110181977425763,0.848045010612798));
#125845=DIRECTION('center_axis',(-1.4081690688991E-16,-6.98296267768627E-15,
1.));
#125846=DIRECTION('ref_axis',(1.,-1.59872115546023E-14,1.40816906889799E-16));
#125847=DIRECTION('',(0.527021707078576,-0.0553875459170319,-0.848045010612805));
#125848=DIRECTION('center_axis',(-1.4081690688991E-16,-6.98296267768627E-15,
1.));
#125849=DIRECTION('ref_axis',(1.,-2.65121258280487E-12,1.40816906871397E-16));
#125850=DIRECTION('',(-0.527020736635418,0.0553967790670702,0.848045010612795));
#125851=DIRECTION('center_axis',(-1.4081690688991E-16,-6.98296267768627E-15,
1.));
#125852=DIRECTION('ref_axis',(1.,-2.75335310107039E-14,1.40816906889718E-16));
#125853=DIRECTION('',(0.529924202082878,4.64200440992836E-6,-0.848045010612807));
#125854=DIRECTION('center_axis',(-1.4081690688991E-16,-6.98296267768627E-15,
1.));
#125855=DIRECTION('ref_axis',(-1.,8.42929103913772E-31,-1.4081690688991E-16));
#125856=DIRECTION('',(-0.529924689637705,5.13655125493133E-6,0.848044705947746));
#125857=DIRECTION('center_axis',(1.4081690688991E-16,6.98296267768627E-15,
-1.));
#125858=DIRECTION('ref_axis',(-1.,8.44830660832796E-31,-1.4081690688991E-16));
#125859=DIRECTION('',(0.527022243656736,-0.0553871050427146,-0.848044705947751));
#125860=DIRECTION('center_axis',(1.4081690688991E-16,6.98296267768627E-15,
-1.));
#125861=DIRECTION('ref_axis',(-1.,8.43549292198398E-31,-1.4081690688991E-16));
#125862=DIRECTION('',(-0.527021169825118,0.0553973218681055,0.84804470594775));
#125863=DIRECTION('center_axis',(1.4081690688991E-16,6.98296267768627E-15,
-1.));
#125864=DIRECTION('ref_axis',(-1.,8.44830660832796E-31,-1.4081690688991E-16));
#125865=DIRECTION('',(0.518345631687772,-0.110172513923351,-0.848044705947755));
#125866=DIRECTION('center_axis',(1.4081690688991E-16,6.98296267768627E-15,
-1.));
#125867=DIRECTION('ref_axis',(-1.,1.06581410364015E-14,-1.40816906889836E-16));
#125868=DIRECTION('',(-0.51834349578966,0.110182562533931,0.848044705947753));
#125869=DIRECTION('center_axis',(1.4081690688991E-16,6.98296267768627E-15,
-1.));
#125870=DIRECTION('ref_axis',(-1.,8.44830660832796E-31,-1.4081690688991E-16));
#125871=DIRECTION('',(0.50398991650726,-0.163750849686354,-0.848044705947748));
#125872=DIRECTION('center_axis',(1.4081690688991E-16,6.98296267768627E-15,
-1.));
#125873=DIRECTION('ref_axis',(-1.,3.37507799486048E-14,-1.40816906889675E-16));
#125874=DIRECTION('',(-0.50398674194399,0.163760619987459,0.848044705947749));
#125875=DIRECTION('center_axis',(1.4081690688991E-16,6.98296267768627E-15,
-1.));
#125876=DIRECTION('ref_axis',(-1.,8.44830660832796E-31,-1.4081690688991E-16));
#125877=DIRECTION('',(0.484112382334808,-0.215535096873135,-0.848044705947749));
#125878=DIRECTION('center_axis',(1.4081690688991E-16,6.98296267768627E-15,
-1.));
#125879=DIRECTION('ref_axis',(-1.,-4.52970994047064E-14,-1.40816906890227E-16));
#125880=DIRECTION('',(-0.484108203887568,0.215544481819274,0.848044705947754));
#125881=DIRECTION('center_axis',(1.4081690688991E-16,6.98296267768627E-15,
-1.));
#125882=DIRECTION('ref_axis',(-1.,-8.88178419700124E-16,-1.40816906889917E-16));
#125883=DIRECTION('',(0.458930811594458,-0.264957896434951,-0.848044705947757));
#125884=DIRECTION('center_axis',(1.4081690688991E-16,6.98296267768627E-15,
-1.));
#125885=DIRECTION('ref_axis',(-1.,8.43549292198398E-31,-1.4081690688991E-16));
#125886=DIRECTION('',(-0.458925675043199,0.264966793202718,0.848044705947754));
#125887=DIRECTION('center_axis',(1.4081690688991E-16,6.98296267768627E-15,
-1.));
#125888=DIRECTION('ref_axis',(-1.,-8.88178419700124E-16,-1.40816906889917E-16));
#125889=DIRECTION('',(0.428721098844841,-0.311477761837424,-0.848044705947759));
#125890=DIRECTION('center_axis',(1.4081690688991E-16,6.98296267768627E-15,
-1.));
#125891=DIRECTION('ref_axis',(-1.,-1.35003119794419E-13,-1.40816906890853E-16));
#125892=DIRECTION('',(-0.428715060466688,0.311486072951948,0.848044705947757));
#125893=DIRECTION('center_axis',(1.4081690688991E-16,6.98296267768627E-15,
-1.));
#125894=DIRECTION('ref_axis',(-1.,8.44830660832796E-31,-1.4081690688991E-16));
#125895=DIRECTION('',(0.393814228020628,-0.354585011700303,-0.848044705947754));
#125896=DIRECTION('center_axis',(1.4081690688991E-16,6.98296267768627E-15,
-1.));
#125897=DIRECTION('ref_axis',(-1.,-1.58095758706622E-13,-1.40816906891014E-16));
#125898=DIRECTION('',(-0.393807353973301,0.354592646103292,0.848044705947754));
#125899=DIRECTION('center_axis',(1.4081690688991E-16,6.98296267768627E-15,
-1.));
#125900=DIRECTION('ref_axis',(-1.,8.44830660832796E-31,-1.4081690688991E-16));
#125901=DIRECTION('',(0.354592646103302,-0.393807353973285,-0.848044705947757));
#125902=DIRECTION('center_axis',(1.4081690688991E-16,6.98296267768627E-15,
-1.));
#125903=DIRECTION('ref_axis',(-1.,8.43549292198398E-31,-1.4081690688991E-16));
#125904=DIRECTION('',(-0.354585011700314,0.393814228020627,0.84804470594775));
#125905=DIRECTION('center_axis',(1.4081690688991E-16,6.98296267768627E-15,
-1.));
#125906=DIRECTION('ref_axis',(-1.,8.44830660832796E-31,-1.4081690688991E-16));
#125907=DIRECTION('',(0.311486072951975,-0.428715060466675,-0.848044705947754));
#125908=DIRECTION('center_axis',(1.4081690688991E-16,6.98296267768627E-15,
-1.));
#125909=DIRECTION('ref_axis',(-1.,8.43549292198398E-31,-1.4081690688991E-16));
#125910=DIRECTION('',(-0.311477761837451,0.428721098844829,0.848044705947755));
#125911=DIRECTION('center_axis',(1.4081690688991E-16,6.98296267768627E-15,
-1.));
#125912=DIRECTION('ref_axis',(-1.,8.44830660832796E-31,-1.4081690688991E-16));
#125913=DIRECTION('',(0.264966793202735,-0.458925675043194,-0.848044705947751));
#125914=DIRECTION('center_axis',(1.4081690688991E-16,6.98296267768627E-15,
-1.));
#125915=DIRECTION('ref_axis',(-1.,8.43549292198398E-31,-1.4081690688991E-16));
#125916=DIRECTION('',(-0.264957896434977,0.458930811594459,0.848044705947748));
#125917=DIRECTION('center_axis',(1.4081690688991E-16,6.98296267768627E-15,
-1.));
#125918=DIRECTION('ref_axis',(-1.,8.44830660832796E-31,-1.4081690688991E-16));
#125919=DIRECTION('',(0.215544481819299,-0.484108203887551,-0.848044705947758));
#125920=DIRECTION('center_axis',(1.4081690688991E-16,6.98296267768627E-15,
-1.));
#125921=DIRECTION('ref_axis',(-1.,8.43549292198398E-31,-1.4081690688991E-16));
#125922=DIRECTION('',(-0.215535096873164,0.484112382334786,0.848044705947755));
#125923=DIRECTION('center_axis',(1.4081690688991E-16,6.98296267768627E-15,
-1.));
#125924=DIRECTION('ref_axis',(-1.,8.44830660832796E-31,-1.4081690688991E-16));
#125925=DIRECTION('',(0.163760619987462,-0.503986741943988,-0.84804470594775));
#125926=DIRECTION('center_axis',(1.4081690688991E-16,6.98296267768627E-15,
-1.));
#125927=DIRECTION('ref_axis',(-1.,8.43549292198398E-31,-1.4081690688991E-16));
#125928=DIRECTION('',(-0.163750849686384,0.503989916507238,0.848044705947755));
#125929=DIRECTION('center_axis',(1.4081690688991E-16,6.98296267768627E-15,
-1.));
#125930=DIRECTION('ref_axis',(-1.,8.44830660832796E-31,-1.4081690688991E-16));
#125931=DIRECTION('',(0.110182562533939,-0.518343495789657,-0.848044705947754));
#125932=DIRECTION('center_axis',(1.4081690688991E-16,6.98296267768627E-15,
-1.));
#125933=DIRECTION('ref_axis',(-1.,8.43549292198398E-31,-1.4081690688991E-16));
#125934=DIRECTION('',(-0.110172513923364,0.518345631687762,0.848044705947759));
#125935=DIRECTION('center_axis',(1.4081690688991E-16,6.98296267768627E-15,
-1.));
#125936=DIRECTION('ref_axis',(-1.,8.44830660832796E-31,-1.4081690688991E-16));
#125937=DIRECTION('',(0.0553973218681131,-0.527021169825101,-0.84804470594776));
#125938=DIRECTION('center_axis',(1.4081690688991E-16,6.98296267768627E-15,
-1.));
#125939=DIRECTION('ref_axis',(-1.,8.43549292198398E-31,-1.4081690688991E-16));
#125940=DIRECTION('',(-0.0553871050427231,0.527022243656726,0.848044705947757));
#125941=DIRECTION('center_axis',(1.4081690688991E-16,6.98296267768627E-15,
-1.));
#125942=DIRECTION('ref_axis',(-1.,8.44830660832796E-31,-1.4081690688991E-16));
#125943=DIRECTION('',(5.13655126277485E-6,-0.529924689637692,-0.848044705947753));
#125944=DIRECTION('center_axis',(1.4081690688991E-16,6.98296267768627E-15,
-1.));
#125945=DIRECTION('ref_axis',(-1.,8.43549292198398E-31,-1.4081690688991E-16));
#125946=DIRECTION('',(5.13655125885311E-6,0.529924689637688,0.848044705947756));
#125947=DIRECTION('center_axis',(1.4081690688991E-16,6.98296267768627E-15,
-1.));
#125948=DIRECTION('ref_axis',(-1.,8.44830660832796E-31,-1.4081690688991E-16));
#125949=DIRECTION('',(-0.0553871050427198,-0.527022243656726,-0.848044705947757));
#125950=DIRECTION('center_axis',(1.4081690688991E-16,6.98296267768627E-15,
-1.));
#125951=DIRECTION('ref_axis',(-1.,8.43549292198398E-31,-1.4081690688991E-16));
#125952=DIRECTION('',(0.0553973218681098,0.527021169825101,0.84804470594776));
#125953=DIRECTION('center_axis',(1.4081690688991E-16,6.98296267768627E-15,
-1.));
#125954=DIRECTION('ref_axis',(-1.,8.44830660832796E-31,-1.4081690688991E-16));
#125955=DIRECTION('',(-0.110172513923356,-0.518345631687777,-0.848044705947751));
#125956=DIRECTION('center_axis',(1.4081690688991E-16,6.98296267768627E-15,
-1.));
#125957=DIRECTION('ref_axis',(-1.,8.43549292198398E-31,-1.4081690688991E-16));
#125958=DIRECTION('',(0.110182562533938,0.518343495789653,0.848044705947757));
#125959=DIRECTION('center_axis',(1.4081690688991E-16,6.98296267768627E-15,
-1.));
#125960=DIRECTION('ref_axis',(-1.,8.44830660832796E-31,-1.4081690688991E-16));
#125961=DIRECTION('',(-0.163750849686368,-0.503989916507249,-0.848044705947751));
#125962=DIRECTION('center_axis',(1.4081690688991E-16,6.98296267768627E-15,
-1.));
#125963=DIRECTION('ref_axis',(-1.,8.43549292198398E-31,-1.4081690688991E-16));
#125964=DIRECTION('',(0.163760619987469,0.503986741943977,0.848044705947755));
#125965=DIRECTION('center_axis',(1.4081690688991E-16,6.98296267768627E-15,
-1.));
#125966=DIRECTION('ref_axis',(-1.,8.44830660832796E-31,-1.4081690688991E-16));
#125967=DIRECTION('',(-0.215535096873149,-0.484112382334797,-0.848044705947752));
#125968=DIRECTION('center_axis',(1.4081690688991E-16,6.98296267768627E-15,
-1.));
#125969=DIRECTION('ref_axis',(-1.,8.43549292198398E-31,-1.4081690688991E-16));
#125970=DIRECTION('',(0.215544481819295,0.484108203887571,0.848044705947748));
#125971=DIRECTION('center_axis',(1.4081690688991E-16,6.98296267768627E-15,
-1.));
#125972=DIRECTION('ref_axis',(-1.,-5.32907051820075E-15,-1.40816906889948E-16));
#125973=DIRECTION('',(-0.264957896434958,-0.458930811594447,-0.848044705947761));
#125974=DIRECTION('center_axis',(1.4081690688991E-16,6.98296267768627E-15,
-1.));
#125975=DIRECTION('ref_axis',(-1.,-1.80122583515185E-12,-1.40816906902488E-16));
#125976=DIRECTION('',(0.264966793202733,0.45892567504319,0.848044705947754));
#125977=DIRECTION('center_axis',(1.4081690688991E-16,6.98296267768627E-15,
-1.));
#125978=DIRECTION('ref_axis',(-1.,-1.06581410364015E-14,-1.40816906889985E-16));
#125979=DIRECTION('',(-0.311477761837441,-0.428721098844834,-0.848044705947756));
#125980=DIRECTION('center_axis',(1.4081690688991E-16,6.98296267768627E-15,
-1.));
#125981=DIRECTION('ref_axis',(-1.,1.89182003396127E-12,-1.408169068767E-16));
#125982=DIRECTION('',(0.311486072951956,0.42871506046668,0.848044705947758));
#125983=DIRECTION('center_axis',(1.4081690688991E-16,6.98296267768627E-15,
-1.));
#125984=DIRECTION('ref_axis',(-1.,8.44830660832796E-31,-1.4081690688991E-16));
#125985=DIRECTION('',(-0.354585011700305,-0.393814228020624,-0.848044705947755));
#125986=DIRECTION('center_axis',(1.4081690688991E-16,6.98296267768627E-15,
-1.));
#125987=DIRECTION('ref_axis',(-1.,8.43549292198398E-31,-1.4081690688991E-16));
#125988=DIRECTION('',(0.354592646103294,0.39380735397329,0.848044705947758));
#125989=DIRECTION('center_axis',(1.4081690688991E-16,6.98296267768627E-15,
-1.));
#125990=DIRECTION('ref_axis',(-1.,8.44830660832796E-31,-1.4081690688991E-16));
#125991=DIRECTION('',(-0.393807353973315,-0.354592646103273,-0.848044705947756));
#125992=DIRECTION('center_axis',(1.4081690688991E-16,6.98296267768627E-15,
-1.));
#125993=DIRECTION('ref_axis',(-1.,8.43549292198398E-31,-1.4081690688991E-16));
#125994=DIRECTION('',(0.393814228020631,0.354585011700291,0.848044705947758));
#125995=DIRECTION('center_axis',(1.4081690688991E-16,6.98296267768627E-15,
-1.));
#125996=DIRECTION('ref_axis',(-1.,8.44830660832796E-31,-1.4081690688991E-16));
#125997=DIRECTION('',(-0.428715060466688,-0.311486072951948,-0.848044705947757));
#125998=DIRECTION('center_axis',(1.4081690688991E-16,6.98296267768627E-15,
-1.));
#125999=DIRECTION('ref_axis',(-1.,-2.1618262735501E-12,-1.40816906905006E-16));
#126000=DIRECTION('',(0.428721098844841,0.311477761837424,0.848044705947759));
#126001=DIRECTION('center_axis',(1.4081690688991E-16,6.98296267768627E-15,
-1.));
#126002=DIRECTION('ref_axis',(-1.,8.44830660832796E-31,-1.4081690688991E-16));
#126003=DIRECTION('',(-0.458925675043199,-0.264966793202717,-0.848044705947754));
#126004=DIRECTION('center_axis',(1.4081690688991E-16,6.98296267768627E-15,
-1.));
#126005=DIRECTION('ref_axis',(-1.,2.25064411552012E-12,-1.40816906874194E-16));
#126006=DIRECTION('',(0.458930811594462,0.264957896434966,0.84804470594775));
#126007=DIRECTION('center_axis',(1.4081690688991E-16,6.98296267768627E-15,
-1.));
#126008=DIRECTION('ref_axis',(-1.,8.44830660832796E-31,-1.4081690688991E-16));
#126009=DIRECTION('',(-0.484108203887567,-0.215544481819293,-0.84804470594775));
#126010=DIRECTION('center_axis',(1.4081690688991E-16,6.98296267768627E-15,
-1.));
#126011=DIRECTION('ref_axis',(-1.,2.34123831432953E-12,-1.40816906873562E-16));
#126012=DIRECTION('',(0.484112382334803,0.215535096873139,0.848044705947751));
#126013=DIRECTION('center_axis',(1.4081690688991E-16,6.98296267768627E-15,
-1.));
#126014=DIRECTION('ref_axis',(-1.,8.44830660832796E-31,-1.4081690688991E-16));
#126015=DIRECTION('',(-0.503986741943985,-0.163760619987452,-0.848044705947754));
#126016=DIRECTION('center_axis',(1.4081690688991E-16,6.98296267768627E-15,
-1.));
#126017=DIRECTION('ref_axis',(-1.,2.43183251313894E-12,-1.40816906872929E-16));
#126018=DIRECTION('',(0.503989916507249,0.163750849686371,0.848044705947751));
#126019=DIRECTION('center_axis',(1.4081690688991E-16,6.98296267768627E-15,
-1.));
#126020=DIRECTION('ref_axis',(-1.,8.44830660832796E-31,-1.4081690688991E-16));
#126021=DIRECTION('',(-0.518343495789664,-0.110182562533935,-0.84804470594775));
#126022=DIRECTION('center_axis',(1.4081690688991E-16,6.98296267768627E-15,
-1.));
#126023=DIRECTION('ref_axis',(-1.,2.52153853352866E-12,-1.40816906872303E-16));
#126024=DIRECTION('',(0.518345631687777,0.110172513923356,0.848044705947751));
#126025=DIRECTION('center_axis',(1.4081690688991E-16,6.98296267768627E-15,
-1.));
#126026=DIRECTION('ref_axis',(-1.,8.44830660832796E-31,-1.4081690688991E-16));
#126027=DIRECTION('',(-0.527021169825118,-0.0553973218681055,-0.84804470594775));
#126028=DIRECTION('center_axis',(1.4081690688991E-16,6.98296267768627E-15,
-1.));
#126029=DIRECTION('ref_axis',(-1.,8.43549292198398E-31,-1.4081690688991E-16));
#126030=DIRECTION('',(0.52702224365674,0.0553871050427153,0.848044705947748));
#126031=DIRECTION('center_axis',(1.4081690688991E-16,6.98296267768627E-15,
-1.));
#126032=DIRECTION('ref_axis',(-1.,8.44830660832796E-31,-1.4081690688991E-16));
#126033=DIRECTION('',(-0.5299246896377,-5.13655125503461E-6,-0.848044705947749));
#126034=DIRECTION('center_axis',(1.4081690688991E-16,6.98296267768627E-15,
-1.));
#126035=DIRECTION('ref_axis',(-1.,8.43549292198398E-31,-1.4081690688991E-16));
#126036=DIRECTION('',(-0.529919264233204,5.85699181126825E-15,-0.848048096156427));
#126037=DIRECTION('center_axis',(1.4081690688991E-16,6.98296267768627E-15,
-1.));
#126038=DIRECTION('ref_axis',(-1.,8.43549292198398E-31,-1.4081690688991E-16));
#126039=DIRECTION('',(0.5299246896377,-5.13655126669649E-6,0.848044705947748));
#126040=DIRECTION('center_axis',(1.4081690688991E-16,6.98296267768627E-15,
-1.));
#126041=DIRECTION('ref_axis',(-1.,8.44830660832796E-31,-1.4081690688991E-16));
#126042=DIRECTION('',(-0.52702224365675,0.0553871050427198,-0.848044705947742));
#126043=DIRECTION('center_axis',(1.4081690688991E-16,6.98296267768627E-15,
-1.));
#126044=DIRECTION('ref_axis',(-1.,8.43549292198398E-31,-1.4081690688991E-16));
#126045=DIRECTION('',(0.527021169825118,-0.0553973218681105,0.84804470594775));
#126046=DIRECTION('center_axis',(1.4081690688991E-16,6.98296267768627E-15,
-1.));
#126047=DIRECTION('ref_axis',(-1.,8.44830660832796E-31,-1.4081690688991E-16));
#126048=DIRECTION('',(-0.518345631687786,0.110172513923365,-0.848044705947744));
#126049=DIRECTION('center_axis',(1.4081690688991E-16,6.98296267768627E-15,
-1.));
#126050=DIRECTION('ref_axis',(-1.,8.43549292198398E-31,-1.4081690688991E-16));
#126051=DIRECTION('',(0.518343495789664,-0.110182562533938,0.84804470594775));
#126052=DIRECTION('center_axis',(1.4081690688991E-16,6.98296267768627E-15,
-1.));
#126053=DIRECTION('ref_axis',(-1.,8.44830660832796E-31,-1.4081690688991E-16));
#126054=DIRECTION('',(-0.503989916507253,0.163750849686366,-0.848044705947749));
#126055=DIRECTION('center_axis',(1.4081690688991E-16,6.98296267768627E-15,
-1.));
#126056=DIRECTION('ref_axis',(-1.,8.43549292198398E-31,-1.4081690688991E-16));
#126057=DIRECTION('',(0.50398674194398,-0.16376061998746,0.848044705947755));
#126058=DIRECTION('center_axis',(1.4081690688991E-16,6.98296267768627E-15,
-1.));
#126059=DIRECTION('ref_axis',(-1.,8.44830660832796E-31,-1.4081690688991E-16));
#126060=DIRECTION('',(-0.484112382334807,0.215535096873148,-0.848044705947747));
#126061=DIRECTION('center_axis',(1.4081690688991E-16,6.98296267768627E-15,
-1.));
#126062=DIRECTION('ref_axis',(-1.,8.43549292198398E-31,-1.4081690688991E-16));
#126063=DIRECTION('',(0.484108203887571,-0.215544481819295,0.848044705947747));
#126064=DIRECTION('center_axis',(1.4081690688991E-16,6.98296267768627E-15,
-1.));
#126065=DIRECTION('ref_axis',(-1.,8.44830660832796E-31,-1.4081690688991E-16));
#126066=DIRECTION('',(-0.458930811594466,0.264957896434968,-0.848044705947747));
#126067=DIRECTION('center_axis',(1.4081690688991E-16,6.98296267768627E-15,
-1.));
#126068=DIRECTION('ref_axis',(-1.,8.43549292198398E-31,-1.4081690688991E-16));
#126069=DIRECTION('',(0.458925675043206,-0.264966793202741,0.848044705947743));
#126070=DIRECTION('center_axis',(1.4081690688991E-16,6.98296267768627E-15,
-1.));
#126071=DIRECTION('ref_axis',(-1.,8.44830660832796E-31,-1.4081690688991E-16));
#126072=DIRECTION('',(-0.428721098844845,0.311477761837453,-0.848044705947746));
#126073=DIRECTION('center_axis',(1.4081690688991E-16,6.98296267768627E-15,
-1.));
#126074=DIRECTION('ref_axis',(-1.,8.43549292198398E-31,-1.4081690688991E-16));
#126075=DIRECTION('',(0.428715060466697,-0.311486072951958,0.848044705947749));
#126076=DIRECTION('center_axis',(1.4081690688991E-16,6.98296267768627E-15,
-1.));
#126077=DIRECTION('ref_axis',(-1.,8.44830660832796E-31,-1.4081690688991E-16));
#126078=DIRECTION('',(-0.393814228020624,0.354585011700306,-0.848044705947755));
#126079=DIRECTION('center_axis',(1.4081690688991E-16,6.98296267768627E-15,
-1.));
#126080=DIRECTION('ref_axis',(-1.,8.43549292198398E-31,-1.4081690688991E-16));
#126081=DIRECTION('',(0.393807353973302,-0.354592646103312,0.848044705947745));
#126082=DIRECTION('center_axis',(1.4081690688991E-16,6.98296267768627E-15,
-1.));
#126083=DIRECTION('ref_axis',(-1.,8.44830660832796E-31,-1.4081690688991E-16));
#126084=DIRECTION('',(-0.354592646103293,0.393807353973316,-0.848044705947747));
#126085=DIRECTION('center_axis',(1.4081690688991E-16,6.98296267768627E-15,
-1.));
#126086=DIRECTION('ref_axis',(-1.,8.43549292198398E-31,-1.4081690688991E-16));
#126087=DIRECTION('',(0.35458501170032,-0.393814228020626,0.848044705947748));
#126088=DIRECTION('center_axis',(1.4081690688991E-16,6.98296267768627E-15,
-1.));
#126089=DIRECTION('ref_axis',(-1.,8.44830660832796E-31,-1.4081690688991E-16));
#126090=DIRECTION('',(-0.311486072951978,0.428715060466679,-0.84804470594775));
#126091=DIRECTION('center_axis',(1.4081690688991E-16,6.98296267768627E-15,
-1.));
#126092=DIRECTION('ref_axis',(-1.,3.5118574714943E-12,-1.40816906865387E-16));
#126093=DIRECTION('',(0.31147776183744,-0.428721098844837,0.848044705947755));
#126094=DIRECTION('center_axis',(1.4081690688991E-16,6.98296267768627E-15,
-1.));
#126095=DIRECTION('ref_axis',(-1.,-1.95399252334028E-14,-1.40816906890047E-16));
#126096=DIRECTION('',(-0.264966793202737,0.4589256750432,-0.848044705947748));
#126097=DIRECTION('center_axis',(1.4081690688991E-16,6.98296267768627E-15,
-1.));
#126098=DIRECTION('ref_axis',(-1.,-3.60245167030371E-12,-1.40816906915066E-16));
#126099=DIRECTION('',(0.264957896434972,-0.458930811594474,0.848044705947742));
#126100=DIRECTION('center_axis',(1.4081690688991E-16,6.98296267768627E-15,
-1.));
#126101=DIRECTION('ref_axis',(-1.,1.95399252334028E-14,-1.40816906889774E-16));
#126102=DIRECTION('',(-0.215544481819303,0.48410820388756,-0.848044705947752));
#126103=DIRECTION('center_axis',(1.4081690688991E-16,6.98296267768627E-15,
-1.));
#126104=DIRECTION('ref_axis',(-1.,1.84652293455656E-12,-1.40816906877016E-16));
#126105=DIRECTION('',(0.215535096873159,-0.484112382334816,0.848044705947739));
#126106=DIRECTION('center_axis',(1.4081690688991E-16,6.98296267768627E-15,
-1.));
#126107=DIRECTION('ref_axis',(-1.,2.1316282072803E-14,-1.40816906889762E-16));
#126108=DIRECTION('',(-0.16376061998747,0.503986741944006,-0.848044705947738));
#126109=DIRECTION('center_axis',(1.4081690688991E-16,6.98296267768627E-15,
-1.));
#126110=DIRECTION('ref_axis',(-1.,1.89093185554157E-12,-1.40816906876706E-16));
#126111=DIRECTION('',(0.163750849686377,-0.503989916507272,0.848044705947736));
#126112=DIRECTION('center_axis',(1.4081690688991E-16,6.98296267768627E-15,
-1.));
#126113=DIRECTION('ref_axis',(-1.,1.06581410364015E-14,-1.40816906889836E-16));
#126114=DIRECTION('',(-0.110182562533946,0.518343495789671,-0.848044705947745));
#126115=DIRECTION('center_axis',(1.4081690688991E-16,6.98296267768627E-15,
-1.));
#126116=DIRECTION('ref_axis',(-1.,1.93622895494627E-12,-1.4081690687639E-16));
#126117=DIRECTION('',(0.110172513923365,-0.51834563168779,0.848044705947742));
#126118=DIRECTION('center_axis',(1.4081690688991E-16,6.98296267768627E-15,
-1.));
#126119=DIRECTION('ref_axis',(-1.,1.06581410364015E-14,-1.40816906889836E-16));
#126120=DIRECTION('',(-0.0553973218681178,0.527021169825125,-0.848044705947745));
#126121=DIRECTION('center_axis',(1.4081690688991E-16,6.98296267768627E-15,
-1.));
#126122=DIRECTION('ref_axis',(-1.,1.98152605435098E-12,-1.40816906876074E-16));
#126123=DIRECTION('',(0.0553871050427273,-0.527022243656745,0.848044705947745));
#126124=DIRECTION('center_axis',(1.4081690688991E-16,6.98296267768627E-15,
-1.));
#126125=DIRECTION('ref_axis',(-1.,1.15463194561016E-14,-1.4081690688983E-16));
#126126=DIRECTION('',(-5.13655126618054E-6,0.529924689637707,-0.848044705947744));
#126127=DIRECTION('',(-5.1365512553442E-6,-0.529924689637711,0.848044705947741));
#126128=DIRECTION('center_axis',(1.4081690688991E-16,6.98296267768627E-15,
-1.));
#126129=DIRECTION('ref_axis',(-1.,1.15463194561016E-14,-1.4081690688983E-16));
#126130=DIRECTION('',(0.0553871050427141,0.527022243656745,-0.848044705947745));
#126131=DIRECTION('center_axis',(1.4081690688991E-16,6.98296267768627E-15,
-1.));
#126132=DIRECTION('ref_axis',(-1.,2.07123207474069E-12,-1.40816906875447E-16));
#126133=DIRECTION('',(-0.0553973218681087,-0.52702116982513,0.848044705947743));
#126134=DIRECTION('center_axis',(1.4081690688991E-16,6.98296267768627E-15,
-1.));
#126135=DIRECTION('ref_axis',(-1.,1.15463194561016E-14,-1.4081690688983E-16));
#126136=DIRECTION('',(0.110172513923356,0.518345631687781,-0.848044705947748));
#126137=DIRECTION('center_axis',(1.4081690688991E-16,6.98296267768627E-15,
-1.));
#126138=DIRECTION('ref_axis',(-1.,2.1165291741454E-12,-1.40816906875131E-16));
#126139=DIRECTION('',(-0.110182562533934,-0.518343495789662,0.848044705947752));
#126140=DIRECTION('center_axis',(1.4081690688991E-16,6.98296267768627E-15,
-1.));
#126141=DIRECTION('ref_axis',(-1.,1.15463194561016E-14,-1.4081690688983E-16));
#126142=DIRECTION('',(0.163750849686359,0.503989916507255,-0.84804470594775));
#126143=DIRECTION('center_axis',(1.4081690688991E-16,6.98296267768627E-15,
-1.));
#126144=DIRECTION('ref_axis',(-1.,4.32276436868051E-12,-1.40816906859725E-16));
#126145=DIRECTION('',(-0.16376061998747,-0.503986741943991,0.848044705947747));
#126146=DIRECTION('center_axis',(1.4081690688991E-16,6.98296267768627E-15,
-1.));
#126147=DIRECTION('ref_axis',(-1.,1.15463194561016E-14,-1.4081690688983E-16));
#126148=DIRECTION('',(0.215535096873149,0.484112382334808,-0.848044705947746));
#126149=DIRECTION('center_axis',(1.4081690688991E-16,6.98296267768627E-15,
-1.));
#126150=DIRECTION('ref_axis',(-1.,2.20623519453511E-12,-1.40816906874504E-16));
#126151=DIRECTION('',(-0.215544481819284,-0.484108203887573,0.848044705947749));
#126152=DIRECTION('center_axis',(1.4081690688991E-16,6.98296267768627E-15,
-1.));
#126153=DIRECTION('ref_axis',(-1.,1.24344978758018E-14,-1.40816906889824E-16));
#126154=DIRECTION('',(0.264957896434972,0.458930811594474,-0.848044705947742));
#126155=DIRECTION('center_axis',(1.4081690688991E-16,6.98296267768627E-15,
-1.));
#126156=DIRECTION('ref_axis',(-1.,4.50306458787963E-12,-1.40816906858466E-16));
#126157=DIRECTION('',(-0.264966793202729,-0.458925675043209,0.848044705947745));
#126158=DIRECTION('center_axis',(1.4081690688991E-16,6.98296267768627E-15,
-1.));
#126159=DIRECTION('ref_axis',(-1.,1.86517468137026E-14,-1.4081690688978E-16));
#126160=DIRECTION('',(0.311477761837426,0.428721098844875,-0.848044705947742));
#126161=DIRECTION('center_axis',(1.4081690688991E-16,6.98296267768627E-15,
-1.));
#126162=DIRECTION('ref_axis',(-1.,1.14841469667226E-12,-1.40816906881891E-16));
#126163=DIRECTION('',(-0.311486072951947,-0.428715060466726,0.848044705947739));
#126164=DIRECTION('center_axis',(1.4081690688991E-16,6.98296267768627E-15,
-1.));
#126165=DIRECTION('ref_axis',(-1.,-1.86517468137026E-14,-1.40816906890041E-16));
#126166=DIRECTION('',(0.354585011700309,0.393814228020635,-0.848044705947748));
#126167=DIRECTION('center_axis',(1.4081690688991E-16,6.98296267768627E-15,
-1.));
#126168=DIRECTION('ref_axis',(-1.,2.34123831432953E-12,-1.40816906873562E-16));
#126169=DIRECTION('',(-0.354592646103299,-0.393807353973315,0.848044705947745));
#126170=DIRECTION('center_axis',(1.4081690688991E-16,6.98296267768627E-15,
-1.));
#126171=DIRECTION('ref_axis',(-1.,-6.21724893790088E-15,-1.40816906889954E-16));
#126172=DIRECTION('',(0.393807353973314,0.354592646103304,-0.848044705947743));
#126173=DIRECTION('center_axis',(1.4081690688991E-16,6.98296267768627E-15,
-1.));
#126174=DIRECTION('ref_axis',(-1.,1.19282361765727E-12,-1.40816906881581E-16));
#126175=DIRECTION('',(-0.393814228020621,-0.354585011700328,0.848044705947747));
#126176=DIRECTION('center_axis',(1.4081690688991E-16,6.98296267768627E-15,
-1.));
#126177=DIRECTION('ref_axis',(-1.,-1.95399252334028E-14,-1.40816906890047E-16));
#126178=DIRECTION('',(0.428715060466673,0.31148607295198,-0.848044705947753));
#126179=DIRECTION('center_axis',(1.4081690688991E-16,6.98296267768627E-15,
-1.));
#126180=DIRECTION('ref_axis',(-1.,2.43183251313894E-12,-1.40816906872929E-16));
#126181=DIRECTION('',(-0.428721098844844,-0.311477761837459,0.848044705947745));
#126182=DIRECTION('center_axis',(1.4081690688991E-16,6.98296267768627E-15,
-1.));
#126183=DIRECTION('ref_axis',(-1.,-1.33226762955019E-14,-1.40816906890003E-16));
#126184=DIRECTION('',(0.458925675043199,0.264966793202751,-0.848044705947744));
#126185=DIRECTION('center_axis',(1.4081690688991E-16,6.98296267768627E-15,
-1.));
#126186=DIRECTION('ref_axis',(-1.,4.9533710466676E-12,-1.40816906855321E-16));
#126187=DIRECTION('',(-0.458930811594451,-0.264957896434974,0.848044705947754));
#126188=DIRECTION('center_axis',(1.4081690688991E-16,6.98296267768627E-15,
-1.));
#126189=DIRECTION('ref_axis',(-1.,1.33226762955019E-14,-1.40816906889817E-16));
#126190=DIRECTION('',(0.484108203887558,0.215544481819315,-0.84804470594775));
#126191=DIRECTION('center_axis',(1.4081690688991E-16,6.98296267768627E-15,
-1.));
#126192=DIRECTION('ref_axis',(-1.,2.52153853352866E-12,-1.40816906872303E-16));
#126193=DIRECTION('',(-0.484112382334805,-0.21553509687316,0.848044705947745));
#126194=DIRECTION('center_axis',(1.4081690688991E-16,6.98296267768627E-15,
-1.));
#126195=DIRECTION('ref_axis',(-1.,4.79616346638068E-14,-1.40816906889576E-16));
#126196=DIRECTION('',(0.503986741943984,0.163760619987471,-0.848044705947751));
#126197=DIRECTION('center_axis',(1.4081690688991E-16,6.98296267768627E-15,
-1.));
#126198=DIRECTION('ref_axis',(-1.,-7.70050689880008E-12,-1.40816906943683E-16));
#126199=DIRECTION('',(-0.503989916507243,-0.163750849686383,0.848044705947753));
#126200=DIRECTION('center_axis',(1.4081690688991E-16,6.98296267768627E-15,
-1.));
#126201=DIRECTION('ref_axis',(-1.,-7.105427357601E-15,-1.4081690688996E-16));
#126202=DIRECTION('',(0.518343495789668,0.110182562533952,-0.848044705947745));
#126203=DIRECTION('center_axis',(1.4081690688991E-16,6.98296267768627E-15,
-1.));
#126204=DIRECTION('ref_axis',(-1.,2.28528307388842E-12,-1.40816906873952E-16));
#126205=DIRECTION('',(-0.518345631687771,-0.110172513923371,0.848044705947753));
#126206=DIRECTION('center_axis',(1.4081690688991E-16,6.98296267768627E-15,
-1.));
#126207=DIRECTION('ref_axis',(-1.,4.35207425653061E-14,-1.40816906889607E-16));
#126208=DIRECTION('',(0.527021169825113,0.0553973218681212,-0.848044705947752));
#126209=DIRECTION('center_axis',(1.4081690688991E-16,6.98296267768627E-15,
-1.));
#126210=DIRECTION('ref_axis',(-1.,2.65654165332307E-12,-1.4081690687136E-16));
#126211=DIRECTION('',(-0.527022243656726,-0.0553871050427333,0.848044705947756));
#126212=DIRECTION('center_axis',(1.4081690688991E-16,6.98296267768627E-15,
-1.));
#126213=DIRECTION('ref_axis',(-1.,-3.5527136788005E-15,-1.40816906889935E-16));
#126214=DIRECTION('',(0.529924689637695,5.13655126659336E-6,-0.848044705947752));
#126215=DIRECTION('center_axis',(1.4081690688991E-16,6.98296267768627E-15,
-1.));
#126216=DIRECTION('ref_axis',(1.,-8.91767816654029E-31,1.4081690688991E-16));
#126217=DIRECTION('center_axis',(-1.4081690688991E-16,-6.98296267768627E-15,
1.));
#126218=DIRECTION('ref_axis',(-1.,8.91767816654029E-31,-1.4081690688991E-16));
#126219=DIRECTION('',(-0.529919264233204,5.98678459741819E-15,-0.848048096156427));
#126220=DIRECTION('center_axis',(-1.4081690688991E-16,-6.98296267768627E-15,
1.));
#126221=DIRECTION('ref_axis',(-1.,8.91767816654029E-31,-1.4081690688991E-16));
#126222=DIRECTION('center_axis',(-1.4081690688991E-16,-6.98296267768627E-15,
1.));
#126223=DIRECTION('ref_axis',(-1.,1.21498023491345E-30,-1.4081690688991E-16));
#126224=DIRECTION('',(-1.40816906889911E-16,-6.98296267768627E-15,1.));
#126225=DIRECTION('center_axis',(-1.4081690688991E-16,-6.98296267768627E-15,
1.));
#126226=DIRECTION('ref_axis',(-1.,8.91767816654029E-31,-1.4081690688991E-16));
#126227=DIRECTION('center_axis',(-1.4081690688991E-16,-6.98296267768627E-15,
1.));
#126228=DIRECTION('ref_axis',(-1.,9.83319205199467E-31,-1.40816906889911E-16));
#126229=DIRECTION('center_axis',(-1.4081690688991E-16,-6.98296267768627E-15,
1.));
#126230=DIRECTION('ref_axis',(-1.,7.97077743482043E-31,-1.4081690688991E-16));
#126231=DIRECTION('',(-0.994521895368275,0.10452846326764,5.89872860613779E-16));
#126232=DIRECTION('center_axis',(-1.4081690688991E-16,-6.98296267768627E-15,
1.));
#126233=DIRECTION('ref_axis',(-1.,8.46073526001725E-31,-1.4081690688991E-16));
#126234=DIRECTION('',(1.,-9.83319205199467E-31,1.40816906889911E-16));
#126235=DIRECTION('center_axis',(-1.4081690688991E-16,-6.98296267768627E-15,
1.));
#126236=DIRECTION('ref_axis',(-1.,7.97077743482043E-31,-1.4081690688991E-16));
#126237=DIRECTION('center_axis',(-1.4081690688991E-16,-6.98296267768627E-15,
1.));
#126238=DIRECTION('ref_axis',(-1.,7.97077743482043E-31,-1.4081690688991E-16));
#126239=DIRECTION('center_axis',(1.4081690688991E-16,6.98296267768627E-15,
-1.));
#126240=DIRECTION('ref_axis',(1.,-7.97077743482043E-31,1.4081690688991E-16));
#126241=DIRECTION('center_axis',(1.4081690688991E-16,6.98296267768627E-15,
-1.));
#126242=DIRECTION('ref_axis',(-1.,7.97577417048809E-31,-1.40816906889911E-16));
#126243=DIRECTION('',(-0.497265611060805,0.0522695260941841,0.866022406579768));
#126244=DIRECTION('',(0.500005191251968,4.7780011719149E-6,-0.866022406579792));
#126245=DIRECTION('center_axis',(-1.4081690688991E-16,-6.98296267768627E-15,
1.));
#126246=DIRECTION('ref_axis',(-1.,9.83319205199467E-31,-1.40816906889911E-16));
#126247=DIRECTION('center_axis',(1.4081690688991E-16,6.98296267768627E-15,
-1.));
#126248=DIRECTION('ref_axis',(-1.,7.98707387273907E-31,-1.4081690688991E-16));
#126249=DIRECTION('',(-0.994521895368275,0.10452846326764,5.89872860613779E-16));
#126250=DIRECTION('center_axis',(-1.4081690688991E-16,-6.98296267768627E-15,
1.));
#126251=DIRECTION('ref_axis',(-1.,7.98248735348668E-31,-1.4081690688991E-16));
#126252=DIRECTION('',(1.,-9.83319205199467E-31,1.40816906889911E-16));
#126253=DIRECTION('center_axis',(-1.4081690688991E-16,-6.98296267768627E-15,
1.));
#126254=DIRECTION('ref_axis',(-1.,7.99150043815584E-31,-1.4081690688991E-16));
#126255=DIRECTION('center_axis',(-1.4081690688991E-16,-6.98296267768627E-15,
1.));
#126256=DIRECTION('ref_axis',(-1.,7.99858039355471E-31,-1.4081690688991E-16));
#126257=DIRECTION('',(-0.497266395846506,0.0522601510654359,-0.86602252174666));
#126258=DIRECTION('center_axis',(-1.4081690688991E-16,-6.98296267768627E-15,
1.));
#126259=DIRECTION('ref_axis',(1.,-3.37507799486047E-14,1.40816906889675E-16));
#126260=DIRECTION('',(0.500004991781248,-4.62770265895208E-6,0.866022521746645));
#126261=DIRECTION('center_axis',(-1.4081690688991E-16,-6.98296267768627E-15,
1.));
#126262=DIRECTION('ref_axis',(-1.,7.99858039355471E-31,-1.4081690688991E-16));
#126263=DIRECTION('center_axis',(-1.4081690688991E-16,-6.98296267768627E-15,
1.));
#126264=DIRECTION('ref_axis',(-1.,7.99858039355471E-31,-1.4081690688991E-16));
#126265=DIRECTION('center_axis',(-1.4081690688991E-16,-6.98296267768627E-15,
1.));
#126266=DIRECTION('ref_axis',(-1.,9.83319205199467E-31,-1.40816906889911E-16));
#126267=DIRECTION('center_axis',(1.4081690688991E-16,6.98296267768627E-15,
-1.));
#126268=DIRECTION('ref_axis',(-1.,8.01265634860448E-31,-1.4081690688991E-16));
#126269=DIRECTION('',(-0.994521895368275,0.10452846326764,5.89872860613779E-16));
#126270=DIRECTION('',(1.,-9.83319205199467E-31,1.40816906889911E-16));
#126271=DIRECTION('center_axis',(-1.4081690688991E-16,-6.98296267768627E-15,
1.));
#126272=DIRECTION('ref_axis',(-1.,8.32577322149061E-31,-1.39145123902276E-16));
#126273=DIRECTION('center_axis',(-0.103464010407632,-0.994633197962203,
-7.86457232282242E-6));
#126274=DIRECTION('ref_axis',(-0.843493966781849,0.0877379732620279,0.529924500330464));
#126275=DIRECTION('center_axis',(0.0010702559647624,0.999999427244995,-7.86457193703672E-6));
#126276=DIRECTION('ref_axis',(1.47312952164193E-6,7.86299981466101E-6,0.999999999968002));
#126277=DIRECTION('center_axis',(-1.4081690688991E-16,-6.98296267768627E-15,
1.));
#126278=DIRECTION('ref_axis',(-1.,8.07722881720021E-31,-1.42096112075504E-16));
#126279=DIRECTION('center_axis',(-0.103509373496232,-0.994628478127866,
9.77051633950369E-6));
#126280=DIRECTION('ref_axis',(0.869950553189692,-0.0905391058403728,-0.484756336027261));
#126281=DIRECTION('center_axis',(0.00102464806169094,0.999999475000305,
9.77058601219822E-6));
#126282=DIRECTION('ref_axis',(0.874641264346837,-0.000891463458120753,-0.484769908301526));
#126283=DIRECTION('center_axis',(-1.4081690688991E-16,-6.98296267768627E-15,
1.));
#126284=DIRECTION('ref_axis',(-1.,8.24049048117772E-31,-1.37719829560012E-16));
#126285=DIRECTION('center_axis',(0.107112171226385,0.994246942387259,-1.81316452017406E-5));
#126286=DIRECTION('ref_axis',(0.861994650485032,-0.092855284670664,0.498340364253106));
#126287=DIRECTION('center_axis',(0.00259831235053356,-0.999996624215829,
-1.81624798012333E-5));
#126288=DIRECTION('ref_axis',(0.865241946199119,0.00223907064273735,0.501349539842431));
#126289=DIRECTION('center_axis',(-1.4081690688991E-16,-6.98296267768627E-15,
1.));
#126290=DIRECTION('ref_axis',(-1.,8.26087817385229E-31,-1.38060560438432E-16));
#126291=DIRECTION('center_axis',(0.10712560498354,0.994245495043206,-1.85257092162474E-5));
#126292=DIRECTION('ref_axis',(0.860265387811452,-0.092699175819097,-0.501348506865306));
#126293=DIRECTION('center_axis',(0.00261182427502986,-0.999996589010146,
-1.84940601812351E-5));
#126294=DIRECTION('ref_axis',(0.866979057021848,0.00227362102099719,-0.498339387699748));
#126295=DIRECTION('center_axis',(-1.4081690688991E-16,-6.98296267768627E-15,
1.));
#126296=DIRECTION('ref_axis',(-1.,9.83319205199467E-31,-1.40816906889911E-16));
#126297=DIRECTION('center_axis',(-1.4081690688991E-16,-6.98296267768627E-15,
1.));
#126298=DIRECTION('ref_axis',(-1.,8.46073526001725E-31,-1.4081690688991E-16));
#126299=DIRECTION('',(0.994521895368275,-0.10452846326764,-5.89872860613779E-16));
#126300=DIRECTION('center_axis',(-1.4081690688991E-16,-6.98296267768627E-15,
1.));
#126301=DIRECTION('ref_axis',(-1.,7.97077743482043E-31,-1.4081690688991E-16));
#126302=DIRECTION('center_axis',(-1.4081690688991E-16,-6.98296267768627E-15,
1.));
#126303=DIRECTION('ref_axis',(-1.,7.97077743482043E-31,-1.4081690688991E-16));
#126304=DIRECTION('center_axis',(-1.4081690688991E-16,-6.98296267768627E-15,
1.));
#126305=DIRECTION('ref_axis',(-1.,7.97077743482043E-31,-1.4081690688991E-16));
#126306=DIRECTION('',(-0.978147600733808,0.207911690817747,1.31409985761785E-15));
#126307=DIRECTION('center_axis',(1.4081690688991E-16,6.98296267768627E-15,
-1.));
#126308=DIRECTION('ref_axis',(1.,-7.97077743482043E-31,1.4081690688991E-16));
#126309=DIRECTION('',(0.497266609935019,-0.0522600224406333,-0.866022406579783));
#126310=DIRECTION('center_axis',(1.4081690688991E-16,6.98296267768627E-15,
-1.));
#126311=DIRECTION('ref_axis',(-1.,7.97577417048809E-31,-1.40816906889911E-16));
#126312=DIRECTION('',(-0.489077884775291,0.103961598321232,0.866022406579773));
#126313=DIRECTION('center_axis',(-1.4081690688991E-16,-6.98296267768627E-15,
1.));
#126314=DIRECTION('ref_axis',(-1.,9.83319205199467E-31,-1.40816906889911E-16));
#126315=DIRECTION('center_axis',(-1.4081690688991E-16,-6.98296267768627E-15,
1.));
#126316=DIRECTION('ref_axis',(-1.,7.98248735348668E-31,-1.4081690688991E-16));
#126317=DIRECTION('',(0.994521895368275,-0.10452846326764,-5.89872860613779E-16));
#126318=DIRECTION('center_axis',(1.4081690688991E-16,6.98296267768627E-15,
-1.));
#126319=DIRECTION('ref_axis',(-1.,7.98707387273907E-31,-1.4081690688991E-16));
#126320=DIRECTION('',(-0.978147600733808,0.207911690817747,1.31409985761785E-15));
#126321=DIRECTION('center_axis',(-1.4081690688991E-16,-6.98296267768627E-15,
1.));
#126322=DIRECTION('ref_axis',(-1.,7.99150043815584E-31,-1.4081690688991E-16));
#126323=DIRECTION('center_axis',(-1.4081690688991E-16,-6.98296267768627E-15,
1.));
#126324=DIRECTION('ref_axis',(1.,-1.95399252334028E-14,1.40816906889774E-16));
#126325=DIRECTION('',(0.497265428393217,-0.0522693557686642,0.866022521746657));
#126326=DIRECTION('center_axis',(-1.4081690688991E-16,-6.98296267768627E-15,
1.));
#126327=DIRECTION('ref_axis',(-1.,7.99858039355471E-31,-1.4081690688991E-16));
#126328=DIRECTION('center_axis',(-1.4081690688991E-16,-6.98296267768627E-15,
1.));
#126329=DIRECTION('ref_axis',(-1.,7.99858039355471E-31,-1.4081690688991E-16));
#126330=DIRECTION('center_axis',(-1.4081690688991E-16,-6.98296267768627E-15,
1.));
#126331=DIRECTION('ref_axis',(-1.,7.99858039355471E-31,-1.4081690688991E-16));
#126332=DIRECTION('',(-0.489079645219224,0.103952356682307,-0.866022521746653));
#126333=DIRECTION('center_axis',(-1.4081690688991E-16,-6.98296267768627E-15,
1.));
#126334=DIRECTION('ref_axis',(-1.,9.83319205199467E-31,-1.40816906889911E-16));
#126335=DIRECTION('',(0.994521895368275,-0.10452846326764,-5.89872860613779E-16));
#126336=DIRECTION('center_axis',(1.4081690688991E-16,6.98296267768627E-15,
-1.));
#126337=DIRECTION('ref_axis',(-1.,8.01265634860448E-31,-1.4081690688991E-16));
#126338=DIRECTION('',(-0.978147600733808,0.207911690817747,1.31409985761785E-15));
#126339=DIRECTION('center_axis',(-1.4081690688991E-16,-6.98296267768627E-15,
1.));
#126340=DIRECTION('ref_axis',(-1.,8.32577322149061E-31,-1.39145123902276E-16));
#126341=DIRECTION('center_axis',(0.105592796389084,0.994409453539578,-7.86457209645399E-6));
#126342=DIRECTION('ref_axis',(2.28696687445887E-6,7.66594167224769E-6,0.999999999968002));
#126343=DIRECTION('center_axis',(-0.206864703430973,-0.97836955922216,-7.8645723370883E-6));
#126344=DIRECTION('ref_axis',(-0.829702103060295,0.175426463587553,0.52992450033046));
#126345=DIRECTION('center_axis',(-1.4081690688991E-16,-6.98296267768627E-15,
1.));
#126346=DIRECTION('ref_axis',(-1.,8.07722881720021E-31,-1.42096112075504E-16));
#126347=DIRECTION('center_axis',(0.105547443322659,0.994414268357301,9.77058606584058E-6));
#126348=DIRECTION('ref_axis',(0.869756704679887,-0.0923114872006333,-0.484769908302064));
#126349=DIRECTION('center_axis',(-0.206909324657823,-0.978360123509835,
9.77051813555105E-6));
#126350=DIRECTION('ref_axis',(0.855720959435949,-0.18097771758911,-0.484756336026932));
#126351=DIRECTION('center_axis',(-1.4081690688991E-16,-6.98296267768627E-15,
1.));
#126352=DIRECTION('ref_axis',(-1.,8.24049048117772E-31,-1.37719829560012E-16));
#126353=DIRECTION('center_axis',(-0.101944031878512,-0.994790135674091,
-1.81624797208528E-5));
#126354=DIRECTION('ref_axis',(0.860736106901394,-0.0882156062115827,0.501349539839177));
#126355=DIRECTION('center_axis',(0.210452504541382,0.977604082951531,-1.81316451947357E-5));
#126356=DIRECTION('ref_axis',(0.847566533384697,-0.182449589865756,0.498340364253253));
#126357=DIRECTION('center_axis',(-1.4081690688991E-16,-6.98296267768627E-15,
1.));
#126358=DIRECTION('ref_axis',(-1.,8.26087817385229E-31,-1.38060560438432E-16));
#126359=DIRECTION('center_axis',(-0.101930590292343,-0.994791513042117,
-1.84940577700706E-5));
#126360=DIRECTION('ref_axis',(0.862467313147314,-0.0883628226287556,-0.49833938769631));
#126361=DIRECTION('center_axis',(0.210465713413695,0.977601239327192,-1.85257175165895E-5));
#126362=DIRECTION('ref_axis',(0.845863061615653,-0.182113579025916,-0.501348506857821));
#126363=DIRECTION('center_axis',(-1.4081690688991E-16,-6.98296267768627E-15,
1.));
#126364=DIRECTION('ref_axis',(-1.,9.83319205199467E-31,-1.40816906889911E-16));
#126365=DIRECTION('center_axis',(-1.4081690688991E-16,-6.98296267768627E-15,
1.));
#126366=DIRECTION('ref_axis',(-1.,8.46073526001725E-31,-1.4081690688991E-16));
#126367=DIRECTION('',(0.978147600733808,-0.207911690817747,-1.31409985761785E-15));
#126368=DIRECTION('center_axis',(-1.4081690688991E-16,-6.98296267768627E-15,
1.));
#126369=DIRECTION('ref_axis',(-1.,7.97077743482043E-31,-1.4081690688991E-16));
#126370=DIRECTION('center_axis',(-1.4081690688991E-16,-6.98296267768627E-15,
1.));
#126371=DIRECTION('ref_axis',(-1.,7.97077743482043E-31,-1.4081690688991E-16));
#126372=DIRECTION('center_axis',(-1.4081690688991E-16,-6.98296267768627E-15,
1.));
#126373=DIRECTION('ref_axis',(-1.,7.97077743482043E-31,-1.4081690688991E-16));
#126374=DIRECTION('',(-0.951056516295158,0.309016994374935,2.02392930158878E-15));
#126375=DIRECTION('center_axis',(1.4081690688991E-16,6.98296267768627E-15,
-1.));
#126376=DIRECTION('ref_axis',(1.,-7.97077743482043E-31,1.4081690688991E-16));
#126377=DIRECTION('',(0.489079871579877,-0.103952251140467,-0.866022406579784));
#126378=DIRECTION('center_axis',(1.4081690688991E-16,6.98296267768627E-15,
-1.));
#126379=DIRECTION('ref_axis',(-1.,7.97577417048809E-31,-1.40816906889911E-16));
#126380=DIRECTION('',(-0.475531718838029,0.154514645521697,0.866022406579792));
#126381=DIRECTION('center_axis',(-1.4081690688991E-16,-6.98296267768627E-15,
1.));
#126382=DIRECTION('ref_axis',(-1.,9.83319205199467E-31,-1.40816906889911E-16));
#126383=DIRECTION('center_axis',(-1.4081690688991E-16,-6.98296267768627E-15,
1.));
#126384=DIRECTION('ref_axis',(-1.,7.98248735348668E-31,-1.4081690688991E-16));
#126385=DIRECTION('',(0.978147600733808,-0.207911690817747,-1.31409985761785E-15));
#126386=DIRECTION('center_axis',(1.4081690688991E-16,6.98296267768627E-15,
-1.));
#126387=DIRECTION('ref_axis',(-1.,7.98707387273907E-31,-1.4081690688991E-16));
#126388=DIRECTION('',(-0.951056516295158,0.309016994374935,2.02392930158878E-15));
#126389=DIRECTION('center_axis',(-1.4081690688991E-16,-6.98296267768627E-15,
1.));
#126390=DIRECTION('ref_axis',(-1.,7.99150043815584E-31,-1.4081690688991E-16));
#126391=DIRECTION('center_axis',(-1.4081690688991E-16,-6.98296267768627E-15,
1.));
#126392=DIRECTION('ref_axis',(1.,-1.4210854715202E-14,1.40816906889811E-16));
#126393=DIRECTION('',(0.489077720912262,-0.103961409834802,0.866022521746651));
#126394=DIRECTION('center_axis',(-1.4081690688991E-16,-6.98296267768627E-15,
1.));
#126395=DIRECTION('ref_axis',(-1.,7.99858039355471E-31,-1.4081690688991E-16));
#126396=DIRECTION('center_axis',(-1.4081690688991E-16,-6.98296267768627E-15,
1.));
#126397=DIRECTION('ref_axis',(-1.,7.99858039355471E-31,-1.4081690688991E-16));
#126398=DIRECTION('center_axis',(-1.4081690688991E-16,-6.98296267768627E-15,
1.));
#126399=DIRECTION('ref_axis',(-1.,7.99858039355471E-31,-1.4081690688991E-16));
#126400=DIRECTION('',(-0.475534435652402,0.154505638525938,-0.86602252174666));
#126401=DIRECTION('center_axis',(-1.4081690688991E-16,-6.98296267768627E-15,
1.));
#126402=DIRECTION('ref_axis',(-1.,9.83319205199467E-31,-1.40816906889911E-16));
#126403=DIRECTION('',(0.978147600733808,-0.207911690817747,-1.31409985761785E-15));
#126404=DIRECTION('center_axis',(1.4081690688991E-16,6.98296267768627E-15,
-1.));
#126405=DIRECTION('ref_axis',(-1.,8.01265634860448E-31,-1.4081690688991E-16));
#126406=DIRECTION('',(-0.951056516295158,0.309016994374935,2.02392930158878E-15));
#126407=DIRECTION('center_axis',(-1.4081690688991E-16,-6.98296267768627E-15,
1.));
#126408=DIRECTION('ref_axis',(-1.,8.32577322149061E-31,-1.39145123902276E-16));
#126409=DIRECTION('center_axis',(0.20895844003943,0.977924521767624,-7.86457210795472E-6));
#126410=DIRECTION('ref_axis',(3.07574773432243E-6,7.38489372014646E-6,0.999999999968002));
#126411=DIRECTION('center_axis',(-0.307998943474314,-0.951386698854286,
-7.86457232392837E-6));
#126412=DIRECTION('ref_axis',(-0.806819849471267,0.261192944867688,0.529924500330479));
#126413=DIRECTION('center_axis',(-1.4081690688991E-16,-6.98296267768627E-15,
1.));
#126414=DIRECTION('ref_axis',(-1.,8.07722881720021E-31,-1.42096112075504E-16));
#126415=DIRECTION('center_axis',(0.208913838706166,0.977934050895862,9.77058399236075E-6));
#126416=DIRECTION('ref_axis',(0.855342908547872,-0.182720126971788,-0.484769908303187));
#126417=DIRECTION('center_axis',(-0.308042333963518,-0.951372650642663,
9.77051317041121E-6));
#126418=DIRECTION('ref_axis',(0.832115907779501,-0.269433499591963,-0.484756336026591));
#126419=DIRECTION('center_axis',(-1.4081690688991E-16,-6.98296267768627E-15,
1.));
#126420=DIRECTION('ref_axis',(-1.,8.24049048117772E-31,-1.37719829560012E-16));
#126421=DIRECTION('center_axis',(-0.205369455961149,-0.978684518232687,
-1.81624796820396E-5));
#126422=DIRECTION('ref_axis',(0.846799862691371,-0.177703774423439,0.50134953984375));
#126423=DIRECTION('center_axis',(0.311487076176625,0.950250388606172,-1.81316452791439E-5));
#126424=DIRECTION('ref_axis',(0.823852299981103,-0.270044939174595,0.498340364251217));
#126425=DIRECTION('center_axis',(-1.4081690688991E-16,-6.98296267768627E-15,
1.));
#126426=DIRECTION('ref_axis',(-1.,8.26087817385229E-31,-1.38060560438432E-16));
#126427=DIRECTION('center_axis',(-0.205356231986263,-0.978687293083125,
-1.84940625565383E-5));
#126428=DIRECTION('ref_axis',(0.848506196903525,-0.17803114470241,-0.498339387699052));
#126429=DIRECTION('center_axis',(0.311499915448438,0.950246179856785,-1.85257197232984E-5));
#126430=DIRECTION('ref_axis',(0.822193282701967,-0.269532707749963,-0.501348506861979));
#126431=DIRECTION('center_axis',(-1.4081690688991E-16,-6.98296267768627E-15,
1.));
#126432=DIRECTION('ref_axis',(-1.,9.83319205199467E-31,-1.40816906889911E-16));
#126433=DIRECTION('center_axis',(-1.4081690688991E-16,-6.98296267768627E-15,
1.));
#126434=DIRECTION('ref_axis',(-1.,8.46073526001725E-31,-1.4081690688991E-16));
#126435=DIRECTION('',(0.951056516295158,-0.309016994374935,-2.02392930158878E-15));
#126436=DIRECTION('center_axis',(-1.4081690688991E-16,-6.98296267768627E-15,
1.));
#126437=DIRECTION('ref_axis',(-1.,7.97077743482043E-31,-1.4081690688991E-16));
#126438=DIRECTION('center_axis',(-1.4081690688991E-16,-6.98296267768627E-15,
1.));
#126439=DIRECTION('ref_axis',(-1.,7.97077743482043E-31,-1.4081690688991E-16));
#126440=DIRECTION('center_axis',(-1.4081690688991E-16,-6.98296267768627E-15,
1.));
#126441=DIRECTION('ref_axis',(-1.,7.97077743482043E-31,-1.4081690688991E-16));
#126442=DIRECTION('',(-0.913545457642606,0.406736643075789,2.71158415259707E-15));
#126443=DIRECTION('center_axis',(1.4081690688991E-16,6.98296267768627E-15,
-1.));
#126444=DIRECTION('ref_axis',(1.,-7.97077743482043E-31,1.4081690688991E-16));
#126445=DIRECTION('',(0.475534671805145,-0.154505557223404,-0.866022406579794));
#126446=DIRECTION('center_axis',(1.4081690688991E-16,6.98296267768627E-15,
-1.));
#126447=DIRECTION('ref_axis',(-1.,7.97577417048809E-31,-1.40816906889911E-16));
#126448=DIRECTION('',(-0.456775527877826,0.203374797931553,0.86602240657978));
#126449=DIRECTION('center_axis',(-1.4081690688991E-16,-6.98296267768627E-15,
1.));
#126450=DIRECTION('ref_axis',(-1.,9.83319205199467E-31,-1.40816906889911E-16));
#126451=DIRECTION('center_axis',(-1.4081690688991E-16,-6.98296267768627E-15,
1.));
#126452=DIRECTION('ref_axis',(-1.,7.98248735348668E-31,-1.4081690688991E-16));
#126453=DIRECTION('',(0.951056516295158,-0.309016994374935,-2.02392930158878E-15));
#126454=DIRECTION('center_axis',(1.4081690688991E-16,6.98296267768627E-15,
-1.));
#126455=DIRECTION('ref_axis',(-1.,7.98707387273907E-31,-1.4081690688991E-16));
#126456=DIRECTION('',(-0.913545457642606,0.406736643075789,2.71158415259707E-15));
#126457=DIRECTION('center_axis',(-1.4081690688991E-16,-6.98296267768627E-15,
1.));
#126458=DIRECTION('ref_axis',(-1.,7.99150043815584E-31,-1.4081690688991E-16));
#126459=DIRECTION('center_axis',(-1.4081690688991E-16,-6.98296267768627E-15,
1.));
#126460=DIRECTION('ref_axis',(1.,-2.04281036531029E-14,1.40816906889768E-16));
#126461=DIRECTION('',(0.47553157557488,-0.154514440939486,0.866022521746652));
#126462=DIRECTION('center_axis',(-1.4081690688991E-16,-6.98296267768627E-15,
1.));
#126463=DIRECTION('ref_axis',(-1.,7.99858039355471E-31,-1.4081690688991E-16));
#126464=DIRECTION('center_axis',(-1.4081690688991E-16,-6.98296267768627E-15,
1.));
#126465=DIRECTION('ref_axis',(-1.,7.99858039355471E-31,-1.4081690688991E-16));
#126466=DIRECTION('center_axis',(-1.4081690688991E-16,-6.98296267768627E-15,
1.));
#126467=DIRECTION('ref_axis',(-1.,7.99858039355471E-31,-1.4081690688991E-16));
#126468=DIRECTION('',(-0.456779171296626,0.203366124261497,-0.866022521746649));
#126469=DIRECTION('center_axis',(-1.4081690688991E-16,-6.98296267768627E-15,
1.));
#126470=DIRECTION('ref_axis',(-1.,9.83319205199467E-31,-1.40816906889911E-16));
#126471=DIRECTION('',(0.951056516295158,-0.309016994374935,-2.02392930158878E-15));
#126472=DIRECTION('center_axis',(1.4081690688991E-16,6.98296267768627E-15,
-1.));
#126473=DIRECTION('ref_axis',(-1.,8.01265634860448E-31,-1.4081690688991E-16));
#126474=DIRECTION('',(-0.913545457642606,0.406736643075789,2.71158415259707E-15));
#126475=DIRECTION('center_axis',(-1.4081690688991E-16,-6.98296267768627E-15,
1.));
#126476=DIRECTION('ref_axis',(-1.,8.32577322149061E-31,-1.39145123902276E-16));
#126477=DIRECTION('center_axis',(0.310034691293364,0.950725244291313,-7.86457215694468E-6));
#126478=DIRECTION('ref_axis',(3.83083003964029E-6,7.02293537238877E-6,0.999999999968002));
#126479=DIRECTION('center_axis',(-0.40575868264004,-0.913980246723291,-7.86457230346941E-6));
#126480=DIRECTION('ref_axis',(-0.775097908773545,0.344097741585733,0.529924500330449));
#126481=DIRECTION('center_axis',(-1.4081690688991E-16,-6.98296267768627E-15,
1.));
#126482=DIRECTION('ref_axis',(-1.,8.07722881720021E-31,-1.42096112075504E-16));
#126483=DIRECTION('center_axis',(0.309991330354408,0.950739383327335,9.77058099945129E-6));
#126484=DIRECTION('ref_axis',(0.831557796517697,-0.271126846795087,-0.484769908304534));
#126485=DIRECTION('center_axis',(-0.405800366994072,-0.913961739927889,
9.77051230122167E-6));
#126486=DIRECTION('ref_axis',(0.799394020106066,-0.354937311790806,-0.484756336026027));
#126487=DIRECTION('center_axis',(-1.4081690688991E-16,-6.98296267768627E-15,
1.));
#126488=DIRECTION('ref_axis',(-1.,8.24049048117772E-31,-1.37719829560012E-16));
#126489=DIRECTION('center_axis',(-0.306544809307814,-0.951856228406665,
-1.81624799272238E-5));
#126490=DIRECTION('ref_axis',(0.823585901983193,-0.265244982895809,0.501349539845338));
#126491=DIRECTION('center_axis',(0.409108930222443,0.912485552150549,-1.81316453655189E-5));
#126492=DIRECTION('ref_axis',(0.79111176837416,-0.354681619618438,0.498340364253942));
#126493=DIRECTION('center_axis',(-1.4081690688991E-16,-6.98296267768627E-15,
1.));
#126494=DIRECTION('ref_axis',(-1.,8.26087817385229E-31,-1.38060560438432E-16));
#126495=DIRECTION('center_axis',(-0.306531947828723,-0.951860370337109,
-1.84940671421675E-5));
#126496=DIRECTION('ref_axis',(0.825248669206747,-0.265748920299438,-0.498339387698962));
#126497=DIRECTION('center_axis',(0.409121259222292,0.912480024389117,-1.85257252778069E-5));
#126498=DIRECTION('ref_axis',(0.789515382127622,-0.353998779723841,-0.501348506867137));
#126499=DIRECTION('center_axis',(-1.4081690688991E-16,-6.98296267768627E-15,
1.));
#126500=DIRECTION('ref_axis',(-1.,9.83319205199467E-31,-1.40816906889911E-16));
#126501=DIRECTION('center_axis',(-1.4081690688991E-16,-6.98296267768627E-15,
1.));
#126502=DIRECTION('ref_axis',(-1.,8.46073526001725E-31,-1.4081690688991E-16));
#126503=DIRECTION('',(0.913545457642606,-0.406736643075789,-2.71158415259707E-15));
#126504=DIRECTION('center_axis',(-1.4081690688991E-16,-6.98296267768627E-15,
1.));
#126505=DIRECTION('ref_axis',(-1.,7.97077743482043E-31,-1.4081690688991E-16));
#126506=DIRECTION('center_axis',(-1.4081690688991E-16,-6.98296267768627E-15,
1.));
#126507=DIRECTION('ref_axis',(-1.,7.97077743482043E-31,-1.4081690688991E-16));
#126508=DIRECTION('center_axis',(-1.4081690688991E-16,-6.98296267768627E-15,
1.));
#126509=DIRECTION('ref_axis',(-1.,7.97077743482043E-31,-1.4081690688991E-16));
#126510=DIRECTION('',(-0.866025403784445,0.499999999999989,3.36953032019404E-15));
#126511=DIRECTION('center_axis',(1.4081690688991E-16,6.98296267768627E-15,
-1.));
#126512=DIRECTION('ref_axis',(1.,-7.97077743482043E-31,1.4081690688991E-16));
#126513=DIRECTION('',(0.456779414654135,-0.203366068089035,-0.866022406579779));
#126514=DIRECTION('center_axis',(1.4081690688991E-16,6.98296267768627E-15,
-1.));
#126515=DIRECTION('ref_axis',(-1.,7.97577417048809E-31,-1.40816906889911E-16));
#126516=DIRECTION('',(-0.433014808647732,0.250006733496379,0.866022406579783));
#126517=DIRECTION('center_axis',(-1.4081690688991E-16,-6.98296267768627E-15,
1.));
#126518=DIRECTION('ref_axis',(-1.,9.83319205199467E-31,-1.40816906889911E-16));
#126519=DIRECTION('center_axis',(-1.4081690688991E-16,-6.98296267768627E-15,
1.));
#126520=DIRECTION('ref_axis',(-1.,7.98248735348668E-31,-1.4081690688991E-16));
#126521=DIRECTION('',(0.913545457642606,-0.406736643075789,-2.71158415259707E-15));
#126522=DIRECTION('center_axis',(1.4081690688991E-16,6.98296267768627E-15,
-1.));
#126523=DIRECTION('ref_axis',(-1.,7.98707387273907E-31,-1.4081690688991E-16));
#126524=DIRECTION('',(-0.866025403784445,0.499999999999989,3.36953032019404E-15));
#126525=DIRECTION('center_axis',(-1.4081690688991E-16,-6.98296267768627E-15,
1.));
#126526=DIRECTION('ref_axis',(-1.,7.99150043815584E-31,-1.4081690688991E-16));
#126527=DIRECTION('center_axis',(-1.4081690688991E-16,-6.98296267768627E-15,
1.));
#126528=DIRECTION('ref_axis',(1.,-2.48689957516035E-14,1.40816906889737E-16));
#126529=DIRECTION('',(0.456775406784114,-0.203374579494981,0.866022521746661));
#126530=DIRECTION('center_axis',(-1.4081690688991E-16,-6.98296267768627E-15,
1.));
#126531=DIRECTION('ref_axis',(-1.,7.99858039355471E-31,-1.4081690688991E-16));
#126532=DIRECTION('center_axis',(-1.4081690688991E-16,-6.98296267768627E-15,
1.));
#126533=DIRECTION('ref_axis',(-1.,7.99858039355471E-31,-1.4081690688991E-16));
#126534=DIRECTION('center_axis',(-1.4081690688991E-16,-6.98296267768627E-15,
1.));
#126535=DIRECTION('ref_axis',(-1.,7.99858039355471E-31,-1.4081690688991E-16));
#126536=DIRECTION('',(-0.433019338752907,0.249998488182543,-0.866022521746657));
#126537=DIRECTION('center_axis',(-1.4081690688991E-16,-6.98296267768627E-15,
1.));
#126538=DIRECTION('ref_axis',(-1.,9.83319205199467E-31,-1.40816906889911E-16));
#126539=DIRECTION('',(0.913545457642606,-0.406736643075789,-2.71158415259707E-15));
#126540=DIRECTION('center_axis',(1.4081690688991E-16,6.98296267768627E-15,
-1.));
#126541=DIRECTION('ref_axis',(-1.,8.01265634860448E-31,-1.4081690688991E-16));
#126542=DIRECTION('',(-0.866025403784445,0.499999999999989,3.36953032019404E-15));
#126543=DIRECTION('center_axis',(-1.4081690688991E-16,-6.98296267768627E-15,
1.));
#126544=DIRECTION('ref_axis',(-1.,8.32577322149061E-31,-1.39145123902276E-16));
#126545=DIRECTION('center_axis',(0.407714137590522,0.913109622086508,-7.86457213947159E-6));
#126546=DIRECTION('ref_axis',(4.54394101111081E-6,6.58403219129901E-6,0.999999999968002));
#126547=DIRECTION('center_axis',(-0.499072844768375,-0.866560035746485,
-7.86457220438562E-6));
#126548=DIRECTION('ref_axis',(-0.734883833187544,0.423232531439973,0.529924500330466));
#126549=DIRECTION('center_axis',(-1.4081690688991E-16,-6.98296267768627E-15,
1.));
#126550=DIRECTION('ref_axis',(-1.,8.07722881720021E-31,-1.42096112075504E-16));
#126551=DIRECTION('center_axis',(0.4076724921206,0.913128216119026,9.77058401138E-6));
#126552=DIRECTION('ref_axis',(0.79866196325535,-0.356563044148319,-0.484769908303717));
#126553=DIRECTION('center_axis',(-0.499112366283222,-0.866537273132379,
9.77051426432124E-6));
#126554=DIRECTION('ref_axis',(0.757913804264544,-0.436552356526389,-0.484756336025125));
#126555=DIRECTION('center_axis',(-1.4081690688991E-16,-6.98296267768627E-15,
1.));
#126556=DIRECTION('ref_axis',(-1.,8.24049048117772E-31,-1.37719829560012E-16));
#126557=DIRECTION('center_axis',(-0.404361593575263,-0.914599202553445,
-1.81624797807593E-5));
#126558=DIRECTION('ref_axis',(0.791348561789699,-0.349880111830686,0.50134953984094));
#126559=DIRECTION('center_axis',(0.502248501217129,0.864723333035712,-1.81316454324455E-5));
#126560=DIRECTION('ref_axis',(0.749703650686919,-0.435432334018187,0.498340364247348));
#126561=DIRECTION('center_axis',(-1.4081690688991E-16,-6.98296267768627E-15,
1.));
#126562=DIRECTION('ref_axis',(-1.,8.26087817385229E-31,-1.38060560438432E-16));
#126563=DIRECTION('center_axis',(-0.404349235492276,-0.914604666189049,
-1.84940481536951E-5));
#126564=DIRECTION('ref_axis',(0.792949544396744,-0.350555095114578,-0.498339387696984));
#126565=DIRECTION('center_axis',(0.502260184874678,0.864716546821242,-1.85257139420342E-5));
#126566=DIRECTION('ref_axis',(0.74818738581782,-0.434586366991852,-0.501348506857176));
#126567=DIRECTION('center_axis',(-1.4081690688991E-16,-6.98296267768627E-15,
1.));
#126568=DIRECTION('ref_axis',(-1.,9.83319205199467E-31,-1.40816906889911E-16));
#126569=DIRECTION('center_axis',(-1.4081690688991E-16,-6.98296267768627E-15,
1.));
#126570=DIRECTION('ref_axis',(-1.,8.46073526001725E-31,-1.4081690688991E-16));
#126571=DIRECTION('',(0.866025403784445,-0.499999999999989,-3.36953032019404E-15));
#126572=DIRECTION('center_axis',(-1.4081690688991E-16,-6.98296267768627E-15,
1.));
#126573=DIRECTION('ref_axis',(-1.,7.97077743482043E-31,-1.4081690688991E-16));
#126574=DIRECTION('center_axis',(-1.4081690688991E-16,-6.98296267768627E-15,
1.));
#126575=DIRECTION('ref_axis',(-1.,7.97077743482043E-31,-1.4081690688991E-16));
#126576=DIRECTION('center_axis',(-1.4081690688991E-16,-6.98296267768627E-15,
1.));
#126577=DIRECTION('ref_axis',(-1.,7.97077743482043E-31,-1.4081690688991E-16));
#126578=DIRECTION('',(-0.809016994374955,0.587785252292463,3.99055920848342E-15));
#126579=DIRECTION('center_axis',(1.4081690688991E-16,6.98296267768627E-15,
-1.));
#126580=DIRECTION('ref_axis',(1.,-7.97077743482043E-31,1.4081690688991E-16));
#126581=DIRECTION('',(0.433019586648926,-0.249998457755604,-0.866022406579768));
#126582=DIRECTION('center_axis',(1.4081690688991E-16,6.98296267768627E-15,
-1.));
#126583=DIRECTION('ref_axis',(-1.,7.97577417048809E-31,-1.40816906889911E-16));
#126584=DIRECTION('',(-0.404509888559958,0.29389954297172,0.866022406579775));
#126585=DIRECTION('center_axis',(-1.4081690688991E-16,-6.98296267768627E-15,
1.));
#126586=DIRECTION('ref_axis',(-1.,9.83319205199467E-31,-1.40816906889911E-16));
#126587=DIRECTION('center_axis',(-1.4081690688991E-16,-6.98296267768627E-15,
1.));
#126588=DIRECTION('ref_axis',(-1.,7.98248735348668E-31,-1.4081690688991E-16));
#126589=DIRECTION('',(0.866025403784445,-0.499999999999989,-3.36953032019404E-15));
#126590=DIRECTION('center_axis',(1.4081690688991E-16,6.98296267768627E-15,
-1.));
#126591=DIRECTION('ref_axis',(-1.,7.98707387273907E-31,-1.4081690688991E-16));
#126592=DIRECTION('',(-0.809016994374955,0.587785252292463,3.99055920848342E-15));
#126593=DIRECTION('center_axis',(-1.4081690688991E-16,-6.98296267768627E-15,
1.));
#126594=DIRECTION('ref_axis',(-1.,7.99150043815584E-31,-1.4081690688991E-16));
#126595=DIRECTION('center_axis',(-1.4081690688991E-16,-6.98296267768627E-15,
1.));
#126596=DIRECTION('ref_axis',(1.,2.66453525910038E-14,1.40816906890097E-16));
#126597=DIRECTION('',(0.433014711050254,-0.250006503598669,0.866022521746654));
#126598=DIRECTION('center_axis',(-1.4081690688991E-16,-6.98296267768627E-15,
1.));
#126599=DIRECTION('ref_axis',(-1.,7.99858039355471E-31,-1.4081690688991E-16));
#126600=DIRECTION('center_axis',(-1.4081690688991E-16,-6.98296267768627E-15,
1.));
#126601=DIRECTION('ref_axis',(-1.,7.99858039355471E-31,-1.4081690688991E-16));
#126602=DIRECTION('center_axis',(-1.4081690688991E-16,-6.98296267768627E-15,
1.));
#126603=DIRECTION('ref_axis',(-1.,7.99858039355471E-31,-1.4081690688991E-16));
#126604=DIRECTION('',(-0.404515255718701,0.293891816351536,-0.866022521746651));
#126605=DIRECTION('center_axis',(-1.4081690688991E-16,-6.98296267768627E-15,
1.));
#126606=DIRECTION('ref_axis',(-1.,9.83319205199467E-31,-1.40816906889911E-16));
#126607=DIRECTION('',(0.866025403784445,-0.499999999999989,-3.36953032019404E-15));
#126608=DIRECTION('center_axis',(1.4081690688991E-16,6.98296267768627E-15,
-1.));
#126609=DIRECTION('ref_axis',(-1.,8.01265634860448E-31,-1.4081690688991E-16));
#126610=DIRECTION('',(-0.809016994374955,0.587785252292463,3.99055920848342E-15));
#126611=DIRECTION('center_axis',(-1.4081690688991E-16,-6.98296267768627E-15,
1.));
#126612=DIRECTION('ref_axis',(-1.,8.32577322149061E-31,-1.39145123902276E-16));
#126613=DIRECTION('center_axis',(0.500926582476573,0.865489779781651,-7.86457212410024E-6));
#126614=DIRECTION('ref_axis',(5.20726760504278E-6,6.07299298703026E-6,0.999999999968002));
#126615=DIRECTION('center_axis',(-0.586919060371635,-0.809645611678731,
-7.86457216103576E-6));
#126616=DIRECTION('ref_axis',(-0.686618216540855,0.49773029711256,0.529924500330469));
#126617=DIRECTION('center_axis',(-1.4081690688991E-16,-6.98296267768627E-15,
1.));
#126618=DIRECTION('ref_axis',(-1.,8.07722881720021E-31,-1.42096112075504E-16));
#126619=DIRECTION('center_axis',(0.500887108754422,0.865512625088838,9.77059208168159E-6));
#126620=DIRECTION('ref_axis',(0.757015822392275,-0.438092662174016,-0.484769908303961));
#126621=DIRECTION('center_axis',(-0.586955986038978,-0.809618842639886,
9.77052194850957E-6));
#126622=DIRECTION('ref_axis',(0.708129726178852,-0.513384442288873,-0.484756336026264));
#126623=DIRECTION('center_axis',(-1.4081690688991E-16,-6.98296267768627E-15,
1.));
#126624=DIRECTION('ref_axis',(-1.,8.24049048117772E-31,-1.37719829560012E-16));
#126625=DIRECTION('center_axis',(-0.497748107605237,-0.867321636444941,
-1.81624800435674E-5));
#126626=DIRECTION('ref_axis',(0.750441041150478,-0.4306818810425,0.501349539840898));
#126627=DIRECTION('center_axis',(0.589885332530148,0.807487024129206,-1.81316451594575E-5));
#126628=DIRECTION('ref_axis',(0.700081622910561,-0.511412360642604,0.498340364254066));
#126629=DIRECTION('center_axis',(-1.4081690688991E-16,-6.98296267768627E-15,
1.));
#126630=DIRECTION('ref_axis',(-1.,8.26087817385229E-31,-1.38060560438432E-16));
#126631=DIRECTION('center_axis',(-0.497736388324913,-0.867328361922543,
-1.84940447271398E-5));
#126632=DIRECTION('ref_axis',(0.751962698441535,-0.43152051494869,-0.498339387697724));
#126633=DIRECTION('center_axis',(0.589896242833519,0.807479053813593,-1.85257084974504E-5));
#126634=DIRECTION('ref_axis',(0.698662091932916,-0.510412535075953,-0.501348506862502));
#126635=DIRECTION('center_axis',(-1.4081690688991E-16,-6.98296267768627E-15,
1.));
#126636=DIRECTION('ref_axis',(-1.,9.83319205199467E-31,-1.40816906889911E-16));
#126637=DIRECTION('center_axis',(-1.4081690688991E-16,-6.98296267768627E-15,
1.));
#126638=DIRECTION('ref_axis',(-1.,8.46073526001725E-31,-1.4081690688991E-16));
#126639=DIRECTION('',(0.809016994374955,-0.587785252292463,-3.99055920848342E-15));
#126640=DIRECTION('center_axis',(-1.4081690688991E-16,-6.98296267768627E-15,
1.));
#126641=DIRECTION('ref_axis',(-1.,7.97077743482043E-31,-1.4081690688991E-16));
#126642=DIRECTION('center_axis',(-1.4081690688991E-16,-6.98296267768627E-15,
1.));
#126643=DIRECTION('ref_axis',(-1.,7.97077743482043E-31,-1.4081690688991E-16));
#126644=DIRECTION('center_axis',(-1.4081690688991E-16,-6.98296267768627E-15,
1.));
#126645=DIRECTION('ref_axis',(-1.,7.97077743482043E-31,-1.4081690688991E-16));
#126646=DIRECTION('',(-0.743144825477402,0.66913060635885,4.56786669500646E-15));
#126647=DIRECTION('center_axis',(1.4081690688991E-16,6.98296267768627E-15,
-1.));
#126648=DIRECTION('ref_axis',(1.,-7.97077743482043E-31,1.4081690688991E-16));
#126649=DIRECTION('',(0.404515505437167,-0.293891812003452,-0.866022406579784));
#126650=DIRECTION('center_axis',(1.4081690688991E-16,6.98296267768627E-15,
-1.));
#126651=DIRECTION('ref_axis',(-1.,7.97577417048809E-31,-1.40816906889911E-16));
#126652=DIRECTION('',(-0.371573073483921,0.33457232755186,0.866022406579786));
#126653=DIRECTION('center_axis',(-1.4081690688991E-16,-6.98296267768627E-15,
1.));
#126654=DIRECTION('ref_axis',(-1.,9.83319205199467E-31,-1.40816906889911E-16));
#126655=DIRECTION('center_axis',(-1.4081690688991E-16,-6.98296267768627E-15,
1.));
#126656=DIRECTION('ref_axis',(-1.,7.98248735348668E-31,-1.4081690688991E-16));
#126657=DIRECTION('',(0.809016994374955,-0.587785252292463,-3.99055920848342E-15));
#126658=DIRECTION('center_axis',(1.4081690688991E-16,6.98296267768627E-15,
-1.));
#126659=DIRECTION('ref_axis',(-1.,7.98707387273907E-31,-1.4081690688991E-16));
#126660=DIRECTION('',(-0.743144825477402,0.66913060635885,4.56786669500646E-15));
#126661=DIRECTION('center_axis',(-1.4081690688991E-16,-6.98296267768627E-15,
1.));
#126662=DIRECTION('ref_axis',(-1.,7.99150043815584E-31,-1.4081690688991E-16));
#126663=DIRECTION('center_axis',(-1.4081690688991E-16,-6.98296267768627E-15,
1.));
#126664=DIRECTION('ref_axis',(1.,-1.95399252334028E-14,1.40816906889774E-16));
#126665=DIRECTION('',(0.404509815527881,-0.293899304131704,0.866022521746692));
#126666=DIRECTION('center_axis',(-1.4081690688991E-16,-6.98296267768627E-15,
1.));
#126667=DIRECTION('ref_axis',(-1.,7.99858039355471E-31,-1.4081690688991E-16));
#126668=DIRECTION('center_axis',(-1.4081690688991E-16,-6.98296267768627E-15,
1.));
#126669=DIRECTION('ref_axis',(-1.,7.99858039355471E-31,-1.4081690688991E-16));
#126670=DIRECTION('center_axis',(-1.4081690688991E-16,-6.98296267768627E-15,
1.));
#126671=DIRECTION('ref_axis',(-1.,7.99858039355471E-31,-1.4081690688991E-16));
#126672=DIRECTION('',(-0.371579218892574,0.334565204279747,-0.866022521746655));
#126673=DIRECTION('center_axis',(-1.4081690688991E-16,-6.98296267768627E-15,
1.));
#126674=DIRECTION('ref_axis',(-1.,9.83319205199467E-31,-1.40816906889911E-16));
#126675=DIRECTION('',(0.809016994374955,-0.587785252292463,-3.99055920848342E-15));
#126676=DIRECTION('center_axis',(1.4081690688991E-16,6.98296267768627E-15,
-1.));
#126677=DIRECTION('ref_axis',(-1.,8.01265634860448E-31,-1.4081690688991E-16));
#126678=DIRECTION('',(-0.743144825477402,0.66913060635885,4.56786669500646E-15));
#126679=DIRECTION('center_axis',(-1.4081690688991E-16,-6.98296267768627E-15,
1.));
#126680=DIRECTION('ref_axis',(-1.,8.32577322149061E-31,-1.39145123902276E-16));
#126681=DIRECTION('center_axis',(0.588650770899369,0.808387450334137,-7.86457205642189E-6));
#126682=DIRECTION('ref_axis',(5.81354222511562E-6,5.49541676348314E-6,0.999999999968002));
#126683=DIRECTION('center_axis',(-0.668334867928742,-0.743860540860193,
-7.86457217696032E-6));
#126684=DIRECTION('ref_axis',(-0.63082986702967,0.566774825493184,0.529924500330471));
#126685=DIRECTION('center_axis',(-1.4081690688991E-16,-6.98296267768627E-15,
1.));
#126686=DIRECTION('ref_axis',(-1.,8.07722881720021E-31,-1.42096112075504E-16));
#126687=DIRECTION('center_axis',(0.588613901402471,0.808414296620426,9.77059026348027E-6));
#126688=DIRECTION('ref_axis',(0.707075657763682,-0.514822445316384,-0.484769908303429));
#126689=DIRECTION('center_axis',(-0.66836879318871,-0.743830058680075,9.77051759200369E-6));
#126690=DIRECTION('ref_axis',(0.650587230627419,-0.584591780668772,-0.484756336027762));
#126691=DIRECTION('center_axis',(-1.4081690688991E-16,-6.98296267768627E-15,
1.));
#126692=DIRECTION('ref_axis',(-1.,8.24049048117772E-31,-1.37719829560012E-16));
#126693=DIRECTION('center_axis',(-0.585681189207855,-0.810541512988815,
-1.81624800237498E-5));
#126694=DIRECTION('ref_axis',(0.701311531421822,-0.506765009437568,0.501349539846722));
#126695=DIRECTION('center_axis',(0.671059256698578,0.7414037184088,-1.81316451876482E-5));
#126696=DIRECTION('ref_axis',(0.642789354375964,-0.581789246426184,0.498340364252971));
#126697=DIRECTION('center_axis',(-1.4081690688991E-16,-6.98296267768627E-15,
1.));
#126698=DIRECTION('ref_axis',(-1.,8.26087817385229E-31,-1.38060560438432E-16));
#126699=DIRECTION('center_axis',(-0.585670237138178,-0.810549426616589,
-1.84940603684897E-5));
#126700=DIRECTION('ref_axis',(0.70273719180265,-0.507758105718623,-0.498339387701155));
#126701=DIRECTION('center_axis',(0.671069274107353,0.741394651319949,-1.85257130833385E-5));
#126702=DIRECTION('ref_axis',(0.641482109969085,-0.580646516618343,-0.501348506857849));
#126703=DIRECTION('center_axis',(-1.4081690688991E-16,-6.98296267768627E-15,
1.));
#126704=DIRECTION('ref_axis',(-1.,9.83319205199467E-31,-1.40816906889911E-16));
#126705=DIRECTION('center_axis',(-1.4081690688991E-16,-6.98296267768627E-15,
1.));
#126706=DIRECTION('ref_axis',(-1.,8.46073526001725E-31,-1.4081690688991E-16));
#126707=DIRECTION('',(0.743144825477402,-0.66913060635885,-4.56786669500646E-15));
#126708=DIRECTION('center_axis',(-1.4081690688991E-16,-6.98296267768627E-15,
1.));
#126709=DIRECTION('ref_axis',(-1.,7.97077743482043E-31,-1.4081690688991E-16));
#126710=DIRECTION('center_axis',(-1.4081690688991E-16,-6.98296267768627E-15,
1.));
#126711=DIRECTION('ref_axis',(-1.,7.97077743482043E-31,-1.4081690688991E-16));
#126712=DIRECTION('center_axis',(-1.4081690688991E-16,-6.98296267768627E-15,
1.));
#126713=DIRECTION('ref_axis',(-1.,7.97077743482043E-31,-1.4081690688991E-16));
#126714=DIRECTION('',(-0.669130606358867,0.743144825477386,5.09512767813144E-15));
#126715=DIRECTION('center_axis',(1.4081690688991E-16,6.98296267768627E-15,
-1.));
#126716=DIRECTION('ref_axis',(1.,-7.97077743482043E-31,1.4081690688991E-16));
#126717=DIRECTION('',(0.371579467697567,-0.33456522605815,-0.86602240657979));
#126718=DIRECTION('center_axis',(1.4081690688991E-16,6.98296267768627E-15,
-1.));
#126719=DIRECTION('ref_axis',(-1.,7.97577417048809E-31,-1.40816906889911E-16));
#126720=DIRECTION('',(-0.334565226058174,0.371579467697563,0.866022406579783));
#126721=DIRECTION('center_axis',(-1.4081690688991E-16,-6.98296267768627E-15,
1.));
#126722=DIRECTION('ref_axis',(-1.,9.83319205199467E-31,-1.40816906889911E-16));
#126723=DIRECTION('center_axis',(-1.4081690688991E-16,-6.98296267768627E-15,
1.));
#126724=DIRECTION('ref_axis',(-1.,7.98248735348668E-31,-1.4081690688991E-16));
#126725=DIRECTION('',(0.743144825477402,-0.66913060635885,-4.56786669500646E-15));
#126726=DIRECTION('center_axis',(1.4081690688991E-16,6.98296267768627E-15,
-1.));
#126727=DIRECTION('ref_axis',(-1.,7.98707387273907E-31,-1.4081690688991E-16));
#126728=DIRECTION('',(-0.669130606358867,0.743144825477386,5.09512767813144E-15));
#126729=DIRECTION('center_axis',(-1.4081690688991E-16,-6.98296267768627E-15,
1.));
#126730=DIRECTION('ref_axis',(-1.,7.99150043815584E-31,-1.4081690688991E-16));
#126731=DIRECTION('center_axis',(-1.4081690688991E-16,-6.98296267768627E-15,
1.));
#126732=DIRECTION('ref_axis',(1.,3.19744231092045E-14,1.40816906890134E-16));
#126733=DIRECTION('',(0.3715730258176,-0.334572082386297,0.866022521746663));
#126734=DIRECTION('center_axis',(-1.4081690688991E-16,-6.98296267768627E-15,
1.));
#126735=DIRECTION('ref_axis',(-1.,7.99858039355471E-31,-1.4081690688991E-16));
#126736=DIRECTION('center_axis',(-1.4081690688991E-16,-6.98296267768627E-15,
1.));
#126737=DIRECTION('ref_axis',(-1.,7.99858039355471E-31,-1.4081690688991E-16));
#126738=DIRECTION('center_axis',(-1.4081690688991E-16,-6.98296267768627E-15,
1.));
#126739=DIRECTION('ref_axis',(-1.,7.99858039355471E-31,-1.4081690688991E-16));
#126740=DIRECTION('',(-0.334572082386318,0.371573025817621,-0.866022521746647));
#126741=DIRECTION('center_axis',(-1.4081690688991E-16,-6.98296267768627E-15,
1.));
#126742=DIRECTION('ref_axis',(-1.,9.83319205199467E-31,-1.40816906889911E-16));
#126743=DIRECTION('',(0.743144825477402,-0.66913060635885,-4.56786669500646E-15));
#126744=DIRECTION('center_axis',(1.4081690688991E-16,6.98296267768627E-15,
-1.));
#126745=DIRECTION('ref_axis',(-1.,8.01265634860448E-31,-1.4081690688991E-16));
#126746=DIRECTION('',(-0.669130606358867,0.743144825477386,5.09512767813144E-15));
#126747=DIRECTION('center_axis',(-1.4081690688991E-16,-6.98296267768627E-15,
1.));
#126748=DIRECTION('ref_axis',(-1.,8.32577322149061E-31,-1.39145123902276E-16));
#126749=DIRECTION('center_axis',(0.669925578293193,0.742428258814735,-7.86457219354815E-6));
#126750=DIRECTION('ref_axis',(6.35612258761182E-6,4.85763177036266E-6,0.999999999968002));
#126751=DIRECTION('center_axis',(-0.742428258814788,-0.669925578293134,
-7.86457211237817E-6));
#126752=DIRECTION('ref_axis',(-0.568130013485616,0.62960965028049,0.529924500330484));
#126753=DIRECTION('center_axis',(-1.4081690688991E-16,-6.98296267768627E-15,
1.));
#126754=DIRECTION('ref_axis',(-1.,8.07722881720021E-31,-1.42096112075504E-16));
#126755=DIRECTION('center_axis',(0.669891716967477,0.742458811950469,9.77057870806457E-6));
#126756=DIRECTION('ref_axis',(0.64938862426354,-0.585911726014409,-0.484769908302819));
#126757=DIRECTION('center_axis',(-0.742458811969724,-0.669891716946137,
9.77052681118192E-6));
#126758=DIRECTION('ref_axis',(0.585916765233986,-0.649394209166681,-0.484756336027208));
#126759=DIRECTION('center_axis',(-1.4081690688991E-16,-6.98296267768627E-15,
1.));
#126760=DIRECTION('ref_axis',(-1.,8.24049048117772E-31,-1.37719829560012E-16));
#126761=DIRECTION('center_axis',(-0.667197425139981,-0.744880927099563,
-1.81624800116486E-5));
#126762=DIRECTION('ref_axis',(0.6444983057982,-0.577295914343043,0.501349539848278));
#126763=DIRECTION('center_axis',(0.744880915222603,0.667197438400643,-1.8131645392542E-5));
#126764=DIRECTION('ref_axis',(0.578454551163162,-0.645791927479786,0.498340364249744));
#126765=DIRECTION('center_axis',(-1.4081690688991E-16,-6.98296267768627E-15,
1.));
#126766=DIRECTION('ref_axis',(-1.,8.26087817385229E-31,-1.38060560438432E-16));
#126767=DIRECTION('center_axis',(-0.667187360273293,-0.744889942172348,
-1.84940770019934E-5));
#126768=DIRECTION('ref_axis',(0.645812349433761,-0.578432592427061,-0.498339387703757));
#126769=DIRECTION('center_axis',(0.744889929987161,0.667187373876725,-1.85257100377501E-5));
#126770=DIRECTION('ref_axis',(0.577273915765722,-0.64451881341307,-0.50134850686236));
#126771=DIRECTION('center_axis',(-1.4081690688991E-16,-6.98296267768627E-15,
1.));
#126772=DIRECTION('ref_axis',(-1.,9.83319205199467E-31,-1.40816906889911E-16));
#126773=DIRECTION('center_axis',(-1.4081690688991E-16,-6.98296267768627E-15,
1.));
#126774=DIRECTION('ref_axis',(-1.,8.46073526001725E-31,-1.4081690688991E-16));
#126775=DIRECTION('',(0.669130606358867,-0.743144825477386,-5.09512767813144E-15));
#126776=DIRECTION('center_axis',(-1.4081690688991E-16,-6.98296267768627E-15,
1.));
#126777=DIRECTION('ref_axis',(-1.,7.97077743482043E-31,-1.4081690688991E-16));
#126778=DIRECTION('center_axis',(-1.4081690688991E-16,-6.98296267768627E-15,
1.));
#126779=DIRECTION('ref_axis',(-1.,7.97077743482043E-31,-1.4081690688991E-16));
#126780=DIRECTION('center_axis',(-1.4081690688991E-16,-6.98296267768627E-15,
1.));
#126781=DIRECTION('ref_axis',(-1.,7.97077743482043E-31,-1.4081690688991E-16));
#126782=DIRECTION('',(-0.587785252292482,0.809016994374941,5.5665653761908E-15));
#126783=DIRECTION('center_axis',(1.4081690688991E-16,6.98296267768627E-15,
-1.));
#126784=DIRECTION('ref_axis',(1.,-7.97077743482043E-31,1.4081690688991E-16));
#126785=DIRECTION('',(0.334572327551888,-0.371573073483894,-0.866022406579786));
#126786=DIRECTION('center_axis',(1.4081690688991E-16,6.98296267768627E-15,
-1.));
#126787=DIRECTION('ref_axis',(-1.,-1.86517468137026E-14,-1.40816906890041E-16));
#126788=DIRECTION('',(-0.29389181200343,0.404515505437148,0.8660224065798));
#126789=DIRECTION('center_axis',(-1.4081690688991E-16,-6.98296267768627E-15,
1.));
#126790=DIRECTION('ref_axis',(-1.,9.83319205199467E-31,-1.40816906889911E-16));
#126791=DIRECTION('center_axis',(-1.4081690688991E-16,-6.98296267768627E-15,
1.));
#126792=DIRECTION('ref_axis',(-1.,7.98248735348668E-31,-1.4081690688991E-16));
#126793=DIRECTION('',(0.669130606358867,-0.743144825477386,-5.09512767813144E-15));
#126794=DIRECTION('center_axis',(1.4081690688991E-16,6.98296267768627E-15,
-1.));
#126795=DIRECTION('ref_axis',(-1.,-1.86517468137026E-14,-1.40816906890041E-16));
#126796=DIRECTION('',(-0.587785252292482,0.809016994374941,5.5665653761908E-15));
#126797=DIRECTION('center_axis',(-1.4081690688991E-16,-6.98296267768627E-15,
1.));
#126798=DIRECTION('ref_axis',(-1.,7.99150043815584E-31,-1.4081690688991E-16));
#126799=DIRECTION('center_axis',(-1.4081690688991E-16,-6.98296267768627E-15,
1.));
#126800=DIRECTION('ref_axis',(1.,2.57571741713036E-14,1.4081690689009E-16));
#126801=DIRECTION('',(0.33456520427975,-0.371579218892551,0.866022521746664));
#126802=DIRECTION('center_axis',(-1.4081690688991E-16,-6.98296267768627E-15,
1.));
#126803=DIRECTION('ref_axis',(-1.,7.99858039355471E-31,-1.4081690688991E-16));
#126804=DIRECTION('center_axis',(-1.4081690688991E-16,-6.98296267768627E-15,
1.));
#126805=DIRECTION('ref_axis',(-1.,7.99858039355471E-31,-1.4081690688991E-16));
#126806=DIRECTION('center_axis',(-1.4081690688991E-16,-6.98296267768627E-15,
1.));
#126807=DIRECTION('ref_axis',(-1.,7.99858039355471E-31,-1.4081690688991E-16));
#126808=DIRECTION('',(-0.29389930413172,0.404509815527947,-0.866022521746656));
#126809=DIRECTION('center_axis',(-1.4081690688991E-16,-6.98296267768627E-15,
1.));
#126810=DIRECTION('ref_axis',(-1.,9.83319205199467E-31,-1.40816906889911E-16));
#126811=DIRECTION('',(0.669130606358867,-0.743144825477386,-5.09512767813144E-15));
#126812=DIRECTION('center_axis',(1.4081690688991E-16,6.98296267768627E-15,
-1.));
#126813=DIRECTION('ref_axis',(-1.,8.01265634860448E-31,-1.4081690688991E-16));
#126814=DIRECTION('',(-0.587785252292482,0.809016994374941,5.5665653761908E-15));
#126815=DIRECTION('center_axis',(-1.4081690688991E-16,-6.98296267768627E-15,
1.));
#126816=DIRECTION('ref_axis',(-1.,8.32577322149061E-31,-1.39145123902276E-16));
#126817=DIRECTION('center_axis',(0.74386054086017,0.668334867928768,-7.86457204182447E-6));
#126818=DIRECTION('ref_axis',(6.82906376097728E-6,4.16662531338862E-6,0.999999999968002));
#126819=DIRECTION('center_axis',(-0.808387450334084,-0.588650770899442,
-7.86457221610675E-6));
#126820=DIRECTION('ref_axis',(-0.49920560862511,0.685546339984938,0.529924500330461));
#126821=DIRECTION('center_axis',(-1.4081690688991E-16,-6.98296267768627E-15,
1.));
#126822=DIRECTION('ref_axis',(-1.,8.07722881720021E-31,-1.42096112075504E-16));
#126823=DIRECTION('center_axis',(0.743830058706459,0.668368793159347,9.77058883205476E-6));
#126824=DIRECTION('ref_axis',(0.58458675310207,-0.650581635231749,-0.484769908303684));
#126825=DIRECTION('center_axis',(-0.808414296645164,-0.588613901368497,
9.77051445187888E-6));
#126826=DIRECTION('ref_axis',(0.51482687315013,-0.707081738815272,-0.484756336025051));
#126827=DIRECTION('center_axis',(-1.4081690688991E-16,-6.98296267768627E-15,
1.));
#126828=DIRECTION('ref_axis',(-1.,8.24049048117772E-31,-1.37719829560012E-16));
#126829=DIRECTION('center_axis',(-0.741403706462227,-0.671059269896628,
-1.81624797328866E-5));
#126830=DIRECTION('ref_axis',(0.580623821869545,-0.641501844407148,0.501349539842046));
#126831=DIRECTION('center_axis',(0.810541502562919,0.585681203637515,-1.81316451185357E-5));
#126832=DIRECTION('ref_axis',(0.507782078836558,-0.702719177033379,0.498340364251134));
#126833=DIRECTION('center_axis',(-1.4081690688991E-16,-6.98296267768627E-15,
1.));
#126834=DIRECTION('ref_axis',(-1.,8.26087817385229E-31,-1.38060560438432E-16));
#126835=DIRECTION('center_axis',(-0.74139463905899,-0.671069287654084,-1.84940651197545E-5));
#126836=DIRECTION('ref_axis',(0.581811851821589,-0.642769650609858,-0.498339387701608));
#126837=DIRECTION('center_axis',(0.810549415920134,0.585670251940739,-1.85256933039895E-5));
#126838=DIRECTION('ref_axis',(0.506740987741753,-0.701329627216764,-0.501348506859757));
#126839=DIRECTION('center_axis',(-1.4081690688991E-16,-6.98296267768627E-15,
1.));
#126840=DIRECTION('ref_axis',(-1.,9.83319205199467E-31,-1.40816906889911E-16));
#126841=DIRECTION('center_axis',(-1.4081690688991E-16,-6.98296267768627E-15,
1.));
#126842=DIRECTION('ref_axis',(-1.,8.46073526001725E-31,-1.4081690688991E-16));
#126843=DIRECTION('',(0.587785252292482,-0.809016994374941,-5.5665653761908E-15));
#126844=DIRECTION('center_axis',(-1.4081690688991E-16,-6.98296267768627E-15,
1.));
#126845=DIRECTION('ref_axis',(-1.,7.97077743482043E-31,-1.4081690688991E-16));
#126846=DIRECTION('center_axis',(-1.4081690688991E-16,-6.98296267768627E-15,
1.));
#126847=DIRECTION('ref_axis',(-1.,7.97077743482043E-31,-1.4081690688991E-16));
#126848=DIRECTION('center_axis',(-1.4081690688991E-16,-6.98296267768627E-15,
1.));
#126849=DIRECTION('ref_axis',(-1.,7.97077743482043E-31,-1.4081690688991E-16));
#126850=DIRECTION('',(-0.50000000000001,0.866025403784433,5.97701461910992E-15));
#126851=DIRECTION('center_axis',(1.4081690688991E-16,6.98296267768627E-15,
-1.));
#126852=DIRECTION('ref_axis',(1.,-7.97077743482043E-31,1.4081690688991E-16));
#126853=DIRECTION('',(0.293899542971754,-0.404509888559887,-0.866022406579796));
#126854=DIRECTION('center_axis',(1.4081690688991E-16,6.98296267768627E-15,
-1.));
#126855=DIRECTION('ref_axis',(-1.,1.95399252334028E-14,-1.40816906889774E-16));
#126856=DIRECTION('',(-0.24999845775561,0.433019586648882,0.866022406579788));
#126857=DIRECTION('center_axis',(-1.4081690688991E-16,-6.98296267768627E-15,
1.));
#126858=DIRECTION('ref_axis',(-1.,9.83319205199467E-31,-1.40816906889911E-16));
#126859=DIRECTION('center_axis',(-1.4081690688991E-16,-6.98296267768627E-15,
1.));
#126860=DIRECTION('ref_axis',(-1.,7.98248735348668E-31,-1.4081690688991E-16));
#126861=DIRECTION('',(0.587785252292482,-0.809016994374941,-5.5665653761908E-15));
#126862=DIRECTION('center_axis',(1.4081690688991E-16,6.98296267768627E-15,
-1.));
#126863=DIRECTION('ref_axis',(-1.,1.86517468137026E-14,-1.4081690688978E-16));
#126864=DIRECTION('',(-0.50000000000001,0.866025403784433,5.97701461910992E-15));
#126865=DIRECTION('center_axis',(-1.4081690688991E-16,-6.98296267768627E-15,
1.));
#126866=DIRECTION('ref_axis',(-1.,7.99150043815584E-31,-1.4081690688991E-16));
#126867=DIRECTION('center_axis',(-1.4081690688991E-16,-6.98296267768627E-15,
1.));
#126868=DIRECTION('ref_axis',(1.,-1.24344978758018E-14,1.40816906889824E-16));
#126869=DIRECTION('',(0.293891816351536,-0.404515255718701,0.866022521746651));
#126870=DIRECTION('center_axis',(-1.4081690688991E-16,-6.98296267768627E-15,
1.));
#126871=DIRECTION('ref_axis',(-1.,7.99858039355471E-31,-1.4081690688991E-16));
#126872=DIRECTION('center_axis',(-1.4081690688991E-16,-6.98296267768627E-15,
1.));
#126873=DIRECTION('ref_axis',(-1.,7.99858039355471E-31,-1.4081690688991E-16));
#126874=DIRECTION('center_axis',(-1.4081690688991E-16,-6.98296267768627E-15,
1.));
#126875=DIRECTION('ref_axis',(-1.,7.99858039355471E-31,-1.4081690688991E-16));
#126876=DIRECTION('',(-0.250006503598685,0.433014711050231,-0.866022521746661));
#126877=DIRECTION('center_axis',(-1.4081690688991E-16,-6.98296267768627E-15,
1.));
#126878=DIRECTION('ref_axis',(-1.,9.83319205199467E-31,-1.40816906889911E-16));
#126879=DIRECTION('',(0.587785252292482,-0.809016994374941,-5.5665653761908E-15));
#126880=DIRECTION('center_axis',(1.4081690688991E-16,6.98296267768627E-15,
-1.));
#126881=DIRECTION('ref_axis',(-1.,-1.95399252334028E-14,-1.40816906890047E-16));
#126882=DIRECTION('',(-0.50000000000001,0.866025403784433,5.97701461910992E-15));
#126883=DIRECTION('center_axis',(-1.4081690688991E-16,-6.98296267768627E-15,
1.));
#126884=DIRECTION('ref_axis',(-1.,8.32577322149061E-31,-1.39145123902276E-16));
#126885=DIRECTION('center_axis',(0.809645611678629,0.586919060371776,-7.86457187793608E-6));
#126886=DIRECTION('ref_axis',(7.22718427493033E-6,3.42996842081855E-6,0.999999999968002));
#126887=DIRECTION('center_axis',(-0.865489779781559,-0.50092658247673,-7.86457232116346E-6));
#126888=DIRECTION('ref_axis',(-0.424811802651054,0.733972040528688,0.529924500330486));
#126889=DIRECTION('center_axis',(-1.4081690688991E-16,-6.98296267768627E-15,
1.));
#126890=DIRECTION('ref_axis',(-1.,8.07722881720021E-31,-1.42096112075504E-16));
#126891=DIRECTION('center_axis',(0.809618842658828,0.586955986012849,9.77058027889881E-6));
#126892=DIRECTION('ref_axis',(0.513380027141257,-0.70812363591068,-0.484769908304012));
#126893=DIRECTION('center_axis',(-0.865512625108597,-0.500887108720281,
9.77052087483086E-6));
#126894=DIRECTION('ref_axis',(0.43809643010891,-0.757022332966292,-0.48475633602471));
#126895=DIRECTION('center_axis',(-1.4081690688991E-16,-6.98296267768627E-15,
1.));
#126896=DIRECTION('ref_axis',(-1.,8.24049048117772E-31,-1.37719829560012E-16));
#126897=DIRECTION('center_axis',(-0.807487013627711,-0.589885346904571,
-1.81624797236099E-5));
#126898=DIRECTION('ref_axis',(0.510387901842864,-0.698679346019309,0.501349539840688));
#126899=DIRECTION('center_axis',(0.867321627584552,0.497748123045508,-1.81316453750404E-5));
#126900=DIRECTION('ref_axis',(0.431546239794831,-0.751947288230892,0.498340364250329));
#126901=DIRECTION('center_axis',(-1.4081690688991E-16,-6.98296267768627E-15,
1.));
#126902=DIRECTION('ref_axis',(-1.,8.26087817385229E-31,-1.38060560438432E-16));
#126903=DIRECTION('center_axis',(-0.807479043037464,-0.589896257585408,
-1.84940653406147E-5));
#126904=DIRECTION('ref_axis',(0.511436901809794,-0.700064389993911,-0.49833938769643));
#126905=DIRECTION('center_axis',(0.867328352821041,0.497736404183517,-1.85257158465585E-5));
#126906=DIRECTION('ref_axis',(0.430656099411607,-0.750456526859266,-0.501348506863148));
#126907=DIRECTION('center_axis',(-1.4081690688991E-16,-6.98296267768627E-15,
1.));
#126908=DIRECTION('ref_axis',(-1.,9.83319205199467E-31,-1.40816906889911E-16));
#126909=DIRECTION('center_axis',(-1.4081690688991E-16,-6.98296267768627E-15,
1.));
#126910=DIRECTION('ref_axis',(-1.,8.46073526001725E-31,-1.4081690688991E-16));
#126911=DIRECTION('',(0.50000000000001,-0.866025403784433,-5.97701461910992E-15));
#126912=DIRECTION('center_axis',(-1.4081690688991E-16,-6.98296267768627E-15,
1.));
#126913=DIRECTION('ref_axis',(-1.,7.97077743482043E-31,-1.4081690688991E-16));
#126914=DIRECTION('center_axis',(-1.4081690688991E-16,-6.98296267768627E-15,
1.));
#126915=DIRECTION('ref_axis',(-1.,7.97077743482043E-31,-1.4081690688991E-16));
#126916=DIRECTION('center_axis',(-1.4081690688991E-16,-6.98296267768627E-15,
1.));
#126917=DIRECTION('ref_axis',(-1.,7.97077743482043E-31,-1.4081690688991E-16));
#126918=DIRECTION('',(-0.40673664307581,0.913545457642596,6.32197843909135E-15));
#126919=DIRECTION('center_axis',(1.4081690688991E-16,6.98296267768627E-15,
-1.));
#126920=DIRECTION('ref_axis',(1.,-7.97077743482043E-31,1.4081690688991E-16));
#126921=DIRECTION('',(0.25000673349641,-0.433014808647711,-0.866022406579784));
#126922=DIRECTION('center_axis',(1.4081690688991E-16,6.98296267768627E-15,
-1.));
#126923=DIRECTION('ref_axis',(-1.,1.95399252334028E-14,-1.40816906889774E-16));
#126924=DIRECTION('',(-0.203366068089037,0.456779414654113,0.86602240657979));
#126925=DIRECTION('center_axis',(-1.4081690688991E-16,-6.98296267768627E-15,
1.));
#126926=DIRECTION('ref_axis',(-1.,9.83319205199467E-31,-1.40816906889911E-16));
#126927=DIRECTION('center_axis',(-1.4081690688991E-16,-6.98296267768627E-15,
1.));
#126928=DIRECTION('ref_axis',(-1.,7.98248735348668E-31,-1.4081690688991E-16));
#126929=DIRECTION('',(0.50000000000001,-0.866025403784433,-5.97701461910992E-15));
#126930=DIRECTION('center_axis',(1.4081690688991E-16,6.98296267768627E-15,
-1.));
#126931=DIRECTION('ref_axis',(-1.,2.04281036531029E-14,-1.40816906889768E-16));
#126932=DIRECTION('',(-0.40673664307581,0.913545457642596,6.32197843909135E-15));
#126933=DIRECTION('center_axis',(-1.4081690688991E-16,-6.98296267768627E-15,
1.));
#126934=DIRECTION('ref_axis',(-1.,7.99150043815584E-31,-1.4081690688991E-16));
#126935=DIRECTION('center_axis',(-1.4081690688991E-16,-6.98296267768627E-15,
1.));
#126936=DIRECTION('ref_axis',(1.,-1.24344978758018E-14,1.40816906889824E-16));
#126937=DIRECTION('',(0.249998488182559,-0.433019338752883,0.866022521746664));
#126938=DIRECTION('center_axis',(-1.4081690688991E-16,-6.98296267768627E-15,
1.));
#126939=DIRECTION('ref_axis',(-1.,7.99858039355471E-31,-1.4081690688991E-16));
#126940=DIRECTION('center_axis',(-1.4081690688991E-16,-6.98296267768627E-15,
1.));
#126941=DIRECTION('ref_axis',(-1.,7.99858039355471E-31,-1.4081690688991E-16));
#126942=DIRECTION('center_axis',(-1.4081690688991E-16,-6.98296267768627E-15,
1.));
#126943=DIRECTION('ref_axis',(-1.,7.99858039355471E-31,-1.4081690688991E-16));
#126944=DIRECTION('',(-0.203374579494996,0.456775406784117,-0.866022521746656));
#126945=DIRECTION('center_axis',(-1.4081690688991E-16,-6.98296267768627E-15,
1.));
#126946=DIRECTION('ref_axis',(-1.,9.83319205199467E-31,-1.40816906889911E-16));
#126947=DIRECTION('',(0.50000000000001,-0.866025403784433,-5.97701461910992E-15));
#126948=DIRECTION('center_axis',(1.4081690688991E-16,6.98296267768627E-15,
-1.));
#126949=DIRECTION('ref_axis',(-1.,-3.90798504668055E-14,-1.40816906890183E-16));
#126950=DIRECTION('',(-0.40673664307581,0.913545457642596,6.32197843909135E-15));
#126951=DIRECTION('center_axis',(-1.4081690688991E-16,-6.98296267768627E-15,
1.));
#126952=DIRECTION('ref_axis',(-1.,8.32577322149061E-31,-1.39145123902276E-16));
#126953=DIRECTION('center_axis',(0.866560035746456,0.499072844768427,-7.86457212100349E-6));
#126954=DIRECTION('ref_axis',(7.54612252965276E-6,2.65573237658703E-6,0.999999999968002));
#126955=DIRECTION('center_axis',(-0.913109622086429,-0.4077141375907,-7.86457242400786E-6));
#126956=DIRECTION('ref_axis',(-0.345763669669516,0.774356189802966,0.529924500330474));
#126957=DIRECTION('center_axis',(-1.4081690688991E-16,-6.98296267768627E-15,
1.));
#126958=DIRECTION('ref_axis',(-1.,8.07722881720021E-31,-1.42096112075504E-16));
#126959=DIRECTION('center_axis',(0.866537273150592,0.4991123662516,9.77058020237922E-6));
#126960=DIRECTION('ref_axis',(0.43654860217139,-0.757907285850219,-0.484769908304301));
#126961=DIRECTION('center_axis',(-0.913128216133684,-0.40767249208777,9.77051909676145E-6));
#126962=DIRECTION('ref_axis',(0.356566110901339,-0.798668832019219,-0.484756336026412));
#126963=DIRECTION('center_axis',(-1.4081690688991E-16,-6.98296267768627E-15,
1.));
#126964=DIRECTION('ref_axis',(-1.,8.24049048117772E-31,-1.37719829560012E-16));
#126965=DIRECTION('center_axis',(-0.864723324094283,-0.50224851661051,-1.8162479892997E-5));
#126966=DIRECTION('ref_axis',(0.434560065157101,-0.748201970507024,0.501349539842277));
#126967=DIRECTION('center_axis',(0.914599195355538,0.404361609857126,-1.81316451782619E-5));
#126968=DIRECTION('ref_axis',(0.350582289841583,-0.792936907580423,0.498340364255423));
#126969=DIRECTION('center_axis',(-1.4081690688991E-16,-6.98296267768627E-15,
1.));
#126970=DIRECTION('ref_axis',(-1.,8.26087817385229E-31,-1.38060560438432E-16));
#126971=DIRECTION('center_axis',(-0.864716537645637,-0.502260200673028,
-1.84940690499114E-5));
#126972=DIRECTION('ref_axis',(0.435458542073093,-0.749689077418544,-0.498339387701703));
#126973=DIRECTION('center_axis',(0.914604658798975,0.404349252206565,-1.85257025671403E-5));
#126974=DIRECTION('ref_axis',(0.349852852737875,-0.791361267753813,-0.501348506859498));
#126975=DIRECTION('center_axis',(-1.4081690688991E-16,-6.98296267768627E-15,
1.));
#126976=DIRECTION('ref_axis',(-1.,9.83319205199467E-31,-1.40816906889911E-16));
#126977=DIRECTION('center_axis',(-1.4081690688991E-16,-6.98296267768627E-15,
1.));
#126978=DIRECTION('ref_axis',(-1.,8.46073526001725E-31,-1.4081690688991E-16));
#126979=DIRECTION('',(0.40673664307581,-0.913545457642596,-6.32197843909135E-15));
#126980=DIRECTION('center_axis',(-1.4081690688991E-16,-6.98296267768627E-15,
1.));
#126981=DIRECTION('ref_axis',(-1.,7.97077743482043E-31,-1.4081690688991E-16));
#126982=DIRECTION('center_axis',(-1.4081690688991E-16,-6.98296267768627E-15,
1.));
#126983=DIRECTION('ref_axis',(-1.,7.97077743482043E-31,-1.4081690688991E-16));
#126984=DIRECTION('center_axis',(-1.4081690688991E-16,-6.98296267768627E-15,
1.));
#126985=DIRECTION('ref_axis',(-1.,7.97077743482043E-31,-1.4081690688991E-16));
#126986=DIRECTION('',(-0.309016994374957,0.95105651629515,6.59767734033506E-15));
#126987=DIRECTION('center_axis',(1.4081690688991E-16,6.98296267768627E-15,
-1.));
#126988=DIRECTION('ref_axis',(1.,-7.97077743482043E-31,1.4081690688991E-16));
#126989=DIRECTION('',(0.203374797931567,-0.456775527877799,-0.866022406579791));
#126990=DIRECTION('center_axis',(1.4081690688991E-16,6.98296267768627E-15,
-1.));
#126991=DIRECTION('ref_axis',(-1.,2.04281036531029E-14,-1.40816906889768E-16));
#126992=DIRECTION('',(-0.154505557223407,0.475534671805162,0.866022406579784));
#126993=DIRECTION('center_axis',(-1.4081690688991E-16,-6.98296267768627E-15,
1.));
#126994=DIRECTION('ref_axis',(-1.,9.83319205199467E-31,-1.40816906889911E-16));
#126995=DIRECTION('center_axis',(-1.4081690688991E-16,-6.98296267768627E-15,
1.));
#126996=DIRECTION('ref_axis',(-1.,7.98248735348668E-31,-1.4081690688991E-16));
#126997=DIRECTION('',(0.40673664307581,-0.913545457642596,-6.32197843909135E-15));
#126998=DIRECTION('center_axis',(1.4081690688991E-16,6.98296267768627E-15,
-1.));
#126999=DIRECTION('ref_axis',(-1.,7.98707387273907E-31,-1.4081690688991E-16));
#127000=DIRECTION('',(-0.309016994374957,0.95105651629515,6.59767734033506E-15));
#127001=DIRECTION('center_axis',(-1.4081690688991E-16,-6.98296267768627E-15,
1.));
#127002=DIRECTION('ref_axis',(-1.,7.99150043815584E-31,-1.4081690688991E-16));
#127003=DIRECTION('center_axis',(-1.4081690688991E-16,-6.98296267768627E-15,
1.));
#127004=DIRECTION('ref_axis',(1.,-1.24344978758018E-14,1.40816906889824E-16));
#127005=DIRECTION('',(0.203366124261494,-0.456779171296592,0.866022521746668));
#127006=DIRECTION('center_axis',(-1.4081690688991E-16,-6.98296267768627E-15,
1.));
#127007=DIRECTION('ref_axis',(-1.,7.99858039355471E-31,-1.4081690688991E-16));
#127008=DIRECTION('center_axis',(-1.4081690688991E-16,-6.98296267768627E-15,
1.));
#127009=DIRECTION('ref_axis',(-1.,7.99858039355471E-31,-1.4081690688991E-16));
#127010=DIRECTION('center_axis',(-1.4081690688991E-16,-6.98296267768627E-15,
1.));
#127011=DIRECTION('ref_axis',(-1.,7.99858039355471E-31,-1.4081690688991E-16));
#127012=DIRECTION('',(-0.154514440939479,0.47553157557488,-0.866022521746653));
#127013=DIRECTION('center_axis',(-1.4081690688991E-16,-6.98296267768627E-15,
1.));
#127014=DIRECTION('ref_axis',(-1.,9.83319205199467E-31,-1.40816906889911E-16));
#127015=DIRECTION('',(0.40673664307581,-0.913545457642596,-6.32197843909135E-15));
#127016=DIRECTION('center_axis',(1.4081690688991E-16,6.98296267768627E-15,
-1.));
#127017=DIRECTION('ref_axis',(-1.,8.01265634860448E-31,-1.4081690688991E-16));
#127018=DIRECTION('',(-0.309016994374957,0.95105651629515,6.59767734033506E-15));
#127019=DIRECTION('center_axis',(-1.4081690688991E-16,-6.98296267768627E-15,
1.));
#127020=DIRECTION('ref_axis',(-1.,8.32577322149061E-31,-1.39145123902276E-16));
#127021=DIRECTION('center_axis',(0.9139802467232,0.405758682640246,-7.86457197746387E-6));
#127022=DIRECTION('ref_axis',(7.78238356101367E-6,1.85239937195226E-6,0.999999999968001));
#127023=DIRECTION('center_axis',(-0.95072524429128,-0.310034691293467,-7.86457228400698E-6));
#127024=DIRECTION('ref_axis',(-0.262927277567181,0.806256330617373,0.52992450033049));
#127025=DIRECTION('center_axis',(-1.4081690688991E-16,-6.98296267768627E-15,
1.));
#127026=DIRECTION('ref_axis',(-1.,8.07722881720021E-31,-1.42096112075504E-16));
#127027=DIRECTION('center_axis',(0.913961739943914,0.405800366957978,9.77058357183956E-6));
#127028=DIRECTION('ref_axis',(0.354934259362539,-0.799387144963771,-0.48476990830438));
#127029=DIRECTION('center_axis',(-0.950739383337938,-0.309991330321888,
9.77051914909191E-6));
#127030=DIRECTION('ref_axis',(0.271129178766832,-0.831564948216754,-0.484756336027174));
#127031=DIRECTION('center_axis',(-1.4081690688991E-16,-6.98296267768627E-15,
1.));
#127032=DIRECTION('ref_axis',(-1.,8.24049048117772E-31,-1.37719829560012E-16));
#127033=DIRECTION('center_axis',(-0.912485544867141,-0.409108946466148,
-1.81624799228571E-5));
#127034=DIRECTION('ref_axis',(0.353971097460695,-0.789527137635747,0.501349539841392));
#127035=DIRECTION('center_axis',(0.951856222950113,0.306544826252847,-1.81316452973037E-5));
#127036=DIRECTION('ref_axis',(0.265777286958593,-0.825238944241564,0.498340364253187));
#127037=DIRECTION('center_axis',(-1.4081690688991E-16,-6.98296267768627E-15,
1.));
#127038=DIRECTION('ref_axis',(-1.,8.26087817385229E-31,-1.38060560438432E-16));
#127039=DIRECTION('center_axis',(-0.912480016910859,-0.409121275902793,
-1.84940621727514E-5));
#127040=DIRECTION('ref_axis',(0.354709207425047,-0.791100014429281,-0.498339387704691));
#127041=DIRECTION('center_axis',(0.951860364738416,0.30653196521219,-1.85257001811446E-5));
#127042=DIRECTION('ref_axis',(0.265216544997311,-0.823595688995009,-0.501348506857781));
#127043=DIRECTION('center_axis',(-1.4081690688991E-16,-6.98296267768627E-15,
1.));
#127044=DIRECTION('ref_axis',(-1.,9.83319205199467E-31,-1.40816906889911E-16));
#127045=DIRECTION('center_axis',(-1.4081690688991E-16,-6.98296267768627E-15,
1.));
#127046=DIRECTION('ref_axis',(-1.,8.46073526001725E-31,-1.4081690688991E-16));
#127047=DIRECTION('',(0.309016994374957,-0.95105651629515,-6.59767734033506E-15));
#127048=DIRECTION('center_axis',(-1.4081690688991E-16,-6.98296267768627E-15,
1.));
#127049=DIRECTION('ref_axis',(-1.,7.97077743482043E-31,-1.4081690688991E-16));
#127050=DIRECTION('center_axis',(-1.4081690688991E-16,-6.98296267768627E-15,
1.));
#127051=DIRECTION('ref_axis',(-1.,7.97077743482043E-31,-1.4081690688991E-16));
#127052=DIRECTION('center_axis',(-1.4081690688991E-16,-6.98296267768627E-15,
1.));
#127053=DIRECTION('ref_axis',(-1.,7.97077743482043E-31,-1.4081690688991E-16));
#127054=DIRECTION('',(-0.20791169081777,0.978147600733803,6.80109070798531E-15));
#127055=DIRECTION('center_axis',(1.4081690688991E-16,6.98296267768627E-15,
-1.));
#127056=DIRECTION('ref_axis',(1.,-7.97077743482043E-31,1.4081690688991E-16));
#127057=DIRECTION('',(0.154514645521721,-0.475531718838048,-0.866022406579777));
#127058=DIRECTION('center_axis',(1.4081690688991E-16,6.98296267768627E-15,
-1.));
#127059=DIRECTION('ref_axis',(-1.,-3.10862446895044E-14,-1.40816906890128E-16));
#127060=DIRECTION('',(-0.103952251140494,0.489079871579876,0.866022406579781));
#127061=DIRECTION('center_axis',(-1.4081690688991E-16,-6.98296267768627E-15,
1.));
#127062=DIRECTION('ref_axis',(-1.,9.83319205199467E-31,-1.40816906889911E-16));
#127063=DIRECTION('center_axis',(-1.4081690688991E-16,-6.98296267768627E-15,
1.));
#127064=DIRECTION('ref_axis',(-1.,7.98248735348668E-31,-1.4081690688991E-16));
#127065=DIRECTION('',(0.309016994374957,-0.95105651629515,-6.59767734033506E-15));
#127066=DIRECTION('center_axis',(1.4081690688991E-16,6.98296267768627E-15,
-1.));
#127067=DIRECTION('ref_axis',(-1.,-3.10862446895044E-14,-1.40816906890128E-16));
#127068=DIRECTION('',(-0.20791169081777,0.978147600733803,6.80109070798531E-15));
#127069=DIRECTION('center_axis',(-1.4081690688991E-16,-6.98296267768627E-15,
1.));
#127070=DIRECTION('ref_axis',(-1.,7.99150043815584E-31,-1.4081690688991E-16));
#127071=DIRECTION('center_axis',(-1.4081690688991E-16,-6.98296267768627E-15,
1.));
#127072=DIRECTION('ref_axis',(1.,3.5527136788005E-14,1.40816906890159E-16));
#127073=DIRECTION('',(0.154505638525959,-0.475534435652405,0.866022521746654));
#127074=DIRECTION('center_axis',(-1.4081690688991E-16,-6.98296267768627E-15,
1.));
#127075=DIRECTION('ref_axis',(-1.,7.99858039355471E-31,-1.4081690688991E-16));
#127076=DIRECTION('center_axis',(-1.4081690688991E-16,-6.98296267768627E-15,
1.));
#127077=DIRECTION('ref_axis',(-1.,7.99858039355471E-31,-1.4081690688991E-16));
#127078=DIRECTION('center_axis',(-1.4081690688991E-16,-6.98296267768627E-15,
1.));
#127079=DIRECTION('ref_axis',(-1.,7.99858039355471E-31,-1.4081690688991E-16));
#127080=DIRECTION('',(-0.103961409834819,0.48907772091222,-0.866022521746672));
#127081=DIRECTION('center_axis',(-1.4081690688991E-16,-6.98296267768627E-15,
1.));
#127082=DIRECTION('ref_axis',(-1.,9.83319205199467E-31,-1.40816906889911E-16));
#127083=DIRECTION('',(0.309016994374957,-0.95105651629515,-6.59767734033506E-15));
#127084=DIRECTION('center_axis',(1.4081690688991E-16,6.98296267768627E-15,
-1.));
#127085=DIRECTION('ref_axis',(-1.,8.01265634860448E-31,-1.4081690688991E-16));
#127086=DIRECTION('',(-0.20791169081777,0.978147600733803,6.80109070798531E-15));
#127087=DIRECTION('center_axis',(-1.4081690688991E-16,-6.98296267768627E-15,
1.));
#127088=DIRECTION('ref_axis',(-1.,8.32577322149061E-31,-1.39145123902276E-16));
#127089=DIRECTION('center_axis',(0.951386698854222,0.30799894347451,-7.86457202755924E-6));
#127090=DIRECTION('ref_axis',(7.93337935782266E-6,1.02877115701158E-6,0.999999999968001));
#127091=DIRECTION('center_axis',(-0.977924521767598,-0.208958440039553,
-7.86457224718168E-6));
#127092=DIRECTION('ref_axis',(-0.177210199190854,0.829322958353518,0.529924500330478));
#127093=DIRECTION('center_axis',(-1.4081690688991E-16,-6.98296267768627E-15,
1.));
#127094=DIRECTION('ref_axis',(-1.,8.07722881720021E-31,-1.42096112075504E-16));
#127095=DIRECTION('center_axis',(0.951372650654724,0.308042333926263,9.77058391111578E-6));
#127096=DIRECTION('ref_axis',(0.269431182533837,-0.832108751235939,-0.484769908301851));
#127097=DIRECTION('center_axis',(-0.97793405090397,-0.208913838668213,9.770513827856E-6));
#127098=DIRECTION('ref_axis',(0.182721698612625,-0.855350264826529,-0.48475633602595));
#127099=DIRECTION('center_axis',(-1.4081690688991E-16,-6.98296267768627E-15,
1.));
#127100=DIRECTION('ref_axis',(-1.,8.24049048117772E-31,-1.37719829560012E-16));
#127101=DIRECTION('center_axis',(-0.950250383060607,-0.311487093092626,
-1.81624797655766E-5));
#127102=DIRECTION('ref_axis',(0.269503948345924,-0.82220208022159,0.501349539847448));
#127103=DIRECTION('center_axis',(0.978684514577279,0.205369473383652,-1.81316451809006E-5));
#127104=DIRECTION('ref_axis',(0.178060372502512,-0.84849949033992,0.498340364246328));
#127105=DIRECTION('center_axis',(-1.4081690688991E-16,-6.98296267768627E-15,
1.));
#127106=DIRECTION('ref_axis',(-1.,8.26087817385229E-31,-1.38060560438432E-16));
#127107=DIRECTION('center_axis',(-0.950246174164118,-0.311499932816086,
-1.84940623667029E-5));
#127108=DIRECTION('ref_axis',(0.270073604474823,-0.823843494138777,-0.498339387697971));
#127109=DIRECTION('center_axis',(0.978687289330155,0.205356249869322,-1.85257125721377E-5));
#127110=DIRECTION('ref_axis',(0.177674469288529,-0.846806623514797,-0.501348506863748));
#127111=DIRECTION('center_axis',(-1.4081690688991E-16,-6.98296267768627E-15,
1.));
#127112=DIRECTION('ref_axis',(-1.,9.83319205199467E-31,-1.40816906889911E-16));
#127113=DIRECTION('center_axis',(-1.4081690688991E-16,-6.98296267768627E-15,
1.));
#127114=DIRECTION('ref_axis',(-1.,8.46073526001725E-31,-1.4081690688991E-16));
#127115=DIRECTION('',(0.20791169081777,-0.978147600733803,-6.80109070798531E-15));
#127116=DIRECTION('center_axis',(-1.4081690688991E-16,-6.98296267768627E-15,
1.));
#127117=DIRECTION('ref_axis',(-1.,7.97077743482043E-31,-1.4081690688991E-16));
#127118=DIRECTION('center_axis',(-1.4081690688991E-16,-6.98296267768627E-15,
1.));
#127119=DIRECTION('ref_axis',(-1.,7.97077743482043E-31,-1.4081690688991E-16));
#127120=DIRECTION('center_axis',(-1.4081690688991E-16,-6.98296267768627E-15,
1.));
#127121=DIRECTION('ref_axis',(-1.,7.97077743482043E-31,-1.4081690688991E-16));
#127122=DIRECTION('',(-0.104528463267664,0.994521895368272,6.92998990261914E-15));
#127123=DIRECTION('center_axis',(1.4081690688991E-16,6.98296267768627E-15,
-1.));
#127124=DIRECTION('ref_axis',(1.,-7.97077743482043E-31,1.4081690688991E-16));
#127125=DIRECTION('',(0.103961598321227,-0.48907788477527,-0.866022406579786));
#127126=DIRECTION('center_axis',(1.4081690688991E-16,6.98296267768627E-15,
-1.));
#127127=DIRECTION('ref_axis',(-1.,-3.19744231092045E-14,-1.40816906890134E-16));
#127128=DIRECTION('',(-0.052260022440647,0.497266609935019,0.866022406579782));
#127129=DIRECTION('center_axis',(-1.4081690688991E-16,-6.98296267768627E-15,
1.));
#127130=DIRECTION('ref_axis',(-1.,9.83319205199467E-31,-1.40816906889911E-16));
#127131=DIRECTION('center_axis',(-1.4081690688991E-16,-6.98296267768627E-15,
1.));
#127132=DIRECTION('ref_axis',(-1.,7.98248735348668E-31,-1.4081690688991E-16));
#127133=DIRECTION('',(0.20791169081777,-0.978147600733803,-6.80109070798531E-15));
#127134=DIRECTION('center_axis',(1.4081690688991E-16,6.98296267768627E-15,
-1.));
#127135=DIRECTION('ref_axis',(-1.,-3.19744231092045E-14,-1.40816906890134E-16));
#127136=DIRECTION('',(-0.104528463267664,0.994521895368272,6.92998990261914E-15));
#127137=DIRECTION('center_axis',(-1.4081690688991E-16,-6.98296267768627E-15,
1.));
#127138=DIRECTION('ref_axis',(-1.,7.99150043815584E-31,-1.4081690688991E-16));
#127139=DIRECTION('center_axis',(-1.4081690688991E-16,-6.98296267768627E-15,
1.));
#127140=DIRECTION('ref_axis',(1.,2.30926389122033E-14,1.40816906890072E-16));
#127141=DIRECTION('',(0.103952356682315,-0.489079645219204,0.866022521746664));
#127142=DIRECTION('center_axis',(-1.4081690688991E-16,-6.98296267768627E-15,
1.));
#127143=DIRECTION('ref_axis',(-1.,7.99858039355471E-31,-1.4081690688991E-16));
#127144=DIRECTION('center_axis',(-1.4081690688991E-16,-6.98296267768627E-15,
1.));
#127145=DIRECTION('ref_axis',(-1.,7.99858039355471E-31,-1.4081690688991E-16));
#127146=DIRECTION('center_axis',(-1.4081690688991E-16,-6.98296267768627E-15,
1.));
#127147=DIRECTION('ref_axis',(-1.,7.99858039355471E-31,-1.4081690688991E-16));
#127148=DIRECTION('',(-0.0522693557686642,0.497265428393217,-0.866022521746657));
#127149=DIRECTION('center_axis',(-1.4081690688991E-16,-6.98296267768627E-15,
1.));
#127150=DIRECTION('ref_axis',(-1.,9.83319205199467E-31,-1.40816906889911E-16));
#127151=DIRECTION('',(0.20791169081777,-0.978147600733803,-6.80109070798531E-15));
#127152=DIRECTION('center_axis',(1.4081690688991E-16,6.98296267768627E-15,
-1.));
#127153=DIRECTION('ref_axis',(-1.,1.06581410364015E-14,-1.40816906889836E-16));
#127154=DIRECTION('',(-0.104528463267664,0.994521895368272,6.92998990261914E-15));
#127155=DIRECTION('center_axis',(-1.4081690688991E-16,-6.98296267768627E-15,
1.));
#127156=DIRECTION('ref_axis',(-1.,8.32577322149061E-31,-1.39145123902276E-16));
#127157=DIRECTION('center_axis',(0.978369559222101,0.206864703431255,-7.86457189927893E-6));
#127158=DIRECTION('ref_axis',(7.99745522714731E-6,1.93871412098472E-7,0.999999999968002));
#127159=DIRECTION('center_axis',(-0.994409453539564,-0.105592796389219,
-7.86457226194514E-6));
#127160=DIRECTION('ref_axis',(-0.0895515687886142,0.843303350210933,0.529924500330486));
#127161=DIRECTION('center_axis',(-1.4081690688991E-16,-6.98296267768627E-15,
1.));
#127162=DIRECTION('ref_axis',(-1.,8.07722881720021E-31,-1.42096112075504E-16));
#127163=DIRECTION('center_axis',(0.978360123517625,0.206909324620987,9.77058623646806E-6));
#127164=DIRECTION('ref_axis',(0.180976161286346,-0.855713599896903,-0.484769908304488));
#127165=DIRECTION('center_axis',(-0.994414268361322,-0.105547443284781,
9.77051728312679E-6));
#127166=DIRECTION('ref_axis',(0.0923122812911233,-0.869764184939502,-0.484756336028063));
#127167=DIRECTION('center_axis',(-1.4081690688991E-16,-6.98296267768627E-15,
1.));
#127168=DIRECTION('ref_axis',(-1.,8.24049048117772E-31,-1.37719829560012E-16));
#127169=DIRECTION('center_axis',(-0.97760407920455,-0.210452521944378,-1.81624797492279E-5));
#127170=DIRECTION('ref_axis',(0.182084057577984,-0.845868804766651,0.501349539840793));
#127171=DIRECTION('center_axis',(0.99479013385986,0.10194404958763,-1.81316452521936E-5));
#127172=DIRECTION('ref_axis',(0.0883925913421765,-0.862463698454775,0.498340364252713));
#127173=DIRECTION('center_axis',(-1.4081690688991E-16,-6.98296267768627E-15,
1.));
#127174=DIRECTION('ref_axis',(-1.,8.26087817385229E-31,-1.38060560438432E-16));
#127175=DIRECTION('center_axis',(-0.97760123548189,-0.210465731277688,-1.84940665228558E-5));
#127176=DIRECTION('ref_axis',(0.182479018596661,-0.847560772126245,-0.498339387691523));
#127177=DIRECTION('center_axis',(0.994791511178768,0.101930608471943,-1.85257116465804E-5));
#127178=DIRECTION('ref_axis',(0.0881857549144703,-0.860739767464731,-0.501348506864164));
#127179=DIRECTION('center_axis',(-1.4081690688991E-16,-6.98296267768627E-15,
1.));
#127180=DIRECTION('ref_axis',(-1.,9.83319205199467E-31,-1.40816906889911E-16));
#127181=DIRECTION('center_axis',(-1.4081690688991E-16,-6.98296267768627E-15,
1.));
#127182=DIRECTION('ref_axis',(-1.,8.46073526001725E-31,-1.4081690688991E-16));
#127183=DIRECTION('',(0.104528463267664,-0.994521895368272,-6.92998990261914E-15));
#127184=DIRECTION('center_axis',(-1.4081690688991E-16,-6.98296267768627E-15,
1.));
#127185=DIRECTION('ref_axis',(-1.,7.97077743482043E-31,-1.4081690688991E-16));
#127186=DIRECTION('center_axis',(-1.4081690688991E-16,-6.98296267768627E-15,
1.));
#127187=DIRECTION('ref_axis',(-1.,7.97077743482043E-31,-1.4081690688991E-16));
#127188=DIRECTION('center_axis',(-1.4081690688991E-16,-6.98296267768627E-15,
1.));
#127189=DIRECTION('ref_axis',(-1.,7.97077743482043E-31,-1.4081690688991E-16));
#127190=DIRECTION('',(-1.04744440165294E-14,1.,6.98296267768627E-15));
#127191=DIRECTION('center_axis',(1.4081690688991E-16,6.98296267768627E-15,
-1.));
#127192=DIRECTION('ref_axis',(1.,-7.97077743482043E-31,1.4081690688991E-16));
#127193=DIRECTION('',(0.0522695260941978,-0.497265611060804,-0.866022406579768));
#127194=DIRECTION('center_axis',(1.4081690688991E-16,6.98296267768627E-15,
-1.));
#127195=DIRECTION('ref_axis',(-1.,1.06581410364015E-14,-1.40816906889836E-16));
#127196=DIRECTION('',(4.77800116018645E-6,0.500005191251989,0.866022406579779));
#127197=DIRECTION('center_axis',(-1.4081690688991E-16,-6.98296267768627E-15,
1.));
#127198=DIRECTION('ref_axis',(-1.,9.83319205199467E-31,-1.40816906889911E-16));
#127199=DIRECTION('center_axis',(-1.4081690688991E-16,-6.98296267768627E-15,
1.));
#127200=DIRECTION('ref_axis',(-1.,7.98248735348668E-31,-1.4081690688991E-16));
#127201=DIRECTION('',(0.104528463267664,-0.994521895368272,-6.92998990261914E-15));
#127202=DIRECTION('center_axis',(1.4081690688991E-16,6.98296267768627E-15,
-1.));
#127203=DIRECTION('ref_axis',(-1.,1.06581410364015E-14,-1.40816906889836E-16));
#127204=DIRECTION('',(-1.04744440165294E-14,1.,6.98296267768627E-15));
#127205=DIRECTION('center_axis',(-1.4081690688991E-16,-6.98296267768627E-15,
1.));
#127206=DIRECTION('ref_axis',(-1.,7.99150043815584E-31,-1.4081690688991E-16));
#127207=DIRECTION('center_axis',(-1.4081690688991E-16,-6.98296267768627E-15,
1.));
#127208=DIRECTION('ref_axis',(1.,-2.30926389122033E-14,1.40816906889749E-16));
#127209=DIRECTION('',(0.0522601510654366,-0.497266395846486,0.866022521746671));
#127210=DIRECTION('center_axis',(-1.4081690688991E-16,-6.98296267768627E-15,
1.));
#127211=DIRECTION('ref_axis',(-1.,7.99858039355471E-31,-1.4081690688991E-16));
#127212=DIRECTION('center_axis',(-1.4081690688991E-16,-6.98296267768627E-15,
1.));
#127213=DIRECTION('ref_axis',(-1.,7.99858039355471E-31,-1.4081690688991E-16));
#127214=DIRECTION('center_axis',(-1.4081690688991E-16,-6.98296267768627E-15,
1.));
#127215=DIRECTION('ref_axis',(-1.,7.99858039355471E-31,-1.4081690688991E-16));
#127216=DIRECTION('',(-4.62770265767274E-6,0.500004991781207,-0.866022521746669));
#127217=DIRECTION('center_axis',(-1.4081690688991E-16,-6.98296267768627E-15,
1.));
#127218=DIRECTION('ref_axis',(-1.,9.83319205199467E-31,-1.40816906889911E-16));
#127219=DIRECTION('',(0.104528463267664,-0.994521895368272,-6.92998990261914E-15));
#127220=DIRECTION('center_axis',(1.4081690688991E-16,6.98296267768627E-15,
-1.));
#127221=DIRECTION('ref_axis',(-1.,-3.28626015289046E-14,-1.4081690689014E-16));
#127222=DIRECTION('',(-1.04744440165294E-14,1.,6.98296267768627E-15));
#127223=DIRECTION('center_axis',(-1.4081690688991E-16,-6.98296267768627E-15,
1.));
#127224=DIRECTION('ref_axis',(-1.,8.32577322149061E-31,-1.39145123902276E-16));
#127225=DIRECTION('center_axis',(0.994633197962181,0.103464010407842,-7.8645720159475E-6));
#127226=DIRECTION('ref_axis',(7.97390952459248E-6,-6.43152286440645E-7,
0.999999999968002));
#127227=DIRECTION('center_axis',(-0.999999427244995,-0.0010702559647401,
-7.86457206393885E-6));
#127228=DIRECTION('ref_axis',(-0.000911792658579952,0.848044334090882,0.529924500330471));
#127229=DIRECTION('center_axis',(-1.4081690688991E-16,-6.98296267768627E-15,
1.));
#127230=DIRECTION('ref_axis',(-1.,8.07722881720021E-31,-1.42096112075504E-16));
#127231=DIRECTION('center_axis',(0.994628478131827,0.103509373458162,9.77058553911475E-6));
#127232=DIRECTION('ref_axis',(0.0905383273445441,-0.869943071289534,-0.484769908303914));
#127233=DIRECTION('center_axis',(-0.999999475000345,-0.00102464802306551,
9.77051628317655E-6));
#127234=DIRECTION('ref_axis',(0.000891471298448989,-0.874648786634207,-0.484756336026909));
#127235=DIRECTION('center_axis',(-1.4081690688991E-16,-6.98296267768627E-15,
1.));
#127236=DIRECTION('ref_axis',(-1.,8.24049048117772E-31,-1.37719829560012E-16));
#127237=DIRECTION('center_axis',(-0.994246940479907,-0.10711218892576,-1.81624797563042E-5));
#127238=DIRECTION('ref_axis',(0.0926692157706902,-0.860268013675041,0.50134953983827));
#127239=DIRECTION('center_axis',(0.999996624262643,-0.00259829454877719,
-1.81316452277342E-5));
#127240=DIRECTION('ref_axis',(0.00224363754548584,0.866978573811876,-0.49834036425087));
#127241=DIRECTION('center_axis',(-1.4081690688991E-16,-6.98296267768627E-15,
1.));
#127242=DIRECTION('ref_axis',(-1.,8.26087817385229E-31,-1.38060560438432E-16));
#127243=DIRECTION('center_axis',(-0.994245493086362,-0.107125623150708,
-1.84940598363496E-5));
#127244=DIRECTION('ref_axis',(0.092885154403067,-0.86199199692417,-0.498339387696979));
#127245=DIRECTION('center_axis',(0.999996589057285,-0.00261180600214046,
-1.85257108111962E-5));
#127246=DIRECTION('ref_axis',(0.00226914104442406,0.865242466403795,0.501348506859647));
#127247=DIRECTION('center_axis',(-1.4081690688991E-16,-6.98296267768627E-15,
1.));
#127248=DIRECTION('ref_axis',(-1.,9.83319205199467E-31,-1.40816906889911E-16));
#127249=DIRECTION('center_axis',(-1.4081690688991E-16,-6.98296267768627E-15,
1.));
#127250=DIRECTION('ref_axis',(-1.,8.46073526001725E-31,-1.4081690688991E-16));
#127251=DIRECTION('',(1.04744440165294E-14,-1.,-6.98296267768627E-15));
#127252=DIRECTION('center_axis',(-1.4081690688991E-16,-6.98296267768627E-15,
1.));
#127253=DIRECTION('ref_axis',(-1.,7.97077743482043E-31,-1.4081690688991E-16));
#127254=DIRECTION('center_axis',(-1.4081690688991E-16,-6.98296267768627E-15,
1.));
#127255=DIRECTION('ref_axis',(-1.,7.97077743482043E-31,-1.4081690688991E-16));
#127256=DIRECTION('center_axis',(-1.4081690688991E-16,-6.98296267768627E-15,
1.));
#127257=DIRECTION('ref_axis',(-1.,7.97077743482043E-31,-1.4081690688991E-16));
#127258=DIRECTION('',(0.104528463267644,0.994521895368274,6.95942865237777E-15));
#127259=DIRECTION('center_axis',(1.4081690688991E-16,6.98296267768627E-15,
-1.));
#127260=DIRECTION('ref_axis',(1.,-7.97077743482043E-31,1.4081690688991E-16));
#127261=DIRECTION('',(4.77800117084862E-6,-0.500005191251989,-0.866022406579779));
#127262=DIRECTION('center_axis',(1.4081690688991E-16,6.98296267768627E-15,
-1.));
#127263=DIRECTION('ref_axis',(-1.,1.15463194561016E-14,-1.4081690688983E-16));
#127264=DIRECTION('',(0.0522695260941882,0.497265611060784,0.86602240657978));
#127265=DIRECTION('center_axis',(-1.4081690688991E-16,-6.98296267768627E-15,
1.));
#127266=DIRECTION('ref_axis',(-1.,9.83319205199467E-31,-1.40816906889911E-16));
#127267=DIRECTION('center_axis',(-1.4081690688991E-16,-6.98296267768627E-15,
1.));
#127268=DIRECTION('ref_axis',(-1.,7.98248735348668E-31,-1.4081690688991E-16));
#127269=DIRECTION('',(1.04744440165294E-14,-1.,-6.98296267768627E-15));
#127270=DIRECTION('center_axis',(1.4081690688991E-16,6.98296267768627E-15,
-1.));
#127271=DIRECTION('ref_axis',(-1.,1.06581410364015E-14,-1.40816906889836E-16));
#127272=DIRECTION('',(0.104528463267644,0.994521895368274,6.95942865237777E-15));
#127273=DIRECTION('center_axis',(-1.4081690688991E-16,-6.98296267768627E-15,
1.));
#127274=DIRECTION('ref_axis',(-1.,7.99150043815584E-31,-1.4081690688991E-16));
#127275=DIRECTION('center_axis',(-1.4081690688991E-16,-6.98296267768627E-15,
1.));
#127276=DIRECTION('ref_axis',(1.,-2.1316282072803E-14,1.40816906889762E-16));
#127277=DIRECTION('',(-4.62770264722375E-6,-0.500004991781227,0.866022521746657));
#127278=DIRECTION('center_axis',(-1.4081690688991E-16,-6.98296267768627E-15,
1.));
#127279=DIRECTION('ref_axis',(-1.,7.99858039355471E-31,-1.4081690688991E-16));
#127280=DIRECTION('center_axis',(-1.4081690688991E-16,-6.98296267768627E-15,
1.));
#127281=DIRECTION('ref_axis',(-1.,7.99858039355471E-31,-1.4081690688991E-16));
#127282=DIRECTION('center_axis',(-1.4081690688991E-16,-6.98296267768627E-15,
1.));
#127283=DIRECTION('ref_axis',(-1.,7.99858039355471E-31,-1.4081690688991E-16));
#127284=DIRECTION('',(0.0522601510654249,0.497266395846527,-0.866022521746648));
#127285=DIRECTION('center_axis',(-1.4081690688991E-16,-6.98296267768627E-15,
1.));
#127286=DIRECTION('ref_axis',(-1.,9.83319205199467E-31,-1.40816906889911E-16));
#127287=DIRECTION('',(1.04744440165294E-14,-1.,-6.98296267768627E-15));
#127288=DIRECTION('center_axis',(1.4081690688991E-16,6.98296267768627E-15,
-1.));
#127289=DIRECTION('ref_axis',(-1.,-3.37507799486048E-14,-1.40816906890146E-16));
#127290=DIRECTION('',(0.104528463267644,0.994521895368274,6.95942865237777E-15));
#127291=DIRECTION('center_axis',(-1.4081690688991E-16,-6.98296267768627E-15,
1.));
#127292=DIRECTION('ref_axis',(-1.,8.32577322149061E-31,-1.39145123902276E-16));
#127293=DIRECTION('center_axis',(0.999999427244995,-0.00107025596495094,
-7.86457221374702E-6));
#127294=DIRECTION('ref_axis',(7.86300009144843E-6,-1.47312952164187E-6,
0.999999999968002));
#127295=DIRECTION('center_axis',(-0.994633197962196,0.103464010407696,-7.86457225038893E-6));
#127296=DIRECTION('ref_axis',(0.0877379732621199,0.843493966781832,0.529924500330476));
#127297=DIRECTION('center_axis',(-1.4081690688991E-16,-6.98296267768627E-15,
1.));
#127298=DIRECTION('ref_axis',(-1.,8.07722881720021E-31,-1.42096112075504E-16));
#127299=DIRECTION('center_axis',(0.999999475000305,-0.00102464806169038,
9.77058611739668E-6));
#127300=DIRECTION('ref_axis',(0.000891463458068991,0.874641264346569,0.484769908302008));
#127301=DIRECTION('center_axis',(-0.994628478127865,0.103509373496238,9.77051631878171E-6));
#127302=DIRECTION('ref_axis',(0.0905391058403046,0.869950553189083,0.484756336028366));
#127303=DIRECTION('center_axis',(-1.4081690688991E-16,-6.98296267768627E-15,
1.));
#127304=DIRECTION('ref_axis',(-1.,8.24049048117772E-31,-1.37719829560012E-16));
#127305=DIRECTION('center_axis',(-0.999996624215829,-0.00259831235054269,
-1.81624797931949E-5));
#127306=DIRECTION('ref_axis',(0.00223907064275388,-0.865241946200867,0.501349539839415));
#127307=DIRECTION('center_axis',(0.994246942387262,-0.107112171226359,-1.81316451653157E-5));
#127308=DIRECTION('ref_axis',(0.0928552846707127,0.861994650485525,-0.498340364252243));
#127309=DIRECTION('center_axis',(-1.4081690688991E-16,-6.98296267768627E-15,
1.));
#127310=DIRECTION('ref_axis',(-1.,8.26087817385229E-31,-1.38060560438432E-16));
#127311=DIRECTION('center_axis',(-0.999996589010146,-0.00261182427508556,
-1.84940601202704E-5));
#127312=DIRECTION('ref_axis',(0.00227362102101954,-0.866979057023569,-0.498339387696754));
#127313=DIRECTION('center_axis',(0.99424549504318,-0.107125604983779,-1.85257088094287E-5));
#127314=DIRECTION('ref_axis',(0.0926991758192284,0.860265387812633,0.501348506863256));
#127315=DIRECTION('center_axis',(-1.4081690688991E-16,-6.98296267768627E-15,
1.));
#127316=DIRECTION('ref_axis',(-1.,9.83319205199467E-31,-1.40816906889911E-16));
#127317=DIRECTION('center_axis',(-1.4081690688991E-16,-6.98296267768627E-15,
1.));
#127318=DIRECTION('ref_axis',(-1.,8.46073526001725E-31,-1.4081690688991E-16));
#127319=DIRECTION('',(-0.104528463267644,-0.994521895368274,-6.95942865237777E-15));
#127320=DIRECTION('center_axis',(-1.4081690688991E-16,-6.98296267768627E-15,
1.));
#127321=DIRECTION('ref_axis',(-1.,7.97077743482043E-31,-1.4081690688991E-16));
#127322=DIRECTION('center_axis',(-1.4081690688991E-16,-6.98296267768627E-15,
1.));
#127323=DIRECTION('ref_axis',(-1.,7.97077743482043E-31,-1.4081690688991E-16));
#127324=DIRECTION('center_axis',(-1.4081690688991E-16,-6.98296267768627E-15,
1.));
#127325=DIRECTION('ref_axis',(-1.,7.97077743482043E-31,-1.4081690688991E-16));
#127326=DIRECTION('',(0.207911690817749,0.978147600733808,6.85964567039975E-15));
#127327=DIRECTION('center_axis',(1.4081690688991E-16,6.98296267768627E-15,
-1.));
#127328=DIRECTION('ref_axis',(1.,-7.97077743482043E-31,1.4081690688991E-16));
#127329=DIRECTION('',(-0.0522600224406443,-0.497266609934999,-0.866022406579794));
#127330=DIRECTION('center_axis',(1.4081690688991E-16,6.98296267768627E-15,
-1.));
#127331=DIRECTION('ref_axis',(-1.,-3.37507799486048E-14,-1.40816906890146E-16));
#127332=DIRECTION('',(0.103961598321227,0.48907788477527,0.866022406579786));
#127333=DIRECTION('center_axis',(-1.4081690688991E-16,-6.98296267768627E-15,
1.));
#127334=DIRECTION('ref_axis',(-1.,9.83319205199467E-31,-1.40816906889911E-16));
#127335=DIRECTION('center_axis',(-1.4081690688991E-16,-6.98296267768627E-15,
1.));
#127336=DIRECTION('ref_axis',(-1.,7.98248735348668E-31,-1.4081690688991E-16));
#127337=DIRECTION('',(-0.104528463267644,-0.994521895368274,-6.95942865237777E-15));
#127338=DIRECTION('center_axis',(1.4081690688991E-16,6.98296267768627E-15,
-1.));
#127339=DIRECTION('ref_axis',(-1.,-3.46389583683049E-14,-1.40816906890152E-16));
#127340=DIRECTION('',(0.207911690817749,0.978147600733808,6.85964567039975E-15));
#127341=DIRECTION('center_axis',(-1.4081690688991E-16,-6.98296267768627E-15,
1.));
#127342=DIRECTION('ref_axis',(-1.,7.99150043815584E-31,-1.4081690688991E-16));
#127343=DIRECTION('center_axis',(-1.4081690688991E-16,-6.98296267768627E-15,
1.));
#127344=DIRECTION('ref_axis',(1.,-1.06581410364015E-14,1.40816906889836E-16));
#127345=DIRECTION('',(-0.0522693557686574,-0.497265428393217,0.866022521746658));
#127346=DIRECTION('center_axis',(-1.4081690688991E-16,-6.98296267768627E-15,
1.));
#127347=DIRECTION('ref_axis',(-1.,7.99858039355471E-31,-1.4081690688991E-16));
#127348=DIRECTION('center_axis',(-1.4081690688991E-16,-6.98296267768627E-15,
1.));
#127349=DIRECTION('ref_axis',(-1.,7.99858039355471E-31,-1.4081690688991E-16));
#127350=DIRECTION('center_axis',(-1.4081690688991E-16,-6.98296267768627E-15,
1.));
#127351=DIRECTION('ref_axis',(-1.,7.99858039355471E-31,-1.4081690688991E-16));
#127352=DIRECTION('',(0.103952356682307,0.489079645219225,-0.866022521746653));
#127353=DIRECTION('center_axis',(-1.4081690688991E-16,-6.98296267768627E-15,
1.));
#127354=DIRECTION('ref_axis',(-1.,9.83319205199467E-31,-1.40816906889911E-16));
#127355=DIRECTION('',(-0.104528463267644,-0.994521895368274,-6.95942865237777E-15));
#127356=DIRECTION('center_axis',(1.4081690688991E-16,6.98296267768627E-15,
-1.));
#127357=DIRECTION('ref_axis',(-1.,1.06581410364015E-14,-1.40816906889836E-16));
#127358=DIRECTION('',(0.207911690817749,0.978147600733808,6.85964567039975E-15));
#127359=DIRECTION('center_axis',(-1.4081690688991E-16,-6.98296267768627E-15,
1.));
#127360=DIRECTION('ref_axis',(-1.,8.32577322149061E-31,-1.39145123902276E-16));
#127361=DIRECTION('center_axis',(0.99440945353958,-0.105592796389062,-7.86457201213219E-6));
#127362=DIRECTION('ref_axis',(7.66594158482965E-6,-2.28696690243272E-6,
0.999999999968001));
#127363=DIRECTION('center_axis',(-0.978369559222146,0.206864703431039,-7.86457226808233E-6));
#127364=DIRECTION('ref_axis',(0.17542646358764,0.829702103060259,0.529924500330489));
#127365=DIRECTION('center_axis',(-1.4081690688991E-16,-6.98296267768627E-15,
1.));
#127366=DIRECTION('ref_axis',(-1.,8.07722881720021E-31,-1.42096112075504E-16));
#127367=DIRECTION('center_axis',(0.994414268357392,-0.1055474433218,9.77058458334715E-6));
#127368=DIRECTION('ref_axis',(0.0923114872004053,0.869756704678088,0.484769908305334));
#127369=DIRECTION('center_axis',(-0.978360123509283,0.206909324660436,9.77051334214024E-6));
#127370=DIRECTION('ref_axis',(0.180977717589009,0.855720959435413,0.484756336027916));
#127371=DIRECTION('center_axis',(-1.4081690688991E-16,-6.98296267768627E-15,
1.));
#127372=DIRECTION('ref_axis',(-1.,8.24049048117772E-31,-1.37719829560012E-16));
#127373=DIRECTION('center_axis',(-0.994790135674094,0.101944031878491,-1.81624797398355E-5));
#127374=DIRECTION('ref_axis',(0.0882156062112462,0.860736106898194,-0.501349539844731));
#127375=DIRECTION('center_axis',(0.977604082951528,-0.210452504541392,-1.81316452147401E-5));
#127376=DIRECTION('ref_axis',(0.182449589865955,0.847566533385627,-0.498340364251598));
#127377=DIRECTION('center_axis',(-1.4081690688991E-16,-6.98296267768627E-15,
1.));
#127378=DIRECTION('ref_axis',(-1.,8.26087817385229E-31,-1.38060560438432E-16));
#127379=DIRECTION('center_axis',(-0.994791513041971,0.101930590293766,-1.84940602080538E-5));
#127380=DIRECTION('ref_axis',(0.0883628226287454,0.862467313146972,0.498339387696903));
#127381=DIRECTION('center_axis',(0.977601239325912,-0.210465713419643,-1.85257069575344E-5));
#127382=DIRECTION('ref_axis',(0.182113579025951,0.845863061615953,0.501348506857301));
#127383=DIRECTION('center_axis',(-1.4081690688991E-16,-6.98296267768627E-15,
1.));
#127384=DIRECTION('ref_axis',(-1.,9.83319205199467E-31,-1.40816906889911E-16));
#127385=DIRECTION('center_axis',(-1.4081690688991E-16,-6.98296267768627E-15,
1.));
#127386=DIRECTION('ref_axis',(-1.,8.46073526001725E-31,-1.4081690688991E-16));
#127387=DIRECTION('',(-0.207911690817749,-0.978147600733808,-6.85964567039975E-15));
#127388=DIRECTION('center_axis',(-1.4081690688991E-16,-6.98296267768627E-15,
1.));
#127389=DIRECTION('ref_axis',(-1.,7.97077743482043E-31,-1.4081690688991E-16));
#127390=DIRECTION('center_axis',(-1.4081690688991E-16,-6.98296267768627E-15,
1.));
#127391=DIRECTION('ref_axis',(-1.,7.97077743482043E-31,-1.4081690688991E-16));
#127392=DIRECTION('center_axis',(-1.4081690688991E-16,-6.98296267768627E-15,
1.));
#127393=DIRECTION('ref_axis',(-1.,7.97077743482043E-31,-1.4081690688991E-16));
#127394=DIRECTION('',(0.309016994374938,0.951056516295157,6.68470697498369E-15));
#127395=DIRECTION('center_axis',(1.4081690688991E-16,6.98296267768627E-15,
-1.));
#127396=DIRECTION('ref_axis',(1.,-7.97077743482043E-31,1.4081690688991E-16));
#127397=DIRECTION('',(-0.103952251140481,-0.489079871579877,-0.866022406579782));
#127398=DIRECTION('center_axis',(1.4081690688991E-16,6.98296267768627E-15,
-1.));
#127399=DIRECTION('ref_axis',(-1.,-3.46389583683049E-14,-1.40816906890152E-16));
#127400=DIRECTION('',(0.154514645521708,0.475531718838049,0.866022406579779));
#127401=DIRECTION('center_axis',(-1.4081690688991E-16,-6.98296267768627E-15,
1.));
#127402=DIRECTION('ref_axis',(-1.,9.83319205199467E-31,-1.40816906889911E-16));
#127403=DIRECTION('center_axis',(-1.4081690688991E-16,-6.98296267768627E-15,
1.));
#127404=DIRECTION('ref_axis',(-1.,7.98248735348668E-31,-1.4081690688991E-16));
#127405=DIRECTION('',(-0.207911690817749,-0.978147600733808,-6.85964567039975E-15));
#127406=DIRECTION('center_axis',(1.4081690688991E-16,6.98296267768627E-15,
-1.));
#127407=DIRECTION('ref_axis',(-1.,-3.5527136788005E-14,-1.40816906890159E-16));
#127408=DIRECTION('',(0.309016994374938,0.951056516295157,6.6847069749837E-15));
#127409=DIRECTION('center_axis',(-1.4081690688991E-16,-6.98296267768627E-15,
1.));
#127410=DIRECTION('ref_axis',(-1.,7.99150043815584E-31,-1.4081690688991E-16));
#127411=DIRECTION('center_axis',(-1.4081690688991E-16,-6.98296267768627E-15,
1.));
#127412=DIRECTION('ref_axis',(1.,-1.06581410364015E-14,1.40816906889836E-16));
#127413=DIRECTION('',(-0.103961409834804,-0.489077720912242,0.866022521746662));
#127414=DIRECTION('center_axis',(-1.4081690688991E-16,-6.98296267768627E-15,
1.));
#127415=DIRECTION('ref_axis',(-1.,7.99858039355471E-31,-1.4081690688991E-16));
#127416=DIRECTION('center_axis',(-1.4081690688991E-16,-6.98296267768627E-15,
1.));
#127417=DIRECTION('ref_axis',(-1.,7.99858039355471E-31,-1.4081690688991E-16));
#127418=DIRECTION('center_axis',(-1.4081690688991E-16,-6.98296267768627E-15,
1.));
#127419=DIRECTION('ref_axis',(-1.,7.99858039355471E-31,-1.4081690688991E-16));
#127420=DIRECTION('',(0.154505638525955,0.475534435652384,-0.866022521746666));
#127421=DIRECTION('center_axis',(-1.4081690688991E-16,-6.98296267768627E-15,
1.));
#127422=DIRECTION('ref_axis',(-1.,9.83319205199467E-31,-1.40816906889911E-16));
#127423=DIRECTION('',(-0.207911690817749,-0.978147600733808,-6.85964567039975E-15));
#127424=DIRECTION('center_axis',(1.4081690688991E-16,6.98296267768627E-15,
-1.));
#127425=DIRECTION('ref_axis',(-1.,8.01265634860448E-31,-1.4081690688991E-16));
#127426=DIRECTION('',(0.309016994374938,0.951056516295157,6.68470697498369E-15));
#127427=DIRECTION('center_axis',(-1.4081690688991E-16,-6.98296267768627E-15,
1.));
#127428=DIRECTION('ref_axis',(-1.,8.32577322149061E-31,-1.39145123902276E-16));
#127429=DIRECTION('center_axis',(0.977924521767629,-0.208958440039405,-7.86457201251932E-6));
#127430=DIRECTION('ref_axis',(7.38489362573485E-6,-3.07574772033552E-6,
0.999999999968002));
#127431=DIRECTION('center_axis',(-0.951386698854271,0.307998943474359,-7.86457228732381E-6));
#127432=DIRECTION('ref_axis',(0.261192944867743,0.806819849471253,0.529924500330472));
#127433=DIRECTION('center_axis',(-1.4081690688991E-16,-6.98296267768627E-15,
1.));
#127434=DIRECTION('ref_axis',(-1.,8.07722881720021E-31,-1.42096112075504E-16));
#127435=DIRECTION('center_axis',(0.977934050896058,-0.208913838705245,9.77058218570699E-6));
#127436=DIRECTION('ref_axis',(0.182720126971887,0.855342908548084,0.484769908302775));
#127437=DIRECTION('center_axis',(-0.951372650642623,0.308042333963641,9.7705129532813E-6));
#127438=DIRECTION('ref_axis',(0.269433499592017,0.832115907779642,0.484756336026318));
#127439=DIRECTION('center_axis',(-1.4081690688991E-16,-6.98296267768627E-15,
1.));
#127440=DIRECTION('ref_axis',(-1.,8.24049048117772E-31,-1.37719829560012E-16));
#127441=DIRECTION('center_axis',(-0.978684518232678,0.205369455961189,-1.81624796489768E-5));
#127442=DIRECTION('ref_axis',(0.177703774423476,0.846799862691456,-0.501349539843592));
#127443=DIRECTION('center_axis',(0.950250388606183,-0.311487076176592,-1.81316452359128E-5));
#127444=DIRECTION('ref_axis',(0.270044939174893,0.823852299982039,-0.498340364249508));
#127445=DIRECTION('center_axis',(-1.4081690688991E-16,-6.98296267768627E-15,
1.));
#127446=DIRECTION('ref_axis',(-1.,8.26087817385229E-31,-1.38060560438432E-16));
#127447=DIRECTION('center_axis',(-0.978687293083712,0.205356231983462,-1.8494057605138E-5));
#127448=DIRECTION('ref_axis',(0.178031144702766,0.848506196905287,0.498339387695926));
#127449=DIRECTION('center_axis',(0.950246179855776,-0.311499915451519,-1.85257140792284E-5));
#127450=DIRECTION('ref_axis',(0.269532707750228,0.822193282702853,0.501348506860385));
#127451=DIRECTION('center_axis',(-1.4081690688991E-16,-6.98296267768627E-15,
1.));
#127452=DIRECTION('ref_axis',(-1.,9.83319205199467E-31,-1.40816906889911E-16));
#127453=DIRECTION('center_axis',(-1.4081690688991E-16,-6.98296267768627E-15,
1.));
#127454=DIRECTION('ref_axis',(-1.,8.46073526001725E-31,-1.4081690688991E-16));
#127455=DIRECTION('',(-0.309016994374938,-0.951056516295157,-6.68470697498369E-15));
#127456=DIRECTION('center_axis',(-1.4081690688991E-16,-6.98296267768627E-15,
1.));
#127457=DIRECTION('ref_axis',(-1.,7.97077743482043E-31,-1.4081690688991E-16));
#127458=DIRECTION('center_axis',(-1.4081690688991E-16,-6.98296267768627E-15,
1.));
#127459=DIRECTION('ref_axis',(-1.,7.97077743482043E-31,-1.4081690688991E-16));
#127460=DIRECTION('center_axis',(-1.4081690688991E-16,-6.98296267768627E-15,
1.));
#127461=DIRECTION('ref_axis',(-1.,7.97077743482043E-31,-1.4081690688991E-16));
#127462=DIRECTION('',(0.406736643075792,0.913545457642605,6.43652923108485E-15));
#127463=DIRECTION('center_axis',(1.4081690688991E-16,6.98296267768627E-15,
-1.));
#127464=DIRECTION('ref_axis',(1.,-7.97077743482043E-31,1.4081690688991E-16));
#127465=DIRECTION('',(-0.154505557223399,-0.475534671805183,-0.866022406579774));
#127466=DIRECTION('center_axis',(1.4081690688991E-16,6.98296267768627E-15,
-1.));
#127467=DIRECTION('ref_axis',(-1.,-3.5527136788005E-14,-1.40816906890159E-16));
#127468=DIRECTION('',(0.20337479793158,0.456775527877798,0.866022406579788));
#127469=DIRECTION('center_axis',(-1.4081690688991E-16,-6.98296267768627E-15,
1.));
#127470=DIRECTION('ref_axis',(-1.,9.83319205199467E-31,-1.40816906889911E-16));
#127471=DIRECTION('center_axis',(-1.4081690688991E-16,-6.98296267768627E-15,
1.));
#127472=DIRECTION('ref_axis',(-1.,7.98248735348668E-31,-1.4081690688991E-16));
#127473=DIRECTION('',(-0.309016994374938,-0.951056516295157,-6.68470697498369E-15));
#127474=DIRECTION('center_axis',(1.4081690688991E-16,6.98296267768627E-15,
-1.));
#127475=DIRECTION('ref_axis',(-1.,-3.5527136788005E-14,-1.40816906890159E-16));
#127476=DIRECTION('',(0.406736643075792,0.913545457642605,6.43652923108485E-15));
#127477=DIRECTION('center_axis',(-1.4081690688991E-16,-6.98296267768627E-15,
1.));
#127478=DIRECTION('ref_axis',(-1.,7.99150043815584E-31,-1.4081690688991E-16));
#127479=DIRECTION('center_axis',(-1.4081690688991E-16,-6.98296267768627E-15,
1.));
#127480=DIRECTION('ref_axis',(1.,1.95399252334028E-14,1.40816906890047E-16));
#127481=DIRECTION('',(-0.154514440939474,-0.47553157557486,0.866022521746665));
#127482=DIRECTION('center_axis',(-1.4081690688991E-16,-6.98296267768627E-15,
1.));
#127483=DIRECTION('ref_axis',(-1.,7.99858039355471E-31,-1.4081690688991E-16));
#127484=DIRECTION('center_axis',(-1.4081690688991E-16,-6.98296267768627E-15,
1.));
#127485=DIRECTION('ref_axis',(-1.,7.99858039355471E-31,-1.4081690688991E-16));
#127486=DIRECTION('center_axis',(-1.4081690688991E-16,-6.98296267768627E-15,
1.));
#127487=DIRECTION('ref_axis',(-1.,7.99858039355471E-31,-1.4081690688991E-16));
#127488=DIRECTION('',(0.203366124261502,0.456779171296608,-0.866022521746657));
#127489=DIRECTION('center_axis',(-1.4081690688991E-16,-6.98296267768627E-15,
1.));
#127490=DIRECTION('ref_axis',(-1.,9.83319205199467E-31,-1.40816906889911E-16));
#127491=DIRECTION('',(-0.309016994374938,-0.951056516295157,-6.68470697498369E-15));
#127492=DIRECTION('center_axis',(1.4081690688991E-16,6.98296267768627E-15,
-1.));
#127493=DIRECTION('ref_axis',(-1.,8.01265634860448E-31,-1.4081690688991E-16));
#127494=DIRECTION('',(0.406736643075792,0.913545457642605,6.43652923108485E-15));
#127495=DIRECTION('center_axis',(-1.4081690688991E-16,-6.98296267768627E-15,
1.));
#127496=DIRECTION('ref_axis',(-1.,8.32577322149061E-31,-1.39145123902276E-16));
#127497=DIRECTION('center_axis',(0.95072524429133,-0.310034691293313,-7.86457201063926E-6));
#127498=DIRECTION('ref_axis',(7.02293521503659E-6,-3.83083005362747E-6,
0.999999999968002));
#127499=DIRECTION('center_axis',(-0.91398024672327,0.405758682640087,-7.86457225127319E-6));
#127500=DIRECTION('ref_axis',(0.344097741585791,0.775097908773505,0.529924500330469));
#127501=DIRECTION('center_axis',(-1.4081690688991E-16,-6.98296267768627E-15,
1.));
#127502=DIRECTION('ref_axis',(-1.,8.07722881720021E-31,-1.42096112075504E-16));
#127503=DIRECTION('center_axis',(0.950739383326639,-0.309991330356541,9.77058507340801E-6));
#127504=DIRECTION('ref_axis',(0.27112684679534,0.831557796518516,0.484769908302987));
#127505=DIRECTION('center_axis',(-0.913961739928689,0.40580036699227,9.770515844718E-6));
#127506=DIRECTION('ref_axis',(0.354937311790399,0.799394020105167,0.484756336027807));
#127507=DIRECTION('center_axis',(-1.4081690688991E-16,-6.98296267768627E-15,
1.));
#127508=DIRECTION('ref_axis',(-1.,8.24049048117772E-31,-1.37719829560012E-16));
#127509=DIRECTION('center_axis',(-0.95185622840662,0.306544809307952,-1.81624796959471E-5));
#127510=DIRECTION('ref_axis',(0.265244982896756,0.8235859019861,-0.501349539840062));
#127511=DIRECTION('center_axis',(0.912485552150601,-0.409108930222327,-1.81316452377115E-5));
#127512=DIRECTION('ref_axis',(0.354681619619059,0.791111768375658,-0.498340364251122));
#127513=DIRECTION('center_axis',(-1.4081690688991E-16,-6.98296267768627E-15,
1.));
#127514=DIRECTION('ref_axis',(-1.,8.26087817385229E-31,-1.38060560438432E-16));
#127515=DIRECTION('center_axis',(-0.951860370340164,0.306531947819237,-1.84940498087876E-5));
#127516=DIRECTION('ref_axis',(0.265748920300266,0.825248669209326,0.498339387694248));
#127517=DIRECTION('center_axis',(0.912480024383678,-0.409121259234423,-1.85257023388232E-5));
#127518=DIRECTION('ref_axis',(0.3539987797255,0.789515382131315,0.501348506860148));
#127519=DIRECTION('center_axis',(-1.4081690688991E-16,-6.98296267768627E-15,
1.));
#127520=DIRECTION('ref_axis',(-1.,9.83319205199467E-31,-1.40816906889911E-16));
#127521=DIRECTION('center_axis',(-1.4081690688991E-16,-6.98296267768627E-15,
1.));
#127522=DIRECTION('ref_axis',(-1.,8.46073526001725E-31,-1.4081690688991E-16));
#127523=DIRECTION('',(-0.406736643075792,-0.913545457642605,-6.43652923108485E-15));
#127524=DIRECTION('center_axis',(-1.4081690688991E-16,-6.98296267768627E-15,
1.));
#127525=DIRECTION('ref_axis',(-1.,7.97077743482043E-31,-1.4081690688991E-16));
#127526=DIRECTION('center_axis',(-1.4081690688991E-16,-6.98296267768627E-15,
1.));
#127527=DIRECTION('ref_axis',(-1.,7.97077743482043E-31,-1.4081690688991E-16));
#127528=DIRECTION('center_axis',(-1.4081690688991E-16,-6.98296267768627E-15,
1.));
#127529=DIRECTION('ref_axis',(-1.,7.97077743482043E-31,-1.4081690688991E-16));
#127530=DIRECTION('',(0.499999999999992,0.866025403784443,6.1178315259999E-15));
#127531=DIRECTION('center_axis',(1.4081690688991E-16,6.98296267768627E-15,
-1.));
#127532=DIRECTION('ref_axis',(1.,-7.97077743482043E-31,1.4081690688991E-16));
#127533=DIRECTION('',(-0.203366068089011,-0.456779414654115,-0.866022406579795));
#127534=DIRECTION('center_axis',(1.4081690688991E-16,6.98296267768627E-15,
-1.));
#127535=DIRECTION('ref_axis',(-1.,1.24344978758018E-14,-1.40816906889824E-16));
#127536=DIRECTION('',(0.250006733496394,0.433014808647735,0.866022406579777));
#127537=DIRECTION('center_axis',(-1.4081690688991E-16,-6.98296267768627E-15,
1.));
#127538=DIRECTION('ref_axis',(-1.,9.83319205199467E-31,-1.40816906889911E-16));
#127539=DIRECTION('center_axis',(-1.4081690688991E-16,-6.98296267768627E-15,
1.));
#127540=DIRECTION('ref_axis',(-1.,7.98248735348668E-31,-1.4081690688991E-16));
#127541=DIRECTION('',(-0.406736643075792,-0.913545457642605,-6.43652923108485E-15));
#127542=DIRECTION('center_axis',(1.4081690688991E-16,6.98296267768627E-15,
-1.));
#127543=DIRECTION('ref_axis',(-1.,1.15463194561016E-14,-1.4081690688983E-16));
#127544=DIRECTION('',(0.499999999999992,0.866025403784443,6.1178315259999E-15));
#127545=DIRECTION('center_axis',(-1.4081690688991E-16,-6.98296267768627E-15,
1.));
#127546=DIRECTION('ref_axis',(-1.,7.99150043815584E-31,-1.4081690688991E-16));
#127547=DIRECTION('center_axis',(-1.4081690688991E-16,-6.98296267768627E-15,
1.));
#127548=DIRECTION('ref_axis',(1.,-1.95399252334028E-14,1.40816906889774E-16));
#127549=DIRECTION('',(-0.203374579494986,-0.456775406784097,0.866022521746669));
#127550=DIRECTION('center_axis',(-1.4081690688991E-16,-6.98296267768627E-15,
1.));
#127551=DIRECTION('ref_axis',(-1.,7.99858039355471E-31,-1.4081690688991E-16));
#127552=DIRECTION('center_axis',(-1.4081690688991E-16,-6.98296267768627E-15,
1.));
#127553=DIRECTION('ref_axis',(-1.,7.99858039355471E-31,-1.4081690688991E-16));
#127554=DIRECTION('center_axis',(-1.4081690688991E-16,-6.98296267768627E-15,
1.));
#127555=DIRECTION('ref_axis',(-1.,7.99858039355471E-31,-1.4081690688991E-16));
#127556=DIRECTION('',(0.249998488182543,0.433019338752906,-0.866022521746657));
#127557=DIRECTION('center_axis',(-1.4081690688991E-16,-6.98296267768627E-15,
1.));
#127558=DIRECTION('ref_axis',(-1.,9.83319205199467E-31,-1.40816906889911E-16));
#127559=DIRECTION('',(-0.406736643075792,-0.913545457642605,-6.43652923108485E-15));
#127560=DIRECTION('center_axis',(1.4081690688991E-16,6.98296267768627E-15,
-1.));
#127561=DIRECTION('ref_axis',(-1.,8.01265634860448E-31,-1.4081690688991E-16));
#127562=DIRECTION('',(0.499999999999992,0.866025403784443,6.1178315259999E-15));
#127563=DIRECTION('center_axis',(-1.4081690688991E-16,-6.98296267768627E-15,
1.));
#127564=DIRECTION('ref_axis',(-1.,8.32577322149061E-31,-1.39145123902276E-16));
#127565=DIRECTION('center_axis',(0.913109622086517,-0.407714137590502,-7.86457206372106E-6));
#127566=DIRECTION('ref_axis',(6.584032128358E-6,-4.54394098313704E-6,0.999999999968002));
#127567=DIRECTION('center_axis',(-0.866560035746507,0.499072844768338,-7.8645722123473E-6));
#127568=DIRECTION('ref_axis',(0.423232531439936,0.734883833187554,0.529924500330482));
#127569=DIRECTION('center_axis',(-1.4081690688991E-16,-6.98296267768627E-15,
1.));
#127570=DIRECTION('ref_axis',(-1.,8.07722881720021E-31,-1.42096112075504E-16));
#127571=DIRECTION('center_axis',(0.913128216118261,-0.407672492122314,9.77058748990148E-6));
#127572=DIRECTION('ref_axis',(0.356563044148465,0.798661963255786,0.484769908302891));
#127573=DIRECTION('center_axis',(-0.866537273131149,0.499112366285359,9.77050983173774E-6));
#127574=DIRECTION('ref_axis',(0.436552356526714,0.757913804265093,0.484756336023973));
#127575=DIRECTION('center_axis',(-1.4081690688991E-16,-6.98296267768627E-15,
1.));
#127576=DIRECTION('ref_axis',(-1.,8.24049048117772E-31,-1.37719829560012E-16));
#127577=DIRECTION('center_axis',(-0.914599202553454,0.404361593575243,-1.81624798752258E-5));
#127578=DIRECTION('ref_axis',(0.349880111830903,0.791348561790119,-0.501349539840125));
#127579=DIRECTION('center_axis',(0.864723333035747,-0.502248501217069,-1.81316451772243E-5));
#127580=DIRECTION('ref_axis',(0.435432334017907,0.749703650686303,-0.49834036424852));
#127581=DIRECTION('center_axis',(-1.4081690688991E-16,-6.98296267768627E-15,
1.));
#127582=DIRECTION('ref_axis',(-1.,8.26087817385229E-31,-1.38060560438432E-16));
#127583=DIRECTION('center_axis',(-0.914604666190226,0.404349235489615,-1.84940430890388E-5));
#127584=DIRECTION('ref_axis',(0.350555095114317,0.792949544396151,0.498339387698112));
#127585=DIRECTION('center_axis',(0.864716546819225,-0.502260184878149,-1.85257070796717E-5));
#127586=DIRECTION('ref_axis',(0.434586366990895,0.748187385816106,0.501348506860563));
#127587=DIRECTION('center_axis',(-1.4081690688991E-16,-6.98296267768627E-15,
1.));
#127588=DIRECTION('ref_axis',(-1.,9.83319205199467E-31,-1.40816906889911E-16));
#127589=DIRECTION('center_axis',(-1.4081690688991E-16,-6.98296267768627E-15,
1.));
#127590=DIRECTION('ref_axis',(-1.,8.46073526001725E-31,-1.4081690688991E-16));
#127591=DIRECTION('',(-0.499999999999992,-0.866025403784443,-6.1178315259999E-15));
#127592=DIRECTION('center_axis',(-1.4081690688991E-16,-6.98296267768627E-15,
1.));
#127593=DIRECTION('ref_axis',(-1.,7.97077743482043E-31,-1.4081690688991E-16));
#127594=DIRECTION('center_axis',(-1.4081690688991E-16,-6.98296267768627E-15,
1.));
#127595=DIRECTION('ref_axis',(-1.,7.97077743482043E-31,-1.4081690688991E-16));
#127596=DIRECTION('center_axis',(-1.4081690688991E-16,-6.98296267768627E-15,
1.));
#127597=DIRECTION('ref_axis',(-1.,7.97077743482043E-31,-1.4081690688991E-16));
#127598=DIRECTION('',(0.587785252292466,0.809016994374953,5.73210557847754E-15));
#127599=DIRECTION('center_axis',(1.4081690688991E-16,6.98296267768627E-15,
-1.));
#127600=DIRECTION('ref_axis',(1.,-7.97077743482043E-31,1.4081690688991E-16));
#127601=DIRECTION('',(-0.249998457755584,-0.433019586648885,-0.866022406579794));
#127602=DIRECTION('center_axis',(1.4081690688991E-16,6.98296267768627E-15,
-1.));
#127603=DIRECTION('ref_axis',(-1.,-3.10862446895044E-14,-1.40816906890128E-16));
#127604=DIRECTION('',(0.29389954297172,0.404509888559958,0.866022406579775));
#127605=DIRECTION('center_axis',(-1.4081690688991E-16,-6.98296267768627E-15,
1.));
#127606=DIRECTION('ref_axis',(-1.,9.83319205199467E-31,-1.40816906889911E-16));
#127607=DIRECTION('center_axis',(-1.4081690688991E-16,-6.98296267768627E-15,
1.));
#127608=DIRECTION('ref_axis',(-1.,7.98248735348668E-31,-1.4081690688991E-16));
#127609=DIRECTION('',(-0.499999999999992,-0.866025403784443,-6.1178315259999E-15));
#127610=DIRECTION('center_axis',(1.4081690688991E-16,6.98296267768627E-15,
-1.));
#127611=DIRECTION('ref_axis',(-1.,-3.01980662698043E-14,-1.40816906890121E-16));
#127612=DIRECTION('',(0.587785252292466,0.809016994374953,5.73210557847754E-15));
#127613=DIRECTION('center_axis',(-1.4081690688991E-16,-6.98296267768627E-15,
1.));
#127614=DIRECTION('ref_axis',(-1.,7.99150043815584E-31,-1.4081690688991E-16));
#127615=DIRECTION('center_axis',(-1.4081690688991E-16,-6.98296267768627E-15,
1.));
#127616=DIRECTION('ref_axis',(1.,-1.95399252334028E-14,1.40816906889774E-16));
#127617=DIRECTION('',(-0.250006503598662,-0.433014711050211,0.866022521746677));
#127618=DIRECTION('center_axis',(-1.4081690688991E-16,-6.98296267768627E-15,
1.));
#127619=DIRECTION('ref_axis',(-1.,7.99858039355471E-31,-1.4081690688991E-16));
#127620=DIRECTION('center_axis',(-1.4081690688991E-16,-6.98296267768627E-15,
1.));
#127621=DIRECTION('ref_axis',(-1.,7.99858039355471E-31,-1.4081690688991E-16));
#127622=DIRECTION('center_axis',(-1.4081690688991E-16,-6.98296267768627E-15,
1.));
#127623=DIRECTION('ref_axis',(-1.,7.99858039355471E-31,-1.4081690688991E-16));
#127624=DIRECTION('',(0.293891816351498,0.404515255718706,-0.866022521746661));
#127625=DIRECTION('center_axis',(-1.4081690688991E-16,-6.98296267768627E-15,
1.));
#127626=DIRECTION('ref_axis',(-1.,9.83319205199467E-31,-1.40816906889911E-16));
#127627=DIRECTION('',(-0.499999999999992,-0.866025403784443,-6.1178315259999E-15));
#127628=DIRECTION('center_axis',(1.4081690688991E-16,6.98296267768627E-15,
-1.));
#127629=DIRECTION('ref_axis',(-1.,6.21724893790088E-15,-1.40816906889867E-16));
#127630=DIRECTION('',(0.587785252292466,0.809016994374953,5.73210557847754E-15));
#127631=DIRECTION('center_axis',(-1.4081690688991E-16,-6.98296267768627E-15,
1.));
#127632=DIRECTION('ref_axis',(-1.,8.32577322149061E-31,-1.39145123902276E-16));
#127633=DIRECTION('center_axis',(0.865489779781638,-0.500926582476595,-7.86457211857109E-6));
#127634=DIRECTION('ref_axis',(6.07299298702999E-6,-5.20726759105563E-6,
0.999999999968002));
#127635=DIRECTION('center_axis',(-0.809645611678775,0.586919060371574,-7.86457229727694E-6));
#127636=DIRECTION('ref_axis',(0.497730297112449,0.686618216540942,0.529924500330461));
#127637=DIRECTION('center_axis',(-1.4081690688991E-16,-6.98296267768627E-15,
1.));
#127638=DIRECTION('ref_axis',(-1.,8.07722881720021E-31,-1.42096112075504E-16));
#127639=DIRECTION('center_axis',(0.865512625090237,-0.500887108752004,9.77058713545332E-6));
#127640=DIRECTION('ref_axis',(0.438092662173875,0.757015822392123,0.484769908304326));
#127641=DIRECTION('center_axis',(-0.809618842639359,0.586955986039705,9.77052025762384E-6));
#127642=DIRECTION('ref_axis',(0.513384442288844,0.70812972617887,0.484756336026268));
#127643=DIRECTION('center_axis',(-1.4081690688991E-16,-6.98296267768627E-15,
1.));
#127644=DIRECTION('ref_axis',(-1.,8.24049048117772E-31,-1.37719829560012E-16));
#127645=DIRECTION('center_axis',(-0.867321636444838,0.497748107605415,-1.81624797475569E-5));
#127646=DIRECTION('ref_axis',(0.430681881043011,0.75044104115131,-0.501349539839213));
#127647=DIRECTION('center_axis',(0.807487024129225,-0.589885332530122,-1.81316451447921E-5));
#127648=DIRECTION('ref_axis',(0.511412360644474,0.700081622913156,-0.4983403642485));
#127649=DIRECTION('center_axis',(-1.4081690688991E-16,-6.98296267768627E-15,
1.));
#127650=DIRECTION('ref_axis',(-1.,8.26087817385229E-31,-1.38060560438432E-16));
#127651=DIRECTION('center_axis',(-0.867328361918079,0.49773638833269,-1.8494060228585E-5));
#127652=DIRECTION('ref_axis',(0.431520514947816,0.751962698439911,0.498339387700931));
#127653=DIRECTION('center_axis',(0.807479053808643,-0.589896242840296,-1.85256939485199E-5));
#127654=DIRECTION('ref_axis',(0.510412535076595,0.69866209193385,0.501348506860547));
#127655=DIRECTION('center_axis',(-1.4081690688991E-16,-6.98296267768627E-15,
1.));
#127656=DIRECTION('ref_axis',(-1.,9.83319205199467E-31,-1.40816906889911E-16));
#127657=DIRECTION('center_axis',(-1.4081690688991E-16,-6.98296267768627E-15,
1.));
#127658=DIRECTION('ref_axis',(-1.,8.46073526001725E-31,-1.4081690688991E-16));
#127659=DIRECTION('',(-0.587785252292466,-0.809016994374953,-5.73210557847754E-15));
#127660=DIRECTION('center_axis',(-1.4081690688991E-16,-6.98296267768627E-15,
1.));
#127661=DIRECTION('ref_axis',(-1.,7.97077743482043E-31,-1.4081690688991E-16));
#127662=DIRECTION('center_axis',(-1.4081690688991E-16,-6.98296267768627E-15,
1.));
#127663=DIRECTION('ref_axis',(-1.,7.97077743482043E-31,-1.4081690688991E-16));
#127664=DIRECTION('center_axis',(-1.4081690688991E-16,-6.98296267768627E-15,
1.));
#127665=DIRECTION('ref_axis',(-1.,7.97077743482043E-31,-1.4081690688991E-16));
#127666=DIRECTION('',(0.669130606358852,0.7431448254774,5.28357748271718E-15));
#127667=DIRECTION('center_axis',(1.4081690688991E-16,6.98296267768627E-15,
-1.));
#127668=DIRECTION('ref_axis',(1.,-7.97077743482043E-31,1.4081690688991E-16));
#127669=DIRECTION('',(-0.293891812003427,-0.40451550543717,-0.866022406579791));
#127670=DIRECTION('center_axis',(1.4081690688991E-16,6.98296267768627E-15,
-1.));
#127671=DIRECTION('ref_axis',(-1.,-1.24344978758018E-14,-1.40816906889997E-16));
#127672=DIRECTION('',(0.334572327551836,0.371573073483924,0.866022406579794));
#127673=DIRECTION('center_axis',(-1.4081690688991E-16,-6.98296267768627E-15,
1.));
#127674=DIRECTION('ref_axis',(-1.,9.83319205199467E-31,-1.40816906889911E-16));
#127675=DIRECTION('center_axis',(-1.4081690688991E-16,-6.98296267768627E-15,
1.));
#127676=DIRECTION('ref_axis',(-1.,7.98248735348668E-31,-1.4081690688991E-16));
#127677=DIRECTION('',(-0.587785252292466,-0.809016994374953,-5.73210557847754E-15));
#127678=DIRECTION('center_axis',(1.4081690688991E-16,6.98296267768627E-15,
-1.));
#127679=DIRECTION('ref_axis',(-1.,-1.86517468137026E-14,-1.40816906890041E-16));
#127680=DIRECTION('',(0.669130606358852,0.7431448254774,5.28357748271718E-15));
#127681=DIRECTION('center_axis',(-1.4081690688991E-16,-6.98296267768627E-15,
1.));
#127682=DIRECTION('ref_axis',(-1.,7.99150043815584E-31,-1.4081690688991E-16));
#127683=DIRECTION('center_axis',(-1.4081690688991E-16,-6.98296267768627E-15,
1.));
#127684=DIRECTION('ref_axis',(1.,-7.99370576998456E-31,1.4081690688991E-16));
#127685=DIRECTION('',(-0.293899304131726,-0.404509815527901,0.866022521746675));
#127686=DIRECTION('center_axis',(-1.4081690688991E-16,-6.98296267768627E-15,
1.));
#127687=DIRECTION('ref_axis',(-1.,7.99858039355471E-31,-1.4081690688991E-16));
#127688=DIRECTION('center_axis',(-1.4081690688991E-16,-6.98296267768627E-15,
1.));
#127689=DIRECTION('ref_axis',(-1.,7.99858039355471E-31,-1.4081690688991E-16));
#127690=DIRECTION('center_axis',(-1.4081690688991E-16,-6.98296267768627E-15,
1.));
#127691=DIRECTION('ref_axis',(-1.,7.99858039355471E-31,-1.4081690688991E-16));
#127692=DIRECTION('',(0.334565204279777,0.371579218892523,-0.866022521746665));
#127693=DIRECTION('center_axis',(-1.4081690688991E-16,-6.98296267768627E-15,
1.));
#127694=DIRECTION('ref_axis',(-1.,9.83319205199467E-31,-1.40816906889911E-16));
#127695=DIRECTION('',(-0.587785252292466,-0.809016994374953,-5.73210557847754E-15));
#127696=DIRECTION('center_axis',(1.4081690688991E-16,6.98296267768627E-15,
-1.));
#127697=DIRECTION('ref_axis',(-1.,-2.48689957516035E-14,-1.40816906890084E-16));
#127698=DIRECTION('',(0.669130606358852,0.7431448254774,5.28357748271718E-15));
#127699=DIRECTION('center_axis',(-1.4081690688991E-16,-6.98296267768627E-15,
1.));
#127700=DIRECTION('ref_axis',(-1.,8.32577322149061E-31,-1.39145123902276E-16));
#127701=DIRECTION('center_axis',(0.808387450334157,-0.588650770899341,-7.86457196308693E-6));
#127702=DIRECTION('ref_axis',(5.49541666557491E-6,-5.81354219714192E-6,
0.999999999968002));
#127703=DIRECTION('center_axis',(-0.743860540860235,0.668334867928696,-7.86457222760781E-6));
#127704=DIRECTION('ref_axis',(0.566774825493132,0.630829867029739,0.529924500330445));
#127705=DIRECTION('center_axis',(-1.4081690688991E-16,-6.98296267768627E-15,
1.));
#127706=DIRECTION('ref_axis',(-1.,8.07722881720021E-31,-1.42096112075504E-16));
#127707=DIRECTION('center_axis',(0.808414296620605,-0.588613901402225,9.77058976039386E-6));
#127708=DIRECTION('ref_axis',(0.514822445316446,0.707075657763804,0.484769908303186));
#127709=DIRECTION('center_axis',(-0.743830058679867,0.668368793188942,9.77051703262605E-6));
#127710=DIRECTION('ref_axis',(0.58459178066967,0.650587230628417,0.484756336025339));
#127711=DIRECTION('center_axis',(-1.4081690688991E-16,-6.98296267768627E-15,
1.));
#127712=DIRECTION('ref_axis',(-1.,8.24049048117772E-31,-1.37719829560012E-16));
#127713=DIRECTION('center_axis',(-0.810541512988669,0.585681189208057,-1.81624797215642E-5));
#127714=DIRECTION('ref_axis',(0.506765009439602,0.701311531424528,-0.501349539840881));
#127715=DIRECTION('center_axis',(0.741403718408774,-0.671059256698607,-1.81316451549613E-5));
#127716=DIRECTION('ref_axis',(0.581789246428761,0.642789354378738,-0.498340364246385));
#127717=DIRECTION('center_axis',(-1.4081690688991E-16,-6.98296267768627E-15,
1.));
#127718=DIRECTION('ref_axis',(-1.,8.26087817385229E-31,-1.38060560438432E-16));
#127719=DIRECTION('center_axis',(-0.810549426627886,0.585670237122544,-1.84940269143515E-5));
#127720=DIRECTION('ref_axis',(0.507758105719755,0.702737191804305,0.498339387697667));
#127721=DIRECTION('center_axis',(0.741394651314913,-0.671069274112917,-1.85257001779312E-5));
#127722=DIRECTION('ref_axis',(0.580646516616626,0.641482109967152,0.501348506862311));
#127723=DIRECTION('center_axis',(-1.4081690688991E-16,-6.98296267768627E-15,
1.));
#127724=DIRECTION('ref_axis',(-1.,9.83319205199467E-31,-1.40816906889911E-16));
#127725=DIRECTION('center_axis',(-1.4081690688991E-16,-6.98296267768627E-15,
1.));
#127726=DIRECTION('ref_axis',(-1.,8.46073526001725E-31,-1.4081690688991E-16));
#127727=DIRECTION('',(-0.669130606358852,-0.7431448254774,-5.28357748271718E-15));
#127728=DIRECTION('center_axis',(-1.4081690688991E-16,-6.98296267768627E-15,
1.));
#127729=DIRECTION('ref_axis',(-1.,7.97077743482043E-31,-1.4081690688991E-16));
#127730=DIRECTION('center_axis',(-1.4081690688991E-16,-6.98296267768627E-15,
1.));
#127731=DIRECTION('ref_axis',(-1.,7.97077743482043E-31,-1.4081690688991E-16));
#127732=DIRECTION('center_axis',(-1.4081690688991E-16,-6.98296267768627E-15,
1.));
#127733=DIRECTION('ref_axis',(-1.,7.97077743482043E-31,-1.4081690688991E-16));
#127734=DIRECTION('',(0.743144825477389,0.669130606358864,4.7771614063965E-15));
#127735=DIRECTION('center_axis',(1.4081690688991E-16,6.98296267768627E-15,
-1.));
#127736=DIRECTION('ref_axis',(1.,-7.97077743482043E-31,1.4081690688991E-16));
#127737=DIRECTION('',(-0.334565226058174,-0.371579467697563,-0.866022406579783));
#127738=DIRECTION('center_axis',(1.4081690688991E-16,6.98296267768627E-15,
-1.));
#127739=DIRECTION('ref_axis',(-1.,-7.105427357601E-15,-1.4081690688996E-16));
#127740=DIRECTION('',(0.371579467697516,0.334565226058181,0.8660224065798));
#127741=DIRECTION('center_axis',(-1.4081690688991E-16,-6.98296267768627E-15,
1.));
#127742=DIRECTION('ref_axis',(-1.,9.83319205199467E-31,-1.40816906889911E-16));
#127743=DIRECTION('center_axis',(-1.4081690688991E-16,-6.98296267768627E-15,
1.));
#127744=DIRECTION('ref_axis',(-1.,7.98248735348668E-31,-1.4081690688991E-16));
#127745=DIRECTION('',(-0.669130606358852,-0.7431448254774,-5.28357748271718E-15));
#127746=DIRECTION('center_axis',(1.4081690688991E-16,6.98296267768627E-15,
-1.));
#127747=DIRECTION('ref_axis',(-1.,-1.24344978758018E-14,-1.40816906889997E-16));
#127748=DIRECTION('',(0.743144825477389,0.669130606358864,4.7771614063965E-15));
#127749=DIRECTION('center_axis',(-1.4081690688991E-16,-6.98296267768627E-15,
1.));
#127750=DIRECTION('ref_axis',(-1.,7.99150043815584E-31,-1.4081690688991E-16));
#127751=DIRECTION('center_axis',(-1.4081690688991E-16,-6.98296267768627E-15,
1.));
#127752=DIRECTION('ref_axis',(1.,-7.99370576998456E-31,1.4081690688991E-16));
#127753=DIRECTION('',(-0.334572082386297,-0.3715730258176,0.866022521746663));
#127754=DIRECTION('center_axis',(-1.4081690688991E-16,-6.98296267768627E-15,
1.));
#127755=DIRECTION('ref_axis',(-1.,7.99858039355471E-31,-1.4081690688991E-16));
#127756=DIRECTION('center_axis',(-1.4081690688991E-16,-6.98296267768627E-15,
1.));
#127757=DIRECTION('ref_axis',(-1.,7.99858039355471E-31,-1.4081690688991E-16));
#127758=DIRECTION('center_axis',(-1.4081690688991E-16,-6.98296267768627E-15,
1.));
#127759=DIRECTION('ref_axis',(-1.,7.99858039355471E-31,-1.4081690688991E-16));
#127760=DIRECTION('',(0.371573025817624,0.334572082386294,-0.866022521746654));
#127761=DIRECTION('center_axis',(-1.4081690688991E-16,-6.98296267768627E-15,
1.));
#127762=DIRECTION('ref_axis',(-1.,9.83319205199467E-31,-1.40816906889911E-16));
#127763=DIRECTION('',(-0.669130606358852,-0.7431448254774,-5.28357748271718E-15));
#127764=DIRECTION('center_axis',(1.4081690688991E-16,6.98296267768627E-15,
-1.));
#127765=DIRECTION('ref_axis',(-1.,3.19744231092045E-14,-1.40816906889687E-16));
#127766=DIRECTION('',(0.743144825477389,0.669130606358864,4.7771614063965E-15));
#127767=DIRECTION('center_axis',(-1.4081690688991E-16,-6.98296267768627E-15,
1.));
#127768=DIRECTION('ref_axis',(-1.,8.32577322149061E-31,-1.39145123902276E-16));
#127769=DIRECTION('center_axis',(0.742428258814862,-0.669925578293053,-7.86457193367171E-6));
#127770=DIRECTION('ref_axis',(4.85763156055902E-6,-6.35612241976888E-6,
0.999999999968002));
#127771=DIRECTION('center_axis',(-0.669925578293245,0.742428258814688,-7.8645722999317E-6));
#127772=DIRECTION('ref_axis',(0.62960965028034,0.568130013485787,0.529924500330479));
#127773=DIRECTION('center_axis',(-1.4081690688991E-16,-6.98296267768627E-15,
1.));
#127774=DIRECTION('ref_axis',(-1.,8.07722881720021E-31,-1.42096112075504E-16));
#127775=DIRECTION('center_axis',(0.742458811944968,-0.669891716973573,9.77059356059858E-6));
#127776=DIRECTION('ref_axis',(0.58591172601474,0.649388624263935,0.484769908301889));
#127777=DIRECTION('center_axis',(-0.669891716941096,0.742458811974272,9.77051458249057E-6));
#127778=DIRECTION('ref_axis',(0.649394209167476,0.585916765234689,0.484756336025292));
#127779=DIRECTION('center_axis',(-1.4081690688991E-16,-6.98296267768627E-15,
1.));
#127780=DIRECTION('ref_axis',(-1.,8.24049048117772E-31,-1.37719829560012E-16));
#127781=DIRECTION('center_axis',(-0.744880927099486,0.667197425140066,-1.81624797614567E-5));
#127782=DIRECTION('ref_axis',(0.577295914344388,0.644498305799741,-0.501349539844748));
#127783=DIRECTION('center_axis',(0.667197438400691,-0.74488091522256,-1.81316453281971E-5));
#127784=DIRECTION('ref_axis',(0.645791927480724,0.578454551164035,-0.498340364247516));
#127785=DIRECTION('center_axis',(-1.4081690688991E-16,-6.98296267768627E-15,
1.));
#127786=DIRECTION('ref_axis',(-1.,8.26087817385229E-31,-1.38060560438432E-16));
#127787=DIRECTION('center_axis',(-0.744889942180744,0.66718736026392,-1.84940550609695E-5));
#127788=DIRECTION('ref_axis',(0.578432592428213,0.645812349435011,0.4983393877008));
#127789=DIRECTION('center_axis',(0.667187373873416,-0.744889929990125,-1.85257023897959E-5));
#127790=DIRECTION('ref_axis',(0.644518813414346,0.577273915766852,0.501348506859419));
#127791=DIRECTION('center_axis',(-1.4081690688991E-16,-6.98296267768627E-15,
1.));
#127792=DIRECTION('ref_axis',(-1.,9.83319205199467E-31,-1.40816906889911E-16));
#127793=DIRECTION('center_axis',(-1.4081690688991E-16,-6.98296267768627E-15,
1.));
#127794=DIRECTION('ref_axis',(-1.,8.46073526001725E-31,-1.4081690688991E-16));
#127795=DIRECTION('',(-0.743144825477389,-0.669130606358864,-4.7771614063965E-15));
#127796=DIRECTION('center_axis',(-1.4081690688991E-16,-6.98296267768627E-15,
1.));
#127797=DIRECTION('ref_axis',(-1.,7.97077743482043E-31,-1.4081690688991E-16));
#127798=DIRECTION('center_axis',(-1.4081690688991E-16,-6.98296267768627E-15,
1.));
#127799=DIRECTION('ref_axis',(-1.,7.97077743482043E-31,-1.4081690688991E-16));
#127800=DIRECTION('center_axis',(-1.4081690688991E-16,-6.98296267768627E-15,
1.));
#127801=DIRECTION('ref_axis',(-1.,7.97077743482043E-31,-1.4081690688991E-16));
#127802=DIRECTION('',(0.809016994374943,0.58778525229248,4.21840575002205E-15));
#127803=DIRECTION('center_axis',(1.4081690688991E-16,6.98296267768627E-15,
-1.));
#127804=DIRECTION('ref_axis',(1.,-7.97077743482043E-31,1.4081690688991E-16));
#127805=DIRECTION('',(-0.371573073483898,-0.334572327551864,-0.866022406579794));
#127806=DIRECTION('center_axis',(1.4081690688991E-16,6.98296267768627E-15,
-1.));
#127807=DIRECTION('ref_axis',(-1.,-1.95399252334028E-14,-1.40816906890047E-16));
#127808=DIRECTION('',(0.404515505437166,0.293891812003465,0.86602240657978));
#127809=DIRECTION('center_axis',(-1.4081690688991E-16,-6.98296267768627E-15,
1.));
#127810=DIRECTION('ref_axis',(-1.,9.83319205199467E-31,-1.40816906889911E-16));
#127811=DIRECTION('center_axis',(-1.4081690688991E-16,-6.98296267768627E-15,
1.));
#127812=DIRECTION('ref_axis',(-1.,7.98248735348668E-31,-1.4081690688991E-16));
#127813=DIRECTION('',(-0.743144825477389,-0.669130606358864,-4.7771614063965E-15));
#127814=DIRECTION('center_axis',(1.4081690688991E-16,6.98296267768627E-15,
-1.));
#127815=DIRECTION('ref_axis',(-1.,-1.33226762955019E-14,-1.40816906890004E-16));
#127816=DIRECTION('',(0.809016994374943,0.58778525229248,4.21840575002205E-15));
#127817=DIRECTION('center_axis',(-1.4081690688991E-16,-6.98296267768627E-15,
1.));
#127818=DIRECTION('ref_axis',(-1.,7.99150043815584E-31,-1.4081690688991E-16));
#127819=DIRECTION('center_axis',(-1.4081690688991E-16,-6.98296267768627E-15,
1.));
#127820=DIRECTION('ref_axis',(1.,-7.99370576998456E-31,1.4081690688991E-16));
#127821=DIRECTION('',(-0.37157921889255,-0.33456520427975,0.866022521746664));
#127822=DIRECTION('center_axis',(-1.4081690688991E-16,-6.98296267768627E-15,
1.));
#127823=DIRECTION('ref_axis',(-1.,7.99858039355471E-31,-1.4081690688991E-16));
#127824=DIRECTION('center_axis',(-1.4081690688991E-16,-6.98296267768627E-15,
1.));
#127825=DIRECTION('ref_axis',(-1.,7.99858039355471E-31,-1.4081690688991E-16));
#127826=DIRECTION('center_axis',(-1.4081690688991E-16,-6.98296267768627E-15,
1.));
#127827=DIRECTION('ref_axis',(-1.,7.99858039355471E-31,-1.4081690688991E-16));
#127828=DIRECTION('',(0.404509815527952,0.293899304131682,-0.866022521746667));
#127829=DIRECTION('center_axis',(-1.4081690688991E-16,-6.98296267768627E-15,
1.));
#127830=DIRECTION('ref_axis',(-1.,9.83319205199467E-31,-1.40816906889911E-16));
#127831=DIRECTION('',(-0.743144825477389,-0.669130606358864,-4.7771614063965E-15));
#127832=DIRECTION('center_axis',(1.4081690688991E-16,6.98296267768627E-15,
-1.));
#127833=DIRECTION('ref_axis',(-1.,-2.57571741713036E-14,-1.4081690689009E-16));
#127834=DIRECTION('',(0.809016994374943,0.58778525229248,4.21840575002205E-15));
#127835=DIRECTION('center_axis',(-1.4081690688991E-16,-6.98296267768627E-15,
1.));
#127836=DIRECTION('ref_axis',(-1.,8.32577322149061E-31,-1.39145123902276E-16));
#127837=DIRECTION('center_axis',(0.668334867928816,-0.743860540860127,-7.86457198807967E-6));
#127838=DIRECTION('ref_axis',(4.16662527142791E-6,-6.82906373300349E-6,
0.999999999968002));
#127839=DIRECTION('center_axis',(-0.58865077089947,0.808387450334064,-7.86457219664369E-6));
#127840=DIRECTION('ref_axis',(0.685546339984931,0.499205608625129,0.529924500330453));
#127841=DIRECTION('center_axis',(-1.4081690688991E-16,-6.98296267768627E-15,
1.));
#127842=DIRECTION('ref_axis',(-1.,8.07722881720021E-31,-1.42096112075504E-16));
#127843=DIRECTION('center_axis',(0.668368793163115,-0.743830058703073,9.77057967136895E-6));
#127844=DIRECTION('ref_axis',(0.650581635231094,0.584586753101467,0.484769908305291));
#127845=DIRECTION('center_axis',(-0.588613901368558,0.808414296645119,9.77051458754715E-6));
#127846=DIRECTION('ref_axis',(0.707081738814029,0.514826873149225,0.484756336027825));
#127847=DIRECTION('center_axis',(-1.4081690688991E-16,-6.98296267768627E-15,
1.));
#127848=DIRECTION('ref_axis',(-1.,8.24049048117772E-31,-1.37719829560012E-16));
#127849=DIRECTION('center_axis',(-0.671059269896464,0.741403706462376,-1.81624794523114E-5));
#127850=DIRECTION('ref_axis',(0.641501844407457,0.580623821869756,-0.501349539841406));
#127851=DIRECTION('center_axis',(0.585681203637541,-0.810541502562901,-1.81316451643526E-5));
#127852=DIRECTION('ref_axis',(0.702719177034256,0.507782078837254,-0.498340364249189));
#127853=DIRECTION('center_axis',(-1.4081690688991E-16,-6.98296267768627E-15,
1.));
#127854=DIRECTION('ref_axis',(-1.,8.26087817385229E-31,-1.38060560438432E-16));
#127855=DIRECTION('center_axis',(-0.671069287648394,0.74139463906414,-1.84940784596614E-5));
#127856=DIRECTION('ref_axis',(0.642769650612951,0.581811851824381,0.49833938769436));
#127857=DIRECTION('center_axis',(0.585670251954522,-0.810549415910174,-1.85257227583356E-5));
#127858=DIRECTION('ref_axis',(0.70132962721531,0.506740987740637,0.501348506862919));
#127859=DIRECTION('center_axis',(-1.4081690688991E-16,-6.98296267768627E-15,
1.));
#127860=DIRECTION('ref_axis',(-1.,9.83319205199467E-31,-1.40816906889911E-16));
#127861=DIRECTION('center_axis',(-1.4081690688991E-16,-6.98296267768627E-15,
1.));
#127862=DIRECTION('ref_axis',(-1.,8.46073526001725E-31,-1.4081690688991E-16));
#127863=DIRECTION('',(-0.809016994374943,-0.58778525229248,-4.21840575002205E-15));
#127864=DIRECTION('center_axis',(-1.4081690688991E-16,-6.98296267768627E-15,
1.));
#127865=DIRECTION('ref_axis',(-1.,7.97077743482043E-31,-1.4081690688991E-16));
#127866=DIRECTION('center_axis',(-1.4081690688991E-16,-6.98296267768627E-15,
1.));
#127867=DIRECTION('ref_axis',(-1.,7.97077743482043E-31,-1.4081690688991E-16));
#127868=DIRECTION('center_axis',(-1.4081690688991E-16,-6.98296267768627E-15,
1.));
#127869=DIRECTION('ref_axis',(-1.,7.97077743482043E-31,-1.4081690688991E-16));
#127870=DIRECTION('',(0.866025403784435,0.500000000000007,3.61343235749219E-15));
#127871=DIRECTION('center_axis',(1.4081690688991E-16,6.98296267768627E-15,
-1.));
#127872=DIRECTION('ref_axis',(1.,-7.97077743482043E-31,1.4081690688991E-16));
#127873=DIRECTION('',(-0.404509888559936,-0.293899542971723,-0.866022406579784));
#127874=DIRECTION('center_axis',(1.4081690688991E-16,6.98296267768627E-15,
-1.));
#127875=DIRECTION('ref_axis',(-1.,3.99680288865056E-14,-1.40816906889631E-16));
#127876=DIRECTION('',(0.433019586648905,0.249998457755594,0.866022406579781));
#127877=DIRECTION('center_axis',(-1.4081690688991E-16,-6.98296267768627E-15,
1.));
#127878=DIRECTION('ref_axis',(-1.,9.83319205199467E-31,-1.40816906889911E-16));
#127879=DIRECTION('center_axis',(-1.4081690688991E-16,-6.98296267768627E-15,
1.));
#127880=DIRECTION('ref_axis',(-1.,7.98248735348668E-31,-1.4081690688991E-16));
#127881=DIRECTION('',(-0.809016994374943,-0.58778525229248,-4.21840575002205E-15));
#127882=DIRECTION('center_axis',(1.4081690688991E-16,6.98296267768627E-15,
-1.));
#127883=DIRECTION('ref_axis',(-1.,3.37507799486048E-14,-1.40816906889675E-16));
#127884=DIRECTION('',(0.866025403784435,0.500000000000007,3.61343235749219E-15));
#127885=DIRECTION('center_axis',(-1.4081690688991E-16,-6.98296267768627E-15,
1.));
#127886=DIRECTION('ref_axis',(-1.,7.99150043815584E-31,-1.4081690688991E-16));
#127887=DIRECTION('center_axis',(-1.4081690688991E-16,-6.98296267768627E-15,
1.));
#127888=DIRECTION('ref_axis',(1.,-7.99370576998456E-31,1.4081690688991E-16));
#127889=DIRECTION('',(-0.404515255718706,-0.293891816351498,0.866022521746661));
#127890=DIRECTION('center_axis',(-1.4081690688991E-16,-6.98296267768627E-15,
1.));
#127891=DIRECTION('ref_axis',(-1.,7.99858039355471E-31,-1.4081690688991E-16));
#127892=DIRECTION('center_axis',(-1.4081690688991E-16,-6.98296267768627E-15,
1.));
#127893=DIRECTION('ref_axis',(-1.,7.99858039355471E-31,-1.4081690688991E-16));
#127894=DIRECTION('center_axis',(-1.4081690688991E-16,-6.98296267768627E-15,
1.));
#127895=DIRECTION('ref_axis',(-1.,7.99858039355471E-31,-1.4081690688991E-16));
#127896=DIRECTION('',(0.433014711050233,0.250006503598672,-0.866022521746663));
#127897=DIRECTION('center_axis',(-1.4081690688991E-16,-6.98296267768627E-15,
1.));
#127898=DIRECTION('ref_axis',(-1.,9.83319205199467E-31,-1.40816906889911E-16));
#127899=DIRECTION('',(-0.809016994374943,-0.58778525229248,-4.21840575002205E-15));
#127900=DIRECTION('center_axis',(1.4081690688991E-16,6.98296267768627E-15,
-1.));
#127901=DIRECTION('ref_axis',(-1.,2.66453525910038E-14,-1.40816906889724E-16));
#127902=DIRECTION('',(0.866025403784435,0.500000000000007,3.61343235749219E-15));
#127903=DIRECTION('center_axis',(-1.4081690688991E-16,-6.98296267768627E-15,
1.));
#127904=DIRECTION('ref_axis',(-1.,8.32577322149061E-31,-1.39145123902276E-16));
#127905=DIRECTION('center_axis',(0.586919060371703,-0.809645611678681,-7.86457199759038E-6));
#127906=DIRECTION('ref_axis',(3.42996853271349E-6,-7.22718433787076E-6,
0.999999999968002));
#127907=DIRECTION('center_axis',(-0.500926582476661,0.865489779781599,-7.86457219974121E-6));
#127908=DIRECTION('ref_axis',(0.733972040528765,0.424811802650939,0.529924500330473));
#127909=DIRECTION('center_axis',(-1.4081690688991E-16,-6.98296267768627E-15,
1.));
#127910=DIRECTION('ref_axis',(-1.,8.07722881720021E-31,-1.42096112075504E-16));
#127911=DIRECTION('center_axis',(0.586955986005525,-0.809618842664138,9.77059659033885E-6));
#127912=DIRECTION('ref_axis',(0.708123635911214,0.513380027141639,0.484769908302828));
#127913=DIRECTION('center_axis',(-0.50088710871783,0.865512625110015,9.77051576765131E-6));
#127914=DIRECTION('ref_axis',(0.757022332964451,0.438096430107843,0.484756336028549));
#127915=DIRECTION('center_axis',(-1.4081690688991E-16,-6.98296267768627E-15,
1.));
#127916=DIRECTION('ref_axis',(-1.,8.24049048117772E-31,-1.37719829560012E-16));
#127917=DIRECTION('center_axis',(-0.589885346904382,0.807487013627849,-1.81624793333984E-5));
#127918=DIRECTION('ref_axis',(0.69867934601742,0.510387901841475,-0.501349539844735));
#127919=DIRECTION('center_axis',(0.497748123045574,-0.867321627584515,-1.81316451742561E-5));
#127920=DIRECTION('ref_axis',(0.751947288231033,0.431546239794873,-0.49834036425008));
#127921=DIRECTION('center_axis',(-1.4081690688991E-16,-6.98296267768627E-15,
1.));
#127922=DIRECTION('ref_axis',(-1.,8.26087817385229E-31,-1.38060560438432E-16));
#127923=DIRECTION('center_axis',(-0.589896257594011,0.80747904303118,-1.84940468888151E-5));
#127924=DIRECTION('ref_axis',(0.700064389995691,0.511436901811145,0.498339387692543));
#127925=DIRECTION('center_axis',(0.497736404187262,-0.867328352818892,-1.85257232350534E-5));
#127926=DIRECTION('ref_axis',(0.750456526860519,0.430656099412363,0.501348506860622));
#127927=DIRECTION('center_axis',(-1.4081690688991E-16,-6.98296267768627E-15,
1.));
#127928=DIRECTION('ref_axis',(-1.,9.83319205199467E-31,-1.40816906889911E-16));
#127929=DIRECTION('center_axis',(-1.4081690688991E-16,-6.98296267768627E-15,
1.));
#127930=DIRECTION('ref_axis',(-1.,8.46073526001725E-31,-1.4081690688991E-16));
#127931=DIRECTION('',(-0.866025403784435,-0.500000000000007,-3.61343235749219E-15));
#127932=DIRECTION('center_axis',(-1.4081690688991E-16,-6.98296267768627E-15,
1.));
#127933=DIRECTION('ref_axis',(-1.,7.97077743482043E-31,-1.4081690688991E-16));
#127934=DIRECTION('center_axis',(-1.4081690688991E-16,-6.98296267768627E-15,
1.));
#127935=DIRECTION('ref_axis',(-1.,7.97077743482043E-31,-1.4081690688991E-16));
#127936=DIRECTION('center_axis',(-1.4081690688991E-16,-6.98296267768627E-15,
1.));
#127937=DIRECTION('ref_axis',(-1.,7.97077743482043E-31,-1.4081690688991E-16));
#127938=DIRECTION('',(0.913545457642598,0.406736643075807,2.96886944389432E-15));
#127939=DIRECTION('center_axis',(1.4081690688991E-16,6.98296267768627E-15,
-1.));
#127940=DIRECTION('ref_axis',(1.,-7.97077743482043E-31,1.4081690688991E-16));
#127941=DIRECTION('',(-0.433014808647732,-0.250006733496379,-0.866022406579783));
#127942=DIRECTION('center_axis',(1.4081690688991E-16,6.98296267768627E-15,
-1.));
#127943=DIRECTION('ref_axis',(-1.,7.10542735760101E-15,-1.40816906889861E-16));
#127944=DIRECTION('',(0.456779414654113,0.203366068089037,0.86602240657979));
#127945=DIRECTION('center_axis',(-1.4081690688991E-16,-6.98296267768627E-15,
1.));
#127946=DIRECTION('ref_axis',(-1.,9.83319205199467E-31,-1.40816906889911E-16));
#127947=DIRECTION('center_axis',(-1.4081690688991E-16,-6.98296267768627E-15,
1.));
#127948=DIRECTION('ref_axis',(-1.,7.98248735348668E-31,-1.4081690688991E-16));
#127949=DIRECTION('',(-0.866025403784435,-0.500000000000007,-3.61343235749219E-15));
#127950=DIRECTION('center_axis',(1.4081690688991E-16,6.98296267768627E-15,
-1.));
#127951=DIRECTION('ref_axis',(-1.,7.10542735760101E-15,-1.40816906889861E-16));
#127952=DIRECTION('',(0.913545457642598,0.406736643075807,2.96886944389432E-15));
#127953=DIRECTION('center_axis',(-1.4081690688991E-16,-6.98296267768627E-15,
1.));
#127954=DIRECTION('ref_axis',(-1.,7.99150043815584E-31,-1.4081690688991E-16));
#127955=DIRECTION('center_axis',(-1.4081690688991E-16,-6.98296267768627E-15,
1.));
#127956=DIRECTION('ref_axis',(1.,-7.99370576998456E-31,1.4081690688991E-16));
#127957=DIRECTION('',(-0.433019338752864,-0.249998488182536,0.86602252174668));
#127958=DIRECTION('center_axis',(-1.4081690688991E-16,-6.98296267768627E-15,
1.));
#127959=DIRECTION('ref_axis',(-1.,7.99858039355471E-31,-1.4081690688991E-16));
#127960=DIRECTION('center_axis',(-1.4081690688991E-16,-6.98296267768627E-15,
1.));
#127961=DIRECTION('ref_axis',(-1.,7.99858039355471E-31,-1.4081690688991E-16));
#127962=DIRECTION('center_axis',(-1.4081690688991E-16,-6.98296267768627E-15,
1.));
#127963=DIRECTION('ref_axis',(-1.,7.99858039355471E-31,-1.4081690688991E-16));
#127964=DIRECTION('',(0.456775406784116,0.203374579494969,-0.866022521746663));
#127965=DIRECTION('center_axis',(-1.4081690688991E-16,-6.98296267768627E-15,
1.));
#127966=DIRECTION('ref_axis',(-1.,9.83319205199467E-31,-1.40816906889911E-16));
#127967=DIRECTION('',(-0.866025403784435,-0.500000000000007,-3.61343235749219E-15));
#127968=DIRECTION('center_axis',(1.4081690688991E-16,6.98296267768627E-15,
-1.));
#127969=DIRECTION('ref_axis',(-1.,8.01265634860448E-31,-1.4081690688991E-16));
#127970=DIRECTION('',(0.913545457642598,0.406736643075807,2.96886944389432E-15));
#127971=DIRECTION('center_axis',(-1.4081690688991E-16,-6.98296267768627E-15,
1.));
#127972=DIRECTION('ref_axis',(-1.,8.32577322149061E-31,-1.39145123902276E-16));
#127973=DIRECTION('center_axis',(0.499072844768409,-0.866560035746466,-7.86457209026023E-6));
#127974=DIRECTION('ref_axis',(2.65573234861323E-6,-7.54612250867244E-6,
0.999999999968002));
#127975=DIRECTION('center_axis',(-0.407714137590658,0.913109622086447,-7.86457230391254E-6));
#127976=DIRECTION('ref_axis',(0.774356189803006,0.345763669669417,0.52992450033048));
#127977=DIRECTION('center_axis',(-1.4081690688991E-16,-6.98296267768627E-15,
1.));
#127978=DIRECTION('ref_axis',(-1.,8.07722881720021E-31,-1.42096112075504E-16));
#127979=DIRECTION('center_axis',(0.499112366251912,-0.866537273150413,9.77057961947491E-6));
#127980=DIRECTION('ref_axis',(0.757907285851233,0.436548602172012,0.484769908302154));
#127981=DIRECTION('center_axis',(-0.407672492090694,0.913128216132379,9.77052487249037E-6));
#127982=DIRECTION('ref_axis',(0.798668832018019,0.356566110900804,0.484756336028782));
#127983=DIRECTION('center_axis',(-1.4081690688991E-16,-6.98296267768627E-15,
1.));
#127984=DIRECTION('ref_axis',(-1.,8.24049048117772E-31,-1.37719829560012E-16));
#127985=DIRECTION('center_axis',(-0.502248516610529,0.864723324094272,-1.81624798592741E-5));
#127986=DIRECTION('ref_axis',(0.74820197050812,0.434560065157779,-0.501349539840054));
#127987=DIRECTION('center_axis',(0.404361609857085,-0.914599195355556,-1.81316452513466E-5));
#127988=DIRECTION('ref_axis',(0.792936907582491,0.350582289842495,-0.498340364251491));
#127989=DIRECTION('center_axis',(-1.4081690688991E-16,-6.98296267768627E-15,
1.));
#127990=DIRECTION('ref_axis',(-1.,8.26087817385229E-31,-1.38060560438432E-16));
#127991=DIRECTION('center_axis',(-0.502260200673814,0.864716537645181,-1.84940675711417E-5));
#127992=DIRECTION('ref_axis',(0.749689077421511,0.435458542074875,0.498339387695682));
#127993=DIRECTION('center_axis',(0.404349252211792,-0.914604658796664,-1.85257124702087E-5));
#127994=DIRECTION('ref_axis',(0.791361267752528,0.349852852737285,0.501348506861938));
#127995=DIRECTION('center_axis',(-1.4081690688991E-16,-6.98296267768627E-15,
1.));
#127996=DIRECTION('ref_axis',(-1.,9.83319205199467E-31,-1.40816906889911E-16));
#127997=DIRECTION('center_axis',(-1.4081690688991E-16,-6.98296267768627E-15,
1.));
#127998=DIRECTION('ref_axis',(-1.,8.46073526001725E-31,-1.4081690688991E-16));
#127999=DIRECTION('',(-0.913545457642598,-0.406736643075807,-2.96886944389432E-15));
#128000=DIRECTION('center_axis',(-1.4081690688991E-16,-6.98296267768627E-15,
1.));
#128001=DIRECTION('ref_axis',(-1.,7.97077743482043E-31,-1.4081690688991E-16));
#128002=DIRECTION('center_axis',(-1.4081690688991E-16,-6.98296267768627E-15,
1.));
#128003=DIRECTION('ref_axis',(-1.,7.97077743482043E-31,-1.4081690688991E-16));
#128004=DIRECTION('center_axis',(-1.4081690688991E-16,-6.98296267768627E-15,
1.));
#128005=DIRECTION('ref_axis',(-1.,7.97077743482043E-31,-1.4081690688991E-16));
#128006=DIRECTION('',(0.951056516295151,0.309016994374955,2.29177897539327E-15));
#128007=DIRECTION('center_axis',(1.4081690688991E-16,6.98296267768627E-15,
-1.));
#128008=DIRECTION('ref_axis',(1.,-7.97077743482043E-31,1.4081690688991E-16));
#128009=DIRECTION('',(-0.456775527877824,-0.20337479793158,-0.866022406579775));
#128010=DIRECTION('center_axis',(1.4081690688991E-16,6.98296267768627E-15,
-1.));
#128011=DIRECTION('ref_axis',(-1.,-2.1316282072803E-14,-1.40816906890059E-16));
#128012=DIRECTION('',(0.475534671805166,0.154505557223409,0.866022406579782));
#128013=DIRECTION('center_axis',(-1.4081690688991E-16,-6.98296267768627E-15,
1.));
#128014=DIRECTION('ref_axis',(-1.,9.83319205199467E-31,-1.40816906889911E-16));
#128015=DIRECTION('center_axis',(-1.4081690688991E-16,-6.98296267768627E-15,
1.));
#128016=DIRECTION('ref_axis',(-1.,7.98248735348668E-31,-1.4081690688991E-16));
#128017=DIRECTION('',(-0.913545457642598,-0.406736643075807,-2.96886944389432E-15));
#128018=DIRECTION('center_axis',(1.4081690688991E-16,6.98296267768627E-15,
-1.));
#128019=DIRECTION('ref_axis',(-1.,-1.77635683940025E-14,-1.40816906890035E-16));
#128020=DIRECTION('',(0.951056516295151,0.309016994374955,2.29177897539327E-15));
#128021=DIRECTION('center_axis',(-1.4081690688991E-16,-6.98296267768627E-15,
1.));
#128022=DIRECTION('ref_axis',(-1.,7.99150043815584E-31,-1.4081690688991E-16));
#128023=DIRECTION('center_axis',(-1.4081690688991E-16,-6.98296267768627E-15,
1.));
#128024=DIRECTION('ref_axis',(1.,-7.99370576998456E-31,1.4081690688991E-16));
#128025=DIRECTION('',(-0.456779171296625,-0.203366124261497,0.866022521746649));
#128026=DIRECTION('center_axis',(-1.4081690688991E-16,-6.98296267768627E-15,
1.));
#128027=DIRECTION('ref_axis',(-1.,7.99858039355471E-31,-1.4081690688991E-16));
#128028=DIRECTION('center_axis',(-1.4081690688991E-16,-6.98296267768627E-15,
1.));
#128029=DIRECTION('ref_axis',(-1.,7.99858039355471E-31,-1.4081690688991E-16));
#128030=DIRECTION('center_axis',(-1.4081690688991E-16,-6.98296267768627E-15,
1.));
#128031=DIRECTION('ref_axis',(-1.,7.99858039355471E-31,-1.4081690688991E-16));
#128032=DIRECTION('',(0.47553157557488,0.154514440939479,-0.866022521746653));
#128033=DIRECTION('center_axis',(-1.4081690688991E-16,-6.98296267768627E-15,
1.));
#128034=DIRECTION('ref_axis',(-1.,9.83319205199467E-31,-1.40816906889911E-16));
#128035=DIRECTION('',(-0.913545457642598,-0.406736643075807,-2.96886944389432E-15));
#128036=DIRECTION('center_axis',(1.4081690688991E-16,6.98296267768627E-15,
-1.));
#128037=DIRECTION('ref_axis',(-1.,-2.04281036531029E-14,-1.40816906890053E-16));
#128038=DIRECTION('',(0.951056516295151,0.309016994374955,2.29177897539327E-15));
#128039=DIRECTION('center_axis',(-1.4081690688991E-16,-6.98296267768627E-15,
1.));
#128040=DIRECTION('ref_axis',(-1.,8.32577322149061E-31,-1.39145123902276E-16));
#128041=DIRECTION('center_axis',(0.405758682640235,-0.913980246723204,-7.86457197116076E-6));
#128042=DIRECTION('ref_axis',(1.85239938593913E-6,-7.78238354702661E-6,
0.999999999968002));
#128043=DIRECTION('center_axis',(-0.310034691293484,0.950725244291274,-7.86457229993127E-6));
#128044=DIRECTION('ref_axis',(0.806256330617376,0.262927277567205,0.529924500330475));
#128045=DIRECTION('center_axis',(-1.4081690688991E-16,-6.98296267768627E-15,
1.));
#128046=DIRECTION('ref_axis',(-1.,8.07722881720021E-31,-1.42096112075504E-16));
#128047=DIRECTION('center_axis',(0.405800366954514,-0.913961739945452,9.77059051480661E-6));
#128048=DIRECTION('ref_axis',(0.799387144964324,0.354934259362841,0.484769908303247));
#128049=DIRECTION('center_axis',(-0.309991330319405,0.950739383338748,9.77051447639857E-6));
#128050=DIRECTION('ref_axis',(0.83156494821626,0.27112917876665,0.484756336028124));
#128051=DIRECTION('center_axis',(-1.4081690688991E-16,-6.98296267768627E-15,
1.));
#128052=DIRECTION('ref_axis',(-1.,8.24049048117772E-31,-1.37719829560012E-16));
#128053=DIRECTION('center_axis',(-0.40910894646611,0.912485544867158,-1.81624798772874E-5));
#128054=DIRECTION('ref_axis',(0.789527137635887,0.353971097460744,-0.501349539841137));
#128055=DIRECTION('center_axis',(0.306544826252958,-0.951856222950077,-1.81316451055346E-5));
#128056=DIRECTION('ref_axis',(0.825238944242033,0.26577728695875,-0.498340364252326));
#128057=DIRECTION('center_axis',(-1.4081690688991E-16,-6.98296267768627E-15,
1.));
#128058=DIRECTION('ref_axis',(-1.,8.26087817385229E-31,-1.38060560438432E-16));
#128059=DIRECTION('center_axis',(-0.409121275907456,0.912480016908768,-1.8494053348855E-5));
#128060=DIRECTION('ref_axis',(0.791100014434309,0.354709207427339,0.498339387695077));
#128061=DIRECTION('center_axis',(0.306531965211348,-0.951860364738688,-1.85256986116291E-5));
#128062=DIRECTION('ref_axis',(0.823595688991342,0.265216544996153,0.501348506864417));
#128063=DIRECTION('center_axis',(-1.4081690688991E-16,-6.98296267768627E-15,
1.));
#128064=DIRECTION('ref_axis',(-1.,9.83319205199467E-31,-1.40816906889911E-16));
#128065=DIRECTION('center_axis',(-1.4081690688991E-16,-6.98296267768627E-15,
1.));
#128066=DIRECTION('ref_axis',(-1.,8.46073526001725E-31,-1.4081690688991E-16));
#128067=DIRECTION('',(-0.951056516295151,-0.309016994374955,-2.29177897539327E-15));
#128068=DIRECTION('center_axis',(-1.4081690688991E-16,-6.98296267768627E-15,
1.));
#128069=DIRECTION('ref_axis',(-1.,7.97077743482043E-31,-1.4081690688991E-16));
#128070=DIRECTION('center_axis',(-1.4081690688991E-16,-6.98296267768627E-15,
1.));
#128071=DIRECTION('ref_axis',(-1.,7.97077743482043E-31,-1.4081690688991E-16));
#128072=DIRECTION('center_axis',(-1.4081690688991E-16,-6.98296267768627E-15,
1.));
#128073=DIRECTION('ref_axis',(-1.,7.97077743482043E-31,-1.4081690688991E-16));
#128074=DIRECTION('',(0.978147600733804,0.207911690817766,1.58957929685223E-15));
#128075=DIRECTION('center_axis',(1.4081690688991E-16,6.98296267768627E-15,
-1.));
#128076=DIRECTION('ref_axis',(1.,-7.97077743482043E-31,1.4081690688991E-16));
#128077=DIRECTION('',(-0.475531718838049,-0.154514645521701,-0.86602240657978));
#128078=DIRECTION('center_axis',(1.4081690688991E-16,6.98296267768627E-15,
-1.));
#128079=DIRECTION('ref_axis',(-1.,4.08562073062058E-14,-1.40816906889625E-16));
#128080=DIRECTION('',(0.489079871579876,0.10395225114048,0.866022406579783));
#128081=DIRECTION('center_axis',(-1.4081690688991E-16,-6.98296267768627E-15,
1.));
#128082=DIRECTION('ref_axis',(-1.,9.83319205199467E-31,-1.40816906889911E-16));
#128083=DIRECTION('center_axis',(-1.4081690688991E-16,-6.98296267768627E-15,
1.));
#128084=DIRECTION('ref_axis',(-1.,7.98248735348668E-31,-1.4081690688991E-16));
#128085=DIRECTION('',(-0.951056516295151,-0.309016994374955,-2.29177897539327E-15));
#128086=DIRECTION('center_axis',(1.4081690688991E-16,6.98296267768627E-15,
-1.));
#128087=DIRECTION('ref_axis',(-1.,3.28626015289046E-14,-1.40816906889681E-16));
#128088=DIRECTION('',(0.978147600733804,0.207911690817766,1.58957929685223E-15));
#128089=DIRECTION('center_axis',(-1.4081690688991E-16,-6.98296267768627E-15,
1.));
#128090=DIRECTION('ref_axis',(-1.,7.99150043815584E-31,-1.4081690688991E-16));
#128091=DIRECTION('center_axis',(-1.4081690688991E-16,-6.98296267768627E-15,
1.));
#128092=DIRECTION('ref_axis',(1.,-7.99370576998456E-31,1.4081690688991E-16));
#128093=DIRECTION('',(-0.475534435652379,-0.154505638525953,0.866022521746669));
#128094=DIRECTION('center_axis',(-1.4081690688991E-16,-6.98296267768627E-15,
1.));
#128095=DIRECTION('ref_axis',(-1.,7.99858039355471E-31,-1.4081690688991E-16));
#128096=DIRECTION('center_axis',(-1.4081690688991E-16,-6.98296267768627E-15,
1.));
#128097=DIRECTION('ref_axis',(-1.,7.99858039355471E-31,-1.4081690688991E-16));
#128098=DIRECTION('center_axis',(-1.4081690688991E-16,-6.98296267768627E-15,
1.));
#128099=DIRECTION('ref_axis',(-1.,7.99858039355471E-31,-1.4081690688991E-16));
#128100=DIRECTION('',(0.489077720912261,0.103961409834809,-0.86602252174665));
#128101=DIRECTION('center_axis',(-1.4081690688991E-16,-6.98296267768627E-15,
1.));
#128102=DIRECTION('ref_axis',(-1.,9.83319205199467E-31,-1.40816906889911E-16));
#128103=DIRECTION('',(-0.951056516295151,-0.309016994374955,-2.29177897539327E-15));
#128104=DIRECTION('center_axis',(1.4081690688991E-16,6.98296267768627E-15,
-1.));
#128105=DIRECTION('ref_axis',(-1.,2.48689957516035E-14,-1.40816906889737E-16));
#128106=DIRECTION('',(0.978147600733804,0.207911690817766,1.58957929685223E-15));
#128107=DIRECTION('center_axis',(-1.4081690688991E-16,-6.98296267768627E-15,
1.));
#128108=DIRECTION('ref_axis',(-1.,8.32577322149061E-31,-1.39145123902276E-16));
#128109=DIRECTION('center_axis',(0.307998943474541,-0.951386698854212,-7.86457199095568E-6));
#128110=DIRECTION('ref_axis',(1.02877118498534E-6,-7.93337931236483E-6,
0.999999999968002));
#128111=DIRECTION('center_axis',(-0.208958440039579,0.977924521767592,-7.86457230358117E-6));
#128112=DIRECTION('ref_axis',(0.829322958353489,0.177210199190901,0.529924500330508));
#128113=DIRECTION('center_axis',(-1.4081690688991E-16,-6.98296267768627E-15,
1.));
#128114=DIRECTION('ref_axis',(-1.,8.07722881720021E-31,-1.42096112075504E-16));
#128115=DIRECTION('center_axis',(0.308042333923395,-0.951372650655653,9.77058934107909E-6));
#128116=DIRECTION('ref_axis',(0.832108751234113,0.269431182533241,0.484769908305316));
#128117=DIRECTION('center_axis',(-0.20891383867053,0.977934050903475,9.77051809992799E-6));
#128118=DIRECTION('ref_axis',(0.85535026482736,0.182721698612803,0.484756336024417));
#128119=DIRECTION('center_axis',(-1.4081690688991E-16,-6.98296267768627E-15,
1.));
#128120=DIRECTION('ref_axis',(-1.,8.24049048117772E-31,-1.37719829560012E-16));
#128121=DIRECTION('center_axis',(-0.311487093092621,0.950250383060608,-1.81624796851363E-5));
#128122=DIRECTION('ref_axis',(0.822202080224231,0.269503948346828,-0.50134953984263));
#128123=DIRECTION('center_axis',(0.205369473383632,-0.978684514577284,-1.81316452252925E-5));
#128124=DIRECTION('ref_axis',(0.84849949033903,0.17806037250233,-0.498340364247908));
#128125=DIRECTION('center_axis',(-1.4081690688991E-16,-6.98296267768627E-15,
1.));
#128126=DIRECTION('ref_axis',(-1.,8.26087817385229E-31,-1.38060560438432E-16));
#128127=DIRECTION('center_axis',(-0.311499932813636,0.950246174164921,-1.84940668588953E-5));
#128128=DIRECTION('ref_axis',(0.823843494140552,0.270073604475409,0.498339387694719));
#128129=DIRECTION('center_axis',(0.20535624986749,-0.97868728933054,-1.8525709393338E-5));
#128130=DIRECTION('ref_axis',(0.846806623518089,0.177674469289194,0.501348506857951));
#128131=DIRECTION('center_axis',(-1.4081690688991E-16,-6.98296267768627E-15,
1.));
#128132=DIRECTION('ref_axis',(-1.,9.83319205199467E-31,-1.40816906889911E-16));
#128133=DIRECTION('center_axis',(-1.4081690688991E-16,-6.98296267768627E-15,
1.));
#128134=DIRECTION('ref_axis',(-1.,8.46073526001725E-31,-1.4081690688991E-16));
#128135=DIRECTION('',(-0.978147600733804,-0.207911690817766,-1.58957929685223E-15));
#128136=DIRECTION('center_axis',(-1.4081690688991E-16,-6.98296267768627E-15,
1.));
#128137=DIRECTION('ref_axis',(-1.,7.97077743482043E-31,-1.4081690688991E-16));
#128138=DIRECTION('center_axis',(-1.4081690688991E-16,-6.98296267768627E-15,
1.));
#128139=DIRECTION('ref_axis',(-1.,7.97077743482043E-31,-1.4081690688991E-16));
#128140=DIRECTION('center_axis',(-1.4081690688991E-16,-6.98296267768627E-15,
1.));
#128141=DIRECTION('ref_axis',(-1.,7.97077743482043E-31,-1.4081690688991E-16));
#128142=DIRECTION('',(0.994521895368273,0.104528463267661,8.69963854894025E-16));
#128143=DIRECTION('center_axis',(1.4081690688991E-16,6.98296267768627E-15,
-1.));
#128144=DIRECTION('ref_axis',(1.,-7.97077743482043E-31,1.4081690688991E-16));
#128145=DIRECTION('',(-0.48907788477529,-0.103961598321232,-0.866022406579774));
#128146=DIRECTION('center_axis',(1.4081690688991E-16,6.98296267768627E-15,
-1.));
#128147=DIRECTION('ref_axis',(-1.,-1.68753899743024E-14,-1.40816906890028E-16));
#128148=DIRECTION('',(0.497266609935039,0.0522600224406394,0.866022406579771));
#128149=DIRECTION('center_axis',(-1.4081690688991E-16,-6.98296267768627E-15,
1.));
#128150=DIRECTION('ref_axis',(-1.,9.83319205199467E-31,-1.40816906889911E-16));
#128151=DIRECTION('center_axis',(-1.4081690688991E-16,-6.98296267768627E-15,
1.));
#128152=DIRECTION('ref_axis',(-1.,7.98248735348668E-31,-1.4081690688991E-16));
#128153=DIRECTION('',(-0.978147600733804,-0.207911690817766,-1.58957929685223E-15));
#128154=DIRECTION('center_axis',(1.4081690688991E-16,6.98296267768627E-15,
-1.));
#128155=DIRECTION('ref_axis',(-1.,-2.22044604925031E-14,-1.40816906890066E-16));
#128156=DIRECTION('',(0.994521895368273,0.104528463267661,8.69963854894025E-16));
#128157=DIRECTION('center_axis',(-1.4081690688991E-16,-6.98296267768627E-15,
1.));
#128158=DIRECTION('ref_axis',(-1.,7.99150043815584E-31,-1.4081690688991E-16));
#128159=DIRECTION('center_axis',(-1.4081690688991E-16,-6.98296267768627E-15,
1.));
#128160=DIRECTION('ref_axis',(1.,-7.99370576998456E-31,1.4081690688991E-16));
#128161=DIRECTION('',(-0.489079645219224,-0.103952356682314,0.866022521746652));
#128162=DIRECTION('center_axis',(-1.4081690688991E-16,-6.98296267768627E-15,
1.));
#128163=DIRECTION('ref_axis',(-1.,7.99858039355471E-31,-1.4081690688991E-16));
#128164=DIRECTION('center_axis',(-1.4081690688991E-16,-6.98296267768627E-15,
1.));
#128165=DIRECTION('ref_axis',(-1.,7.99858039355471E-31,-1.4081690688991E-16));
#128166=DIRECTION('center_axis',(-1.4081690688991E-16,-6.98296267768627E-15,
1.));
#128167=DIRECTION('ref_axis',(-1.,7.99858039355471E-31,-1.4081690688991E-16));
#128168=DIRECTION('',(0.497265428393237,0.0522693557686703,-0.866022521746645));
#128169=DIRECTION('center_axis',(-1.4081690688991E-16,-6.98296267768627E-15,
1.));
#128170=DIRECTION('ref_axis',(-1.,9.83319205199467E-31,-1.40816906889911E-16));
#128171=DIRECTION('',(-0.978147600733804,-0.207911690817766,-1.58957929685223E-15));
#128172=DIRECTION('center_axis',(1.4081690688991E-16,6.98296267768627E-15,
-1.));
#128173=DIRECTION('ref_axis',(-1.,-2.39808173319034E-14,-1.40816906890078E-16));
#128174=DIRECTION('',(0.994521895368273,0.104528463267661,8.69963854894025E-16));
#128175=DIRECTION('center_axis',(-1.4081690688991E-16,-6.98296267768627E-15,
1.));
#128176=DIRECTION('ref_axis',(-1.,8.32577322149061E-31,-1.39145123902276E-16));
#128177=DIRECTION('center_axis',(0.206864703431171,-0.978369559222118,-7.86457205940785E-6));
#128178=DIRECTION('ref_axis',(1.93871496019899E-7,-7.99745537400948E-6,
0.999999999968001));
#128179=DIRECTION('center_axis',(-0.105592796389226,0.994409453539563,-7.86457227510478E-6));
#128180=DIRECTION('ref_axis',(0.843303350210945,0.0895515687886275,0.529924500330464));
#128181=DIRECTION('center_axis',(-1.4081690688991E-16,-6.98296267768627E-15,
1.));
#128182=DIRECTION('ref_axis',(-1.,8.07722881720021E-31,-1.42096112075504E-16));
#128183=DIRECTION('center_axis',(0.206909324622084,-0.978360123517393,9.77058419069398E-6));
#128184=DIRECTION('ref_axis',(0.855713599897009,0.180976161286358,0.484769908304296));
#128185=DIRECTION('center_axis',(-0.105547443284138,0.99441426836139,9.77051615051766E-6));
#128186=DIRECTION('ref_axis',(0.869764184940149,0.0923122812911752,0.484756336026892));
#128187=DIRECTION('center_axis',(-1.4081690688991E-16,-6.98296267768627E-15,
1.));
#128188=DIRECTION('ref_axis',(-1.,8.24049048117772E-31,-1.37719829560012E-16));
#128189=DIRECTION('center_axis',(-0.2104525219444,0.977604079204545,-1.81624797895158E-5));
#128190=DIRECTION('ref_axis',(0.845868804765923,0.182084057577827,-0.501349539842078));
#128191=DIRECTION('center_axis',(0.101944049587683,-0.994790133859855,-1.81316451673808E-5));
#128192=DIRECTION('ref_axis',(0.862463698457448,0.0883925913424541,-0.498340364248037));
#128193=DIRECTION('center_axis',(-1.4081690688991E-16,-6.98296267768627E-15,
1.));
#128194=DIRECTION('ref_axis',(-1.,8.26087817385229E-31,-1.38060560438432E-16));
#128195=DIRECTION('center_axis',(-0.210465731280713,0.977601235481239,-1.84940611137989E-5));
#128196=DIRECTION('ref_axis',(0.847560772121457,0.182479018595617,0.49833938770005));
#128197=DIRECTION('center_axis',(0.101930608471618,-0.994791511178802,-1.8525711081838E-5));
#128198=DIRECTION('ref_axis',(0.860739767467695,0.0881857549147744,0.50134850685902));
#128199=DIRECTION('center_axis',(-1.4081690688991E-16,-6.98296267768627E-15,
1.));
#128200=DIRECTION('ref_axis',(-1.,9.83319205199467E-31,-1.40816906889911E-16));
#128201=DIRECTION('center_axis',(-1.4081690688991E-16,-6.98296267768627E-15,
1.));
#128202=DIRECTION('ref_axis',(-1.,8.46073526001725E-31,-1.4081690688991E-16));
#128203=DIRECTION('',(-0.994521895368273,-0.104528463267661,-8.69963854894025E-16));
#128204=DIRECTION('center_axis',(-1.4081690688991E-16,-6.98296267768627E-15,
1.));
#128205=DIRECTION('ref_axis',(-1.,7.97077743482043E-31,-1.4081690688991E-16));
#128206=DIRECTION('center_axis',(-1.4081690688991E-16,-6.98296267768627E-15,
1.));
#128207=DIRECTION('ref_axis',(-1.,7.97077743482043E-31,-1.4081690688991E-16));
#128208=DIRECTION('center_axis',(-1.4081690688991E-16,-6.98296267768627E-15,
1.));
#128209=DIRECTION('ref_axis',(-1.,7.97077743482043E-31,-1.4081690688991E-16));
#128210=DIRECTION('',(1.,-9.83319205199467E-31,1.40816906889911E-16));
#128211=DIRECTION('center_axis',(1.4081690688991E-16,6.98296267768627E-15,
-1.));
#128212=DIRECTION('ref_axis',(1.,-7.97077743482043E-31,1.4081690688991E-16));
#128213=DIRECTION('',(-0.497265611060784,-0.0522695260941848,-0.86602240657978));
#128214=DIRECTION('center_axis',(1.4081690688991E-16,6.98296267768627E-15,
-1.));
#128215=DIRECTION('ref_axis',(-1.,-5.32907051820075E-15,-1.40816906889948E-16));
#128216=DIRECTION('',(0.500005191251989,-4.77800117170159E-6,0.866022406579779));
#128217=DIRECTION('center_axis',(-1.4081690688991E-16,-6.98296267768627E-15,
1.));
#128218=DIRECTION('ref_axis',(-1.,9.83319205199467E-31,-1.40816906889911E-16));
#128219=DIRECTION('center_axis',(-1.4081690688991E-16,-6.98296267768627E-15,
1.));
#128220=DIRECTION('ref_axis',(-1.,7.98248735348668E-31,-1.4081690688991E-16));
#128221=DIRECTION('',(-0.994521895368273,-0.104528463267661,-8.69963854894025E-16));
#128222=DIRECTION('center_axis',(1.4081690688991E-16,6.98296267768627E-15,
-1.));
#128223=DIRECTION('ref_axis',(-1.,-1.24344978758018E-14,-1.40816906889997E-16));
#128224=DIRECTION('',(1.,-9.83319205199467E-31,1.40816906889911E-16));
#128225=DIRECTION('center_axis',(-1.4081690688991E-16,-6.98296267768627E-15,
1.));
#128226=DIRECTION('ref_axis',(-1.,7.99150043815584E-31,-1.4081690688991E-16));
#128227=DIRECTION('center_axis',(-1.4081690688991E-16,-6.98296267768627E-15,
1.));
#128228=DIRECTION('ref_axis',(1.,-7.99370576998456E-31,1.4081690688991E-16));
#128229=DIRECTION('',(-0.497266395846526,-0.0522601510654453,0.866022521746648));
#128230=DIRECTION('center_axis',(-1.4081690688991E-16,-6.98296267768627E-15,
1.));
#128231=DIRECTION('ref_axis',(-1.,7.99858039355471E-31,-1.4081690688991E-16));
#128232=DIRECTION('center_axis',(-1.4081690688991E-16,-6.98296267768627E-15,
1.));
#128233=DIRECTION('ref_axis',(-1.,7.99858039355471E-31,-1.4081690688991E-16));
#128234=DIRECTION('center_axis',(-1.4081690688991E-16,-6.98296267768627E-15,
1.));
#128235=DIRECTION('ref_axis',(-1.,7.99858039355471E-31,-1.4081690688991E-16));
#128236=DIRECTION('',(0.500004991781227,4.62770265895213E-6,-0.866022521746658));
#128237=DIRECTION('center_axis',(-1.4081690688991E-16,-6.98296267768627E-15,
1.));
#128238=DIRECTION('ref_axis',(-1.,9.83319205199467E-31,-1.40816906889911E-16));
#128239=DIRECTION('',(-0.994521895368273,-0.104528463267661,-8.69963854894025E-16));
#128240=DIRECTION('center_axis',(1.4081690688991E-16,6.98296267768627E-15,
-1.));
#128241=DIRECTION('ref_axis',(-1.,-1.86517468137026E-14,-1.40816906890041E-16));
#128242=DIRECTION('',(1.,-9.83319205199467E-31,1.40816906889911E-16));
#128243=DIRECTION('center_axis',(-1.4081690688991E-16,-6.98296267768627E-15,
1.));
#128244=DIRECTION('ref_axis',(-1.,8.32577322149061E-31,-1.39145123902276E-16));
#128245=DIRECTION('center_axis',(0.10346401040783,-0.994633197962182,-7.86457203728972E-6));
#128246=DIRECTION('ref_axis',(-6.43152314414477E-7,-7.97390954906981E-6,
0.999999999968001));
#128247=DIRECTION('center_axis',(-0.00107025596492904,0.999999427244995,
-7.86457228206508E-6));
#128248=DIRECTION('ref_axis',(0.848044334090877,0.000911792658855751,0.529924500330479));
#128249=DIRECTION('center_axis',(-1.4081690688991E-16,-6.98296267768627E-15,
1.));
#128250=DIRECTION('ref_axis',(-1.,8.07722881720021E-31,-1.42096112075504E-16));
#128251=DIRECTION('center_axis',(0.10350937345709,-0.994628478131939,9.77058738226894E-6));
#128252=DIRECTION('ref_axis',(0.869943071288686,0.0905383273444065,0.484769908305461));
#128253=DIRECTION('center_axis',(-0.00102464802306466,0.999999475000345,
9.7705163072413E-6));
#128254=DIRECTION('ref_axis',(0.874648786633691,0.000891471298436039,0.484756336027841));
#128255=DIRECTION('center_axis',(-1.4081690688991E-16,-6.98296267768627E-15,
1.));
#128256=DIRECTION('ref_axis',(-1.,8.24049048117772E-31,-1.37719829560012E-16));
#128257=DIRECTION('center_axis',(-0.107112188925754,0.994246940479908,-1.81624798062462E-5));
#128258=DIRECTION('ref_axis',(0.86026801367229,0.0926692157703631,-0.501349539843051));
#128259=DIRECTION('center_axis',(-0.00259829454878754,-0.999996624262643,
-1.81316452336422E-5));
#128260=DIRECTION('ref_axis',(0.866978573810612,-0.00224363754548855,-0.49834036425307));
#128261=DIRECTION('center_axis',(-1.4081690688991E-16,-6.98296267768627E-15,
1.));
#128262=DIRECTION('ref_axis',(-1.,8.26087817385229E-31,-1.38060560438432E-16));
#128263=DIRECTION('center_axis',(-0.107125623149976,0.99424549308644,-1.84940610889373E-5));
#128264=DIRECTION('ref_axis',(0.861991996925822,0.0928851544032302,0.498339387694092));
#128265=DIRECTION('center_axis',(-0.00261180600211858,-0.999996589057285,
-1.85257108738633E-5));
#128266=DIRECTION('ref_axis',(0.865242466403372,-0.00226914104443546,0.501348506860378));
#128267=DIRECTION('center_axis',(-1.4081690688991E-16,-6.98296267768627E-15,
1.));
#128268=DIRECTION('ref_axis',(-1.,9.83319205199467E-31,-1.40816906889911E-16));
#128269=DIRECTION('center_axis',(-1.4081690688991E-16,-6.98296267768627E-15,
1.));
#128270=DIRECTION('ref_axis',(-1.,8.46073526001725E-31,-1.4081690688991E-16));
#128271=DIRECTION('',(-1.,9.83319205199467E-31,-1.40816906889911E-16));
#128272=DIRECTION('center_axis',(-1.4081690688991E-16,-6.98296267768627E-15,
1.));
#128273=DIRECTION('ref_axis',(-1.,7.97077743482043E-31,-1.4081690688991E-16));
#128274=DIRECTION('center_axis',(-1.4081690688991E-16,-6.98296267768627E-15,
1.));
#128275=DIRECTION('ref_axis',(-1.,7.97077743482043E-31,-1.4081690688991E-16));
#128276=DIRECTION('center_axis',(-1.4081690688991E-16,-6.98296267768627E-15,
1.));
#128277=DIRECTION('ref_axis',(-1.,7.97077743482043E-31,-1.4081690688991E-16));
#128278=DIRECTION('',(0.994521895368274,-0.104528463267647,-5.89872860613828E-16));
#128279=DIRECTION('center_axis',(1.4081690688991E-16,6.98296267768627E-15,
-1.));
#128280=DIRECTION('ref_axis',(1.,-7.97077743482043E-31,1.4081690688991E-16));
#128281=DIRECTION('',(-0.500005191251989,-4.77800115933347E-6,-0.866022406579779));
#128282=DIRECTION('center_axis',(1.4081690688991E-16,6.98296267768627E-15,
-1.));
#128283=DIRECTION('ref_axis',(-1.,7.97577417048809E-31,-1.40816906889911E-16));
#128284=DIRECTION('',(0.497265611060783,-0.0522695260942018,0.86602240657978));
#128285=DIRECTION('center_axis',(-1.4081690688991E-16,-6.98296267768627E-15,
1.));
#128286=DIRECTION('ref_axis',(-1.,9.83319205199467E-31,-1.40816906889911E-16));
#128287=DIRECTION('center_axis',(-1.4081690688991E-16,-6.98296267768627E-15,
1.));
#128288=DIRECTION('ref_axis',(-1.,7.98248735348668E-31,-1.4081690688991E-16));
#128289=DIRECTION('',(-1.,9.83319205199467E-31,-1.40816906889911E-16));
#128290=DIRECTION('center_axis',(1.4081690688991E-16,6.98296267768627E-15,
-1.));
#128291=DIRECTION('ref_axis',(-1.,7.98707387273907E-31,-1.4081690688991E-16));
#128292=DIRECTION('',(0.994521895368274,-0.104528463267647,-5.89872860613828E-16));
#128293=DIRECTION('center_axis',(-1.4081690688991E-16,-6.98296267768627E-15,
1.));
#128294=DIRECTION('ref_axis',(-1.,7.99150043815584E-31,-1.4081690688991E-16));
#128295=DIRECTION('center_axis',(-1.4081690688991E-16,-6.98296267768627E-15,
1.));
#128296=DIRECTION('ref_axis',(1.,-7.99370576998456E-31,1.4081690688991E-16));
#128297=DIRECTION('',(-0.500004991781227,4.62770264658402E-6,0.866022521746657));
#128298=DIRECTION('center_axis',(-1.4081690688991E-16,-6.98296267768627E-15,
1.));
#128299=DIRECTION('ref_axis',(-1.,7.99858039355471E-31,-1.4081690688991E-16));
#128300=DIRECTION('center_axis',(-1.4081690688991E-16,-6.98296267768627E-15,
1.));
#128301=DIRECTION('ref_axis',(-1.,7.99858039355471E-31,-1.4081690688991E-16));
#128302=DIRECTION('center_axis',(-1.4081690688991E-16,-6.98296267768627E-15,
1.));
#128303=DIRECTION('ref_axis',(-1.,7.99858039355471E-31,-1.4081690688991E-16));
#128304=DIRECTION('',(0.497266395846507,-0.0522601510654256,-0.86602252174666));
#128305=DIRECTION('center_axis',(-1.4081690688991E-16,-6.98296267768627E-15,
1.));
#128306=DIRECTION('ref_axis',(-1.,9.83319205199467E-31,-1.40816906889911E-16));
#128307=DIRECTION('',(-1.,9.83319205199467E-31,-1.40816906889911E-16));
#128308=DIRECTION('center_axis',(1.4081690688991E-16,6.98296267768627E-15,
-1.));
#128309=DIRECTION('ref_axis',(-1.,8.01265634860448E-31,-1.4081690688991E-16));
#128310=DIRECTION('',(0.994521895368274,-0.104528463267647,-5.89872860613828E-16));
#128311=DIRECTION('center_axis',(-1.4081690688991E-16,-6.98296267768627E-15,
1.));
#128312=DIRECTION('ref_axis',(-1.,8.32577322149061E-31,-1.39145123902276E-16));
#128313=DIRECTION('center_axis',(-0.00107025596477632,-0.999999427244995,
-7.86457202049714E-6));
#128314=DIRECTION('ref_axis',(-1.47312953562887E-6,-7.86299989814554E-6,
0.999999999968002));
#128315=DIRECTION('center_axis',(0.103464010407677,0.994633197962198,-7.86457228356451E-6));
#128316=DIRECTION('ref_axis',(0.84349396678185,-0.0877379732620883,0.529924500330452));
#128317=DIRECTION('center_axis',(-1.4081690688991E-16,-6.98296267768627E-15,
1.));
#128318=DIRECTION('ref_axis',(-1.,8.07722881720021E-31,-1.42096112075504E-16));
#128319=DIRECTION('center_axis',(-0.00102464806165045,-0.999999475000305,
9.77058601886064E-6));
#128320=DIRECTION('ref_axis',(0.874641264344646,-0.000891463458079829,0.484769908305479));
#128321=DIRECTION('center_axis',(0.103509373496843,0.994628478127802,9.77051526104263E-6));
#128322=DIRECTION('ref_axis',(0.869950553189323,-0.0905391058403489,0.484756336027927));
#128323=DIRECTION('center_axis',(-1.4081690688991E-16,-6.98296267768627E-15,
1.));
#128324=DIRECTION('ref_axis',(-1.,8.24049048117772E-31,-1.37719829560012E-16));
#128325=DIRECTION('center_axis',(-0.00259831235056312,0.999996624215829,
-1.81624797722911E-5));
#128326=DIRECTION('ref_axis',(0.865241946199094,0.00223907064277737,-0.501349539842474));
#128327=DIRECTION('center_axis',(-0.107112171226389,-0.994246942387258,
-1.81316452158989E-5));
#128328=DIRECTION('ref_axis',(0.861994650487816,-0.0928552846709603,-0.498340364248234));
#128329=DIRECTION('center_axis',(-1.4081690688991E-16,-6.98296267768627E-15,
1.));
#128330=DIRECTION('ref_axis',(-1.,8.26087817385229E-31,-1.38060560438432E-16));
#128331=DIRECTION('center_axis',(-0.0026118242750409,0.999996589010146,
-1.84940601491707E-5));
#128332=DIRECTION('ref_axis',(0.866979057020819,0.00227362102098813,0.498339387701539));
#128333=DIRECTION('center_axis',(-0.107125604983594,-0.9942454950432,-1.85257091479021E-5));
#128334=DIRECTION('ref_axis',(0.860265387815186,-0.0926991758195122,0.501348506858822));
#128335=DIRECTION('center_axis',(-1.4081690688991E-16,-6.98296267768627E-15,
1.));
#128336=DIRECTION('ref_axis',(-1.,9.83319205199467E-31,-1.40816906889911E-16));
#128337=DIRECTION('center_axis',(-1.4081690688991E-16,-6.98296267768627E-15,
1.));
#128338=DIRECTION('ref_axis',(-1.,8.46073526001725E-31,-1.4081690688991E-16));
#128339=DIRECTION('',(-0.994521895368274,0.104528463267647,5.89872860613828E-16));
#128340=DIRECTION('center_axis',(-1.4081690688991E-16,-6.98296267768627E-15,
1.));
#128341=DIRECTION('ref_axis',(-1.,7.97077743482043E-31,-1.4081690688991E-16));
#128342=DIRECTION('center_axis',(-1.4081690688991E-16,-6.98296267768627E-15,
1.));
#128343=DIRECTION('ref_axis',(-1.,7.97077743482043E-31,-1.4081690688991E-16));
#128344=DIRECTION('center_axis',(-1.4081690688991E-16,-6.98296267768627E-15,
1.));
#128345=DIRECTION('ref_axis',(-1.,7.97077743482043E-31,-1.4081690688991E-16));
#128346=DIRECTION('',(0.978147600733807,-0.207911690817753,-1.3140998576179E-15));
#128347=DIRECTION('center_axis',(1.4081690688991E-16,6.98296267768627E-15,
-1.));
#128348=DIRECTION('ref_axis',(1.,-7.97077743482043E-31,1.4081690688991E-16));
#128349=DIRECTION('',(-0.49726660993504,0.0522600224406429,-0.86602240657977));
#128350=DIRECTION('center_axis',(1.4081690688991E-16,6.98296267768627E-15,
-1.));
#128351=DIRECTION('ref_axis',(-1.,7.97577417048809E-31,-1.40816906889911E-16));
#128352=DIRECTION('',(0.489077884775249,-0.103961598321242,0.866022406579796));
#128353=DIRECTION('center_axis',(-1.4081690688991E-16,-6.98296267768627E-15,
1.));
#128354=DIRECTION('ref_axis',(-1.,9.83319205199467E-31,-1.40816906889911E-16));
#128355=DIRECTION('center_axis',(-1.4081690688991E-16,-6.98296267768627E-15,
1.));
#128356=DIRECTION('ref_axis',(-1.,7.98248735348668E-31,-1.4081690688991E-16));
#128357=DIRECTION('',(-0.994521895368274,0.104528463267647,5.89872860613828E-16));
#128358=DIRECTION('center_axis',(1.4081690688991E-16,6.98296267768627E-15,
-1.));
#128359=DIRECTION('ref_axis',(-1.,7.98707387273907E-31,-1.4081690688991E-16));
#128360=DIRECTION('',(0.978147600733807,-0.207911690817753,-1.3140998576179E-15));
#128361=DIRECTION('center_axis',(-1.4081690688991E-16,-6.98296267768627E-15,
1.));
#128362=DIRECTION('ref_axis',(-1.,7.99150043815584E-31,-1.4081690688991E-16));
#128363=DIRECTION('center_axis',(-1.4081690688991E-16,-6.98296267768627E-15,
1.));
#128364=DIRECTION('ref_axis',(1.,-7.99370576998456E-31,1.4081690688991E-16));
#128365=DIRECTION('',(-0.497265428393217,0.0522693557686506,0.866022521746658));
#128366=DIRECTION('center_axis',(-1.4081690688991E-16,-6.98296267768627E-15,
1.));
#128367=DIRECTION('ref_axis',(-1.,7.99858039355471E-31,-1.4081690688991E-16));
#128368=DIRECTION('center_axis',(-1.4081690688991E-16,-6.98296267768627E-15,
1.));
#128369=DIRECTION('ref_axis',(-1.,7.99858039355471E-31,-1.4081690688991E-16));
#128370=DIRECTION('center_axis',(-1.4081690688991E-16,-6.98296267768627E-15,
1.));
#128371=DIRECTION('ref_axis',(-1.,7.99858039355471E-31,-1.4081690688991E-16));
#128372=DIRECTION('',(0.489079645219225,-0.1039523566823,-0.866022521746653));
#128373=DIRECTION('center_axis',(-1.4081690688991E-16,-6.98296267768627E-15,
1.));
#128374=DIRECTION('ref_axis',(-1.,9.83319205199467E-31,-1.40816906889911E-16));
#128375=DIRECTION('',(-0.994521895368274,0.104528463267647,5.89872860613828E-16));
#128376=DIRECTION('center_axis',(1.4081690688991E-16,6.98296267768627E-15,
-1.));
#128377=DIRECTION('ref_axis',(-1.,8.01265634860448E-31,-1.4081690688991E-16));
#128378=DIRECTION('',(0.978147600733807,-0.207911690817753,-1.3140998576179E-15));
#128379=DIRECTION('center_axis',(-1.4081690688991E-16,-6.98296267768627E-15,
1.));
#128380=DIRECTION('ref_axis',(-1.,8.32577322149061E-31,-1.39145123902276E-16));
#128381=DIRECTION('center_axis',(-0.105592796389069,-0.99440945353958,-7.86457202324616E-6));
#128382=DIRECTION('ref_axis',(-2.28696686047185E-6,-7.66594159881603E-6,
0.999999999968002));
#128383=DIRECTION('center_axis',(0.206864703431021,0.97836955922215,-7.8645722885402E-6));
#128384=DIRECTION('ref_axis',(0.829702103060282,-0.17542646358762,0.529924500330458));
#128385=DIRECTION('center_axis',(-1.4081690688991E-16,-6.98296267768627E-15,
1.));
#128386=DIRECTION('ref_axis',(-1.,8.07722881720021E-31,-1.42096112075504E-16));
#128387=DIRECTION('center_axis',(-0.105547443321967,-0.994414268357374,
9.77058488673039E-6));
#128388=DIRECTION('ref_axis',(0.869756704678642,-0.0923114872004638,0.48476990830433));
#128389=DIRECTION('center_axis',(0.206909324658795,0.97836012350963,9.77051638199737E-6));
#128390=DIRECTION('ref_axis',(0.855720959435164,-0.180977717588963,0.484756336028372));
#128391=DIRECTION('center_axis',(-1.4081690688991E-16,-6.98296267768627E-15,
1.));
#128392=DIRECTION('ref_axis',(-1.,8.24049048117772E-31,-1.37719829560012E-16));
#128393=DIRECTION('center_axis',(0.101944031878469,0.994790135674096,-1.81624797646096E-5));
#128394=DIRECTION('ref_axis',(0.860736106897086,-0.0882156062111255,-0.501349539846655));
#128395=DIRECTION('center_axis',(-0.210452504541414,-0.977604082951524,
-1.81316452978814E-5));
#128396=DIRECTION('ref_axis',(0.847566533387204,-0.182449589866272,-0.4983403642488));
#128397=DIRECTION('center_axis',(-1.4081690688991E-16,-6.98296267768627E-15,
1.));
#128398=DIRECTION('ref_axis',(-1.,8.26087817385229E-31,-1.38060560438432E-16));
#128399=DIRECTION('center_axis',(0.101930590295467,0.994791513041797,-1.84940631498201E-5));
#128400=DIRECTION('ref_axis',(0.862467313147321,-0.088362822628798,0.498339387696289));
#128401=DIRECTION('center_axis',(-0.210465713418178,-0.977601239326227,
-1.85257095408342E-5));
#128402=DIRECTION('ref_axis',(0.845863061613335,-0.182113579025386,0.501348506861923));
#128403=DIRECTION('center_axis',(-1.4081690688991E-16,-6.98296267768627E-15,
1.));
#128404=DIRECTION('ref_axis',(-1.,9.83319205199467E-31,-1.40816906889911E-16));
#128405=DIRECTION('center_axis',(-1.4081690688991E-16,-6.98296267768627E-15,
1.));
#128406=DIRECTION('ref_axis',(-1.,8.46073526001725E-31,-1.4081690688991E-16));
#128407=DIRECTION('',(-0.978147600733807,0.207911690817753,1.3140998576179E-15));
#128408=DIRECTION('center_axis',(-1.4081690688991E-16,-6.98296267768627E-15,
1.));
#128409=DIRECTION('ref_axis',(-1.,7.97077743482043E-31,-1.4081690688991E-16));
#128410=DIRECTION('center_axis',(-1.4081690688991E-16,-6.98296267768627E-15,
1.));
#128411=DIRECTION('ref_axis',(-1.,7.97077743482043E-31,-1.4081690688991E-16));
#128412=DIRECTION('center_axis',(-1.4081690688991E-16,-6.98296267768627E-15,
1.));
#128413=DIRECTION('ref_axis',(-1.,7.97077743482043E-31,-1.4081690688991E-16));
#128414=DIRECTION('',(0.951056516295155,-0.309016994374942,-2.02392930158883E-15));
#128415=DIRECTION('center_axis',(1.4081690688991E-16,6.98296267768627E-15,
-1.));
#128416=DIRECTION('ref_axis',(1.,-7.97077743482043E-31,1.4081690688991E-16));
#128417=DIRECTION('',(-0.489079871579896,0.103952251140493,-0.86602240657977));
#128418=DIRECTION('center_axis',(1.4081690688991E-16,6.98296267768627E-15,
-1.));
#128419=DIRECTION('ref_axis',(-1.,7.97577417048809E-31,-1.40816906889911E-16));
#128420=DIRECTION('',(0.475531718838027,-0.15451464552171,0.86602240657979));
#128421=DIRECTION('center_axis',(-1.4081690688991E-16,-6.98296267768627E-15,
1.));
#128422=DIRECTION('ref_axis',(-1.,9.83319205199467E-31,-1.40816906889911E-16));
#128423=DIRECTION('center_axis',(-1.4081690688991E-16,-6.98296267768627E-15,
1.));
#128424=DIRECTION('ref_axis',(-1.,7.98248735348668E-31,-1.4081690688991E-16));
#128425=DIRECTION('',(-0.978147600733807,0.207911690817753,1.3140998576179E-15));
#128426=DIRECTION('center_axis',(1.4081690688991E-16,6.98296267768627E-15,
-1.));
#128427=DIRECTION('ref_axis',(-1.,7.98707387273907E-31,-1.4081690688991E-16));
#128428=DIRECTION('',(0.951056516295155,-0.309016994374942,-2.02392930158883E-15));
#128429=DIRECTION('center_axis',(-1.4081690688991E-16,-6.98296267768627E-15,
1.));
#128430=DIRECTION('ref_axis',(-1.,7.99150043815584E-31,-1.4081690688991E-16));
#128431=DIRECTION('center_axis',(-1.4081690688991E-16,-6.98296267768627E-15,
1.));
#128432=DIRECTION('ref_axis',(1.,-7.99370576998456E-31,1.4081690688991E-16));
#128433=DIRECTION('',(-0.489077720912262,0.103961409834795,0.866022521746651));
#128434=DIRECTION('center_axis',(-1.4081690688991E-16,-6.98296267768627E-15,
1.));
#128435=DIRECTION('ref_axis',(-1.,7.99858039355471E-31,-1.4081690688991E-16));
#128436=DIRECTION('center_axis',(-1.4081690688991E-16,-6.98296267768627E-15,
1.));
#128437=DIRECTION('ref_axis',(-1.,7.99858039355471E-31,-1.4081690688991E-16));
#128438=DIRECTION('center_axis',(-1.4081690688991E-16,-6.98296267768627E-15,
1.));
#128439=DIRECTION('ref_axis',(-1.,7.99858039355471E-31,-1.4081690688991E-16));
#128440=DIRECTION('',(0.475534435652402,-0.154505638525938,-0.86602252174666));
#128441=DIRECTION('center_axis',(-1.4081690688991E-16,-6.98296267768627E-15,
1.));
#128442=DIRECTION('ref_axis',(-1.,9.83319205199467E-31,-1.40816906889911E-16));
#128443=DIRECTION('',(-0.978147600733807,0.207911690817753,1.3140998576179E-15));
#128444=DIRECTION('center_axis',(1.4081690688991E-16,6.98296267768627E-15,
-1.));
#128445=DIRECTION('ref_axis',(-1.,8.01265634860448E-31,-1.4081690688991E-16));
#128446=DIRECTION('',(0.951056516295155,-0.309016994374942,-2.02392930158883E-15));
#128447=DIRECTION('center_axis',(-1.4081690688991E-16,-6.98296267768627E-15,
1.));
#128448=DIRECTION('ref_axis',(-1.,8.32577322149061E-31,-1.39145123902276E-16));
#128449=DIRECTION('center_axis',(-0.208958440039409,-0.977924521767629,
-7.8645720061062E-6));
#128450=DIRECTION('ref_axis',(-3.07574767837472E-6,-7.38489362573465E-6,
0.999999999968001));
#128451=DIRECTION('center_axis',(0.30799894347438,0.951386698854264,-7.86457224109976E-6));
#128452=DIRECTION('ref_axis',(0.806819849471229,-0.26119294486778,0.529924500330491));
#128453=DIRECTION('center_axis',(-1.4081690688991E-16,-6.98296267768627E-15,
1.));
#128454=DIRECTION('ref_axis',(-1.,8.07722881720021E-31,-1.42096112075504E-16));
#128455=DIRECTION('center_axis',(-0.208913838705841,-0.977934050895931,
9.77058339197564E-6));
#128456=DIRECTION('ref_axis',(0.855342908547101,-0.182720126971624,0.484769908304609));
#128457=DIRECTION('center_axis',(0.308042333962524,0.951372650642984,9.77051511636161E-6));
#128458=DIRECTION('ref_axis',(0.832115907779852,-0.269433499592107,0.484756336025908));
#128459=DIRECTION('center_axis',(-1.4081690688991E-16,-6.98296267768627E-15,
1.));
#128460=DIRECTION('ref_axis',(-1.,8.24049048117772E-31,-1.37719829560012E-16));
#128461=DIRECTION('center_axis',(0.205369455961115,0.978684518232694,-1.81624798107456E-5));
#128462=DIRECTION('ref_axis',(0.846799862691689,-0.177703774423541,-0.501349539843176));
#128463=DIRECTION('center_axis',(-0.311487076176515,-0.950250388606208,
-1.81316450997518E-5));
#128464=DIRECTION('ref_axis',(0.8238522999842,-0.270044939175598,-0.498340364245554));
#128465=DIRECTION('center_axis',(-1.4081690688991E-16,-6.98296267768627E-15,
1.));
#128466=DIRECTION('ref_axis',(-1.,8.26087817385229E-31,-1.38060560438432E-16));
#128467=DIRECTION('center_axis',(0.205356231983588,0.978687293083686,-1.84940578039158E-5));
#128468=DIRECTION('ref_axis',(0.84850619690631,-0.178031144702993,0.498339387694101));
#128469=DIRECTION('center_axis',(-0.311499915462665,-0.950246179852122,
-1.85256937060462E-5));
#128470=DIRECTION('ref_axis',(0.822193282703536,-0.269532707750384,0.50134850685918));
#128471=DIRECTION('center_axis',(-1.4081690688991E-16,-6.98296267768627E-15,
1.));
#128472=DIRECTION('ref_axis',(-1.,9.83319205199467E-31,-1.40816906889911E-16));
#128473=DIRECTION('center_axis',(-1.4081690688991E-16,-6.98296267768627E-15,
1.));
#128474=DIRECTION('ref_axis',(-1.,8.46073526001725E-31,-1.4081690688991E-16));
#128475=DIRECTION('',(-0.951056516295155,0.309016994374942,2.02392930158883E-15));
#128476=DIRECTION('center_axis',(-1.4081690688991E-16,-6.98296267768627E-15,
1.));
#128477=DIRECTION('ref_axis',(-1.,7.97077743482043E-31,-1.4081690688991E-16));
#128478=DIRECTION('center_axis',(-1.4081690688991E-16,-6.98296267768627E-15,
1.));
#128479=DIRECTION('ref_axis',(-1.,7.97077743482043E-31,-1.4081690688991E-16));
#128480=DIRECTION('center_axis',(-1.4081690688991E-16,-6.98296267768627E-15,
1.));
#128481=DIRECTION('ref_axis',(-1.,7.97077743482043E-31,-1.4081690688991E-16));
#128482=DIRECTION('',(0.913545457642603,-0.406736643075795,-2.71158415259712E-15));
#128483=DIRECTION('center_axis',(1.4081690688991E-16,6.98296267768627E-15,
-1.));
#128484=DIRECTION('ref_axis',(1.,-7.97077743482043E-31,1.4081690688991E-16));
#128485=DIRECTION('',(-0.475534671805145,0.154505557223411,-0.866022406579793));
#128486=DIRECTION('center_axis',(1.4081690688991E-16,6.98296267768627E-15,
-1.));
#128487=DIRECTION('ref_axis',(-1.,7.97577417048809E-31,-1.40816906889911E-16));
#128488=DIRECTION('',(0.456775527877802,-0.203374797931582,0.866022406579786));
#128489=DIRECTION('center_axis',(-1.4081690688991E-16,-6.98296267768627E-15,
1.));
#128490=DIRECTION('ref_axis',(-1.,9.83319205199467E-31,-1.40816906889911E-16));
#128491=DIRECTION('center_axis',(-1.4081690688991E-16,-6.98296267768627E-15,
1.));
#128492=DIRECTION('ref_axis',(-1.,7.98248735348668E-31,-1.4081690688991E-16));
#128493=DIRECTION('',(-0.951056516295155,0.309016994374942,2.02392930158883E-15));
#128494=DIRECTION('center_axis',(1.4081690688991E-16,6.98296267768627E-15,
-1.));
#128495=DIRECTION('ref_axis',(-1.,7.98707387273907E-31,-1.4081690688991E-16));
#128496=DIRECTION('',(0.913545457642603,-0.406736643075795,-2.71158415259712E-15));
#128497=DIRECTION('center_axis',(-1.4081690688991E-16,-6.98296267768627E-15,
1.));
#128498=DIRECTION('ref_axis',(-1.,7.99150043815584E-31,-1.4081690688991E-16));
#128499=DIRECTION('center_axis',(-1.4081690688991E-16,-6.98296267768627E-15,
1.));
#128500=DIRECTION('ref_axis',(1.,-7.99370576998456E-31,1.4081690688991E-16));
#128501=DIRECTION('',(-0.47553157557486,0.154514440939468,0.866022521746666));
#128502=DIRECTION('center_axis',(-1.4081690688991E-16,-6.98296267768627E-15,
1.));
#128503=DIRECTION('ref_axis',(-1.,7.99858039355471E-31,-1.4081690688991E-16));
#128504=DIRECTION('center_axis',(-1.4081690688991E-16,-6.98296267768627E-15,
1.));
#128505=DIRECTION('ref_axis',(-1.,7.99858039355471E-31,-1.4081690688991E-16));
#128506=DIRECTION('center_axis',(-1.4081690688991E-16,-6.98296267768627E-15,
1.));
#128507=DIRECTION('ref_axis',(-1.,7.99858039355471E-31,-1.4081690688991E-16));
#128508=DIRECTION('',(0.456779171296619,-0.203366124261481,-0.866022521746656));
#128509=DIRECTION('center_axis',(-1.4081690688991E-16,-6.98296267768627E-15,
1.));
#128510=DIRECTION('ref_axis',(-1.,9.83319205199467E-31,-1.40816906889911E-16));
#128511=DIRECTION('',(-0.951056516295155,0.309016994374942,2.02392930158883E-15));
#128512=DIRECTION('center_axis',(1.4081690688991E-16,6.98296267768627E-15,
-1.));
#128513=DIRECTION('ref_axis',(-1.,8.01265634860448E-31,-1.4081690688991E-16));
#128514=DIRECTION('',(0.913545457642603,-0.406736643075795,-2.71158415259712E-15));
#128515=DIRECTION('center_axis',(-1.4081690688991E-16,-6.98296267768627E-15,
1.));
#128516=DIRECTION('ref_axis',(-1.,8.32577322149061E-31,-1.39145123902276E-16));
#128517=DIRECTION('center_axis',(-0.310034691293285,-0.950725244291339,
-7.86457195103406E-6));
#128518=DIRECTION('ref_axis',(-3.83082999767964E-6,-7.02293516957875E-6,
0.999999999968002));
#128519=DIRECTION('center_axis',(0.405758682640086,0.913980246723271,-7.86457225038894E-6));
#128520=DIRECTION('ref_axis',(0.775097908773516,-0.344097741585796,0.52992450033045));
#128521=DIRECTION('center_axis',(-1.4081690688991E-16,-6.98296267768627E-15,
1.));
#128522=DIRECTION('ref_axis',(-1.,8.07722881720021E-31,-1.42096112075504E-16));
#128523=DIRECTION('center_axis',(-0.309991330356945,-0.950739383326507,
9.77058572337612E-6));
#128524=DIRECTION('ref_axis',(0.831557796518639,-0.271126846795441,0.484769908302721));
#128525=DIRECTION('center_axis',(0.405800366992264,0.913961739928691,9.77051586747459E-6));
#128526=DIRECTION('ref_axis',(0.799394020104308,-0.354937311790024,0.4847563360295));
#128527=DIRECTION('center_axis',(-1.4081690688991E-16,-6.98296267768627E-15,
1.));
#128528=DIRECTION('ref_axis',(-1.,8.24049048117772E-31,-1.37719829560012E-16));
#128529=DIRECTION('center_axis',(0.306544809307919,0.951856228406631,-1.81624797016104E-5));
#128530=DIRECTION('ref_axis',(0.82358590198436,-0.265244982896167,-0.501349539843232));
#128531=DIRECTION('center_axis',(-0.409108930222424,-0.912485552150557,
-1.81316453007737E-5));
#128532=DIRECTION('ref_axis',(0.791111768376538,-0.35468161961952,-0.498340364249396));
#128533=DIRECTION('center_axis',(-1.4081690688991E-16,-6.98296267768627E-15,
1.));
#128534=DIRECTION('ref_axis',(-1.,8.26087817385229E-31,-1.38060560438432E-16));
#128535=DIRECTION('center_axis',(0.306531947828316,0.95186037033724,-1.84940663645596E-5));
#128536=DIRECTION('ref_axis',(0.825248669207167,-0.265748920299591,0.498339387698185));
#128537=DIRECTION('center_axis',(-0.409121259236094,-0.912480024382929,
-1.85256990525701E-5));
#128538=DIRECTION('ref_axis',(0.789515382129796,-0.35399877972475,0.50134850686307));
#128539=DIRECTION('center_axis',(-1.4081690688991E-16,-6.98296267768627E-15,
1.));
#128540=DIRECTION('ref_axis',(-1.,9.83319205199467E-31,-1.40816906889911E-16));
#128541=DIRECTION('center_axis',(-1.4081690688991E-16,-6.98296267768627E-15,
1.));
#128542=DIRECTION('ref_axis',(-1.,8.46073526001725E-31,-1.4081690688991E-16));
#128543=DIRECTION('',(-0.913545457642603,0.406736643075795,2.71158415259712E-15));
#128544=DIRECTION('center_axis',(-1.4081690688991E-16,-6.98296267768627E-15,
1.));
#128545=DIRECTION('ref_axis',(-1.,7.97077743482043E-31,-1.4081690688991E-16));
#128546=DIRECTION('center_axis',(-1.4081690688991E-16,-6.98296267768627E-15,
1.));
#128547=DIRECTION('ref_axis',(-1.,7.97077743482043E-31,-1.4081690688991E-16));
#128548=DIRECTION('center_axis',(-1.4081690688991E-16,-6.98296267768627E-15,
1.));
#128549=DIRECTION('ref_axis',(-1.,7.97077743482043E-31,-1.4081690688991E-16));
#128550=DIRECTION('',(0.866025403784442,-0.499999999999995,-3.36953032019409E-15));
#128551=DIRECTION('center_axis',(1.4081690688991E-16,6.98296267768627E-15,
-1.));
#128552=DIRECTION('ref_axis',(1.,-7.97077743482043E-31,1.4081690688991E-16));
#128553=DIRECTION('',(-0.456779414654135,0.203366068089035,-0.866022406579779));
#128554=DIRECTION('center_axis',(1.4081690688991E-16,6.98296267768627E-15,
-1.));
#128555=DIRECTION('ref_axis',(-1.,7.97577417048809E-31,-1.40816906889911E-16));
#128556=DIRECTION('',(0.433014808647741,-0.250006733496384,0.866022406579777));
#128557=DIRECTION('center_axis',(-1.4081690688991E-16,-6.98296267768627E-15,
1.));
#128558=DIRECTION('ref_axis',(-1.,9.83319205199467E-31,-1.40816906889911E-16));
#128559=DIRECTION('center_axis',(-1.4081690688991E-16,-6.98296267768627E-15,
1.));
#128560=DIRECTION('ref_axis',(-1.,7.98248735348668E-31,-1.4081690688991E-16));
#128561=DIRECTION('',(-0.913545457642603,0.406736643075795,2.71158415259712E-15));
#128562=DIRECTION('center_axis',(1.4081690688991E-16,6.98296267768627E-15,
-1.));
#128563=DIRECTION('ref_axis',(-1.,-8.88178419700125E-16,-1.40816906889917E-16));
#128564=DIRECTION('',(0.866025403784442,-0.499999999999995,-3.36953032019409E-15));
#128565=DIRECTION('center_axis',(-1.4081690688991E-16,-6.98296267768627E-15,
1.));
#128566=DIRECTION('ref_axis',(-1.,7.99150043815584E-31,-1.4081690688991E-16));
#128567=DIRECTION('center_axis',(-1.4081690688991E-16,-6.98296267768627E-15,
1.));
#128568=DIRECTION('ref_axis',(1.,-7.99370576998456E-31,1.4081690688991E-16));
#128569=DIRECTION('',(-0.456775406784115,0.203374579494968,0.866022521746664));
#128570=DIRECTION('center_axis',(-1.4081690688991E-16,-6.98296267768627E-15,
1.));
#128571=DIRECTION('ref_axis',(-1.,7.99858039355471E-31,-1.4081690688991E-16));
#128572=DIRECTION('center_axis',(-1.4081690688991E-16,-6.98296267768627E-15,
1.));
#128573=DIRECTION('ref_axis',(-1.,7.99858039355471E-31,-1.4081690688991E-16));
#128574=DIRECTION('center_axis',(-1.4081690688991E-16,-6.98296267768627E-15,
1.));
#128575=DIRECTION('ref_axis',(-1.,7.99858039355471E-31,-1.4081690688991E-16));
#128576=DIRECTION('',(0.433019338752905,-0.249998488182556,-0.866022521746654));
#128577=DIRECTION('center_axis',(-1.4081690688991E-16,-6.98296267768627E-15,
1.));
#128578=DIRECTION('ref_axis',(-1.,9.83319205199467E-31,-1.40816906889911E-16));
#128579=DIRECTION('',(-0.913545457642603,0.406736643075795,2.71158415259712E-15));
#128580=DIRECTION('center_axis',(1.4081690688991E-16,6.98296267768627E-15,
-1.));
#128581=DIRECTION('ref_axis',(-1.,-8.88178419700124E-16,-1.40816906889917E-16));
#128582=DIRECTION('',(0.866025403784442,-0.499999999999995,-3.36953032019409E-15));
#128583=DIRECTION('center_axis',(-1.4081690688991E-16,-6.98296267768627E-15,
1.));
#128584=DIRECTION('ref_axis',(-1.,8.32577322149061E-31,-1.39145123902276E-16));
#128585=DIRECTION('center_axis',(-0.40771413759047,-0.913109622086531,-7.86457197304049E-6));
#128586=DIRECTION('ref_axis',(-4.54394094117637E-6,-6.58403204443663E-6,
0.999999999968002));
#128587=DIRECTION('center_axis',(0.499072844768338,0.866560035746507,-7.86457221234716E-6));
#128588=DIRECTION('ref_axis',(0.734883833187562,-0.42323253143994,0.529924500330467));
#128589=DIRECTION('center_axis',(-1.4081690688991E-16,-6.98296267768627E-15,
1.));
#128590=DIRECTION('ref_axis',(-1.,8.07722881720021E-31,-1.42096112075504E-16));
#128591=DIRECTION('center_axis',(-0.407672492120118,-0.913128216119242,
9.77058304390627E-6));
#128592=DIRECTION('ref_axis',(0.798661963253854,-0.356563044147659,0.484769908306667));
#128593=DIRECTION('center_axis',(0.499112366281669,0.866537273133274,9.77051750932866E-6));
#128594=DIRECTION('ref_axis',(0.75791380426364,-0.436552356525874,0.484756336027001));
#128595=DIRECTION('center_axis',(-1.4081690688991E-16,-6.98296267768627E-15,
1.));
#128596=DIRECTION('ref_axis',(-1.,8.24049048117772E-31,-1.37719829560012E-16));
#128597=DIRECTION('center_axis',(0.404361593575304,0.914599202553427,-1.81624796427904E-5));
#128598=DIRECTION('ref_axis',(0.791348561789414,-0.349880111830527,-0.5013495398415));
#128599=DIRECTION('center_axis',(-0.50224850121709,-0.864723333035735,-1.81316452500637E-5));
#128600=DIRECTION('ref_axis',(0.749703650682099,-0.435432334015447,-0.498340364256994));
#128601=DIRECTION('center_axis',(-1.4081690688991E-16,-6.98296267768627E-15,
1.));
#128602=DIRECTION('ref_axis',(-1.,8.26087817385229E-31,-1.38060560438432E-16));
#128603=DIRECTION('center_axis',(0.404349235502748,0.914604666184419,-1.84940679887669E-5));
#128604=DIRECTION('ref_axis',(0.792949544396104,-0.350555095114341,0.498339387698169));
#128605=DIRECTION('center_axis',(-0.502260184873573,-0.864716546821883,
-1.8525716205892E-5));
#128606=DIRECTION('ref_axis',(0.748187385815693,-0.434586366990651,0.501348506861391));
#128607=DIRECTION('center_axis',(-1.4081690688991E-16,-6.98296267768627E-15,
1.));
#128608=DIRECTION('ref_axis',(-1.,9.83319205199467E-31,-1.40816906889911E-16));
#128609=DIRECTION('center_axis',(-1.4081690688991E-16,-6.98296267768627E-15,
1.));
#128610=DIRECTION('ref_axis',(-1.,8.46073526001725E-31,-1.4081690688991E-16));
#128611=DIRECTION('',(-0.866025403784442,0.499999999999995,3.36953032019409E-15));
#128612=DIRECTION('center_axis',(-1.4081690688991E-16,-6.98296267768627E-15,
1.));
#128613=DIRECTION('ref_axis',(-1.,7.97077743482043E-31,-1.4081690688991E-16));
#128614=DIRECTION('center_axis',(-1.4081690688991E-16,-6.98296267768627E-15,
1.));
#128615=DIRECTION('ref_axis',(-1.,7.97077743482043E-31,-1.4081690688991E-16));
#128616=DIRECTION('center_axis',(-1.4081690688991E-16,-6.98296267768627E-15,
1.));
#128617=DIRECTION('ref_axis',(-1.,7.97077743482043E-31,-1.4081690688991E-16));
#128618=DIRECTION('',(0.80901699437495,-0.587785252292469,-3.99055920848346E-15));
#128619=DIRECTION('center_axis',(1.4081690688991E-16,6.98296267768627E-15,
-1.));
#128620=DIRECTION('ref_axis',(1.,-7.97077743482043E-31,1.4081690688991E-16));
#128621=DIRECTION('',(-0.433019586648885,0.249998457755584,-0.866022406579794));
#128622=DIRECTION('center_axis',(1.4081690688991E-16,6.98296267768627E-15,
-1.));
#128623=DIRECTION('ref_axis',(-1.,7.97577417048809E-31,-1.40816906889911E-16));
#128624=DIRECTION('',(0.404509888559933,-0.293899542971735,0.866022406579781));
#128625=DIRECTION('center_axis',(-1.4081690688991E-16,-6.98296267768627E-15,
1.));
#128626=DIRECTION('ref_axis',(-1.,9.83319205199467E-31,-1.40816906889911E-16));
#128627=DIRECTION('center_axis',(-1.4081690688991E-16,-6.98296267768627E-15,
1.));
#128628=DIRECTION('ref_axis',(-1.,7.98248735348668E-31,-1.4081690688991E-16));
#128629=DIRECTION('',(-0.866025403784442,0.499999999999995,3.36953032019409E-15));
#128630=DIRECTION('center_axis',(1.4081690688991E-16,6.98296267768627E-15,
-1.));
#128631=DIRECTION('ref_axis',(-1.,-8.88178419700125E-16,-1.40816906889917E-16));
#128632=DIRECTION('',(0.80901699437495,-0.587785252292469,-3.99055920848346E-15));
#128633=DIRECTION('center_axis',(-1.4081690688991E-16,-6.98296267768627E-15,
1.));
#128634=DIRECTION('ref_axis',(-1.,7.99150043815584E-31,-1.4081690688991E-16));
#128635=DIRECTION('center_axis',(-1.4081690688991E-16,-6.98296267768627E-15,
1.));
#128636=DIRECTION('ref_axis',(1.,-7.99370576998456E-31,1.4081690688991E-16));
#128637=DIRECTION('',(-0.433014711050232,0.250006503598672,0.866022521746664));
#128638=DIRECTION('center_axis',(-1.4081690688991E-16,-6.98296267768627E-15,
1.));
#128639=DIRECTION('ref_axis',(-1.,7.99858039355471E-31,-1.4081690688991E-16));
#128640=DIRECTION('center_axis',(-1.4081690688991E-16,-6.98296267768627E-15,
1.));
#128641=DIRECTION('ref_axis',(-1.,7.99858039355471E-31,-1.4081690688991E-16));
#128642=DIRECTION('center_axis',(-1.4081690688991E-16,-6.98296267768627E-15,
1.));
#128643=DIRECTION('ref_axis',(-1.,7.99858039355471E-31,-1.4081690688991E-16));
#128644=DIRECTION('',(0.4045152557187,-0.293891816351548,-0.866022521746648));
#128645=DIRECTION('center_axis',(-1.4081690688991E-16,-6.98296267768627E-15,
1.));
#128646=DIRECTION('ref_axis',(-1.,9.83319205199467E-31,-1.40816906889911E-16));
#128647=DIRECTION('',(-0.866025403784442,0.499999999999995,3.36953032019409E-15));
#128648=DIRECTION('center_axis',(1.4081690688991E-16,6.98296267768627E-15,
-1.));
#128649=DIRECTION('ref_axis',(-1.,8.01265634860448E-31,-1.4081690688991E-16));
#128650=DIRECTION('',(0.80901699437495,-0.587785252292469,-3.99055920848346E-15));
#128651=DIRECTION('center_axis',(-1.4081690688991E-16,-6.98296267768627E-15,
1.));
#128652=DIRECTION('ref_axis',(-1.,8.32577322149061E-31,-1.39145123902276E-16));
#128653=DIRECTION('center_axis',(-0.500926582476549,-0.865489779781664,
-7.86457205664364E-6));
#128654=DIRECTION('ref_axis',(-5.20726753510821E-6,-6.0729929450695E-6,
0.999999999968002));
#128655=DIRECTION('center_axis',(0.586919060371537,0.809645611678802,-7.86457238663011E-6));
#128656=DIRECTION('ref_axis',(0.686618216540999,-0.497730297112391,0.529924500330442));
#128657=DIRECTION('center_axis',(-1.4081690688991E-16,-6.98296267768627E-15,
1.));
#128658=DIRECTION('ref_axis',(-1.,8.07722881720021E-31,-1.42096112075504E-16));
#128659=DIRECTION('center_axis',(-0.500887108752324,-0.865512625090052,
9.77058776453254E-6));
#128660=DIRECTION('ref_axis',(0.757015822392177,-0.438092662173928,0.484769908304193));
#128661=DIRECTION('center_axis',(0.586955986040212,0.809618842638991,9.77051913842785E-6));
#128662=DIRECTION('ref_axis',(0.708129726178395,-0.513384442288506,0.484756336027318));
#128663=DIRECTION('center_axis',(-1.4081690688991E-16,-6.98296267768627E-15,
1.));
#128664=DIRECTION('ref_axis',(-1.,8.24049048117772E-31,-1.37719829560012E-16));
#128665=DIRECTION('center_axis',(0.497748107605313,0.867321636444897,-1.8162479830695E-5));
#128666=DIRECTION('ref_axis',(0.750441041151826,-0.430681881043238,-0.501349539838247));
#128667=DIRECTION('center_axis',(-0.58988533253017,-0.807487024129189,-1.81316452233006E-5));
#128668=DIRECTION('ref_axis',(0.700081622911622,-0.51141236064337,-0.498340364251789));
#128669=DIRECTION('center_axis',(-1.4081690688991E-16,-6.98296267768627E-15,
1.));
#128670=DIRECTION('ref_axis',(-1.,8.26087817385229E-31,-1.38060560438432E-16));
#128671=DIRECTION('center_axis',(0.497736388334897,0.867328361916813,-1.84940646400988E-5));
#128672=DIRECTION('ref_axis',(0.751962698442603,-0.431520514949369,0.498339387695524));
#128673=DIRECTION('center_axis',(-0.589896242825295,-0.807479053819601,
-1.85257260569587E-5));
#128674=DIRECTION('ref_axis',(0.698662091935,-0.510412535077464,0.50134850685806));
#128675=DIRECTION('center_axis',(-1.4081690688991E-16,-6.98296267768627E-15,
1.));
#128676=DIRECTION('ref_axis',(-1.,9.83319205199467E-31,-1.40816906889911E-16));
#128677=DIRECTION('center_axis',(-1.4081690688991E-16,-6.98296267768627E-15,
1.));
#128678=DIRECTION('ref_axis',(-1.,8.46073526001725E-31,-1.4081690688991E-16));
#128679=DIRECTION('',(-0.80901699437495,0.587785252292469,3.99055920848346E-15));
#128680=DIRECTION('center_axis',(-1.4081690688991E-16,-6.98296267768627E-15,
1.));
#128681=DIRECTION('ref_axis',(-1.,7.97077743482043E-31,-1.4081690688991E-16));
#128682=DIRECTION('center_axis',(-1.4081690688991E-16,-6.98296267768627E-15,
1.));
#128683=DIRECTION('ref_axis',(-1.,7.97077743482043E-31,-1.4081690688991E-16));
#128684=DIRECTION('center_axis',(-1.4081690688991E-16,-6.98296267768627E-15,
1.));
#128685=DIRECTION('ref_axis',(-1.,7.97077743482043E-31,-1.4081690688991E-16));
#128686=DIRECTION('',(0.743144825477398,-0.669130606358854,-4.56786669500649E-15));
#128687=DIRECTION('center_axis',(1.4081690688991E-16,6.98296267768627E-15,
-1.));
#128688=DIRECTION('ref_axis',(1.,-7.97077743482043E-31,1.4081690688991E-16));
#128689=DIRECTION('',(-0.404515505437171,0.293891812003427,-0.866022406579791));
#128690=DIRECTION('center_axis',(1.4081690688991E-16,6.98296267768627E-15,
-1.));
#128691=DIRECTION('ref_axis',(-1.,-8.88178419700124E-16,-1.40816906889917E-16));
#128692=DIRECTION('',(0.371573073483921,-0.33457232755186,0.866022406579786));
#128693=DIRECTION('center_axis',(-1.4081690688991E-16,-6.98296267768627E-15,
1.));
#128694=DIRECTION('ref_axis',(-1.,9.83319205199467E-31,-1.40816906889911E-16));
#128695=DIRECTION('center_axis',(-1.4081690688991E-16,-6.98296267768627E-15,
1.));
#128696=DIRECTION('ref_axis',(-1.,7.98248735348668E-31,-1.4081690688991E-16));
#128697=DIRECTION('',(-0.80901699437495,0.587785252292469,3.99055920848346E-15));
#128698=DIRECTION('center_axis',(1.4081690688991E-16,6.98296267768627E-15,
-1.));
#128699=DIRECTION('ref_axis',(-1.,7.98707387273907E-31,-1.4081690688991E-16));
#128700=DIRECTION('',(0.743144825477398,-0.669130606358854,-4.56786669500649E-15));
#128701=DIRECTION('center_axis',(-1.4081690688991E-16,-6.98296267768627E-15,
1.));
#128702=DIRECTION('ref_axis',(-1.,7.99150043815584E-31,-1.4081690688991E-16));
#128703=DIRECTION('center_axis',(-1.4081690688991E-16,-6.98296267768627E-15,
1.));
#128704=DIRECTION('ref_axis',(1.,-7.99370576998456E-31,1.4081690688991E-16));
#128705=DIRECTION('',(-0.404509815527948,0.293899304131707,0.86602252174666));
#128706=DIRECTION('center_axis',(-1.4081690688991E-16,-6.98296267768627E-15,
1.));
#128707=DIRECTION('ref_axis',(-1.,7.99858039355471E-31,-1.4081690688991E-16));
#128708=DIRECTION('center_axis',(-1.4081690688991E-16,-6.98296267768627E-15,
1.));
#128709=DIRECTION('ref_axis',(-1.,7.99858039355471E-31,-1.4081690688991E-16));
#128710=DIRECTION('center_axis',(-1.4081690688991E-16,-6.98296267768627E-15,
1.));
#128711=DIRECTION('ref_axis',(-1.,7.99858039355471E-31,-1.4081690688991E-16));
#128712=DIRECTION('',(0.371579218892551,-0.33456520427975,-0.866022521746664));
#128713=DIRECTION('center_axis',(-1.4081690688991E-16,-6.98296267768627E-15,
1.));
#128714=DIRECTION('ref_axis',(-1.,9.83319205199467E-31,-1.40816906889911E-16));
#128715=DIRECTION('',(-0.80901699437495,0.587785252292469,3.99055920848346E-15));
#128716=DIRECTION('center_axis',(1.4081690688991E-16,6.98296267768627E-15,
-1.));
#128717=DIRECTION('ref_axis',(-1.,8.01265634860448E-31,-1.4081690688991E-16));
#128718=DIRECTION('',(0.743144825477398,-0.669130606358854,-4.56786669500649E-15));
#128719=DIRECTION('center_axis',(-1.4081690688991E-16,-6.98296267768627E-15,
1.));
#128720=DIRECTION('ref_axis',(-1.,8.32577322149061E-31,-1.39145123902276E-16));
#128721=DIRECTION('center_axis',(-0.588650770899369,-0.808387450334138,
-7.86457204757439E-6));
#128722=DIRECTION('ref_axis',(-5.81354223910265E-6,-5.4954167425029E-6,
0.999999999968001));
#128723=DIRECTION('center_axis',(0.668334867928669,0.743860540860259,-7.8645723350969E-6));
#128724=DIRECTION('ref_axis',(0.630829867029799,-0.566774825493072,0.529924500330438));
#128725=DIRECTION('center_axis',(-1.4081690688991E-16,-6.98296267768627E-15,
1.));
#128726=DIRECTION('ref_axis',(-1.,8.07722881720021E-31,-1.42096112075504E-16));
#128727=DIRECTION('center_axis',(-0.588613901400178,-0.808414296622096,
9.77058519236102E-6));
#128728=DIRECTION('ref_axis',(0.707075657763138,-0.514822445315961,0.484769908304672));
#128729=DIRECTION('center_axis',(0.668368793191875,0.743830058677232,9.77050991880942E-6));
#128730=DIRECTION('ref_axis',(0.650587230628311,-0.584591780669575,0.484756336025596));
#128731=DIRECTION('center_axis',(-1.4081690688991E-16,-6.98296267768627E-15,
1.));
#128732=DIRECTION('ref_axis',(-1.,8.24049048117772E-31,-1.37719829560012E-16));
#128733=DIRECTION('center_axis',(0.58568118920789,0.81054151298879,-1.81624800754865E-5));
#128734=DIRECTION('ref_axis',(0.70131153142444,-0.506765009439537,-0.50134953984107));
#128735=DIRECTION('center_axis',(-0.671059256698626,-0.741403718408757,
-1.81316452525126E-5));
#128736=DIRECTION('ref_axis',(0.642789354378864,-0.58178924642884,-0.49834036424613));
#128737=DIRECTION('center_axis',(-1.4081690688991E-16,-6.98296267768627E-15,
1.));
#128738=DIRECTION('ref_axis',(-1.,8.26087817385229E-31,-1.38060560438432E-16));
#128739=DIRECTION('center_axis',(0.585670237127502,0.810549426624303,-1.84940374120092E-5));
#128740=DIRECTION('ref_axis',(0.702737191803893,-0.507758105719546,0.49833938769846));
#128741=DIRECTION('center_axis',(-0.671069274109347,-0.741394651318144,
-1.85257084724781E-5));
#128742=DIRECTION('ref_axis',(0.641482109966384,-0.580646516615919,0.501348506864113));
#128743=DIRECTION('center_axis',(-1.4081690688991E-16,-6.98296267768627E-15,
1.));
#128744=DIRECTION('ref_axis',(-1.,9.83319205199467E-31,-1.40816906889911E-16));
#128745=DIRECTION('center_axis',(-1.4081690688991E-16,-6.98296267768627E-15,
1.));
#128746=DIRECTION('ref_axis',(-1.,8.46073526001725E-31,-1.4081690688991E-16));
#128747=DIRECTION('',(-0.743144825477398,0.669130606358854,4.56786669500649E-15));
#128748=DIRECTION('center_axis',(-1.4081690688991E-16,-6.98296267768627E-15,
1.));
#128749=DIRECTION('ref_axis',(-1.,7.97077743482043E-31,-1.4081690688991E-16));
#128750=DIRECTION('center_axis',(-1.4081690688991E-16,-6.98296267768627E-15,
1.));
#128751=DIRECTION('ref_axis',(-1.,7.97077743482043E-31,-1.4081690688991E-16));
#128752=DIRECTION('center_axis',(-1.4081690688991E-16,-6.98296267768627E-15,
1.));
#128753=DIRECTION('ref_axis',(-1.,7.97077743482043E-31,-1.4081690688991E-16));
#128754=DIRECTION('',(0.669130606358862,-0.743144825477391,-5.09512767813147E-15));
#128755=DIRECTION('center_axis',(1.4081690688991E-16,6.98296267768627E-15,
-1.));
#128756=DIRECTION('ref_axis',(1.,-7.97077743482043E-31,1.4081690688991E-16));
#128757=DIRECTION('',(-0.371579467697567,0.33456522605815,-0.86602240657979));
#128758=DIRECTION('center_axis',(1.4081690688991E-16,6.98296267768627E-15,
-1.));
#128759=DIRECTION('ref_axis',(-1.,8.88178419700126E-16,-1.40816906889904E-16));
#128760=DIRECTION('',(0.334565226058153,-0.371579467697543,0.866022406579799));
#128761=DIRECTION('center_axis',(-1.4081690688991E-16,-6.98296267768627E-15,
1.));
#128762=DIRECTION('ref_axis',(-1.,9.83319205199467E-31,-1.40816906889911E-16));
#128763=DIRECTION('center_axis',(-1.4081690688991E-16,-6.98296267768627E-15,
1.));
#128764=DIRECTION('ref_axis',(-1.,7.98248735348668E-31,-1.4081690688991E-16));
#128765=DIRECTION('',(-0.743144825477398,0.669130606358854,4.56786669500649E-15));
#128766=DIRECTION('center_axis',(1.4081690688991E-16,6.98296267768627E-15,
-1.));
#128767=DIRECTION('ref_axis',(-1.,7.98707387273907E-31,-1.4081690688991E-16));
#128768=DIRECTION('',(0.669130606358862,-0.743144825477391,-5.09512767813147E-15));
#128769=DIRECTION('center_axis',(-1.4081690688991E-16,-6.98296267768627E-15,
1.));
#128770=DIRECTION('ref_axis',(-1.,7.99150043815584E-31,-1.4081690688991E-16));
#128771=DIRECTION('center_axis',(-1.4081690688991E-16,-6.98296267768627E-15,
1.));
#128772=DIRECTION('ref_axis',(1.,-7.99370576998456E-31,1.4081690688991E-16));
#128773=DIRECTION('',(-0.3715730258176,0.334572082386297,0.866022521746663));
#128774=DIRECTION('center_axis',(-1.4081690688991E-16,-6.98296267768627E-15,
1.));
#128775=DIRECTION('ref_axis',(-1.,7.99858039355471E-31,-1.4081690688991E-16));
#128776=DIRECTION('center_axis',(-1.4081690688991E-16,-6.98296267768627E-15,
1.));
#128777=DIRECTION('ref_axis',(-1.,7.99858039355471E-31,-1.4081690688991E-16));
#128778=DIRECTION('center_axis',(-1.4081690688991E-16,-6.98296267768627E-15,
1.));
#128779=DIRECTION('ref_axis',(-1.,7.99858039355471E-31,-1.4081690688991E-16));
#128780=DIRECTION('',(0.334572082386317,-0.37157302581762,-0.866022521746647));
#128781=DIRECTION('center_axis',(-1.4081690688991E-16,-6.98296267768627E-15,
1.));
#128782=DIRECTION('ref_axis',(-1.,9.83319205199467E-31,-1.40816906889911E-16));
#128783=DIRECTION('',(-0.743144825477398,0.669130606358854,4.56786669500649E-15));
#128784=DIRECTION('center_axis',(1.4081690688991E-16,6.98296267768627E-15,
-1.));
#128785=DIRECTION('ref_axis',(-1.,8.88178419700126E-16,-1.40816906889904E-16));
#128786=DIRECTION('',(0.669130606358862,-0.743144825477391,-5.09512767813147E-15));
#128787=DIRECTION('center_axis',(-1.4081690688991E-16,-6.98296267768627E-15,
1.));
#128788=DIRECTION('ref_axis',(-1.,8.32577322149061E-31,-1.39145123902276E-16));
#128789=DIRECTION('center_axis',(-0.669925578293101,-0.742428258814818,
-7.86457203518997E-6));
#128790=DIRECTION('ref_axis',(-6.35612246172978E-6,-4.85763167245441E-6,
0.999999999968002));
#128791=DIRECTION('center_axis',(0.742428258814711,0.66992557829322,-7.86457232381813E-6));
#128792=DIRECTION('ref_axis',(0.568130013485777,-0.629609650280374,0.529924500330449));
#128793=DIRECTION('center_axis',(-1.4081690688991E-16,-6.98296267768627E-15,
1.));
#128794=DIRECTION('ref_axis',(-1.,8.07722881720021E-31,-1.42096112075504E-16));
#128795=DIRECTION('center_axis',(-0.669891716968524,-0.742458811949524,
9.77058138072136E-6));
#128796=DIRECTION('ref_axis',(0.649388624263403,-0.585911726014202,0.484769908303252));
#128797=DIRECTION('center_axis',(0.742458811977019,0.669891716938052,9.77050718766635E-6));
#128798=DIRECTION('ref_axis',(0.585916765234264,-0.649394209167008,0.484756336026434));
#128799=DIRECTION('center_axis',(-1.4081690688991E-16,-6.98296267768627E-15,
1.));
#128800=DIRECTION('ref_axis',(-1.,8.24049048117772E-31,-1.37719829560012E-16));
#128801=DIRECTION('center_axis',(0.667197425140074,0.744880927099479,-1.8162479743951E-5));
#128802=DIRECTION('ref_axis',(0.644498305799933,-0.57729591434456,-0.501349539844304));
#128803=DIRECTION('center_axis',(-0.744880915222522,-0.667197438400734,
-1.81316451348809E-5));
#128804=DIRECTION('ref_axis',(0.578454551160941,-0.645791927477339,-0.498340364255494));
#128805=DIRECTION('center_axis',(-1.4081690688991E-16,-6.98296267768627E-15,
1.));
#128806=DIRECTION('ref_axis',(-1.,8.26087817385229E-31,-1.38060560438432E-16));
#128807=DIRECTION('center_axis',(0.667187360262395,0.74488994218211,-1.84940515154987E-5));
#128808=DIRECTION('ref_axis',(0.645812349436813,-0.578432592429817,0.498339387696602));
#128809=DIRECTION('center_axis',(-0.744889929984709,-0.667187373879462,
-1.85257164452763E-5));
#128810=DIRECTION('ref_axis',(0.577273915766496,-0.644518813413982,0.501348506860296));
#128811=DIRECTION('center_axis',(-1.4081690688991E-16,-6.98296267768627E-15,
1.));
#128812=DIRECTION('ref_axis',(-1.,9.83319205199467E-31,-1.40816906889911E-16));
#128813=DIRECTION('center_axis',(-1.4081690688991E-16,-6.98296267768627E-15,
1.));
#128814=DIRECTION('ref_axis',(-1.,8.46073526001725E-31,-1.4081690688991E-16));
#128815=DIRECTION('',(-0.669130606358862,0.743144825477391,5.09512767813147E-15));
#128816=DIRECTION('center_axis',(-1.4081690688991E-16,-6.98296267768627E-15,
1.));
#128817=DIRECTION('ref_axis',(-1.,7.97077743482043E-31,-1.4081690688991E-16));
#128818=DIRECTION('center_axis',(-1.4081690688991E-16,-6.98296267768627E-15,
1.));
#128819=DIRECTION('ref_axis',(-1.,7.97077743482043E-31,-1.4081690688991E-16));
#128820=DIRECTION('center_axis',(-1.4081690688991E-16,-6.98296267768627E-15,
1.));
#128821=DIRECTION('ref_axis',(-1.,7.97077743482043E-31,-1.4081690688991E-16));
#128822=DIRECTION('',(0.587785252292477,-0.809016994374945,-5.56656537619083E-15));
#128823=DIRECTION('center_axis',(1.4081690688991E-16,6.98296267768627E-15,
-1.));
#128824=DIRECTION('ref_axis',(1.,-7.97077743482043E-31,1.4081690688991E-16));
#128825=DIRECTION('',(-0.334572327551839,0.371573073483901,-0.866022406579803));
#128826=DIRECTION('center_axis',(1.4081690688991E-16,6.98296267768627E-15,
-1.));
#128827=DIRECTION('ref_axis',(-1.,8.88178419700126E-16,-1.40816906889904E-16));
#128828=DIRECTION('',(0.293891812003449,-0.404515505437191,0.866022406579774));
#128829=DIRECTION('center_axis',(-1.4081690688991E-16,-6.98296267768627E-15,
1.));
#128830=DIRECTION('ref_axis',(-1.,9.83319205199467E-31,-1.40816906889911E-16));
#128831=DIRECTION('center_axis',(-1.4081690688991E-16,-6.98296267768627E-15,
1.));
#128832=DIRECTION('ref_axis',(-1.,7.98248735348668E-31,-1.4081690688991E-16));
#128833=DIRECTION('',(-0.669130606358862,0.743144825477391,5.09512767813147E-15));
#128834=DIRECTION('center_axis',(1.4081690688991E-16,6.98296267768627E-15,
-1.));
#128835=DIRECTION('ref_axis',(-1.,7.98707387273907E-31,-1.4081690688991E-16));
#128836=DIRECTION('',(0.587785252292477,-0.809016994374945,-5.56656537619083E-15));
#128837=DIRECTION('center_axis',(-1.4081690688991E-16,-6.98296267768627E-15,
1.));
#128838=DIRECTION('ref_axis',(-1.,7.99150043815584E-31,-1.4081690688991E-16));
#128839=DIRECTION('center_axis',(-1.4081690688991E-16,-6.98296267768627E-15,
1.));
#128840=DIRECTION('ref_axis',(1.,-1.06581410364015E-14,1.40816906889836E-16));
#128841=DIRECTION('',(-0.334565204279747,0.371579218892574,0.866022521746655));
#128842=DIRECTION('center_axis',(-1.4081690688991E-16,-6.98296267768627E-15,
1.));
#128843=DIRECTION('ref_axis',(-1.,7.99858039355471E-31,-1.4081690688991E-16));
#128844=DIRECTION('center_axis',(-1.4081690688991E-16,-6.98296267768627E-15,
1.));
#128845=DIRECTION('ref_axis',(-1.,7.99858039355471E-31,-1.4081690688991E-16));
#128846=DIRECTION('center_axis',(-1.4081690688991E-16,-6.98296267768627E-15,
1.));
#128847=DIRECTION('ref_axis',(-1.,7.99858039355471E-31,-1.4081690688991E-16));
#128848=DIRECTION('',(0.293899304131692,-0.404509815527973,-0.866022521746654));
#128849=DIRECTION('center_axis',(-1.4081690688991E-16,-6.98296267768627E-15,
1.));
#128850=DIRECTION('ref_axis',(-1.,9.83319205199467E-31,-1.40816906889911E-16));
#128851=DIRECTION('',(-0.669130606358862,0.743144825477391,5.09512767813147E-15));
#128852=DIRECTION('center_axis',(1.4081690688991E-16,6.98296267768627E-15,
-1.));
#128853=DIRECTION('ref_axis',(-1.,8.01265634860448E-31,-1.4081690688991E-16));
#128854=DIRECTION('',(0.587785252292477,-0.809016994374945,-5.56656537619083E-15));
#128855=DIRECTION('center_axis',(-1.4081690688991E-16,-6.98296267768627E-15,
1.));
#128856=DIRECTION('ref_axis',(-1.,8.32577322149061E-31,-1.39145123902276E-16));
#128857=DIRECTION('center_axis',(-0.743860540860149,-0.668334867928791,
-7.86457203541079E-6));
#128858=DIRECTION('ref_axis',(-6.82906373999688E-6,-4.16662532737549E-6,
0.999999999968002));
#128859=DIRECTION('center_axis',(0.808387450334027,0.588650770899521,-7.86457235190628E-6));
#128860=DIRECTION('ref_axis',(0.499205608625243,-0.685546339984863,0.529924500330433));
#128861=DIRECTION('center_axis',(-1.4081690688991E-16,-6.98296267768627E-15,
1.));
#128862=DIRECTION('ref_axis',(-1.,8.07722881720021E-31,-1.42096112075504E-16));
#128863=DIRECTION('center_axis',(-0.74383005870373,-0.668368793162384,9.77058148516564E-6));
#128864=DIRECTION('ref_axis',(0.584586753102489,-0.6505816352322,0.484769908302574));
#128865=DIRECTION('center_axis',(0.808414296646392,0.58861390136681,9.7705106400194E-6));
#128866=DIRECTION('ref_axis',(0.514826873149565,-0.707081738814457,0.48475633602684));
#128867=DIRECTION('center_axis',(-1.4081690688991E-16,-6.98296267768627E-15,
1.));
#128868=DIRECTION('ref_axis',(-1.,8.24049048117772E-31,-1.37719829560012E-16));
#128869=DIRECTION('center_axis',(0.74140370646244,0.671059269896393,-1.81624792922045E-5));
#128870=DIRECTION('ref_axis',(0.580623821868732,-0.641501844406329,-0.501349539844034));
#128871=DIRECTION('center_axis',(-0.810541502562932,-0.585681203637498,
-1.81316452566355E-5));
#128872=DIRECTION('ref_axis',(0.507782078837387,-0.702719177034441,-0.498340364248792));
#128873=DIRECTION('center_axis',(-1.4081690688991E-16,-6.98296267768627E-15,
1.));
#128874=DIRECTION('ref_axis',(-1.,8.26087817385229E-31,-1.38060560438432E-16));
#128875=DIRECTION('center_axis',(0.74139463906873,0.671069287643322,-1.84940903563101E-5));
#128876=DIRECTION('ref_axis',(0.581811851822687,-0.642769650611083,0.498339387698746));
#128877=DIRECTION('center_axis',(-0.810549415911435,-0.585670251952778,
-1.85257190592093E-5));
#128878=DIRECTION('ref_axis',(0.506740987740971,-0.701329627215785,0.501348506861918));
#128879=DIRECTION('center_axis',(-1.4081690688991E-16,-6.98296267768627E-15,
1.));
#128880=DIRECTION('ref_axis',(-1.,9.83319205199467E-31,-1.40816906889911E-16));
#128881=DIRECTION('center_axis',(-1.4081690688991E-16,-6.98296267768627E-15,
1.));
#128882=DIRECTION('ref_axis',(-1.,8.46073526001725E-31,-1.4081690688991E-16));
#128883=DIRECTION('',(-0.587785252292477,0.809016994374945,5.56656537619083E-15));
#128884=DIRECTION('center_axis',(-1.4081690688991E-16,-6.98296267768627E-15,
1.));
#128885=DIRECTION('ref_axis',(-1.,7.97077743482043E-31,-1.4081690688991E-16));
#128886=DIRECTION('center_axis',(-1.4081690688991E-16,-6.98296267768627E-15,
1.));
#128887=DIRECTION('ref_axis',(-1.,7.97077743482043E-31,-1.4081690688991E-16));
#128888=DIRECTION('center_axis',(-1.4081690688991E-16,-6.98296267768627E-15,
1.));
#128889=DIRECTION('ref_axis',(-1.,7.97077743482043E-31,-1.4081690688991E-16));
#128890=DIRECTION('',(0.500000000000004,-0.866025403784436,-5.97701461910994E-15));
#128891=DIRECTION('center_axis',(1.4081690688991E-16,6.98296267768627E-15,
-1.));
#128892=DIRECTION('ref_axis',(1.,-7.97077743482043E-31,1.4081690688991E-16));
#128893=DIRECTION('',(-0.293899542971751,0.404509888559909,-0.866022406579787));
#128894=DIRECTION('center_axis',(1.4081690688991E-16,6.98296267768627E-15,
-1.));
#128895=DIRECTION('ref_axis',(-1.,7.97577417048809E-31,-1.40816906889911E-16));
#128896=DIRECTION('',(0.24999845775561,-0.433019586648882,0.866022406579788));
#128897=DIRECTION('center_axis',(-1.4081690688991E-16,-6.98296267768627E-15,
1.));
#128898=DIRECTION('ref_axis',(-1.,9.83319205199467E-31,-1.40816906889911E-16));
#128899=DIRECTION('center_axis',(-1.4081690688991E-16,-6.98296267768627E-15,
1.));
#128900=DIRECTION('ref_axis',(-1.,7.98248735348668E-31,-1.4081690688991E-16));
#128901=DIRECTION('',(-0.587785252292477,0.809016994374945,5.56656537619083E-15));
#128902=DIRECTION('center_axis',(1.4081690688991E-16,6.98296267768627E-15,
-1.));
#128903=DIRECTION('ref_axis',(-1.,-1.77635683940025E-15,-1.40816906889923E-16));
#128904=DIRECTION('',(0.500000000000004,-0.866025403784436,-5.97701461910994E-15));
#128905=DIRECTION('center_axis',(-1.4081690688991E-16,-6.98296267768627E-15,
1.));
#128906=DIRECTION('ref_axis',(-1.,7.99150043815584E-31,-1.4081690688991E-16));
#128907=DIRECTION('center_axis',(-1.4081690688991E-16,-6.98296267768627E-15,
1.));
#128908=DIRECTION('ref_axis',(1.,-1.06581410364015E-14,1.40816906889836E-16));
#128909=DIRECTION('',(-0.293891816351504,0.40451525571866,0.866022521746681));
#128910=DIRECTION('center_axis',(-1.4081690688991E-16,-6.98296267768627E-15,
1.));
#128911=DIRECTION('ref_axis',(-1.,7.99858039355471E-31,-1.4081690688991E-16));
#128912=DIRECTION('center_axis',(-1.4081690688991E-16,-6.98296267768627E-15,
1.));
#128913=DIRECTION('ref_axis',(-1.,7.99858039355471E-31,-1.4081690688991E-16));
#128914=DIRECTION('center_axis',(-1.4081690688991E-16,-6.98296267768627E-15,
1.));
#128915=DIRECTION('ref_axis',(-1.,7.99858039355471E-31,-1.4081690688991E-16));
#128916=DIRECTION('',(0.250006503598675,-0.43301471105021,-0.866022521746674));
#128917=DIRECTION('center_axis',(-1.4081690688991E-16,-6.98296267768627E-15,
1.));
#128918=DIRECTION('ref_axis',(-1.,9.83319205199467E-31,-1.40816906889911E-16));
#128919=DIRECTION('',(-0.587785252292477,0.809016994374945,5.56656537619083E-15));
#128920=DIRECTION('center_axis',(1.4081690688991E-16,6.98296267768627E-15,
-1.));
#128921=DIRECTION('ref_axis',(-1.,8.01265634860448E-31,-1.4081690688991E-16));
#128922=DIRECTION('',(0.500000000000004,-0.866025403784436,-5.97701461910994E-15));
#128923=DIRECTION('center_axis',(-1.4081690688991E-16,-6.98296267768627E-15,
1.));
#128924=DIRECTION('ref_axis',(-1.,8.32577322149061E-31,-1.39145123902276E-16));
#128925=DIRECTION('center_axis',(-0.809645611678698,-0.58691906037168,-7.86457201904425E-6));
#128926=DIRECTION('ref_axis',(-7.22718433787083E-6,-3.42996857467424E-6,
0.999999999968002));
#128927=DIRECTION('center_axis',(0.865489779781569,0.500926582476713,-7.86457233244357E-6));
#128928=DIRECTION('ref_axis',(0.424811802651058,-0.73397204052872,0.529924500330439));
#128929=DIRECTION('center_axis',(-1.4081690688991E-16,-6.98296267768627E-15,
1.));
#128930=DIRECTION('ref_axis',(-1.,8.07722881720021E-31,-1.42096112075504E-16));
#128931=DIRECTION('center_axis',(-0.809618842664134,-0.58695598600553,9.77059657011212E-6));
#128932=DIRECTION('ref_axis',(0.513380027140978,-0.708123635910311,0.484769908304848));
#128933=DIRECTION('center_axis',(0.86551262510965,0.50088710871846,9.77051708363798E-6));
#128934=DIRECTION('ref_axis',(0.438096430108474,-0.757022332965543,0.484756336026273));
#128935=DIRECTION('center_axis',(-1.4081690688991E-16,-6.98296267768627E-15,
1.));
#128936=DIRECTION('ref_axis',(-1.,8.24049048117772E-31,-1.37719829560012E-16));
#128937=DIRECTION('center_axis',(0.807487013627704,0.58988534690458,-1.81624797733012E-5));
#128938=DIRECTION('ref_axis',(0.51038790184082,-0.698679346016538,-0.50134953984663));
#128939=DIRECTION('center_axis',(-0.867321627584508,-0.497748123045586,
-1.81316451898425E-5));
#128940=DIRECTION('ref_axis',(0.431546239795072,-0.751947288231341,-0.498340364249442));
#128941=DIRECTION('center_axis',(-1.4081690688991E-16,-6.98296267768627E-15,
1.));
#128942=DIRECTION('ref_axis',(-1.,8.26087817385229E-31,-1.38060560438432E-16));
#128943=DIRECTION('center_axis',(0.807479043032716,0.589896257591909,-1.84940513261902E-5));
#128944=DIRECTION('ref_axis',(0.511436901809379,-0.700064389993352,0.498339387697642));
#128945=DIRECTION('center_axis',(-0.867328352822391,-0.497736404181166,
-1.85257110601528E-5));
#128946=DIRECTION('ref_axis',(0.430656099412309,-0.750456526860381,0.501348506860876));
#128947=DIRECTION('center_axis',(-1.4081690688991E-16,-6.98296267768627E-15,
1.));
#128948=DIRECTION('ref_axis',(-1.,9.83319205199467E-31,-1.40816906889911E-16));
#128949=DIRECTION('center_axis',(-1.4081690688991E-16,-6.98296267768627E-15,
1.));
#128950=DIRECTION('ref_axis',(-1.,8.46073526001725E-31,-1.4081690688991E-16));
#128951=DIRECTION('',(-0.500000000000004,0.866025403784436,5.97701461910994E-15));
#128952=DIRECTION('center_axis',(-1.4081690688991E-16,-6.98296267768627E-15,
1.));
#128953=DIRECTION('ref_axis',(-1.,7.97077743482043E-31,-1.4081690688991E-16));
#128954=DIRECTION('center_axis',(-1.4081690688991E-16,-6.98296267768627E-15,
1.));
#128955=DIRECTION('ref_axis',(-1.,7.97077743482043E-31,-1.4081690688991E-16));
#128956=DIRECTION('center_axis',(-1.4081690688991E-16,-6.98296267768627E-15,
1.));
#128957=DIRECTION('ref_axis',(-1.,7.97077743482043E-31,-1.4081690688991E-16));
#128958=DIRECTION('',(0.406736643075804,-0.913545457642599,-6.32197843909137E-15));
#128959=DIRECTION('center_axis',(1.4081690688991E-16,6.98296267768627E-15,
-1.));
#128960=DIRECTION('ref_axis',(1.,-7.97077743482043E-31,1.4081690688991E-16));
#128961=DIRECTION('',(-0.250006733496394,0.433014808647735,-0.866022406579777));
#128962=DIRECTION('center_axis',(1.4081690688991E-16,6.98296267768627E-15,
-1.));
#128963=DIRECTION('ref_axis',(-1.,7.97577417048809E-31,-1.40816906889911E-16));
#128964=DIRECTION('',(0.203366068089048,-0.456779414654134,0.866022406579776));
#128965=DIRECTION('center_axis',(-1.4081690688991E-16,-6.98296267768627E-15,
1.));
#128966=DIRECTION('ref_axis',(-1.,9.83319205199467E-31,-1.40816906889911E-16));
#128967=DIRECTION('center_axis',(-1.4081690688991E-16,-6.98296267768627E-15,
1.));
#128968=DIRECTION('ref_axis',(-1.,7.98248735348668E-31,-1.4081690688991E-16));
#128969=DIRECTION('',(-0.500000000000004,0.866025403784436,5.97701461910994E-15));
#128970=DIRECTION('center_axis',(1.4081690688991E-16,6.98296267768627E-15,
-1.));
#128971=DIRECTION('ref_axis',(-1.,7.98707387273907E-31,-1.4081690688991E-16));
#128972=DIRECTION('',(0.406736643075804,-0.913545457642599,-6.32197843909137E-15));
#128973=DIRECTION('center_axis',(-1.4081690688991E-16,-6.98296267768627E-15,
1.));
#128974=DIRECTION('ref_axis',(-1.,7.99150043815584E-31,-1.4081690688991E-16));
#128975=DIRECTION('center_axis',(-1.4081690688991E-16,-6.98296267768627E-15,
1.));
#128976=DIRECTION('ref_axis',(1.,4.44089209850062E-15,1.40816906889941E-16));
#128977=DIRECTION('',(-0.249998488182552,0.433019338752927,0.866022521746644));
#128978=DIRECTION('center_axis',(-1.4081690688991E-16,-6.98296267768627E-15,
1.));
#128979=DIRECTION('ref_axis',(-1.,7.99858039355471E-31,-1.4081690688991E-16));
#128980=DIRECTION('center_axis',(-1.4081690688991E-16,-6.98296267768627E-15,
1.));
#128981=DIRECTION('ref_axis',(-1.,7.99858039355471E-31,-1.4081690688991E-16));
#128982=DIRECTION('center_axis',(-1.4081690688991E-16,-6.98296267768627E-15,
1.));
#128983=DIRECTION('ref_axis',(-1.,7.99858039355471E-31,-1.4081690688991E-16));
#128984=DIRECTION('',(0.203374579494966,-0.456775406784111,-0.866022521746666));
#128985=DIRECTION('center_axis',(-1.4081690688991E-16,-6.98296267768627E-15,
1.));
#128986=DIRECTION('ref_axis',(-1.,9.83319205199467E-31,-1.40816906889911E-16));
#128987=DIRECTION('',(-0.500000000000004,0.866025403784436,5.97701461910994E-15));
#128988=DIRECTION('center_axis',(1.4081690688991E-16,6.98296267768627E-15,
-1.));
#128989=DIRECTION('ref_axis',(-1.,8.01265634860448E-31,-1.4081690688991E-16));
#128990=DIRECTION('',(0.406736643075804,-0.913545457642599,-6.32197843909137E-15));
#128991=DIRECTION('center_axis',(-1.4081690688991E-16,-6.98296267768627E-15,
1.));
#128992=DIRECTION('ref_axis',(-1.,8.32577322149061E-31,-1.39145123902276E-16));
#128993=DIRECTION('center_axis',(-0.866560035746415,-0.499072844768497,
-7.86457190912175E-6));
#128994=DIRECTION('ref_axis',(-7.54612232684255E-6,-2.65573230665248E-6,
0.999999999968002));
#128995=DIRECTION('center_axis',(0.913109622086441,0.407714137590671,-7.86457235765693E-6));
#128996=DIRECTION('ref_axis',(0.345763669669472,-0.774356189803008,0.529924500330442));
#128997=DIRECTION('center_axis',(-1.4081690688991E-16,-6.98296267768627E-15,
1.));
#128998=DIRECTION('ref_axis',(-1.,8.07722881720021E-31,-1.42096112075504E-16));
#128999=DIRECTION('center_axis',(-0.86653727315328,-0.499112366246934,9.77058997059964E-6));
#129000=DIRECTION('ref_axis',(0.436548602172256,-0.757907285851671,0.484769908301251));
#129001=DIRECTION('center_axis',(0.913128216134695,0.407672492085507,9.77051465153252E-6));
#129002=DIRECTION('ref_axis',(0.356566110901248,-0.798668832019048,0.48475633602676));
#129003=DIRECTION('center_axis',(-1.4081690688991E-16,-6.98296267768627E-15,
1.));
#129004=DIRECTION('ref_axis',(-1.,8.24049048117772E-31,-1.37719829560012E-16));
#129005=DIRECTION('center_axis',(0.864723324094334,0.502248516610423,-1.81624797431789E-5));
#129006=DIRECTION('ref_axis',(0.434560065157393,-0.748201970507551,-0.501349539841237));
#129007=DIRECTION('center_axis',(-0.914599195355563,-0.404361609857069,
-1.81316451872637E-5));
#129008=DIRECTION('ref_axis',(0.350582289842822,-0.792936907583349,-0.498340364249896));
#129009=DIRECTION('center_axis',(-1.4081690688991E-16,-6.98296267768627E-15,
1.));
#129010=DIRECTION('ref_axis',(-1.,8.26087817385229E-31,-1.38060560438432E-16));
#129011=DIRECTION('center_axis',(0.864716537642879,0.502260200677778,-1.84940595705526E-5));
#129012=DIRECTION('ref_axis',(0.435458542074697,-0.74968907742123,0.498339387696262));
#129013=DIRECTION('center_axis',(-0.914604658795487,-0.404349252214455,
-1.85257175418162E-5));
#129014=DIRECTION('ref_axis',(0.34985285273649,-0.791361267750787,0.501348506865241));
#129015=DIRECTION('center_axis',(-1.4081690688991E-16,-6.98296267768627E-15,
1.));
#129016=DIRECTION('ref_axis',(-1.,9.83319205199467E-31,-1.40816906889911E-16));
#129017=DIRECTION('center_axis',(-1.4081690688991E-16,-6.98296267768627E-15,
1.));
#129018=DIRECTION('ref_axis',(-1.,8.46073526001725E-31,-1.4081690688991E-16));
#129019=DIRECTION('',(-0.406736643075804,0.913545457642599,6.32197843909137E-15));
#129020=DIRECTION('center_axis',(-1.4081690688991E-16,-6.98296267768627E-15,
1.));
#129021=DIRECTION('ref_axis',(-1.,7.97077743482043E-31,-1.4081690688991E-16));
#129022=DIRECTION('center_axis',(-1.4081690688991E-16,-6.98296267768627E-15,
1.));
#129023=DIRECTION('ref_axis',(-1.,7.97077743482043E-31,-1.4081690688991E-16));
#129024=DIRECTION('center_axis',(-1.4081690688991E-16,-6.98296267768627E-15,
1.));
#129025=DIRECTION('ref_axis',(-1.,7.97077743482043E-31,-1.4081690688991E-16));
#129026=DIRECTION('',(0.309016994374951,-0.951056516295152,-6.59767734033507E-15));
#129027=DIRECTION('center_axis',(1.4081690688991E-16,6.98296267768627E-15,
-1.));
#129028=DIRECTION('ref_axis',(1.,-7.97077743482043E-31,1.4081690688991E-16));
#129029=DIRECTION('',(-0.203374797931581,0.456775527877827,-0.866022406579773));
#129030=DIRECTION('center_axis',(1.4081690688991E-16,6.98296267768627E-15,
-1.));
#129031=DIRECTION('ref_axis',(-1.,7.97577417048809E-31,-1.40816906889911E-16));
#129032=DIRECTION('',(0.154505557223423,-0.475534671805169,0.866022406579778));
#129033=DIRECTION('center_axis',(-1.4081690688991E-16,-6.98296267768627E-15,
1.));
#129034=DIRECTION('ref_axis',(-1.,9.83319205199467E-31,-1.40816906889911E-16));
#129035=DIRECTION('center_axis',(-1.4081690688991E-16,-6.98296267768627E-15,
1.));
#129036=DIRECTION('ref_axis',(-1.,7.98248735348668E-31,-1.4081690688991E-16));
#129037=DIRECTION('',(-0.406736643075804,0.913545457642599,6.32197843909137E-15));
#129038=DIRECTION('center_axis',(1.4081690688991E-16,6.98296267768627E-15,
-1.));
#129039=DIRECTION('ref_axis',(-1.,7.98707387273907E-31,-1.4081690688991E-16));
#129040=DIRECTION('',(0.309016994374951,-0.951056516295152,-6.59767734033507E-15));
#129041=DIRECTION('center_axis',(-1.4081690688991E-16,-6.98296267768627E-15,
1.));
#129042=DIRECTION('ref_axis',(-1.,7.99150043815584E-31,-1.4081690688991E-16));
#129043=DIRECTION('center_axis',(-1.4081690688991E-16,-6.98296267768627E-15,
1.));
#129044=DIRECTION('ref_axis',(1.,-7.99370576998456E-31,1.4081690688991E-16));
#129045=DIRECTION('',(-0.203366124261499,0.456779171296629,0.866022521746647));
#129046=DIRECTION('center_axis',(-1.4081690688991E-16,-6.98296267768627E-15,
1.));
#129047=DIRECTION('ref_axis',(-1.,7.99858039355471E-31,-1.4081690688991E-16));
#129048=DIRECTION('center_axis',(-1.4081690688991E-16,-6.98296267768627E-15,
1.));
#129049=DIRECTION('ref_axis',(-1.,7.99858039355471E-31,-1.4081690688991E-16));
#129050=DIRECTION('center_axis',(-1.4081690688991E-16,-6.98296267768627E-15,
1.));
#129051=DIRECTION('ref_axis',(-1.,7.99858039355471E-31,-1.4081690688991E-16));
#129052=DIRECTION('',(0.154514440939472,-0.475531575574881,-0.866022521746654));
#129053=DIRECTION('center_axis',(-1.4081690688991E-16,-6.98296267768627E-15,
1.));
#129054=DIRECTION('ref_axis',(-1.,9.83319205199467E-31,-1.40816906889911E-16));
#129055=DIRECTION('',(-0.406736643075804,0.913545457642599,6.32197843909137E-15));
#129056=DIRECTION('center_axis',(1.4081690688991E-16,6.98296267768627E-15,
-1.));
#129057=DIRECTION('ref_axis',(-1.,8.01265634860448E-31,-1.4081690688991E-16));
#129058=DIRECTION('',(0.309016994374951,-0.951056516295152,-6.59767734033507E-15));
#129059=DIRECTION('center_axis',(-1.4081690688991E-16,-6.98296267768627E-15,
1.));
#129060=DIRECTION('ref_axis',(-1.,8.32577322149061E-31,-1.39145123902276E-16));
#129061=DIRECTION('center_axis',(-0.913980246723226,-0.405758682640185,
-7.86457207997714E-6));
#129062=DIRECTION('ref_axis',(-7.78238363794176E-6,-1.85239945587372E-6,
0.999999999968002));
#129063=DIRECTION('center_axis',(0.950725244291261,0.310034691293523,-7.86457239813168E-6));
#129064=DIRECTION('ref_axis',(0.262927277567293,-0.806256330617357,0.529924500330459));
#129065=DIRECTION('center_axis',(-1.4081690688991E-16,-6.98296267768627E-15,
1.));
#129066=DIRECTION('ref_axis',(-1.,8.07722881720021E-31,-1.42096112075504E-16));
#129067=DIRECTION('center_axis',(-0.913961739946,-0.405800366953278,9.77059292800127E-6));
#129068=DIRECTION('ref_axis',(0.354934259362583,-0.799387144963777,0.484769908304337));
#129069=DIRECTION('center_axis',(0.950739383338137,0.309991330321278,9.77051800362196E-6));
#129070=DIRECTION('ref_axis',(0.271129178767072,-0.831564948217509,0.484756336025744));
#129071=DIRECTION('center_axis',(-1.4081690688991E-16,-6.98296267768627E-15,
1.));
#129072=DIRECTION('ref_axis',(-1.,8.24049048117772E-31,-1.37719829560012E-16));
#129073=DIRECTION('center_axis',(0.912485544867181,0.409108946466059,-1.81624797516694E-5));
#129074=DIRECTION('ref_axis',(0.353971097460658,-0.789527137635661,-0.501349539841553));
#129075=DIRECTION('center_axis',(-0.951856222950087,-0.306544826252928,
-1.81316451597188E-5));
#129076=DIRECTION('ref_axis',(0.265777286958649,-0.825238944241719,-0.498340364252901));
#129077=DIRECTION('center_axis',(-1.4081690688991E-16,-6.98296267768627E-15,
1.));
#129078=DIRECTION('ref_axis',(-1.,8.26087817385229E-31,-1.38060560438432E-16));
#129079=DIRECTION('center_axis',(0.912480016913784,0.409121275896266,-1.84940747170214E-5));
#129080=DIRECTION('ref_axis',(0.354709207427226,-0.791100014434018,0.49833938769562));
#129081=DIRECTION('center_axis',(-0.951860364736425,-0.306531965218374,
-1.85257114665936E-5));
#129082=DIRECTION('ref_axis',(0.265216544996837,-0.823595688993655,0.501348506860256));
#129083=DIRECTION('center_axis',(-1.4081690688991E-16,-6.98296267768627E-15,
1.));
#129084=DIRECTION('ref_axis',(-1.,9.83319205199467E-31,-1.40816906889911E-16));
#129085=DIRECTION('center_axis',(-1.4081690688991E-16,-6.98296267768627E-15,
1.));
#129086=DIRECTION('ref_axis',(-1.,8.46073526001725E-31,-1.4081690688991E-16));
#129087=DIRECTION('',(-0.309016994374951,0.951056516295152,6.59767734033507E-15));
#129088=DIRECTION('center_axis',(-1.4081690688991E-16,-6.98296267768627E-15,
1.));
#129089=DIRECTION('ref_axis',(-1.,7.97077743482043E-31,-1.4081690688991E-16));
#129090=DIRECTION('center_axis',(-1.4081690688991E-16,-6.98296267768627E-15,
1.));
#129091=DIRECTION('ref_axis',(-1.,7.97077743482043E-31,-1.4081690688991E-16));
#129092=DIRECTION('center_axis',(-1.4081690688991E-16,-6.98296267768627E-15,
1.));
#129093=DIRECTION('ref_axis',(-1.,7.97077743482043E-31,-1.4081690688991E-16));
#129094=DIRECTION('',(0.207911690817763,-0.978147600733805,-6.80109070798532E-15));
#129095=DIRECTION('center_axis',(1.4081690688991E-16,6.98296267768627E-15,
-1.));
#129096=DIRECTION('ref_axis',(1.,-7.97077743482043E-31,1.4081690688991E-16));
#129097=DIRECTION('',(-0.15451464552171,0.475531718838027,-0.86602240657979));
#129098=DIRECTION('center_axis',(1.4081690688991E-16,6.98296267768627E-15,
-1.));
#129099=DIRECTION('ref_axis',(-1.,7.97577417048809E-31,-1.40816906889911E-16));
#129100=DIRECTION('',(0.103952251140481,-0.489079871579877,0.866022406579782));
#129101=DIRECTION('center_axis',(-1.4081690688991E-16,-6.98296267768627E-15,
1.));
#129102=DIRECTION('ref_axis',(-1.,9.83319205199467E-31,-1.40816906889911E-16));
#129103=DIRECTION('center_axis',(-1.4081690688991E-16,-6.98296267768627E-15,
1.));
#129104=DIRECTION('ref_axis',(-1.,7.98248735348668E-31,-1.4081690688991E-16));
#129105=DIRECTION('',(-0.309016994374951,0.951056516295152,6.59767734033507E-15));
#129106=DIRECTION('center_axis',(1.4081690688991E-16,6.98296267768627E-15,
-1.));
#129107=DIRECTION('ref_axis',(-1.,7.98707387273907E-31,-1.4081690688991E-16));
#129108=DIRECTION('',(0.207911690817763,-0.978147600733805,-6.80109070798532E-15));
#129109=DIRECTION('center_axis',(-1.4081690688991E-16,-6.98296267768627E-15,
1.));
#129110=DIRECTION('ref_axis',(-1.,7.99150043815584E-31,-1.4081690688991E-16));
#129111=DIRECTION('center_axis',(-1.4081690688991E-16,-6.98296267768627E-15,
1.));
#129112=DIRECTION('ref_axis',(1.,-7.99370576998456E-31,1.4081690688991E-16));
#129113=DIRECTION('',(-0.15450563852595,0.475534435652397,0.86602252174666));
#129114=DIRECTION('center_axis',(-1.4081690688991E-16,-6.98296267768627E-15,
1.));
#129115=DIRECTION('ref_axis',(-1.,7.99858039355471E-31,-1.4081690688991E-16));
#129116=DIRECTION('center_axis',(-1.4081690688991E-16,-6.98296267768627E-15,
1.));
#129117=DIRECTION('ref_axis',(-1.,7.99858039355471E-31,-1.4081690688991E-16));
#129118=DIRECTION('center_axis',(-1.4081690688991E-16,-6.98296267768627E-15,
1.));
#129119=DIRECTION('ref_axis',(-1.,7.99858039355471E-31,-1.4081690688991E-16));
#129120=DIRECTION('',(0.103961409834821,-0.489077720912281,-0.866022521746637));
#129121=DIRECTION('center_axis',(-1.4081690688991E-16,-6.98296267768627E-15,
1.));
#129122=DIRECTION('ref_axis',(-1.,9.83319205199467E-31,-1.40816906889911E-16));
#129123=DIRECTION('',(-0.309016994374951,0.951056516295152,6.59767734033507E-15));
#129124=DIRECTION('center_axis',(1.4081690688991E-16,6.98296267768627E-15,
-1.));
#129125=DIRECTION('ref_axis',(-1.,8.01265634860448E-31,-1.4081690688991E-16));
#129126=DIRECTION('',(0.207911690817763,-0.978147600733805,-6.80109070798532E-15));
#129127=DIRECTION('center_axis',(-1.4081690688991E-16,-6.98296267768627E-15,
1.));
#129128=DIRECTION('ref_axis',(-1.,8.32577322149061E-31,-1.39145123902276E-16));
#129129=DIRECTION('center_axis',(-0.95138669885423,-0.307998943474485,-7.8645720778757E-6));
#129130=DIRECTION('ref_axis',(-7.93337939628674E-6,-1.02877119897231E-6,
0.999999999968002));
#129131=DIRECTION('center_axis',(0.977924521767604,0.208958440039522,-7.86457220880847E-6));
#129132=DIRECTION('ref_axis',(0.177210199190816,-0.829322958353561,0.529924500330424));
#129133=DIRECTION('center_axis',(-1.4081690688991E-16,-6.98296267768627E-15,
1.));
#129134=DIRECTION('ref_axis',(-1.,8.07722881720021E-31,-1.42096112075504E-16));
#129135=DIRECTION('center_axis',(-0.951372650655529,-0.308042333923779,
9.77058867857651E-6));
#129136=DIRECTION('ref_axis',(0.269431182533647,-0.832108751235263,0.484769908303116));
#129137=DIRECTION('center_axis',(0.977934050903442,0.208913838670687,9.77051839951797E-6));
#129138=DIRECTION('ref_axis',(0.182721698612432,-0.855350264825644,0.484756336027584));
#129139=DIRECTION('center_axis',(-1.4081690688991E-16,-6.98296267768627E-15,
1.));
#129140=DIRECTION('ref_axis',(-1.,8.24049048117772E-31,-1.37719829560012E-16));
#129141=DIRECTION('center_axis',(0.950250383060611,0.311487093092615,-1.8162479738927E-5));
#129142=DIRECTION('ref_axis',(0.269503948346045,-0.82220208022195,-0.501349539846792));
#129143=DIRECTION('center_axis',(-0.978684514577287,-0.205369473383614,
-1.81316452205297E-5));
#129144=DIRECTION('ref_axis',(0.178060372501871,-0.848499490336936,-0.498340364251638));
#129145=DIRECTION('center_axis',(-1.4081690688991E-16,-6.98296267768627E-15,
1.));
#129146=DIRECTION('ref_axis',(-1.,8.26087817385229E-31,-1.38060560438432E-16));
#129147=DIRECTION('center_axis',(0.95024617416422,0.311499932815776,-1.84940629314651E-5));
#129148=DIRECTION('ref_axis',(0.270073604475813,-0.823843494141799,0.498339387692437));
#129149=DIRECTION('center_axis',(-0.97868728932903,-0.205356249874684,-1.85257221081351E-5));
#129150=DIRECTION('ref_axis',(0.177674469289125,-0.846806623517829,0.501348506858415));
#129151=DIRECTION('center_axis',(-1.4081690688991E-16,-6.98296267768627E-15,
1.));
#129152=DIRECTION('ref_axis',(-1.,9.83319205199467E-31,-1.40816906889911E-16));
#129153=DIRECTION('center_axis',(-1.4081690688991E-16,-6.98296267768627E-15,
1.));
#129154=DIRECTION('ref_axis',(-1.,8.46073526001725E-31,-1.4081690688991E-16));
#129155=DIRECTION('',(-0.207911690817763,0.978147600733805,6.80109070798532E-15));
#129156=DIRECTION('center_axis',(-1.4081690688991E-16,-6.98296267768627E-15,
1.));
#129157=DIRECTION('ref_axis',(-1.,7.97077743482043E-31,-1.4081690688991E-16));
#129158=DIRECTION('center_axis',(-1.4081690688991E-16,-6.98296267768627E-15,
1.));
#129159=DIRECTION('ref_axis',(-1.,7.97077743482043E-31,-1.4081690688991E-16));
#129160=DIRECTION('center_axis',(-1.4081690688991E-16,-6.98296267768627E-15,
1.));
#129161=DIRECTION('ref_axis',(-1.,7.97077743482043E-31,-1.4081690688991E-16));
#129162=DIRECTION('',(0.104528463267657,-0.994521895368273,-6.92998990261915E-15));
#129163=DIRECTION('center_axis',(1.4081690688991E-16,6.98296267768627E-15,
-1.));
#129164=DIRECTION('ref_axis',(1.,-7.97077743482043E-31,1.4081690688991E-16));
#129165=DIRECTION('',(-0.103961598321241,0.48907788477527,-0.866022406579784));
#129166=DIRECTION('center_axis',(1.4081690688991E-16,6.98296267768627E-15,
-1.));
#129167=DIRECTION('ref_axis',(-1.,7.97577417048809E-31,-1.40816906889911E-16));
#129168=DIRECTION('',(0.0522600224406469,-0.497266609935018,0.866022406579782));
#129169=DIRECTION('center_axis',(-1.4081690688991E-16,-6.98296267768627E-15,
1.));
#129170=DIRECTION('ref_axis',(-1.,9.83319205199467E-31,-1.40816906889911E-16));
#129171=DIRECTION('center_axis',(-1.4081690688991E-16,-6.98296267768627E-15,
1.));
#129172=DIRECTION('ref_axis',(-1.,7.98248735348668E-31,-1.4081690688991E-16));
#129173=DIRECTION('',(-0.207911690817763,0.978147600733805,6.80109070798532E-15));
#129174=DIRECTION('center_axis',(1.4081690688991E-16,6.98296267768627E-15,
-1.));
#129175=DIRECTION('ref_axis',(-1.,7.98707387273907E-31,-1.4081690688991E-16));
#129176=DIRECTION('',(0.104528463267657,-0.994521895368273,-6.92998990261915E-15));
#129177=DIRECTION('center_axis',(-1.4081690688991E-16,-6.98296267768627E-15,
1.));
#129178=DIRECTION('ref_axis',(-1.,7.99150043815584E-31,-1.4081690688991E-16));
#129179=DIRECTION('center_axis',(-1.4081690688991E-16,-6.98296267768627E-15,
1.));
#129180=DIRECTION('ref_axis',(1.,-7.99370576998456E-31,1.4081690688991E-16));
#129181=DIRECTION('',(-0.103952356682308,0.489079645219203,0.866022521746665));
#129182=DIRECTION('center_axis',(-1.4081690688991E-16,-6.98296267768627E-15,
1.));
#129183=DIRECTION('ref_axis',(-1.,7.99858039355471E-31,-1.4081690688991E-16));
#129184=DIRECTION('center_axis',(-1.4081690688991E-16,-6.98296267768627E-15,
1.));
#129185=DIRECTION('ref_axis',(-1.,7.99858039355471E-31,-1.4081690688991E-16));
#129186=DIRECTION('center_axis',(-1.4081690688991E-16,-6.98296267768627E-15,
1.));
#129187=DIRECTION('ref_axis',(-1.,7.99858039355471E-31,-1.4081690688991E-16));
#129188=DIRECTION('',(0.0522693557686684,-0.497265428393196,-0.866022521746669));
#129189=DIRECTION('center_axis',(-1.4081690688991E-16,-6.98296267768627E-15,
1.));
#129190=DIRECTION('ref_axis',(-1.,9.83319205199467E-31,-1.40816906889911E-16));
#129191=DIRECTION('',(-0.207911690817763,0.978147600733805,6.80109070798532E-15));
#129192=DIRECTION('center_axis',(1.4081690688991E-16,6.98296267768627E-15,
-1.));
#129193=DIRECTION('ref_axis',(-1.,8.01265634860448E-31,-1.4081690688991E-16));
#129194=DIRECTION('',(0.104528463267657,-0.994521895368273,-6.92998990261915E-15));
#129195=DIRECTION('center_axis',(-1.4081690688991E-16,-6.98296267768627E-15,
1.));
#129196=DIRECTION('ref_axis',(-1.,8.32577322149061E-31,-1.39145123902276E-16));
#129197=DIRECTION('center_axis',(-0.97836955922212,-0.206864703431162,-7.86457204713208E-6));
#129198=DIRECTION('ref_axis',(-7.99745536701625E-6,-1.93871482032999E-7,
0.999999999968002));
#129199=DIRECTION('center_axis',(0.994409453539566,0.1055927963892,-7.86457224402987E-6));
#129200=DIRECTION('ref_axis',(0.089551568788591,-0.843303350210964,0.52992450033044));
#129201=DIRECTION('center_axis',(-1.4081690688991E-16,-6.98296267768627E-15,
1.));
#129202=DIRECTION('ref_axis',(-1.,8.07722881720021E-31,-1.42096112075504E-16));
#129203=DIRECTION('center_axis',(-0.978360123517457,-0.206909324621784,
9.77058473225947E-6));
#129204=DIRECTION('ref_axis',(0.180976161286408,-0.855713599897275,0.484769908303809));
#129205=DIRECTION('center_axis',(0.994414268361371,0.10554744328432,9.77051646637645E-6));
#129206=DIRECTION('ref_axis',(0.0923122812912403,-0.869764184940697,0.484756336025897));
#129207=DIRECTION('center_axis',(-1.4081690688991E-16,-6.98296267768627E-15,
1.));
#129208=DIRECTION('ref_axis',(-1.,8.24049048117772E-31,-1.37719829560012E-16));
#129209=DIRECTION('center_axis',(0.977604079204538,0.21045252194443,-1.81624797767727E-5));
#129210=DIRECTION('ref_axis',(0.182084057577967,-0.845868804766416,-0.501349539841195));
#129211=DIRECTION('center_axis',(-0.994790133859859,-0.101944049587639,
-1.81316452111653E-5));
#129212=DIRECTION('ref_axis',(0.088392591342371,-0.862463698456793,-0.498340364249185));
#129213=DIRECTION('center_axis',(-1.4081690688991E-16,-6.98296267768627E-15,
1.));
#129214=DIRECTION('ref_axis',(-1.,8.26087817385229E-31,-1.38060560438432E-16));
#129215=DIRECTION('center_axis',(0.977601235480708,0.210465731283179,-1.84940567618171E-5));
#129216=DIRECTION('ref_axis',(0.182479018595484,-0.84756077212075,0.498339387701301));
#129217=DIRECTION('center_axis',(-0.994791511178781,-0.101930608471819,
-1.85257114470306E-5));
#129218=DIRECTION('ref_axis',(0.0881857549149666,-0.860739767469655,0.501348506855623));
#129219=DIRECTION('center_axis',(-1.4081690688991E-16,-6.98296267768627E-15,
1.));
#129220=DIRECTION('ref_axis',(-1.,9.83319205199467E-31,-1.40816906889911E-16));
#129221=DIRECTION('center_axis',(-1.4081690688991E-16,-6.98296267768627E-15,
1.));
#129222=DIRECTION('ref_axis',(-1.,8.46073526001725E-31,-1.4081690688991E-16));
#129223=DIRECTION('',(-0.104528463267657,0.994521895368273,6.92998990261915E-15));
#129224=DIRECTION('center_axis',(-1.4081690688991E-16,-6.98296267768627E-15,
1.));
#129225=DIRECTION('ref_axis',(-1.,7.97077743482043E-31,-1.4081690688991E-16));
#129226=DIRECTION('center_axis',(-1.4081690688991E-16,-6.98296267768627E-15,
1.));
#129227=DIRECTION('ref_axis',(-1.,7.97077743482043E-31,-1.4081690688991E-16));
#129228=DIRECTION('center_axis',(-1.4081690688991E-16,-6.98296267768627E-15,
1.));
#129229=DIRECTION('ref_axis',(-1.,7.97077743482043E-31,-1.4081690688991E-16));
#129230=DIRECTION('',(3.49148133884313E-15,-1.,-6.98296267768627E-15));
#129231=DIRECTION('center_axis',(1.4081690688991E-16,6.98296267768627E-15,
-1.));
#129232=DIRECTION('ref_axis',(1.,-7.97077743482043E-31,1.4081690688991E-16));
#129233=DIRECTION('',(-0.0522695260941984,0.497265611060783,-0.86602240657978));
#129234=DIRECTION('center_axis',(1.4081690688991E-16,6.98296267768627E-15,
-1.));
#129235=DIRECTION('ref_axis',(-1.,7.97577417048809E-31,-1.40816906889911E-16));
#129236=DIRECTION('',(-4.77800116381158E-6,-0.500005191251988,0.86602240657978));
#129237=DIRECTION('center_axis',(-1.4081690688991E-16,-6.98296267768627E-15,
1.));
#129238=DIRECTION('ref_axis',(-1.,9.83319205199467E-31,-1.40816906889911E-16));
#129239=DIRECTION('center_axis',(-1.4081690688991E-16,-6.98296267768627E-15,
1.));
#129240=DIRECTION('ref_axis',(-1.,7.98248735348668E-31,-1.4081690688991E-16));
#129241=DIRECTION('',(-0.104528463267657,0.994521895368273,6.92998990261915E-15));
#129242=DIRECTION('center_axis',(1.4081690688991E-16,6.98296267768627E-15,
-1.));
#129243=DIRECTION('ref_axis',(-1.,7.98707387273907E-31,-1.4081690688991E-16));
#129244=DIRECTION('',(3.49148133884313E-15,-1.,-6.98296267768627E-15));
#129245=DIRECTION('center_axis',(-1.4081690688991E-16,-6.98296267768627E-15,
1.));
#129246=DIRECTION('ref_axis',(-1.,7.99150043815584E-31,-1.4081690688991E-16));
#129247=DIRECTION('center_axis',(-1.4081690688991E-16,-6.98296267768627E-15,
1.));
#129248=DIRECTION('ref_axis',(1.,-7.99370576998456E-31,1.4081690688991E-16));
#129249=DIRECTION('',(-0.0522601510654385,0.497266395846527,0.866022521746648));
#129250=DIRECTION('center_axis',(-1.4081690688991E-16,-6.98296267768627E-15,
1.));
#129251=DIRECTION('ref_axis',(-1.,7.99858039355471E-31,-1.4081690688991E-16));
#129252=DIRECTION('center_axis',(-1.4081690688991E-16,-6.98296267768627E-15,
1.));
#129253=DIRECTION('ref_axis',(-1.,7.99858039355471E-31,-1.4081690688991E-16));
#129254=DIRECTION('center_axis',(-1.4081690688991E-16,-6.98296267768627E-15,
1.));
#129255=DIRECTION('ref_axis',(-1.,7.99858039355471E-31,-1.4081690688991E-16));
#129256=DIRECTION('',(4.62770265447403E-6,-0.500004991781227,-0.866022521746657));
#129257=DIRECTION('center_axis',(-1.4081690688991E-16,-6.98296267768627E-15,
1.));
#129258=DIRECTION('ref_axis',(-1.,9.83319205199467E-31,-1.40816906889911E-16));
#129259=DIRECTION('',(-0.104528463267657,0.994521895368273,6.92998990261915E-15));
#129260=DIRECTION('center_axis',(1.4081690688991E-16,6.98296267768627E-15,
-1.));
#129261=DIRECTION('ref_axis',(-1.,8.01265634860448E-31,-1.4081690688991E-16));
#129262=DIRECTION('',(3.49148133884313E-15,-1.,-6.98296267768627E-15));
#129263=DIRECTION('center_axis',(-1.4081690688991E-16,-6.98296267768627E-15,
1.));
#129264=DIRECTION('ref_axis',(-1.,8.32577322149061E-31,-1.39145123902276E-16));
#129265=DIRECTION('center_axis',(-0.994633197962183,-0.103464010407821,
-7.86457204165851E-6));
#129266=DIRECTION('ref_axis',(-7.97390954732109E-6,6.43152258466824E-7,
0.999999999968002));
#129267=DIRECTION('center_axis',(0.999999427244995,0.00107025596491169,
-7.8645722516888E-6));
#129268=DIRECTION('ref_axis',(0.000911792658824946,-0.848044334090887,0.529924500330464));
#129269=DIRECTION('center_axis',(-1.4081690688991E-16,-6.98296267768627E-15,
1.));
#129270=DIRECTION('ref_axis',(-1.,8.07722881720021E-31,-1.42096112075504E-16));
#129271=DIRECTION('center_axis',(-0.994628478131894,-0.103509373457524,
9.77058659696217E-6));
#129272=DIRECTION('ref_axis',(0.0905383273445894,-0.869943071290438,0.484769908302283));
#129273=DIRECTION('center_axis',(0.999999475000345,0.00102464802303793,
9.77051626642102E-6));
#129274=DIRECTION('ref_axis',(0.000891471298433148,-0.874648786634365,0.484756336026624));
#129275=DIRECTION('center_axis',(-1.4081690688991E-16,-6.98296267768627E-15,
1.));
#129276=DIRECTION('ref_axis',(-1.,8.24049048117772E-31,-1.37719829560012E-16));
#129277=DIRECTION('center_axis',(0.994246940479906,0.107112188925769,-1.81624797621619E-5));
#129278=DIRECTION('ref_axis',(0.0926692157700999,-0.860268013669517,-0.501349539847857));
#129279=DIRECTION('center_axis',(-0.999996624262643,0.00259829454877836,
-1.81316452333963E-5));
#129280=DIRECTION('ref_axis',(0.00224363754548965,0.866978573814012,0.498340364247155));
#129281=DIRECTION('center_axis',(-1.4081690688991E-16,-6.98296267768627E-15,
1.));
#129282=DIRECTION('ref_axis',(-1.,8.26087817385229E-31,-1.38060560438432E-16));
#129283=DIRECTION('center_axis',(0.994245493086127,0.107125623152885,-1.84940559963087E-5));
#129284=DIRECTION('ref_axis',(0.0928851544033258,-0.861991996926722,0.498339387692517));
#129285=DIRECTION('center_axis',(-0.999996589057286,0.00261180600205774,
-1.85257109659478E-5));
#129286=DIRECTION('ref_axis',(0.00226914104443498,0.865242466405694,-0.50134850685637));
#129287=DIRECTION('center_axis',(-1.4081690688991E-16,-6.98296267768627E-15,
1.));
#129288=DIRECTION('ref_axis',(-1.,9.83319205199467E-31,-1.40816906889911E-16));
#129289=DIRECTION('center_axis',(-1.4081690688991E-16,-6.98296267768627E-15,
1.));
#129290=DIRECTION('ref_axis',(-1.,8.46073526001725E-31,-1.4081690688991E-16));
#129291=DIRECTION('',(-3.49148133884313E-15,1.,6.98296267768627E-15));
#129292=DIRECTION('center_axis',(-1.4081690688991E-16,-6.98296267768627E-15,
1.));
#129293=DIRECTION('ref_axis',(-1.,7.97077743482043E-31,-1.4081690688991E-16));
#129294=DIRECTION('center_axis',(-1.4081690688991E-16,-6.98296267768627E-15,
1.));
#129295=DIRECTION('ref_axis',(-1.,7.97077743482043E-31,-1.4081690688991E-16));
#129296=DIRECTION('center_axis',(-1.4081690688991E-16,-6.98296267768627E-15,
1.));
#129297=DIRECTION('ref_axis',(-1.,7.97077743482043E-31,-1.4081690688991E-16));
#129298=DIRECTION('',(-0.10452846326765,-0.994521895368274,-6.95942865237777E-15));
#129299=DIRECTION('center_axis',(1.4081690688991E-16,6.98296267768627E-15,
-1.));
#129300=DIRECTION('ref_axis',(1.,-7.97077743482043E-31,1.4081690688991E-16));
#129301=DIRECTION('',(-4.77800116722347E-6,0.500005191251988,-0.86602240657978));
#129302=DIRECTION('center_axis',(1.4081690688991E-16,6.98296267768627E-15,
-1.));
#129303=DIRECTION('ref_axis',(-1.,7.97577417048809E-31,-1.40816906889911E-16));
#129304=DIRECTION('',(-0.0522695260941984,-0.497265611060783,0.86602240657978));
#129305=DIRECTION('center_axis',(-1.4081690688991E-16,-6.98296267768627E-15,
1.));
#129306=DIRECTION('ref_axis',(-1.,9.83319205199467E-31,-1.40816906889911E-16));
#129307=DIRECTION('center_axis',(-1.4081690688991E-16,-6.98296267768627E-15,
1.));
#129308=DIRECTION('ref_axis',(-1.,7.98248735348668E-31,-1.4081690688991E-16));
#129309=DIRECTION('',(-3.49148133884313E-15,1.,6.98296267768627E-15));
#129310=DIRECTION('center_axis',(1.4081690688991E-16,6.98296267768627E-15,
-1.));
#129311=DIRECTION('ref_axis',(-1.,7.98707387273907E-31,-1.4081690688991E-16));
#129312=DIRECTION('',(-0.10452846326765,-0.994521895368274,-6.95942865237777E-15));
#129313=DIRECTION('center_axis',(-1.4081690688991E-16,-6.98296267768627E-15,
1.));
#129314=DIRECTION('ref_axis',(-1.,7.99150043815584E-31,-1.4081690688991E-16));
#129315=DIRECTION('center_axis',(-1.4081690688991E-16,-6.98296267768627E-15,
1.));
#129316=DIRECTION('ref_axis',(1.,-7.99370576998456E-31,1.4081690688991E-16));
#129317=DIRECTION('',(4.62770265084889E-6,0.500004991781227,0.866022521746657));
#129318=DIRECTION('center_axis',(-1.4081690688991E-16,-6.98296267768627E-15,
1.));
#129319=DIRECTION('ref_axis',(-1.,7.99858039355471E-31,-1.4081690688991E-16));
#129320=DIRECTION('center_axis',(-1.4081690688991E-16,-6.98296267768627E-15,
1.));
#129321=DIRECTION('ref_axis',(-1.,7.99858039355471E-31,-1.4081690688991E-16));
#129322=DIRECTION('center_axis',(-1.4081690688991E-16,-6.98296267768627E-15,
1.));
#129323=DIRECTION('ref_axis',(-1.,7.99858039355471E-31,-1.4081690688991E-16));
#129324=DIRECTION('',(-0.0522601510654325,-0.497266395846506,-0.86602252174666));
#129325=DIRECTION('center_axis',(-1.4081690688991E-16,-6.98296267768627E-15,
1.));
#129326=DIRECTION('ref_axis',(-1.,9.83319205199467E-31,-1.40816906889911E-16));
#129327=DIRECTION('',(-3.49148133884313E-15,1.,6.98296267768627E-15));
#129328=DIRECTION('center_axis',(1.4081690688991E-16,6.98296267768627E-15,
-1.));
#129329=DIRECTION('ref_axis',(-1.,8.01265634860448E-31,-1.4081690688991E-16));
#129330=DIRECTION('',(-0.10452846326765,-0.994521895368274,-6.95942865237777E-15));
#129331=DIRECTION('center_axis',(-1.4081690688991E-16,-6.98296267768627E-15,
1.));
#129332=DIRECTION('ref_axis',(-1.,8.32577322149061E-31,-1.39145123902276E-16));
#129333=DIRECTION('center_axis',(-0.999999427244995,0.00107025596477908,
-7.86457202530775E-6));
#129334=DIRECTION('ref_axis',(-7.86299990295341E-6,1.47312954961576E-6,
0.999999999968002));
#129335=DIRECTION('center_axis',(0.994633197962195,-0.103464010407701,-7.86457224889578E-6));
#129336=DIRECTION('ref_axis',(-0.0877379732621264,-0.843493966781859,0.529924500330433));
#129337=DIRECTION('center_axis',(-1.4081690688991E-16,-6.98296267768627E-15,
1.));
#129338=DIRECTION('ref_axis',(-1.,8.07722881720021E-31,-1.42096112075504E-16));
#129339=DIRECTION('center_axis',(-0.999999475000305,0.00102464806168852,
9.7705860071373E-6));
#129340=DIRECTION('ref_axis',(0.000891463458118558,0.874641264344406,-0.484769908305911));
#129341=DIRECTION('center_axis',(0.994628478127856,-0.10350937349633,9.77051619636314E-6));
#129342=DIRECTION('ref_axis',(0.0905391058404323,0.869950553190108,-0.484756336026502));
#129343=DIRECTION('center_axis',(-1.4081690688991E-16,-6.98296267768627E-15,
1.));
#129344=DIRECTION('ref_axis',(-1.,8.24049048117772E-31,-1.37719829560012E-16));
#129345=DIRECTION('center_axis',(0.999996624215829,0.00259831235056682,
-1.81624797792608E-5));
#129346=DIRECTION('ref_axis',(0.00223907064277466,-0.865241946198171,-0.501349539844066));
#129347=DIRECTION('center_axis',(-0.994246942387264,0.107112171226335,-1.81316451412819E-5));
#129348=DIRECTION('ref_axis',(0.0928552846708738,0.861994650487102,0.498340364249486));
#129349=DIRECTION('center_axis',(-1.4081690688991E-16,-6.98296267768627E-15,
1.));
#129350=DIRECTION('ref_axis',(-1.,8.26087817385229E-31,-1.38060560438432E-16));
#129351=DIRECTION('center_axis',(0.999996589010146,0.00261182427508522,
-1.84940600871693E-5));
#129352=DIRECTION('ref_axis',(0.00227362102100115,-0.866979057022949,0.498339387697832));
#129353=DIRECTION('center_axis',(-0.994245495043239,0.10712560498323,-1.85257097907709E-5));
#129354=DIRECTION('ref_axis',(0.092699175819317,0.860265387813317,-0.501348506862066));
#129355=DIRECTION('center_axis',(-1.4081690688991E-16,-6.98296267768627E-15,
1.));
#129356=DIRECTION('ref_axis',(-1.,9.83319205199467E-31,-1.40816906889911E-16));
#129357=DIRECTION('center_axis',(-1.4081690688991E-16,-6.98296267768627E-15,
1.));
#129358=DIRECTION('ref_axis',(-1.,8.46073526001725E-31,-1.4081690688991E-16));
#129359=DIRECTION('',(0.10452846326765,0.994521895368274,6.95942865237777E-15));
#129360=DIRECTION('center_axis',(-1.4081690688991E-16,-6.98296267768627E-15,
1.));
#129361=DIRECTION('ref_axis',(-1.,7.97077743482043E-31,-1.4081690688991E-16));
#129362=DIRECTION('center_axis',(-1.4081690688991E-16,-6.98296267768627E-15,
1.));
#129363=DIRECTION('ref_axis',(-1.,7.97077743482043E-31,-1.4081690688991E-16));
#129364=DIRECTION('center_axis',(-1.4081690688991E-16,-6.98296267768627E-15,
1.));
#129365=DIRECTION('ref_axis',(-1.,7.97077743482043E-31,-1.4081690688991E-16));
#129366=DIRECTION('',(-0.207911690817756,-0.978147600733806,-6.85964567039975E-15));
#129367=DIRECTION('center_axis',(1.4081690688991E-16,6.98296267768627E-15,
-1.));
#129368=DIRECTION('ref_axis',(1.,-7.97077743482043E-31,1.4081690688991E-16));
#129369=DIRECTION('',(0.0522600224406469,0.497266609935018,-0.866022406579782));
#129370=DIRECTION('center_axis',(1.4081690688991E-16,6.98296267768627E-15,
-1.));
#129371=DIRECTION('ref_axis',(-1.,7.97577417048809E-31,-1.40816906889911E-16));
#129372=DIRECTION('',(-0.103961598321246,-0.48907788477529,0.866022406579772));
#129373=DIRECTION('center_axis',(-1.4081690688991E-16,-6.98296267768627E-15,
1.));
#129374=DIRECTION('ref_axis',(-1.,9.83319205199467E-31,-1.40816906889911E-16));
#129375=DIRECTION('center_axis',(-1.4081690688991E-16,-6.98296267768627E-15,
1.));
#129376=DIRECTION('ref_axis',(-1.,7.98248735348668E-31,-1.4081690688991E-16));
#129377=DIRECTION('',(0.10452846326765,0.994521895368274,6.95942865237777E-15));
#129378=DIRECTION('center_axis',(1.4081690688991E-16,6.98296267768627E-15,
-1.));
#129379=DIRECTION('ref_axis',(-1.,7.98707387273907E-31,-1.4081690688991E-16));
#129380=DIRECTION('',(-0.207911690817756,-0.978147600733806,-6.85964567039975E-15));
#129381=DIRECTION('center_axis',(-1.4081690688991E-16,-6.98296267768627E-15,
1.));
#129382=DIRECTION('ref_axis',(-1.,7.99150043815584E-31,-1.4081690688991E-16));
#129383=DIRECTION('center_axis',(-1.4081690688991E-16,-6.98296267768627E-15,
1.));
#129384=DIRECTION('ref_axis',(1.,-7.99370576998456E-31,1.4081690688991E-16));
#129385=DIRECTION('',(0.0522693557686642,0.497265428393217,0.866022521746657));
#129386=DIRECTION('center_axis',(-1.4081690688991E-16,-6.98296267768627E-15,
1.));
#129387=DIRECTION('ref_axis',(-1.,7.99858039355471E-31,-1.4081690688991E-16));
#129388=DIRECTION('center_axis',(-1.4081690688991E-16,-6.98296267768627E-15,
1.));
#129389=DIRECTION('ref_axis',(-1.,7.99858039355471E-31,-1.4081690688991E-16));
#129390=DIRECTION('center_axis',(-1.4081690688991E-16,-6.98296267768627E-15,
1.));
#129391=DIRECTION('ref_axis',(-1.,7.99858039355471E-31,-1.4081690688991E-16));
#129392=DIRECTION('',(-0.103952356682315,-0.489079645219203,-0.866022521746664));
#129393=DIRECTION('center_axis',(-1.4081690688991E-16,-6.98296267768627E-15,
1.));
#129394=DIRECTION('ref_axis',(-1.,9.83319205199467E-31,-1.40816906889911E-16));
#129395=DIRECTION('',(0.10452846326765,0.994521895368274,6.95942865237777E-15));
#129396=DIRECTION('center_axis',(1.4081690688991E-16,6.98296267768627E-15,
-1.));
#129397=DIRECTION('ref_axis',(-1.,8.01265634860448E-31,-1.4081690688991E-16));
#129398=DIRECTION('',(-0.207911690817756,-0.978147600733806,-6.85964567039975E-15));
#129399=DIRECTION('center_axis',(-1.4081690688991E-16,-6.98296267768627E-15,
1.));
#129400=DIRECTION('ref_axis',(-1.,8.32577322149061E-31,-1.39145123902276E-16));
#129401=DIRECTION('center_axis',(-0.99440945353958,0.105592796389069,-7.8645720232461E-6));
#129402=DIRECTION('ref_axis',(-7.66594160056427E-6,2.28696684648491E-6,
0.999999999968002));
#129403=DIRECTION('center_axis',(0.978369559222141,-0.206864703431062,-7.86457222351689E-6));
#129404=DIRECTION('ref_axis',(-0.175426463587687,-0.829702103060253,0.529924500330482));
#129405=DIRECTION('center_axis',(-1.4081690688991E-16,-6.98296267768627E-15,
1.));
#129406=DIRECTION('ref_axis',(-1.,8.07722881720021E-31,-1.42096112075504E-16));
#129407=DIRECTION('center_axis',(-0.994414268357388,0.105547443321838,9.77058454997984E-6));
#129408=DIRECTION('ref_axis',(0.0923114872006156,0.869756704679602,-0.484769908302578));
#129409=DIRECTION('center_axis',(0.97836012350987,-0.206909324657662,9.77051847768451E-6));
#129410=DIRECTION('ref_axis',(0.180977717589303,0.855720959436757,-0.484756336025433));
#129411=DIRECTION('center_axis',(-1.4081690688991E-16,-6.98296267768627E-15,
1.));
#129412=DIRECTION('ref_axis',(-1.,8.24049048117772E-31,-1.37719829560012E-16));
#129413=DIRECTION('center_axis',(0.994790135674088,-0.101944031878547,-1.81624797219411E-5));
#129414=DIRECTION('ref_axis',(0.0882156062118037,0.860736106903253,0.501349539835948));
#129415=DIRECTION('center_axis',(-0.977604082951534,0.210452504541368,-1.81316451866862E-5));
#129416=DIRECTION('ref_axis',(0.18244958986568,0.847566533384385,0.498340364253811));
#129417=DIRECTION('center_axis',(-1.4081690688991E-16,-6.98296267768627E-15,
1.));
#129418=DIRECTION('ref_axis',(-1.,8.26087817385229E-31,-1.38060560438432E-16));
#129419=DIRECTION('center_axis',(0.994791513041809,-0.101930590295349,-1.84940629635532E-5));
#129420=DIRECTION('ref_axis',(0.0883628226288196,0.862467313147628,-0.498339387695754));
#129421=DIRECTION('center_axis',(-0.977601239326386,0.210465713417443,-1.85257108287527E-5));
#129422=DIRECTION('ref_axis',(0.182113579025484,0.845863061613818,-0.501348506861073));
#129423=DIRECTION('center_axis',(-1.4081690688991E-16,-6.98296267768627E-15,
1.));
#129424=DIRECTION('ref_axis',(-1.,9.83319205199467E-31,-1.40816906889911E-16));
#129425=DIRECTION('center_axis',(-1.4081690688991E-16,-6.98296267768627E-15,
1.));
#129426=DIRECTION('ref_axis',(-1.,8.46073526001725E-31,-1.4081690688991E-16));
#129427=DIRECTION('',(0.207911690817756,0.978147600733806,6.85964567039975E-15));
#129428=DIRECTION('center_axis',(-1.4081690688991E-16,-6.98296267768627E-15,
1.));
#129429=DIRECTION('ref_axis',(-1.,7.97077743482043E-31,-1.4081690688991E-16));
#129430=DIRECTION('center_axis',(-1.4081690688991E-16,-6.98296267768627E-15,
1.));
#129431=DIRECTION('ref_axis',(-1.,7.97077743482043E-31,-1.4081690688991E-16));
#129432=DIRECTION('center_axis',(-1.4081690688991E-16,-6.98296267768627E-15,
1.));
#129433=DIRECTION('ref_axis',(-1.,7.97077743482043E-31,-1.4081690688991E-16));
#129434=DIRECTION('',(-0.309016994374945,-0.951056516295154,-6.68470697498368E-15));
#129435=DIRECTION('center_axis',(1.4081690688991E-16,6.98296267768627E-15,
-1.));
#129436=DIRECTION('ref_axis',(1.,-7.97077743482043E-31,1.4081690688991E-16));
#129437=DIRECTION('',(0.103952251140481,0.489079871579877,-0.866022406579782));
#129438=DIRECTION('center_axis',(1.4081690688991E-16,6.98296267768627E-15,
-1.));
#129439=DIRECTION('ref_axis',(-1.,7.97577417048809E-31,-1.40816906889911E-16));
#129440=DIRECTION('',(-0.154514645521688,-0.47553171883805,0.866022406579782));
#129441=DIRECTION('center_axis',(-1.4081690688991E-16,-6.98296267768627E-15,
1.));
#129442=DIRECTION('ref_axis',(-1.,9.83319205199467E-31,-1.40816906889911E-16));
#129443=DIRECTION('center_axis',(-1.4081690688991E-16,-6.98296267768627E-15,
1.));
#129444=DIRECTION('ref_axis',(-1.,7.98248735348668E-31,-1.4081690688991E-16));
#129445=DIRECTION('',(0.207911690817756,0.978147600733806,6.85964567039975E-15));
#129446=DIRECTION('center_axis',(1.4081690688991E-16,6.98296267768627E-15,
-1.));
#129447=DIRECTION('ref_axis',(-1.,7.98707387273907E-31,-1.4081690688991E-16));
#129448=DIRECTION('',(-0.309016994374945,-0.951056516295154,-6.68470697498368E-15));
#129449=DIRECTION('center_axis',(-1.4081690688991E-16,-6.98296267768627E-15,
1.));
#129450=DIRECTION('ref_axis',(-1.,7.99150043815584E-31,-1.4081690688991E-16));
#129451=DIRECTION('center_axis',(-1.4081690688991E-16,-6.98296267768627E-15,
1.));
#129452=DIRECTION('ref_axis',(1.,-7.99370576998456E-31,1.4081690688991E-16));
#129453=DIRECTION('',(0.103961409834803,0.489077720912241,0.866022521746662));
#129454=DIRECTION('center_axis',(-1.4081690688991E-16,-6.98296267768627E-15,
1.));
#129455=DIRECTION('ref_axis',(-1.,7.99858039355471E-31,-1.4081690688991E-16));
#129456=DIRECTION('center_axis',(-1.4081690688991E-16,-6.98296267768627E-15,
1.));
#129457=DIRECTION('ref_axis',(-1.,7.99858039355471E-31,-1.4081690688991E-16));
#129458=DIRECTION('center_axis',(-1.4081690688991E-16,-6.98296267768627E-15,
1.));
#129459=DIRECTION('ref_axis',(-1.,7.99858039355471E-31,-1.4081690688991E-16));
#129460=DIRECTION('',(-0.154505638525963,-0.475534435652396,-0.866022521746659));
#129461=DIRECTION('center_axis',(-1.4081690688991E-16,-6.98296267768627E-15,
1.));
#129462=DIRECTION('ref_axis',(-1.,9.83319205199467E-31,-1.40816906889911E-16));
#129463=DIRECTION('',(0.207911690817756,0.978147600733806,6.85964567039975E-15));
#129464=DIRECTION('center_axis',(1.4081690688991E-16,6.98296267768627E-15,
-1.));
#129465=DIRECTION('ref_axis',(-1.,8.01265634860448E-31,-1.4081690688991E-16));
#129466=DIRECTION('',(-0.309016994374945,-0.951056516295154,-6.68470697498368E-15));
#129467=DIRECTION('center_axis',(-1.4081690688991E-16,-6.98296267768627E-15,
1.));
#129468=DIRECTION('ref_axis',(-1.,8.32577322149061E-31,-1.39145123902276E-16));
#129469=DIRECTION('center_axis',(-0.977924521767628,0.208958440039413,-7.86457201262958E-6));
#129470=DIRECTION('ref_axis',(-7.38489362573486E-6,3.07574770634862E-6,
0.999999999968002));
#129471=DIRECTION('center_axis',(0.951386698854285,-0.307998943474316,-7.86457238851017E-6));
#129472=DIRECTION('ref_axis',(-0.26119294486766,-0.806819849471295,0.529924500330449));
#129473=DIRECTION('center_axis',(-1.4081690688991E-16,-6.98296267768627E-15,
1.));
#129474=DIRECTION('ref_axis',(-1.,8.07722881720021E-31,-1.42096112075504E-16));
#129475=DIRECTION('center_axis',(-0.977934050895432,0.208913838708178,9.77058768185539E-6));
#129476=DIRECTION('ref_axis',(0.182720126971878,0.855342908548244,-0.484769908302497));
#129477=DIRECTION('center_axis',(0.951372650643604,-0.308042333960611,9.77051871801589E-6));
#129478=DIRECTION('ref_axis',(0.269433499591928,0.832115907779339,-0.484756336026888));
#129479=DIRECTION('center_axis',(-1.4081690688991E-16,-6.98296267768627E-15,
1.));
#129480=DIRECTION('ref_axis',(-1.,8.24049048117772E-31,-1.37719829560012E-16));
#129481=DIRECTION('center_axis',(0.978684518232685,-0.205369455961155,-1.81624797422718E-5));
#129482=DIRECTION('ref_axis',(0.177703774423219,0.846799862690149,0.50134953984589));
#129483=DIRECTION('center_axis',(-0.950250388606176,0.311487076176613,-1.81316452346279E-5));
#129484=DIRECTION('ref_axis',(0.270044939174658,0.82385229998126,0.498340364250924));
#129485=DIRECTION('center_axis',(-1.4081690688991E-16,-6.98296267768627E-15,
1.));
#129486=DIRECTION('ref_axis',(-1.,8.26087817385229E-31,-1.38060560438432E-16));
#129487=DIRECTION('center_axis',(0.978687293082038,-0.205356231991439,-1.84940717020688E-5));
#129488=DIRECTION('ref_axis',(0.178031144703119,0.848506196906769,-0.498339387693276));
#129489=DIRECTION('center_axis',(-0.950246179854334,0.311499915455917,-1.85257060786387E-5));
#129490=DIRECTION('ref_axis',(0.269532707750638,0.822193282704124,-0.50134850685808));
#129491=DIRECTION('center_axis',(-1.4081690688991E-16,-6.98296267768627E-15,
1.));
#129492=DIRECTION('ref_axis',(-1.,9.83319205199467E-31,-1.40816906889911E-16));
#129493=DIRECTION('center_axis',(-1.4081690688991E-16,-6.98296267768627E-15,
1.));
#129494=DIRECTION('ref_axis',(-1.,8.46073526001725E-31,-1.4081690688991E-16));
#129495=DIRECTION('',(0.309016994374945,0.951056516295154,6.68470697498368E-15));
#129496=DIRECTION('center_axis',(-1.4081690688991E-16,-6.98296267768627E-15,
1.));
#129497=DIRECTION('ref_axis',(-1.,7.97077743482043E-31,-1.4081690688991E-16));
#129498=DIRECTION('center_axis',(-1.4081690688991E-16,-6.98296267768627E-15,
1.));
#129499=DIRECTION('ref_axis',(-1.,7.97077743482043E-31,-1.4081690688991E-16));
#129500=DIRECTION('center_axis',(-1.4081690688991E-16,-6.98296267768627E-15,
1.));
#129501=DIRECTION('ref_axis',(-1.,7.97077743482043E-31,-1.4081690688991E-16));
#129502=DIRECTION('',(-0.406736643075798,-0.913545457642602,-6.43652923108483E-15));
#129503=DIRECTION('center_axis',(1.4081690688991E-16,6.98296267768627E-15,
-1.));
#129504=DIRECTION('ref_axis',(1.,-7.97077743482043E-31,1.4081690688991E-16));
#129505=DIRECTION('',(0.154505557223428,0.47553467180519,-0.866022406579765));
#129506=DIRECTION('center_axis',(1.4081690688991E-16,6.98296267768627E-15,
-1.));
#129507=DIRECTION('ref_axis',(-1.,7.97577417048809E-31,-1.40816906889911E-16));
#129508=DIRECTION('',(-0.203374797931581,-0.456775527877827,0.866022406579773));
#129509=DIRECTION('center_axis',(-1.4081690688991E-16,-6.98296267768627E-15,
1.));
#129510=DIRECTION('ref_axis',(-1.,9.83319205199467E-31,-1.40816906889911E-16));
#129511=DIRECTION('center_axis',(-1.4081690688991E-16,-6.98296267768627E-15,
1.));
#129512=DIRECTION('ref_axis',(-1.,7.98248735348668E-31,-1.4081690688991E-16));
#129513=DIRECTION('',(0.309016994374945,0.951056516295154,6.68470697498368E-15));
#129514=DIRECTION('center_axis',(1.4081690688991E-16,6.98296267768627E-15,
-1.));
#129515=DIRECTION('ref_axis',(-1.,7.98707387273907E-31,-1.4081690688991E-16));
#129516=DIRECTION('',(-0.406736643075798,-0.913545457642602,-6.43652923108483E-15));
#129517=DIRECTION('center_axis',(-1.4081690688991E-16,-6.98296267768627E-15,
1.));
#129518=DIRECTION('ref_axis',(-1.,7.99150043815584E-31,-1.4081690688991E-16));
#129519=DIRECTION('center_axis',(-1.4081690688991E-16,-6.98296267768627E-15,
1.));
#129520=DIRECTION('ref_axis',(1.,-7.99370576998456E-31,1.4081690688991E-16));
#129521=DIRECTION('',(0.154514440939479,0.47553157557488,0.866022521746653));
#129522=DIRECTION('center_axis',(-1.4081690688991E-16,-6.98296267768627E-15,
1.));
#129523=DIRECTION('ref_axis',(-1.,7.99858039355471E-31,-1.4081690688991E-16));
#129524=DIRECTION('center_axis',(-1.4081690688991E-16,-6.98296267768627E-15,
1.));
#129525=DIRECTION('ref_axis',(-1.,7.99858039355471E-31,-1.4081690688991E-16));
#129526=DIRECTION('center_axis',(-1.4081690688991E-16,-6.98296267768627E-15,
1.));
#129527=DIRECTION('ref_axis',(-1.,7.99858039355471E-31,-1.4081690688991E-16));
#129528=DIRECTION('',(-0.203366124261494,-0.456779171296591,-0.866022521746668));
#129529=DIRECTION('center_axis',(-1.4081690688991E-16,-6.98296267768627E-15,
1.));
#129530=DIRECTION('ref_axis',(-1.,9.83319205199467E-31,-1.40816906889911E-16));
#129531=DIRECTION('',(0.309016994374945,0.951056516295154,6.68470697498368E-15));
#129532=DIRECTION('center_axis',(1.4081690688991E-16,6.98296267768627E-15,
-1.));
#129533=DIRECTION('ref_axis',(-1.,8.01265634860448E-31,-1.4081690688991E-16));
#129534=DIRECTION('',(-0.406736643075798,-0.913545457642602,-6.43652923108483E-15));
#129535=DIRECTION('center_axis',(-1.4081690688991E-16,-6.98296267768627E-15,
1.));
#129536=DIRECTION('ref_axis',(-1.,8.32577322149061E-31,-1.39145123902276E-16));
#129537=DIRECTION('center_axis',(-0.950725244291359,0.310034691293224,-7.86457185161666E-6));
#129538=DIRECTION('ref_axis',(-7.02293506467738E-6,3.83082999767987E-6,
0.999999999968002));
#129539=DIRECTION('center_axis',(0.913980246723279,-0.405758682640066,-7.86457228997838E-6));
#129540=DIRECTION('ref_axis',(-0.344097741585765,-0.775097908773538,0.529924500330438));
#129541=DIRECTION('center_axis',(-1.4081690688991E-16,-6.98296267768627E-15,
1.));
#129542=DIRECTION('ref_axis',(-1.,8.07722881720021E-31,-1.42096112075504E-16));
#129543=DIRECTION('center_axis',(-0.950739383327522,0.309991330353832,9.77057983430093E-6));
#129544=DIRECTION('ref_axis',(0.271126846795281,0.83155779651818,-0.484769908303596));
#129545=DIRECTION('center_axis',(0.913961739929012,-0.405800366991542,9.77051730791796E-6));
#129546=DIRECTION('ref_axis',(0.354937311790441,0.799394020105231,-0.484756336027671));
#129547=DIRECTION('center_axis',(-1.4081690688991E-16,-6.98296267768627E-15,
1.));
#129548=DIRECTION('ref_axis',(-1.,8.24049048117772E-31,-1.37719829560012E-16));
#129549=DIRECTION('center_axis',(0.951856228406634,-0.30654480930791,-1.81624798152503E-5));
#129550=DIRECTION('ref_axis',(0.265244982896449,0.823585901985077,0.501349539841905));
#129551=DIRECTION('center_axis',(-0.912485552150597,0.409108930222335,-1.8131645163321E-5));
#129552=DIRECTION('ref_axis',(0.354681619617918,0.791111768373005,0.498340364256145));
#129553=DIRECTION('center_axis',(-1.4081690688991E-16,-6.98296267768627E-15,
1.));
#129554=DIRECTION('ref_axis',(-1.,8.26087817385229E-31,-1.38060560438432E-16));
#129555=DIRECTION('center_axis',(0.951860370339,-0.306531947822854,-1.84940563905878E-5));
#129556=DIRECTION('ref_axis',(0.265748920300046,0.825248669208596,-0.498339387695576));
#129557=DIRECTION('center_axis',(-0.912480024380723,0.409121259241015,-1.85256897665016E-5));
#129558=DIRECTION('ref_axis',(0.353998779726462,0.78951538213359,-0.501348506855887));
#129559=DIRECTION('center_axis',(-1.4081690688991E-16,-6.98296267768627E-15,
1.));
#129560=DIRECTION('ref_axis',(-1.,9.83319205199467E-31,-1.40816906889911E-16));
#129561=DIRECTION('center_axis',(-1.4081690688991E-16,-6.98296267768627E-15,
1.));
#129562=DIRECTION('ref_axis',(-1.,8.46073526001725E-31,-1.4081690688991E-16));
#129563=DIRECTION('',(0.406736643075798,0.913545457642602,6.43652923108483E-15));
#129564=DIRECTION('center_axis',(-1.4081690688991E-16,-6.98296267768627E-15,
1.));
#129565=DIRECTION('ref_axis',(-1.,7.97077743482043E-31,-1.4081690688991E-16));
#129566=DIRECTION('center_axis',(-1.4081690688991E-16,-6.98296267768627E-15,
1.));
#129567=DIRECTION('ref_axis',(-1.,7.97077743482043E-31,-1.4081690688991E-16));
#129568=DIRECTION('center_axis',(-1.4081690688991E-16,-6.98296267768627E-15,
1.));
#129569=DIRECTION('ref_axis',(-1.,7.97077743482043E-31,-1.4081690688991E-16));
#129570=DIRECTION('',(-0.499999999999998,-0.86602540378444,-6.11783152599987E-15));
#129571=DIRECTION('center_axis',(1.4081690688991E-16,6.98296267768627E-15,
-1.));
#129572=DIRECTION('ref_axis',(1.,-7.97077743482043E-31,1.4081690688991E-16));
#129573=DIRECTION('',(0.203366068089045,0.456779414654155,-0.866022406579766));
#129574=DIRECTION('center_axis',(1.4081690688991E-16,6.98296267768627E-15,
-1.));
#129575=DIRECTION('ref_axis',(-1.,-5.32907051820075E-15,-1.40816906889948E-16));
#129576=DIRECTION('',(-0.250006733496381,-0.433014808647736,0.86602240657978));
#129577=DIRECTION('center_axis',(-1.4081690688991E-16,-6.98296267768627E-15,
1.));
#129578=DIRECTION('ref_axis',(-1.,9.83319205199467E-31,-1.40816906889911E-16));
#129579=DIRECTION('center_axis',(-1.4081690688991E-16,-6.98296267768627E-15,
1.));
#129580=DIRECTION('ref_axis',(-1.,7.98248735348668E-31,-1.4081690688991E-16));
#129581=DIRECTION('',(0.406736643075798,0.913545457642602,6.43652923108483E-15));
#129582=DIRECTION('center_axis',(1.4081690688991E-16,6.98296267768627E-15,
-1.));
#129583=DIRECTION('ref_axis',(-1.,4.44089209850063E-15,-1.40816906889879E-16));
#129584=DIRECTION('',(-0.499999999999998,-0.86602540378444,-6.11783152599987E-15));
#129585=DIRECTION('center_axis',(-1.4081690688991E-16,-6.98296267768627E-15,
1.));
#129586=DIRECTION('ref_axis',(-1.,7.99150043815584E-31,-1.4081690688991E-16));
#129587=DIRECTION('center_axis',(-1.4081690688991E-16,-6.98296267768627E-15,
1.));
#129588=DIRECTION('ref_axis',(1.,-7.99370576998456E-31,1.4081690688991E-16));
#129589=DIRECTION('',(0.203374579494977,0.456775406784131,0.866022521746654));
#129590=DIRECTION('center_axis',(-1.4081690688991E-16,-6.98296267768627E-15,
1.));
#129591=DIRECTION('ref_axis',(-1.,7.99858039355471E-31,-1.4081690688991E-16));
#129592=DIRECTION('center_axis',(-1.4081690688991E-16,-6.98296267768627E-15,
1.));
#129593=DIRECTION('ref_axis',(-1.,7.99858039355471E-31,-1.4081690688991E-16));
#129594=DIRECTION('center_axis',(-1.4081690688991E-16,-6.98296267768627E-15,
1.));
#129595=DIRECTION('ref_axis',(-1.,7.99858039355471E-31,-1.4081690688991E-16));
#129596=DIRECTION('',(-0.249998488182568,-0.433019338752903,-0.866022521746651));
#129597=DIRECTION('center_axis',(-1.4081690688991E-16,-6.98296267768627E-15,
1.));
#129598=DIRECTION('ref_axis',(-1.,9.83319205199467E-31,-1.40816906889911E-16));
#129599=DIRECTION('',(0.406736643075798,0.913545457642602,6.43652923108483E-15));
#129600=DIRECTION('center_axis',(1.4081690688991E-16,6.98296267768627E-15,
-1.));
#129601=DIRECTION('ref_axis',(-1.,4.44089209850063E-15,-1.40816906889879E-16));
#129602=DIRECTION('',(-0.499999999999998,-0.86602540378444,-6.11783152599987E-15));
#129603=DIRECTION('center_axis',(-1.4081690688991E-16,-6.98296267768627E-15,
1.));
#129604=DIRECTION('ref_axis',(-1.,8.32577322149061E-31,-1.39145123902276E-16));
#129605=DIRECTION('center_axis',(-0.9131096220865,0.40771413759054,-7.8645720700241E-6));
#129606=DIRECTION('ref_axis',(-6.5840321423447E-6,4.54394095516308E-6,0.999999999968002));
#129607=DIRECTION('center_axis',(0.866560035746487,-0.499072844768372,-7.86457221102025E-6));
#129608=DIRECTION('ref_axis',(-0.423232531439977,-0.734883833187562,0.529924500330438));
#129609=DIRECTION('center_axis',(-1.4081690688991E-16,-6.98296267768627E-15,
1.));
#129610=DIRECTION('ref_axis',(-1.,8.07722881720021E-31,-1.42096112075504E-16));
#129611=DIRECTION('center_axis',(-0.913128216116196,0.407672492126938,9.77059649425398E-6));
#129612=DIRECTION('ref_axis',(0.356563044148269,0.798661963255189,-0.484769908304018));
#129613=DIRECTION('center_axis',(0.866537273133727,-0.499112366280882,9.77051914612337E-6));
#129614=DIRECTION('ref_axis',(0.436552356525903,0.757913804263692,-0.484756336026894));
#129615=DIRECTION('center_axis',(-1.4081690688991E-16,-6.98296267768627E-15,
1.));
#129616=DIRECTION('ref_axis',(-1.,8.24049048117772E-31,-1.37719829560012E-16));
#129617=DIRECTION('center_axis',(0.91459920255343,-0.404361593575297,-1.81624797483359E-5));
#129618=DIRECTION('ref_axis',(0.349880111830071,0.791348561788269,0.501349539843626));
#129619=DIRECTION('center_axis',(-0.864723333035792,0.502248501216991,-1.81316450871321E-5));
#129620=DIRECTION('ref_axis',(0.435432334017441,0.749703650685568,0.498340364250033));
#129621=DIRECTION('center_axis',(-1.4081690688991E-16,-6.98296267768627E-15,
1.));
#129622=DIRECTION('ref_axis',(-1.,8.26087817385229E-31,-1.38060560438432E-16));
#129623=DIRECTION('center_axis',(0.914604666183639,-0.404349235504512,-1.84940712939604E-5));
#129624=DIRECTION('ref_axis',(0.350555095115197,0.792949544397979,-0.498339387694583));
#129625=DIRECTION('center_axis',(-0.864716546823295,0.502260184871142,-1.85257210458366E-5));
#129626=DIRECTION('ref_axis',(0.434586366990142,0.748187385814829,-0.501348506863122));
#129627=DIRECTION('center_axis',(-1.4081690688991E-16,-6.98296267768627E-15,
1.));
#129628=DIRECTION('ref_axis',(-1.,9.83319205199467E-31,-1.40816906889911E-16));
#129629=DIRECTION('center_axis',(-1.4081690688991E-16,-6.98296267768627E-15,
1.));
#129630=DIRECTION('ref_axis',(-1.,8.46073526001725E-31,-1.4081690688991E-16));
#129631=DIRECTION('',(0.499999999999998,0.86602540378444,6.11783152599987E-15));
#129632=DIRECTION('center_axis',(-1.4081690688991E-16,-6.98296267768627E-15,
1.));
#129633=DIRECTION('ref_axis',(-1.,7.97077743482043E-31,-1.4081690688991E-16));
#129634=DIRECTION('center_axis',(-1.4081690688991E-16,-6.98296267768627E-15,
1.));
#129635=DIRECTION('ref_axis',(-1.,7.97077743482043E-31,-1.4081690688991E-16));
#129636=DIRECTION('center_axis',(-1.4081690688991E-16,-6.98296267768627E-15,
1.));
#129637=DIRECTION('ref_axis',(-1.,7.97077743482043E-31,-1.4081690688991E-16));
#129638=DIRECTION('',(-0.587785252292471,-0.809016994374949,-5.73210557847752E-15));
#129639=DIRECTION('center_axis',(1.4081690688991E-16,6.98296267768627E-15,
-1.));
#129640=DIRECTION('ref_axis',(1.,-7.97077743482043E-31,1.4081690688991E-16));
#129641=DIRECTION('',(0.24999845775561,0.433019586648882,-0.866022406579788));
#129642=DIRECTION('center_axis',(1.4081690688991E-16,6.98296267768627E-15,
-1.));
#129643=DIRECTION('ref_axis',(-1.,7.97577417048809E-31,-1.40816906889911E-16));
#129644=DIRECTION('',(-0.293899542971744,-0.404509888559955,0.866022406579768));
#129645=DIRECTION('center_axis',(-1.4081690688991E-16,-6.98296267768627E-15,
1.));
#129646=DIRECTION('ref_axis',(-1.,9.83319205199467E-31,-1.40816906889911E-16));
#129647=DIRECTION('center_axis',(-1.4081690688991E-16,-6.98296267768627E-15,
1.));
#129648=DIRECTION('ref_axis',(-1.,7.98248735348668E-31,-1.4081690688991E-16));
#129649=DIRECTION('',(0.499999999999998,0.86602540378444,6.11783152599987E-15));
#129650=DIRECTION('center_axis',(1.4081690688991E-16,6.98296267768627E-15,
-1.));
#129651=DIRECTION('ref_axis',(-1.,7.98707387273907E-31,-1.4081690688991E-16));
#129652=DIRECTION('',(-0.587785252292471,-0.809016994374949,-5.73210557847752E-15));
#129653=DIRECTION('center_axis',(-1.4081690688991E-16,-6.98296267768627E-15,
1.));
#129654=DIRECTION('ref_axis',(-1.,7.99150043815584E-31,-1.4081690688991E-16));
#129655=DIRECTION('center_axis',(-1.4081690688991E-16,-6.98296267768627E-15,
1.));
#129656=DIRECTION('ref_axis',(1.,-7.99370576998456E-31,1.4081690688991E-16));
#129657=DIRECTION('',(0.250006503598672,0.433014711050232,0.866022521746664));
#129658=DIRECTION('center_axis',(-1.4081690688991E-16,-6.98296267768627E-15,
1.));
#129659=DIRECTION('ref_axis',(-1.,7.99858039355471E-31,-1.4081690688991E-16));
#129660=DIRECTION('center_axis',(-1.4081690688991E-16,-6.98296267768627E-15,
1.));
#129661=DIRECTION('ref_axis',(-1.,7.99858039355471E-31,-1.4081690688991E-16));
#129662=DIRECTION('center_axis',(-1.4081690688991E-16,-6.98296267768627E-15,
1.));
#129663=DIRECTION('ref_axis',(-1.,7.99858039355471E-31,-1.4081690688991E-16));
#129664=DIRECTION('',(-0.293891816351551,-0.404515255718677,-0.866022521746657));
#129665=DIRECTION('center_axis',(-1.4081690688991E-16,-6.98296267768627E-15,
1.));
#129666=DIRECTION('ref_axis',(-1.,9.83319205199467E-31,-1.40816906889911E-16));
#129667=DIRECTION('',(0.499999999999998,0.86602540378444,6.11783152599987E-15));
#129668=DIRECTION('center_axis',(1.4081690688991E-16,6.98296267768627E-15,
-1.));
#129669=DIRECTION('ref_axis',(-1.,8.01265634860448E-31,-1.4081690688991E-16));
#129670=DIRECTION('',(-0.587785252292471,-0.809016994374949,-5.73210557847752E-15));
#129671=DIRECTION('center_axis',(-1.4081690688991E-16,-6.98296267768627E-15,
1.));
#129672=DIRECTION('ref_axis',(-1.,8.32577322149061E-31,-1.39145123902276E-16));
#129673=DIRECTION('center_axis',(-0.865489779781644,0.500926582476584,-7.86457211702301E-6));
#129674=DIRECTION('ref_axis',(-6.07299298703037E-6,5.20726757706905E-6,
0.999999999968002));
#129675=DIRECTION('center_axis',(0.809645611678812,-0.586919060371522,-7.86457243086484E-6));
#129676=DIRECTION('ref_axis',(-0.497730297112349,-0.686618216541007,0.529924500330471));
#129677=DIRECTION('center_axis',(-1.4081690688991E-16,-6.98296267768627E-15,
1.));
#129678=DIRECTION('ref_axis',(-1.,8.07722881720021E-31,-1.42096112075504E-16));
#129679=DIRECTION('center_axis',(-0.865512625090032,0.50088710875236,9.7705877695898E-6));
#129680=DIRECTION('ref_axis',(0.438092662174206,0.757015822392589,-0.484769908303299));
#129681=DIRECTION('center_axis',(0.809618842641174,-0.586955986037201,9.7705258656919E-6));
#129682=DIRECTION('ref_axis',(0.513384442288674,0.708129726178612,-0.484756336026824));
#129683=DIRECTION('center_axis',(-1.4081690688991E-16,-6.98296267768627E-15,
1.));
#129684=DIRECTION('ref_axis',(-1.,8.24049048117772E-31,-1.37719829560012E-16));
#129685=DIRECTION('center_axis',(0.867321636444868,-0.497748107605364,-1.81624797230982E-5));
#129686=DIRECTION('ref_axis',(0.430681881041376,0.750441041148587,0.501349539844694));
#129687=DIRECTION('center_axis',(-0.807487024129147,0.589885332530228,-1.81316452770967E-5));
#129688=DIRECTION('ref_axis',(0.511412360643298,0.700081622911464,0.498340364252085));
#129689=DIRECTION('center_axis',(-1.4081690688991E-16,-6.98296267768627E-15,
1.));
#129690=DIRECTION('ref_axis',(-1.,8.26087817385229E-31,-1.38060560438432E-16));
#129691=DIRECTION('center_axis',(0.867328361917146,-0.497736388334316,-1.84940634502467E-5));
#129692=DIRECTION('ref_axis',(0.431520514948145,0.751962698440445,-0.498339387699841));
#129693=DIRECTION('center_axis',(-0.807479053808288,0.589896242840782,-1.85256928077167E-5));
#129694=DIRECTION('ref_axis',(0.510412535077489,0.69866209193516,-0.501348506857811));
#129695=DIRECTION('center_axis',(-1.4081690688991E-16,-6.98296267768627E-15,
1.));
#129696=DIRECTION('ref_axis',(-1.,9.83319205199467E-31,-1.40816906889911E-16));
#129697=DIRECTION('center_axis',(-1.4081690688991E-16,-6.98296267768627E-15,
1.));
#129698=DIRECTION('ref_axis',(-1.,8.46073526001725E-31,-1.4081690688991E-16));
#129699=DIRECTION('',(0.587785252292471,0.809016994374949,5.73210557847752E-15));
#129700=DIRECTION('center_axis',(-1.4081690688991E-16,-6.98296267768627E-15,
1.));
#129701=DIRECTION('ref_axis',(-1.,7.97077743482043E-31,-1.4081690688991E-16));
#129702=DIRECTION('center_axis',(-1.4081690688991E-16,-6.98296267768627E-15,
1.));
#129703=DIRECTION('ref_axis',(-1.,7.97077743482043E-31,-1.4081690688991E-16));
#129704=DIRECTION('center_axis',(-1.4081690688991E-16,-6.98296267768627E-15,
1.));
#129705=DIRECTION('ref_axis',(-1.,7.97077743482043E-31,-1.4081690688991E-16));
#129706=DIRECTION('',(-0.669130606358857,-0.743144825477395,-5.28357748271715E-15));
#129707=DIRECTION('center_axis',(1.4081690688991E-16,6.98296267768627E-15,
-1.));
#129708=DIRECTION('ref_axis',(1.,-7.97077743482043E-31,1.4081690688991E-16));
#129709=DIRECTION('',(0.293891812003452,0.404515505437167,-0.866022406579784));
#129710=DIRECTION('center_axis',(1.4081690688991E-16,6.98296267768627E-15,
-1.));
#129711=DIRECTION('ref_axis',(-1.,7.97577417048809E-31,-1.40816906889911E-16));
#129712=DIRECTION('',(-0.334572327551836,-0.371573073483925,0.866022406579793));
#129713=DIRECTION('center_axis',(-1.4081690688991E-16,-6.98296267768627E-15,
1.));
#129714=DIRECTION('ref_axis',(-1.,9.83319205199467E-31,-1.40816906889911E-16));
#129715=DIRECTION('center_axis',(-1.4081690688991E-16,-6.98296267768627E-15,
1.));
#129716=DIRECTION('ref_axis',(-1.,7.98248735348668E-31,-1.4081690688991E-16));
#129717=DIRECTION('',(0.587785252292471,0.809016994374949,5.73210557847752E-15));
#129718=DIRECTION('center_axis',(1.4081690688991E-16,6.98296267768627E-15,
-1.));
#129719=DIRECTION('ref_axis',(-1.,7.98707387273907E-31,-1.4081690688991E-16));
#129720=DIRECTION('',(-0.669130606358857,-0.743144825477395,-5.28357748271715E-15));
#129721=DIRECTION('center_axis',(-1.4081690688991E-16,-6.98296267768627E-15,
1.));
#129722=DIRECTION('ref_axis',(-1.,7.99150043815584E-31,-1.4081690688991E-16));
#129723=DIRECTION('center_axis',(-1.4081690688991E-16,-6.98296267768627E-15,
1.));
#129724=DIRECTION('ref_axis',(1.,-7.99370576998456E-31,1.4081690688991E-16));
#129725=DIRECTION('',(0.293899304131716,0.404509815527969,0.866022521746647));
#129726=DIRECTION('center_axis',(-1.4081690688991E-16,-6.98296267768627E-15,
1.));
#129727=DIRECTION('ref_axis',(-1.,7.99858039355471E-31,-1.4081690688991E-16));
#129728=DIRECTION('center_axis',(-1.4081690688991E-16,-6.98296267768627E-15,
1.));
#129729=DIRECTION('ref_axis',(-1.,7.99858039355471E-31,-1.4081690688991E-16));
#129730=DIRECTION('center_axis',(-1.4081690688991E-16,-6.98296267768627E-15,
1.));
#129731=DIRECTION('ref_axis',(-1.,7.99858039355471E-31,-1.4081690688991E-16));
#129732=DIRECTION('',(-0.334565204279747,-0.371579218892574,-0.866022521746655));
#129733=DIRECTION('center_axis',(-1.4081690688991E-16,-6.98296267768627E-15,
1.));
#129734=DIRECTION('ref_axis',(-1.,9.83319205199467E-31,-1.40816906889911E-16));
#129735=DIRECTION('',(0.587785252292471,0.809016994374949,5.73210557847752E-15));
#129736=DIRECTION('center_axis',(1.4081690688991E-16,6.98296267768627E-15,
-1.));
#129737=DIRECTION('ref_axis',(-1.,8.01265634860448E-31,-1.4081690688991E-16));
#129738=DIRECTION('',(-0.669130606358857,-0.743144825477395,-5.28357748271715E-15));
#129739=DIRECTION('center_axis',(-1.4081690688991E-16,-6.98296267768627E-15,
1.));
#129740=DIRECTION('ref_axis',(-1.,8.32577322149061E-31,-1.39145123902276E-16));
#129741=DIRECTION('center_axis',(-0.808387450334232,0.588650770899239,-7.86457176580283E-6));
#129742=DIRECTION('ref_axis',(-5.49541651871241E-6,5.81354205727288E-6,
0.999999999968002));
#129743=DIRECTION('center_axis',(0.743860540860255,-0.668334867928674,-7.8645722585724E-6));
#129744=DIRECTION('ref_axis',(-0.566774825493092,-0.630829867029758,0.529924500330465));
#129745=DIRECTION('center_axis',(-1.4081690688991E-16,-6.98296267768627E-15,
1.));
#129746=DIRECTION('ref_axis',(-1.,8.07722881720021E-31,-1.42096112075504E-16));
#129747=DIRECTION('center_axis',(-0.808414296620484,0.588613901402391,9.77059021400816E-6));
#129748=DIRECTION('ref_axis',(0.514822445316503,0.70707565776395,-0.484769908302912));
#129749=DIRECTION('center_axis',(0.74383005867795,-0.668368793191075,9.77051183441469E-6));
#129750=DIRECTION('ref_axis',(0.584591780669533,0.650587230628282,-0.484756336025686));
#129751=DIRECTION('center_axis',(-1.4081690688991E-16,-6.98296267768627E-15,
1.));
#129752=DIRECTION('ref_axis',(-1.,8.24049048117772E-31,-1.37719829560012E-16));
#129753=DIRECTION('center_axis',(0.810541512988639,-0.585681189208098,-1.81624797439544E-5));
#129754=DIRECTION('ref_axis',(0.50676500943756,0.701311531421608,0.501349539847031));
#129755=DIRECTION('center_axis',(-0.741403718408824,0.671059256698552,-1.81316450741316E-5));
#129756=DIRECTION('ref_axis',(0.581789246426899,0.642789354376716,0.498340364251167));
#129757=DIRECTION('center_axis',(-1.4081690688991E-16,-6.98296267768627E-15,
1.));
#129758=DIRECTION('ref_axis',(-1.,8.26087817385229E-31,-1.38060560438432E-16));
#129759=DIRECTION('center_axis',(0.810549426613657,-0.585670237142235,-1.84940689245547E-5));
#129760=DIRECTION('ref_axis',(0.507758105718737,0.702737191802679,-0.498339387700997));
#129761=DIRECTION('center_axis',(-0.741394651315224,0.671069274112574,-1.85257009851561E-5));
#129762=DIRECTION('ref_axis',(0.580646516616596,0.641482109967114,-0.501348506862394));
#129763=DIRECTION('center_axis',(-1.4081690688991E-16,-6.98296267768627E-15,
1.));
#129764=DIRECTION('ref_axis',(-1.,9.83319205199467E-31,-1.40816906889911E-16));
#129765=DIRECTION('center_axis',(-1.4081690688991E-16,-6.98296267768627E-15,
1.));
#129766=DIRECTION('ref_axis',(-1.,8.46073526001725E-31,-1.4081690688991E-16));
#129767=DIRECTION('',(0.669130606358857,0.743144825477395,5.28357748271715E-15));
#129768=DIRECTION('center_axis',(-1.4081690688991E-16,-6.98296267768627E-15,
1.));
#129769=DIRECTION('ref_axis',(-1.,7.97077743482043E-31,-1.4081690688991E-16));
#129770=DIRECTION('center_axis',(-1.4081690688991E-16,-6.98296267768627E-15,
1.));
#129771=DIRECTION('ref_axis',(-1.,7.97077743482043E-31,-1.4081690688991E-16));
#129772=DIRECTION('center_axis',(-1.4081690688991E-16,-6.98296267768627E-15,
1.));
#129773=DIRECTION('ref_axis',(-1.,7.97077743482043E-31,-1.4081690688991E-16));
#129774=DIRECTION('',(-0.743144825477393,-0.669130606358859,-4.77716140639646E-15));
#129775=DIRECTION('center_axis',(1.4081690688991E-16,6.98296267768627E-15,
-1.));
#129776=DIRECTION('ref_axis',(1.,-7.97077743482043E-31,1.4081690688991E-16));
#129777=DIRECTION('',(0.334565226058181,0.371579467697516,-0.8660224065798));
#129778=DIRECTION('center_axis',(1.4081690688991E-16,6.98296267768627E-15,
-1.));
#129779=DIRECTION('ref_axis',(-1.,7.97577417048809E-31,-1.40816906889911E-16));
#129780=DIRECTION('',(-0.371579467697537,-0.334565226058201,0.866022406579784));
#129781=DIRECTION('center_axis',(-1.4081690688991E-16,-6.98296267768627E-15,
1.));
#129782=DIRECTION('ref_axis',(-1.,9.83319205199467E-31,-1.40816906889911E-16));
#129783=DIRECTION('center_axis',(-1.4081690688991E-16,-6.98296267768627E-15,
1.));
#129784=DIRECTION('ref_axis',(-1.,7.98248735348668E-31,-1.4081690688991E-16));
#129785=DIRECTION('',(0.669130606358857,0.743144825477395,5.28357748271715E-15));
#129786=DIRECTION('center_axis',(1.4081690688991E-16,6.98296267768627E-15,
-1.));
#129787=DIRECTION('ref_axis',(-1.,7.98707387273907E-31,-1.4081690688991E-16));
#129788=DIRECTION('',(-0.743144825477393,-0.669130606358859,-4.77716140639646E-15));
#129789=DIRECTION('center_axis',(-1.4081690688991E-16,-6.98296267768627E-15,
1.));
#129790=DIRECTION('ref_axis',(-1.,7.99150043815584E-31,-1.4081690688991E-16));
#129791=DIRECTION('center_axis',(-1.4081690688991E-16,-6.98296267768627E-15,
1.));
#129792=DIRECTION('ref_axis',(1.,8.88178419700124E-16,1.40816906889917E-16));
#129793=DIRECTION('',(0.334572082386297,0.3715730258176,0.866022521746663));
#129794=DIRECTION('center_axis',(-1.4081690688991E-16,-6.98296267768627E-15,
1.));
#129795=DIRECTION('ref_axis',(-1.,7.99858039355471E-31,-1.4081690688991E-16));
#129796=DIRECTION('center_axis',(-1.4081690688991E-16,-6.98296267768627E-15,
1.));
#129797=DIRECTION('ref_axis',(-1.,7.99858039355471E-31,-1.4081690688991E-16));
#129798=DIRECTION('center_axis',(-1.4081690688991E-16,-6.98296267768627E-15,
1.));
#129799=DIRECTION('ref_axis',(-1.,7.99858039355471E-31,-1.4081690688991E-16));
#129800=DIRECTION('',(-0.371573025817624,-0.334572082386294,-0.866022521746654));
#129801=DIRECTION('center_axis',(-1.4081690688991E-16,-6.98296267768627E-15,
1.));
#129802=DIRECTION('ref_axis',(-1.,9.83319205199467E-31,-1.40816906889911E-16));
#129803=DIRECTION('',(0.669130606358857,0.743144825477395,5.28357748271715E-15));
#129804=DIRECTION('center_axis',(1.4081690688991E-16,6.98296267768627E-15,
-1.));
#129805=DIRECTION('ref_axis',(-1.,1.06581410364015E-14,-1.40816906889836E-16));
#129806=DIRECTION('',(-0.743144825477393,-0.669130606358859,-4.77716140639646E-15));
#129807=DIRECTION('center_axis',(-1.4081690688991E-16,-6.98296267768627E-15,
1.));
#129808=DIRECTION('ref_axis',(-1.,8.32577322149061E-31,-1.39145123902276E-16));
#129809=DIRECTION('center_axis',(-0.742428258814693,0.66992557829324,-7.8645722868831E-6));
#129810=DIRECTION('ref_axis',(-4.85763186827067E-6,6.35612260159829E-6,
0.999999999968001));
#129811=DIRECTION('center_axis',(0.669925578293297,-0.742428258814641,-7.8645724034394E-6));
#129812=DIRECTION('ref_axis',(-0.629609650280272,-0.568130013485873,0.529924500330467));
#129813=DIRECTION('center_axis',(-1.4081690688991E-16,-6.98296267768627E-15,
1.));
#129814=DIRECTION('ref_axis',(-1.,8.07722881720021E-31,-1.42096112075504E-16));
#129815=DIRECTION('center_axis',(-0.742458811943861,0.669891716974801,9.77059652327666E-6));
#129816=DIRECTION('ref_axis',(0.585911726014692,0.649388624263867,-0.484769908302039));
#129817=DIRECTION('center_axis',(0.669891716946153,-0.742458811969709,9.77052689495564E-6));
#129818=DIRECTION('ref_axis',(0.649394209166457,0.585916765233755,-0.484756336027786));
#129819=DIRECTION('center_axis',(-1.4081690688991E-16,-6.98296267768627E-15,
1.));
#129820=DIRECTION('ref_axis',(-1.,8.24049048117772E-31,-1.37719829560012E-16));
#129821=DIRECTION('center_axis',(0.744880927099454,-0.667197425140102,-1.81624797771564E-5));
#129822=DIRECTION('ref_axis',(0.577295914345283,0.644498305800666,0.501349539842528));
#129823=DIRECTION('center_axis',(-0.667197438400621,0.744880915222623,-1.81316453516109E-5));
#129824=DIRECTION('ref_axis',(0.64579192747986,0.578454551163167,0.498340364249643));
#129825=DIRECTION('center_axis',(-1.4081690688991E-16,-6.98296267768627E-15,
1.));
#129826=DIRECTION('ref_axis',(-1.,8.26087817385229E-31,-1.38060560438432E-16));
#129827=DIRECTION('center_axis',(0.744889942174867,-0.667187360270481,-1.84940703591896E-5));
#129828=DIRECTION('ref_axis',(0.578432592428572,0.645812349435392,-0.498339387699889));
#129829=DIRECTION('center_axis',(-0.667187373871816,0.744889929991558,-1.85256986638901E-5));
#129830=DIRECTION('ref_axis',(0.644518813413593,0.57727391576619,-0.501348506861149));
#129831=DIRECTION('center_axis',(-1.4081690688991E-16,-6.98296267768627E-15,
1.));
#129832=DIRECTION('ref_axis',(-1.,9.83319205199467E-31,-1.40816906889911E-16));
#129833=DIRECTION('center_axis',(-1.4081690688991E-16,-6.98296267768627E-15,
1.));
#129834=DIRECTION('ref_axis',(-1.,8.46073526001725E-31,-1.4081690688991E-16));
#129835=DIRECTION('',(0.743144825477393,0.669130606358859,4.77716140639646E-15));
#129836=DIRECTION('center_axis',(-1.4081690688991E-16,-6.98296267768627E-15,
1.));
#129837=DIRECTION('ref_axis',(-1.,7.97077743482043E-31,-1.4081690688991E-16));
#129838=DIRECTION('center_axis',(-1.4081690688991E-16,-6.98296267768627E-15,
1.));
#129839=DIRECTION('ref_axis',(-1.,7.97077743482043E-31,-1.4081690688991E-16));
#129840=DIRECTION('center_axis',(-1.4081690688991E-16,-6.98296267768627E-15,
1.));
#129841=DIRECTION('ref_axis',(-1.,7.97077743482043E-31,-1.4081690688991E-16));
#129842=DIRECTION('',(-0.809016994374947,-0.587785252292474,-4.21840575002201E-15));
#129843=DIRECTION('center_axis',(1.4081690688991E-16,6.98296267768627E-15,
-1.));
#129844=DIRECTION('ref_axis',(1.,-7.97077743482043E-31,1.4081690688991E-16));
#129845=DIRECTION('',(0.3715730734839,0.334572327551839,-0.866022406579802));
#129846=DIRECTION('center_axis',(1.4081690688991E-16,6.98296267768627E-15,
-1.));
#129847=DIRECTION('ref_axis',(-1.,7.97577417048809E-31,-1.40816906889911E-16));
#129848=DIRECTION('',(-0.40451550543717,-0.293891812003427,0.866022406579791));
#129849=DIRECTION('center_axis',(-1.4081690688991E-16,-6.98296267768627E-15,
1.));
#129850=DIRECTION('ref_axis',(-1.,9.83319205199467E-31,-1.40816906889911E-16));
#129851=DIRECTION('center_axis',(-1.4081690688991E-16,-6.98296267768627E-15,
1.));
#129852=DIRECTION('ref_axis',(-1.,7.98248735348668E-31,-1.4081690688991E-16));
#129853=DIRECTION('',(0.743144825477393,0.669130606358859,4.77716140639646E-15));
#129854=DIRECTION('center_axis',(1.4081690688991E-16,6.98296267768627E-15,
-1.));
#129855=DIRECTION('ref_axis',(-1.,7.98707387273907E-31,-1.4081690688991E-16));
#129856=DIRECTION('',(-0.809016994374947,-0.587785252292474,-4.21840575002201E-15));
#129857=DIRECTION('center_axis',(-1.4081690688991E-16,-6.98296267768627E-15,
1.));
#129858=DIRECTION('ref_axis',(-1.,7.99150043815584E-31,-1.4081690688991E-16));
#129859=DIRECTION('center_axis',(-1.4081690688991E-16,-6.98296267768627E-15,
1.));
#129860=DIRECTION('ref_axis',(1.,-7.99370576998456E-31,1.4081690688991E-16));
#129861=DIRECTION('',(0.37157921889255,0.33456520427975,0.866022521746664));
#129862=DIRECTION('center_axis',(-1.4081690688991E-16,-6.98296267768627E-15,
1.));
#129863=DIRECTION('ref_axis',(-1.,7.99858039355471E-31,-1.4081690688991E-16));
#129864=DIRECTION('center_axis',(-1.4081690688991E-16,-6.98296267768627E-15,
1.));
#129865=DIRECTION('ref_axis',(-1.,7.99858039355471E-31,-1.4081690688991E-16));
#129866=DIRECTION('center_axis',(-1.4081690688991E-16,-6.98296267768627E-15,
1.));
#129867=DIRECTION('ref_axis',(-1.,7.99858039355471E-31,-1.4081690688991E-16));
#129868=DIRECTION('',(-0.404509815527948,-0.293899304131707,-0.86602252174666));
#129869=DIRECTION('center_axis',(-1.4081690688991E-16,-6.98296267768627E-15,
1.));
#129870=DIRECTION('ref_axis',(-1.,9.83319205199467E-31,-1.40816906889911E-16));
#129871=DIRECTION('',(0.743144825477393,0.669130606358859,4.77716140639646E-15));
#129872=DIRECTION('center_axis',(1.4081690688991E-16,6.98296267768627E-15,
-1.));
#129873=DIRECTION('ref_axis',(-1.,1.06581410364015E-14,-1.40816906889836E-16));
#129874=DIRECTION('',(-0.809016994374947,-0.587785252292474,-4.21840575002201E-15));
#129875=DIRECTION('center_axis',(-1.4081690688991E-16,-6.98296267768627E-15,
1.));
#129876=DIRECTION('ref_axis',(-1.,8.32577322149061E-31,-1.39145123902276E-16));
#129877=DIRECTION('center_axis',(-0.668334867928916,0.743860540860037,-7.86457174434936E-6));
#129878=DIRECTION('ref_axis',(-4.16662513155882E-6,6.82906352319985E-6,
0.999999999968002));
#129879=DIRECTION('center_axis',(0.588650770899605,-0.808387450333965,-7.86457259917611E-6));
#129880=DIRECTION('ref_axis',(-0.68554633998471,-0.499205608625405,0.529924500330479));
#129881=DIRECTION('center_axis',(-1.4081690688991E-16,-6.98296267768627E-15,
1.));
#129882=DIRECTION('ref_axis',(-1.,8.07722881720021E-31,-1.42096112075504E-16));
#129883=DIRECTION('center_axis',(-0.668368793156571,0.743830058708953,9.77059567102182E-6));
#129884=DIRECTION('ref_axis',(0.650581635231353,0.584586753101783,-0.484769908304563));
#129885=DIRECTION('center_axis',(0.58861390137142,-0.808414296643035,9.77052095728339E-6));
#129886=DIRECTION('ref_axis',(0.707081738813595,0.51482687314892,-0.484756336028781));
#129887=DIRECTION('center_axis',(-1.4081690688991E-16,-6.98296267768627E-15,
1.));
#129888=DIRECTION('ref_axis',(-1.,8.24049048117772E-31,-1.37719829560012E-16));
#129889=DIRECTION('center_axis',(0.671059269896725,-0.74140370646214,-1.81624800062407E-5));
#129890=DIRECTION('ref_axis',(0.64150184440888,0.58062382187108,0.501349539838051));
#129891=DIRECTION('center_axis',(-0.585681203637433,0.810541502562979,-1.81316453546949E-5));
#129892=DIRECTION('ref_axis',(0.702719177033075,0.507782078836375,0.498340364251751));
#129893=DIRECTION('center_axis',(-1.4081690688991E-16,-6.98296267768627E-15,
1.));
#129894=DIRECTION('ref_axis',(-1.,8.26087817385229E-31,-1.38060560438432E-16));
#129895=DIRECTION('center_axis',(0.671069287653591,-0.741394639059436,-1.84940662719067E-5));
#129896=DIRECTION('ref_axis',(0.642769650610767,0.581811851822409,-0.498339387699479));
#129897=DIRECTION('center_axis',(-0.585670251949389,0.810549415913883,-1.85257117335253E-5));
#129898=DIRECTION('ref_axis',(0.701329627215442,0.506740987740792,-0.501348506862578));
#129899=DIRECTION('center_axis',(-1.4081690688991E-16,-6.98296267768627E-15,
1.));
#129900=DIRECTION('ref_axis',(-1.,9.83319205199467E-31,-1.40816906889911E-16));
#129901=DIRECTION('center_axis',(-1.4081690688991E-16,-6.98296267768627E-15,
1.));
#129902=DIRECTION('ref_axis',(-1.,8.46073526001725E-31,-1.4081690688991E-16));
#129903=DIRECTION('',(0.809016994374947,0.587785252292474,4.21840575002201E-15));
#129904=DIRECTION('center_axis',(-1.4081690688991E-16,-6.98296267768627E-15,
1.));
#129905=DIRECTION('ref_axis',(-1.,7.97077743482043E-31,-1.4081690688991E-16));
#129906=DIRECTION('center_axis',(-1.4081690688991E-16,-6.98296267768627E-15,
1.));
#129907=DIRECTION('ref_axis',(-1.,7.97077743482043E-31,-1.4081690688991E-16));
#129908=DIRECTION('center_axis',(-1.4081690688991E-16,-6.98296267768627E-15,
1.));
#129909=DIRECTION('ref_axis',(-1.,7.97077743482043E-31,-1.4081690688991E-16));
#129910=DIRECTION('',(-0.866025403784438,-0.500000000000001,-3.61343235749215E-15));
#129911=DIRECTION('center_axis',(1.4081690688991E-16,6.98296267768627E-15,
-1.));
#129912=DIRECTION('ref_axis',(1.,-7.97077743482043E-31,1.4081690688991E-16));
#129913=DIRECTION('',(0.404509888559913,0.293899542971726,-0.866022406579794));
#129914=DIRECTION('center_axis',(1.4081690688991E-16,6.98296267768627E-15,
-1.));
#129915=DIRECTION('ref_axis',(-1.,7.97577417048809E-31,-1.40816906889911E-16));
#129916=DIRECTION('',(-0.433019586648905,-0.249998457755607,0.866022406579778));
#129917=DIRECTION('center_axis',(-1.4081690688991E-16,-6.98296267768627E-15,
1.));
#129918=DIRECTION('ref_axis',(-1.,9.83319205199467E-31,-1.40816906889911E-16));
#129919=DIRECTION('center_axis',(-1.4081690688991E-16,-6.98296267768627E-15,
1.));
#129920=DIRECTION('ref_axis',(-1.,7.98248735348668E-31,-1.4081690688991E-16));
#129921=DIRECTION('',(0.809016994374947,0.587785252292474,4.21840575002201E-15));
#129922=DIRECTION('center_axis',(1.4081690688991E-16,6.98296267768627E-15,
-1.));
#129923=DIRECTION('ref_axis',(-1.,7.98707387273907E-31,-1.4081690688991E-16));
#129924=DIRECTION('',(-0.866025403784438,-0.500000000000001,-3.61343235749215E-15));
#129925=DIRECTION('center_axis',(-1.4081690688991E-16,-6.98296267768627E-15,
1.));
#129926=DIRECTION('ref_axis',(-1.,7.99150043815584E-31,-1.4081690688991E-16));
#129927=DIRECTION('center_axis',(-1.4081690688991E-16,-6.98296267768627E-15,
1.));
#129928=DIRECTION('ref_axis',(1.,-7.99370576998456E-31,1.4081690688991E-16));
#129929=DIRECTION('',(0.40451525571868,0.293891816351526,0.866022521746664));
#129930=DIRECTION('center_axis',(-1.4081690688991E-16,-6.98296267768627E-15,
1.));
#129931=DIRECTION('ref_axis',(-1.,7.99858039355471E-31,-1.4081690688991E-16));
#129932=DIRECTION('center_axis',(-1.4081690688991E-16,-6.98296267768627E-15,
1.));
#129933=DIRECTION('ref_axis',(-1.,7.99858039355471E-31,-1.4081690688991E-16));
#129934=DIRECTION('center_axis',(-1.4081690688991E-16,-6.98296267768627E-15,
1.));
#129935=DIRECTION('ref_axis',(-1.,7.99858039355471E-31,-1.4081690688991E-16));
#129936=DIRECTION('',(-0.433014711050233,-0.250006503598672,-0.866022521746663));
#129937=DIRECTION('center_axis',(-1.4081690688991E-16,-6.98296267768627E-15,
1.));
#129938=DIRECTION('ref_axis',(-1.,9.83319205199467E-31,-1.40816906889911E-16));
#129939=DIRECTION('',(0.809016994374947,0.587785252292474,4.21840575002201E-15));
#129940=DIRECTION('center_axis',(1.4081690688991E-16,6.98296267768627E-15,
-1.));
#129941=DIRECTION('ref_axis',(-1.,1.24344978758018E-14,-1.40816906889824E-16));
#129942=DIRECTION('',(-0.866025403784438,-0.500000000000001,-3.61343235749215E-15));
#129943=DIRECTION('center_axis',(-1.4081690688991E-16,-6.98296267768627E-15,
1.));
#129944=DIRECTION('ref_axis',(-1.,8.32577322149061E-31,-1.39145123902276E-16));
#129945=DIRECTION('center_axis',(-0.586919060371807,0.809645611678606,-7.86457181291262E-6));
#129946=DIRECTION('ref_axis',(-3.4299684487921E-6,7.2271841840149E-6,0.999999999968002));
#129947=DIRECTION('center_axis',(0.500926582476734,-0.865489779781557,-7.86457237844701E-6));
#129948=DIRECTION('ref_axis',(-0.733972040528689,-0.424811802651091,0.529924500330455));
#129949=DIRECTION('center_axis',(-1.4081690688991E-16,-6.98296267768627E-15,
1.));
#129950=DIRECTION('ref_axis',(-1.,8.07722881720021E-31,-1.42096112075504E-16));
#129951=DIRECTION('center_axis',(-0.586955986007611,0.809618842662625,9.77059194293215E-6));
#129952=DIRECTION('ref_axis',(0.708123635910574,0.513380027141175,-0.484769908304254));
#129953=DIRECTION('center_axis',(0.500887108717654,-0.865512625110117,9.77051538527543E-6));
#129954=DIRECTION('ref_axis',(0.757022332966266,0.438096430108902,-0.484756336024758));
#129955=DIRECTION('center_axis',(-1.4081690688991E-16,-6.98296267768627E-15,
1.));
#129956=DIRECTION('ref_axis',(-1.,8.24049048117772E-31,-1.37719829560012E-16));
#129957=DIRECTION('center_axis',(0.589885346904554,-0.807487013627723,-1.81624797025065E-5));
#129958=DIRECTION('ref_axis',(0.698679346016,0.510387901840437,0.50134953984777));
#129959=DIRECTION('center_axis',(-0.497748123045552,0.867321627584527,-1.81316453185413E-5));
#129960=DIRECTION('ref_axis',(0.75194728823168,0.431546239795302,0.498340364248732));
#129961=DIRECTION('center_axis',(-1.4081690688991E-16,-6.98296267768627E-15,
1.));
#129962=DIRECTION('ref_axis',(-1.,8.26087817385229E-31,-1.38060560438432E-16));
#129963=DIRECTION('center_axis',(0.589896257574276,-0.807479043045597,-1.84940891229696E-5));
#129964=DIRECTION('ref_axis',(0.700064389991712,0.511436901808062,-0.498339387701296));
#129965=DIRECTION('center_axis',(-0.497736404184271,0.867328352820608,-1.85257173268874E-5));
#129966=DIRECTION('ref_axis',(0.75045652685783,0.430656099410795,-0.501348506865995));
#129967=DIRECTION('center_axis',(-1.4081690688991E-16,-6.98296267768627E-15,
1.));
#129968=DIRECTION('ref_axis',(-1.,9.83319205199467E-31,-1.40816906889911E-16));
#129969=DIRECTION('center_axis',(-1.4081690688991E-16,-6.98296267768627E-15,
1.));
#129970=DIRECTION('ref_axis',(-1.,8.46073526001725E-31,-1.4081690688991E-16));
#129971=DIRECTION('',(0.866025403784438,0.500000000000001,3.61343235749215E-15));
#129972=DIRECTION('center_axis',(-1.4081690688991E-16,-6.98296267768627E-15,
1.));
#129973=DIRECTION('ref_axis',(-1.,7.97077743482043E-31,-1.4081690688991E-16));
#129974=DIRECTION('center_axis',(-1.4081690688991E-16,-6.98296267768627E-15,
1.));
#129975=DIRECTION('ref_axis',(-1.,7.97077743482043E-31,-1.4081690688991E-16));
#129976=DIRECTION('center_axis',(-1.4081690688991E-16,-6.98296267768627E-15,
1.));
#129977=DIRECTION('ref_axis',(-1.,7.97077743482043E-31,-1.4081690688991E-16));
#129978=DIRECTION('',(-0.913545457642601,-0.406736643075801,-2.96886944389428E-15));
#129979=DIRECTION('center_axis',(1.4081690688991E-16,6.98296267768627E-15,
-1.));
#129980=DIRECTION('ref_axis',(1.,-7.97077743482043E-31,1.4081690688991E-16));
#129981=DIRECTION('',(0.43301480864772,0.250006733496374,-0.86602240657979));
#129982=DIRECTION('center_axis',(1.4081690688991E-16,6.98296267768627E-15,
-1.));
#129983=DIRECTION('ref_axis',(-1.,7.97577417048809E-31,-1.40816906889911E-16));
#129984=DIRECTION('',(-0.456779414654134,-0.203366068089034,0.866022406579779));
#129985=DIRECTION('center_axis',(-1.4081690688991E-16,-6.98296267768627E-15,
1.));
#129986=DIRECTION('ref_axis',(-1.,9.83319205199467E-31,-1.40816906889911E-16));
#129987=DIRECTION('center_axis',(-1.4081690688991E-16,-6.98296267768627E-15,
1.));
#129988=DIRECTION('ref_axis',(-1.,7.98248735348668E-31,-1.4081690688991E-16));
#129989=DIRECTION('',(0.866025403784438,0.500000000000001,3.61343235749215E-15));
#129990=DIRECTION('center_axis',(1.4081690688991E-16,6.98296267768627E-15,
-1.));
#129991=DIRECTION('ref_axis',(-1.,-1.24344978758018E-14,-1.40816906889997E-16));
#129992=DIRECTION('',(-0.913545457642601,-0.406736643075801,-2.96886944389428E-15));
#129993=DIRECTION('center_axis',(-1.4081690688991E-16,-6.98296267768627E-15,
1.));
#129994=DIRECTION('ref_axis',(-1.,7.99150043815584E-31,-1.4081690688991E-16));
#129995=DIRECTION('center_axis',(-1.4081690688991E-16,-6.98296267768627E-15,
1.));
#129996=DIRECTION('ref_axis',(1.,-7.99370576998456E-31,1.4081690688991E-16));
#129997=DIRECTION('',(0.433019338752905,0.249998488182556,0.866022521746654));
#129998=DIRECTION('center_axis',(-1.4081690688991E-16,-6.98296267768627E-15,
1.));
#129999=DIRECTION('ref_axis',(-1.,7.99858039355471E-31,-1.4081690688991E-16));
#130000=DIRECTION('center_axis',(-1.4081690688991E-16,-6.98296267768627E-15,
1.));
#130001=DIRECTION('ref_axis',(-1.,7.99858039355471E-31,-1.4081690688991E-16));
#130002=DIRECTION('center_axis',(-1.4081690688991E-16,-6.98296267768627E-15,
1.));
#130003=DIRECTION('ref_axis',(-1.,7.99858039355471E-31,-1.4081690688991E-16));
#130004=DIRECTION('',(-0.456775406784136,-0.203374579494979,-0.86602252174665));
#130005=DIRECTION('center_axis',(-1.4081690688991E-16,-6.98296267768627E-15,
1.));
#130006=DIRECTION('ref_axis',(-1.,9.83319205199467E-31,-1.40816906889911E-16));
#130007=DIRECTION('',(0.866025403784438,0.500000000000001,3.61343235749215E-15));
#130008=DIRECTION('center_axis',(1.4081690688991E-16,6.98296267768627E-15,
-1.));
#130009=DIRECTION('ref_axis',(-1.,8.01265634860448E-31,-1.4081690688991E-16));
#130010=DIRECTION('',(-0.913545457642601,-0.406736643075801,-2.96886944389428E-15));
#130011=DIRECTION('center_axis',(-1.4081690688991E-16,-6.98296267768627E-15,
1.));
#130012=DIRECTION('ref_axis',(-1.,8.32577322149061E-31,-1.39145123902276E-16));
#130013=DIRECTION('center_axis',(-0.499072844768457,0.866560035746438,-7.86457193853739E-6));
#130014=DIRECTION('ref_axis',(-2.65573230665241E-6,7.54612235481617E-6,
0.999999999968002));
#130015=DIRECTION('center_axis',(0.4077141375907,-0.913109622086428,-7.86457248217639E-6));
#130016=DIRECTION('ref_axis',(-0.774356189802968,-0.34576366966955,0.529924500330449));
#130017=DIRECTION('center_axis',(-1.4081690688991E-16,-6.98296267768627E-15,
1.));
#130018=DIRECTION('ref_axis',(-1.,8.07722881720021E-31,-1.42096112075504E-16));
#130019=DIRECTION('center_axis',(-0.499112366248239,0.866537273152528,9.77058724011587E-6));
#130020=DIRECTION('ref_axis',(0.757907285850955,0.436548602171837,-0.484769908302748));
#130021=DIRECTION('center_axis',(0.407672492086805,-0.913128216134115,9.77051721567626E-6));
#130022=DIRECTION('ref_axis',(0.798668832019429,0.356566110901419,-0.484756336026007));
#130023=DIRECTION('center_axis',(-1.4081690688991E-16,-6.98296267768627E-15,
1.));
#130024=DIRECTION('ref_axis',(-1.,8.24049048117772E-31,-1.37719829560012E-16));
#130025=DIRECTION('center_axis',(0.502248516610505,-0.864723324094286,-1.81624798863006E-5));
#130026=DIRECTION('ref_axis',(0.74820197050765,0.434560065157462,0.50134953984103));
#130027=DIRECTION('center_axis',(-0.40436160985703,0.91459919535558,-1.81316453178961E-5));
#130028=DIRECTION('ref_axis',(0.792936907585205,0.350582289843673,0.498340364246343));
#130029=DIRECTION('center_axis',(-1.4081690688991E-16,-6.98296267768627E-15,
1.));
#130030=DIRECTION('ref_axis',(-1.,8.26087817385229E-31,-1.38060560438432E-16));
#130031=DIRECTION('center_axis',(0.502260200678538,-0.864716537642437,-1.84940579829993E-5));
#130032=DIRECTION('ref_axis',(0.74968907742253,0.435458542075418,-0.498339387693675));
#130033=DIRECTION('center_axis',(-0.404349252215686,0.914604658794943,-1.85257198772365E-5));
#130034=DIRECTION('ref_axis',(0.791361267751807,0.349852852736935,-0.501348506863321));
#130035=DIRECTION('center_axis',(-1.4081690688991E-16,-6.98296267768627E-15,
1.));
#130036=DIRECTION('ref_axis',(-1.,9.83319205199467E-31,-1.40816906889911E-16));
#130037=DIRECTION('center_axis',(-1.4081690688991E-16,-6.98296267768627E-15,
1.));
#130038=DIRECTION('ref_axis',(-1.,8.46073526001725E-31,-1.4081690688991E-16));
#130039=DIRECTION('',(0.913545457642601,0.406736643075801,2.96886944389428E-15));
#130040=DIRECTION('center_axis',(-1.4081690688991E-16,-6.98296267768627E-15,
1.));
#130041=DIRECTION('ref_axis',(-1.,7.97077743482043E-31,-1.4081690688991E-16));
#130042=DIRECTION('center_axis',(-1.4081690688991E-16,-6.98296267768627E-15,
1.));
#130043=DIRECTION('ref_axis',(-1.,7.97077743482043E-31,-1.4081690688991E-16));
#130044=DIRECTION('center_axis',(-1.4081690688991E-16,-6.98296267768627E-15,
1.));
#130045=DIRECTION('ref_axis',(-1.,7.97077743482043E-31,-1.4081690688991E-16));
#130046=DIRECTION('',(-0.951056516295153,-0.309016994374948,-2.29177897539323E-15));
#130047=DIRECTION('center_axis',(1.4081690688991E-16,6.98296267768627E-15,
-1.));
#130048=DIRECTION('ref_axis',(1.,-7.97077743482043E-31,1.4081690688991E-16));
#130049=DIRECTION('',(0.456775527877823,0.203374797931579,-0.866022406579775));
#130050=DIRECTION('center_axis',(1.4081690688991E-16,6.98296267768627E-15,
-1.));
#130051=DIRECTION('ref_axis',(-1.,7.97577417048809E-31,-1.40816906889911E-16));
#130052=DIRECTION('',(-0.475534671805145,-0.154505557223411,0.866022406579793));
#130053=DIRECTION('center_axis',(-1.4081690688991E-16,-6.98296267768627E-15,
1.));
#130054=DIRECTION('ref_axis',(-1.,9.83319205199467E-31,-1.40816906889911E-16));
#130055=DIRECTION('center_axis',(-1.4081690688991E-16,-6.98296267768627E-15,
1.));
#130056=DIRECTION('ref_axis',(-1.,7.98248735348668E-31,-1.4081690688991E-16));
#130057=DIRECTION('',(0.9135454576426,0.406736643075801,2.96886944389428E-15));
#130058=DIRECTION('center_axis',(1.4081690688991E-16,6.98296267768627E-15,
-1.));
#130059=DIRECTION('ref_axis',(-1.,1.24344978758018E-14,-1.40816906889824E-16));
#130060=DIRECTION('',(-0.951056516295153,-0.309016994374948,-2.29177897539323E-15));
#130061=DIRECTION('center_axis',(-1.4081690688991E-16,-6.98296267768627E-15,
1.));
#130062=DIRECTION('ref_axis',(-1.,7.99150043815584E-31,-1.4081690688991E-16));
#130063=DIRECTION('center_axis',(-1.4081690688991E-16,-6.98296267768627E-15,
1.));
#130064=DIRECTION('ref_axis',(1.,-7.99370576998456E-31,1.4081690688991E-16));
#130065=DIRECTION('',(0.456779171296638,0.203366124261504,0.866022521746641));
#130066=DIRECTION('center_axis',(-1.4081690688991E-16,-6.98296267768627E-15,
1.));
#130067=DIRECTION('ref_axis',(-1.,7.99858039355471E-31,-1.4081690688991E-16));
#130068=DIRECTION('center_axis',(-1.4081690688991E-16,-6.98296267768627E-15,
1.));
#130069=DIRECTION('ref_axis',(-1.,7.99858039355471E-31,-1.4081690688991E-16));
#130070=DIRECTION('center_axis',(-1.4081690688991E-16,-6.98296267768627E-15,
1.));
#130071=DIRECTION('ref_axis',(-1.,7.99858039355471E-31,-1.4081690688991E-16));
#130072=DIRECTION('',(-0.47553157557488,-0.154514440939479,-0.866022521746653));
#130073=DIRECTION('center_axis',(-1.4081690688991E-16,-6.98296267768627E-15,
1.));
#130074=DIRECTION('ref_axis',(-1.,9.83319205199467E-31,-1.40816906889911E-16));
#130075=DIRECTION('',(0.913545457642601,0.406736643075801,2.96886944389428E-15));
#130076=DIRECTION('center_axis',(1.4081690688991E-16,6.98296267768627E-15,
-1.));
#130077=DIRECTION('ref_axis',(-1.,1.24344978758018E-14,-1.40816906889824E-16));
#130078=DIRECTION('',(-0.951056516295153,-0.309016994374948,-2.29177897539323E-15));
#130079=DIRECTION('center_axis',(-1.4081690688991E-16,-6.98296267768627E-15,
1.));
#130080=DIRECTION('ref_axis',(-1.,8.32577322149061E-31,-1.39145123902276E-16));
#130081=DIRECTION('center_axis',(-0.405758682640331,0.913980246723162,-7.86457182175925E-6));
#130082=DIRECTION('ref_axis',(-1.85239931600469E-6,7.78238341415138E-6,
0.999999999968001));
#130083=DIRECTION('center_axis',(0.310034691293513,-0.950725244291265,-7.86457232249133E-6));
#130084=DIRECTION('ref_axis',(-0.806256330617362,-0.262927277567242,0.529924500330477));
#130085=DIRECTION('center_axis',(-1.4081690688991E-16,-6.98296267768627E-15,
1.));
#130086=DIRECTION('ref_axis',(-1.,8.07722881720021E-31,-1.42096112075504E-16));
#130087=DIRECTION('center_axis',(-0.405800366958868,0.913961739943519,9.77058183081883E-6));
#130088=DIRECTION('ref_axis',(0.799387144964317,0.35493425936279,-0.484769908303295));
#130089=DIRECTION('center_axis',(0.309991330319623,-0.950739383338677,9.77051486152074E-6));
#130090=DIRECTION('ref_axis',(0.831564948217564,0.271129178767091,-0.484756336025639));
#130091=DIRECTION('center_axis',(-1.4081690688991E-16,-6.98296267768627E-15,
1.));
#130092=DIRECTION('ref_axis',(-1.,8.24049048117772E-31,-1.37719829560012E-16));
#130093=DIRECTION('center_axis',(0.409108946466101,-0.912485544867162,-1.81624798278693E-5));
#130094=DIRECTION('ref_axis',(0.78952713763448,0.353971097460131,0.501349539843786));
#130095=DIRECTION('center_axis',(-0.306544826252812,0.951856222950124,-1.81316452657696E-5));
#130096=DIRECTION('ref_axis',(0.825238944242273,0.265777286958772,0.498340364251916));
#130097=DIRECTION('center_axis',(-1.4081690688991E-16,-6.98296267768627E-15,
1.));
#130098=DIRECTION('ref_axis',(-1.,8.26087817385229E-31,-1.38060560438432E-16));
#130099=DIRECTION('center_axis',(0.409121275899175,-0.91248001691248,-1.84940690708923E-5));
#130100=DIRECTION('ref_axis',(0.791100014432547,0.354709207426512,-0.498339387698464));
#130101=DIRECTION('center_axis',(-0.306531965213273,0.951860364738068,-1.85257020962267E-5));
#130102=DIRECTION('ref_axis',(0.823595688993123,0.265216544996729,-0.501348506861187));
#130103=DIRECTION('center_axis',(-1.4081690688991E-16,-6.98296267768627E-15,
1.));
#130104=DIRECTION('ref_axis',(-1.,9.83319205199467E-31,-1.40816906889911E-16));
#130105=DIRECTION('center_axis',(-1.4081690688991E-16,-6.98296267768627E-15,
1.));
#130106=DIRECTION('ref_axis',(-1.,8.46073526001725E-31,-1.4081690688991E-16));
#130107=DIRECTION('',(0.951056516295153,0.309016994374948,2.29177897539323E-15));
#130108=DIRECTION('center_axis',(-1.4081690688991E-16,-6.98296267768627E-15,
1.));
#130109=DIRECTION('ref_axis',(-1.,7.97077743482043E-31,-1.4081690688991E-16));
#130110=DIRECTION('center_axis',(-1.4081690688991E-16,-6.98296267768627E-15,
1.));
#130111=DIRECTION('ref_axis',(-1.,7.97077743482043E-31,-1.4081690688991E-16));
#130112=DIRECTION('center_axis',(-1.4081690688991E-16,-6.98296267768627E-15,
1.));
#130113=DIRECTION('ref_axis',(-1.,7.97077743482043E-31,-1.4081690688991E-16));
#130114=DIRECTION('',(-0.978147600733806,-0.20791169081776,-1.58957929685218E-15));
#130115=DIRECTION('center_axis',(1.4081690688991E-16,6.98296267768627E-15,
-1.));
#130116=DIRECTION('ref_axis',(1.,-7.97077743482043E-31,1.4081690688991E-16));
#130117=DIRECTION('',(0.475531718838049,0.154514645521708,-0.866022406579779));
#130118=DIRECTION('center_axis',(1.4081690688991E-16,6.98296267768627E-15,
-1.));
#130119=DIRECTION('ref_axis',(-1.,7.97577417048809E-31,-1.40816906889911E-16));
#130120=DIRECTION('',(-0.489079871579875,-0.103952251140501,0.866022406579781));
#130121=DIRECTION('center_axis',(-1.4081690688991E-16,-6.98296267768627E-15,
1.));
#130122=DIRECTION('ref_axis',(-1.,9.83319205199467E-31,-1.40816906889911E-16));
#130123=DIRECTION('center_axis',(-1.4081690688991E-16,-6.98296267768627E-15,
1.));
#130124=DIRECTION('ref_axis',(-1.,7.98248735348668E-31,-1.4081690688991E-16));
#130125=DIRECTION('',(0.951056516295153,0.309016994374948,2.29177897539323E-15));
#130126=DIRECTION('center_axis',(1.4081690688991E-16,6.98296267768627E-15,
-1.));
#130127=DIRECTION('ref_axis',(-1.,7.98707387273907E-31,-1.4081690688991E-16));
#130128=DIRECTION('',(-0.978147600733806,-0.20791169081776,-1.58957929685218E-15));
#130129=DIRECTION('center_axis',(-1.4081690688991E-16,-6.98296267768627E-15,
1.));
#130130=DIRECTION('ref_axis',(-1.,7.99150043815584E-31,-1.4081690688991E-16));
#130131=DIRECTION('center_axis',(-1.4081690688991E-16,-6.98296267768627E-15,
1.));
#130132=DIRECTION('ref_axis',(1.,-7.99370576998456E-31,1.4081690688991E-16));
#130133=DIRECTION('',(0.475534435652401,0.154505638525951,0.866022521746658));
#130134=DIRECTION('center_axis',(-1.4081690688991E-16,-6.98296267768627E-15,
1.));
#130135=DIRECTION('ref_axis',(-1.,7.99858039355471E-31,-1.4081690688991E-16));
#130136=DIRECTION('center_axis',(-1.4081690688991E-16,-6.98296267768627E-15,
1.));
#130137=DIRECTION('ref_axis',(-1.,7.99858039355471E-31,-1.4081690688991E-16));
#130138=DIRECTION('center_axis',(-1.4081690688991E-16,-6.98296267768627E-15,
1.));
#130139=DIRECTION('ref_axis',(-1.,7.99858039355471E-31,-1.4081690688991E-16));
#130140=DIRECTION('',(-0.489077720912241,-0.103961409834797,-0.866022521746663));
#130141=DIRECTION('center_axis',(-1.4081690688991E-16,-6.98296267768627E-15,
1.));
#130142=DIRECTION('ref_axis',(-1.,9.83319205199467E-31,-1.40816906889911E-16));
#130143=DIRECTION('',(0.951056516295153,0.309016994374948,2.29177897539323E-15));
#130144=DIRECTION('center_axis',(1.4081690688991E-16,6.98296267768627E-15,
-1.));
#130145=DIRECTION('ref_axis',(-1.,1.33226762955019E-14,-1.40816906889817E-16));
#130146=DIRECTION('',(-0.978147600733806,-0.20791169081776,-1.58957929685218E-15));
#130147=DIRECTION('center_axis',(-1.4081690688991E-16,-6.98296267768627E-15,
1.));
#130148=DIRECTION('ref_axis',(-1.,8.32577322149061E-31,-1.39145123902276E-16));
#130149=DIRECTION('center_axis',(-0.307998943474451,0.951386698854241,-7.86457217331017E-6));
#130150=DIRECTION('ref_axis',(-1.02877118498542E-6,7.93337950118864E-6,
0.999999999968002));
#130151=DIRECTION('center_axis',(0.208958440039605,-0.977924521767587,-7.86457232448164E-6));
#130152=DIRECTION('ref_axis',(-0.829322958353508,-0.177210199190942,0.529924500330464));
#130153=DIRECTION('center_axis',(-1.4081690688991E-16,-6.98296267768627E-15,
1.));
#130154=DIRECTION('ref_axis',(-1.,8.07722881720021E-31,-1.42096112075504E-16));
#130155=DIRECTION('center_axis',(-0.308042333920874,0.951372650656469,9.77059417868512E-6));
#130156=DIRECTION('ref_axis',(0.83210875123558,0.269431182533746,-0.484769908302517));
#130157=DIRECTION('center_axis',(0.208913838670284,-0.977934050903528,9.77051762784349E-6));
#130158=DIRECTION('ref_axis',(0.855350264826107,0.182721698612545,-0.484756336026725));
#130159=DIRECTION('center_axis',(-1.4081690688991E-16,-6.98296267768627E-15,
1.));
#130160=DIRECTION('ref_axis',(-1.,8.24049048117772E-31,-1.37719829560012E-16));
#130161=DIRECTION('center_axis',(0.311487093092632,-0.950250383060605,-1.81624797870643E-5));
#130162=DIRECTION('ref_axis',(0.822202080224617,0.26950394834691,0.501349539841953));
#130163=DIRECTION('center_axis',(-0.205369473383596,0.978684514577291,-1.81316452352081E-5));
#130164=DIRECTION('ref_axis',(0.848499490339199,0.178060372502337,0.498340364247618));
#130165=DIRECTION('center_axis',(-1.4081690688991E-16,-6.98296267768627E-15,
1.));
#130166=DIRECTION('ref_axis',(-1.,8.26087817385229E-31,-1.38060560438432E-16));
#130167=DIRECTION('center_axis',(0.311499932819129,-0.950246174163121,-1.84940568302248E-5));
#130168=DIRECTION('ref_axis',(0.823843494140198,0.270073604475308,-0.498339387695358));
#130169=DIRECTION('center_axis',(-0.205356249869677,0.978687289330081,-1.85257132684071E-5));
#130170=DIRECTION('ref_axis',(0.84680662351654,0.177674469288859,-0.501348506860686));
#130171=DIRECTION('center_axis',(-1.4081690688991E-16,-6.98296267768627E-15,
1.));
#130172=DIRECTION('ref_axis',(-1.,9.83319205199467E-31,-1.40816906889911E-16));
#130173=DIRECTION('center_axis',(-1.4081690688991E-16,-6.98296267768627E-15,
1.));
#130174=DIRECTION('ref_axis',(-1.,8.46073526001725E-31,-1.4081690688991E-16));
#130175=DIRECTION('',(0.978147600733806,0.20791169081776,1.58957929685218E-15));
#130176=DIRECTION('center_axis',(-1.4081690688991E-16,-6.98296267768627E-15,
1.));
#130177=DIRECTION('ref_axis',(-1.,7.97077743482043E-31,-1.4081690688991E-16));
#130178=DIRECTION('center_axis',(-1.4081690688991E-16,-6.98296267768627E-15,
1.));
#130179=DIRECTION('ref_axis',(-1.,7.97077743482043E-31,-1.4081690688991E-16));
#130180=DIRECTION('center_axis',(-1.4081690688991E-16,-6.98296267768627E-15,
1.));
#130181=DIRECTION('ref_axis',(-1.,7.97077743482043E-31,-1.4081690688991E-16));
#130182=DIRECTION('',(-0.994521895368273,-0.104528463267654,-8.69963854893977E-16));
#130183=DIRECTION('center_axis',(1.4081690688991E-16,6.98296267768627E-15,
-1.));
#130184=DIRECTION('ref_axis',(1.,-7.97077743482043E-31,1.4081690688991E-16));
#130185=DIRECTION('',(0.48907788477527,0.103961598321241,-0.866022406579784));
#130186=DIRECTION('center_axis',(1.4081690688991E-16,6.98296267768627E-15,
-1.));
#130187=DIRECTION('ref_axis',(-1.,7.97577417048809E-31,-1.40816906889911E-16));
#130188=DIRECTION('',(-0.497266609935059,-0.0522600224406523,0.866022406579758));
#130189=DIRECTION('center_axis',(-1.4081690688991E-16,-6.98296267768627E-15,
1.));
#130190=DIRECTION('ref_axis',(-1.,9.83319205199467E-31,-1.40816906889911E-16));
#130191=DIRECTION('center_axis',(-1.4081690688991E-16,-6.98296267768627E-15,
1.));
#130192=DIRECTION('ref_axis',(-1.,7.98248735348668E-31,-1.4081690688991E-16));
#130193=DIRECTION('',(0.978147600733806,0.20791169081776,1.58957929685218E-15));
#130194=DIRECTION('center_axis',(1.4081690688991E-16,6.98296267768627E-15,
-1.));
#130195=DIRECTION('ref_axis',(-1.,7.98707387273907E-31,-1.4081690688991E-16));
#130196=DIRECTION('',(-0.994521895368273,-0.104528463267654,-8.69963854893977E-16));
#130197=DIRECTION('center_axis',(-1.4081690688991E-16,-6.98296267768627E-15,
1.));
#130198=DIRECTION('ref_axis',(-1.,7.99150043815584E-31,-1.4081690688991E-16));
#130199=DIRECTION('center_axis',(-1.4081690688991E-16,-6.98296267768627E-15,
1.));
#130200=DIRECTION('ref_axis',(1.,-7.99370576998456E-31,1.4081690688991E-16));
#130201=DIRECTION('',(0.489079645219225,0.103952356682307,0.866022521746653));
#130202=DIRECTION('center_axis',(-1.4081690688991E-16,-6.98296267768627E-15,
1.));
#130203=DIRECTION('ref_axis',(-1.,7.99858039355471E-31,-1.4081690688991E-16));
#130204=DIRECTION('center_axis',(-1.4081690688991E-16,-6.98296267768627E-15,
1.));
#130205=DIRECTION('ref_axis',(-1.,7.99858039355471E-31,-1.4081690688991E-16));
#130206=DIRECTION('center_axis',(-1.4081690688991E-16,-6.98296267768627E-15,
1.));
#130207=DIRECTION('ref_axis',(-1.,7.99858039355471E-31,-1.4081690688991E-16));
#130208=DIRECTION('',(-0.497265428393217,-0.052269355768654,-0.866022521746658));
#130209=DIRECTION('center_axis',(-1.4081690688991E-16,-6.98296267768627E-15,
1.));
#130210=DIRECTION('ref_axis',(-1.,9.83319205199467E-31,-1.40816906889911E-16));
#130211=DIRECTION('',(0.978147600733806,0.20791169081776,1.58957929685218E-15));
#130212=DIRECTION('center_axis',(1.4081690688991E-16,6.98296267768627E-15,
-1.));
#130213=DIRECTION('ref_axis',(-1.,8.01265634860448E-31,-1.4081690688991E-16));
#130214=DIRECTION('',(-0.994521895368273,-0.104528463267654,-8.69963854893977E-16));
#130215=DIRECTION('center_axis',(-1.4081690688991E-16,-6.98296267768627E-15,
1.));
#130216=DIRECTION('ref_axis',(-1.,8.32577322149061E-31,-1.39145123902276E-16));
#130217=DIRECTION('center_axis',(-0.206864703431196,0.978369559222113,-7.86457193300846E-6));
#130218=DIRECTION('ref_axis',(-1.93871482032996E-7,7.99745524812744E-6,
0.999999999968002));
#130219=DIRECTION('center_axis',(0.10559279638925,-0.99440945353956,-7.86457230109251E-6));
#130220=DIRECTION('ref_axis',(-0.843303350210939,-0.0895515687886603,0.529924500330468));
#130221=DIRECTION('center_axis',(-1.4081690688991E-16,-6.98296267768627E-15,
1.));
#130222=DIRECTION('ref_axis',(-1.,8.07722881720021E-31,-1.42096112075504E-16));
#130223=DIRECTION('center_axis',(-0.206909324622309,0.978360123517346,9.77058376346471E-6));
#130224=DIRECTION('ref_axis',(0.85571359989698,0.180976161286345,-0.484769908304352));
#130225=DIRECTION('center_axis',(0.10554744328483,-0.994414268361317,9.77051740345421E-6));
#130226=DIRECTION('ref_axis',(0.86976418493997,0.0923122812911577,-0.484756336027217));
#130227=DIRECTION('center_axis',(-1.4081690688991E-16,-6.98296267768627E-15,
1.));
#130228=DIRECTION('ref_axis',(-1.,8.24049048117772E-31,-1.37719829560012E-16));
#130229=DIRECTION('center_axis',(0.210452521944419,-0.977604079204541,-1.81624797886102E-5));
#130230=DIRECTION('ref_axis',(0.84586880476805,0.182084057578303,0.501349539838316));
#130231=DIRECTION('center_axis',(-0.10194404958761,0.994790133859862,-1.81316452628073E-5));
#130232=DIRECTION('ref_axis',(0.862463698457381,0.0883925913424311,0.498340364248156));
#130233=DIRECTION('center_axis',(-1.4081690688991E-16,-6.98296267768627E-15,
1.));
#130234=DIRECTION('ref_axis',(-1.,8.26087817385229E-31,-1.38060560438432E-16));
#130235=DIRECTION('center_axis',(0.210465731283201,-0.977601235480703,-1.84940567325367E-5));
#130236=DIRECTION('ref_axis',(0.847560772121326,0.182479018595613,-0.498339387700273));
#130237=DIRECTION('center_axis',(-0.10193060847116,0.994791511178849,-1.85257102811266E-5));
#130238=DIRECTION('ref_axis',(0.860739767468925,0.0881857549149035,-0.501348506856886));
#130239=DIRECTION('center_axis',(-1.4081690688991E-16,-6.98296267768627E-15,
1.));
#130240=DIRECTION('ref_axis',(-1.,9.83319205199467E-31,-1.40816906889911E-16));
#130241=DIRECTION('center_axis',(-1.4081690688991E-16,-6.98296267768627E-15,
1.));
#130242=DIRECTION('ref_axis',(-1.,9.83319205199467E-31,-1.40816906889911E-16));
#130243=DIRECTION('center_axis',(-1.4081690688991E-16,-6.98296267768627E-15,
1.));
#130244=DIRECTION('ref_axis',(-1.,8.46073526001725E-31,-1.4081690688991E-16));
#130245=DIRECTION('',(0.994521895368273,0.104528463267654,8.69963854893977E-16));
#130246=DIRECTION('center_axis',(-1.4081690688991E-16,-6.98296267768627E-15,
1.));
#130247=DIRECTION('ref_axis',(-1.,7.97077743482043E-31,-1.4081690688991E-16));
#130248=DIRECTION('center_axis',(-1.4081690688991E-16,-6.98296267768627E-15,
1.));
#130249=DIRECTION('ref_axis',(-1.,7.97077743482043E-31,-1.4081690688991E-16));
#130250=DIRECTION('center_axis',(-1.4081690688991E-16,-6.98296267768627E-15,
1.));
#130251=DIRECTION('ref_axis',(-1.,7.97077743482043E-31,-1.4081690688991E-16));
#130252=DIRECTION('',(-1.,9.83319205199467E-31,-1.40816906889911E-16));
#130253=DIRECTION('center_axis',(1.4081690688991E-16,6.98296267768627E-15,
-1.));
#130254=DIRECTION('ref_axis',(1.,-7.97077743482043E-31,1.4081690688991E-16));
#130255=DIRECTION('',(0.497265611060784,0.0522695260942052,-0.866022406579779));
#130256=DIRECTION('center_axis',(1.4081690688991E-16,6.98296267768627E-15,
-1.));
#130257=DIRECTION('ref_axis',(-1.,7.97577417048809E-31,-1.40816906889911E-16));
#130258=DIRECTION('',(-0.500005191251968,4.77800115976002E-6,0.866022406579792));
#130259=DIRECTION('center_axis',(-1.4081690688991E-16,-6.98296267768627E-15,
1.));
#130260=DIRECTION('ref_axis',(-1.,9.83319205199467E-31,-1.40816906889911E-16));
#130261=DIRECTION('center_axis',(-1.4081690688991E-16,-6.98296267768627E-15,
1.));
#130262=DIRECTION('ref_axis',(-1.,7.98248735348668E-31,-1.4081690688991E-16));
#130263=DIRECTION('',(0.994521895368273,0.104528463267654,8.69963854893977E-16));
#130264=DIRECTION('center_axis',(1.4081690688991E-16,6.98296267768627E-15,
-1.));
#130265=DIRECTION('ref_axis',(-1.,7.98707387273907E-31,-1.4081690688991E-16));
#130266=DIRECTION('',(-1.,9.83319205199467E-31,-1.40816906889911E-16));
#130267=DIRECTION('center_axis',(-1.4081690688991E-16,-6.98296267768627E-15,
1.));
#130268=DIRECTION('ref_axis',(-1.,7.99150043815584E-31,-1.4081690688991E-16));
#130269=DIRECTION('center_axis',(-1.4081690688991E-16,-6.98296267768627E-15,
1.));
#130270=DIRECTION('ref_axis',(1.,-7.99370576998456E-31,1.4081690688991E-16));
#130271=DIRECTION('',(0.497266395846506,0.052260151065429,0.86602252174666));
#130272=DIRECTION('center_axis',(-1.4081690688991E-16,-6.98296267768627E-15,
1.));
#130273=DIRECTION('ref_axis',(-1.,7.99858039355471E-31,-1.4081690688991E-16));
#130274=DIRECTION('center_axis',(-1.4081690688991E-16,-6.98296267768627E-15,
1.));
#130275=DIRECTION('ref_axis',(-1.,7.99858039355471E-31,-1.4081690688991E-16));
#130276=DIRECTION('center_axis',(-1.4081690688991E-16,-6.98296267768627E-15,
1.));
#130277=DIRECTION('ref_axis',(-1.,7.99858039355471E-31,-1.4081690688991E-16));
#130278=DIRECTION('',(-0.500004991781247,-4.62770264658395E-6,-0.866022521746646));
#130279=DIRECTION('center_axis',(-1.4081690688991E-16,-6.98296267768627E-15,
1.));
#130280=DIRECTION('ref_axis',(-1.,9.83319205199467E-31,-1.40816906889911E-16));
#130281=DIRECTION('',(0.994521895368273,0.104528463267654,8.69963854893977E-16));
#130282=DIRECTION('center_axis',(1.4081690688991E-16,6.98296267768627E-15,
-1.));
#130283=DIRECTION('ref_axis',(-1.,-8.88178419700124E-16,-1.40816906889917E-16));
#130284=DIRECTION('',(-1.,9.83319205199467E-31,-1.40816906889911E-16));
#130285=DIRECTION('center_axis',(-1.4081690688991E-16,-6.98296267768627E-15,
1.));
#130286=DIRECTION('ref_axis',(-1.,9.83319205199467E-31,-1.40816906889911E-16));
#130287=DIRECTION('center_axis',(1.4081690688991E-16,6.98296267768627E-15,
-1.));
#130288=DIRECTION('ref_axis',(1.,-9.83319205199467E-31,1.40816906889911E-16));
#130289=DIRECTION('center_axis',(-1.4081690688991E-16,-6.98296267768627E-15,
1.));
#130290=DIRECTION('ref_axis',(-1.,8.32577322149061E-31,-1.39145123902276E-16));
#130291=DIRECTION('center_axis',(-0.103464010407694,0.994633197962196,-7.86457221782119E-6));
#130292=DIRECTION('ref_axis',(6.43152272453736E-7,7.97390972565421E-6,0.999999999968002));
#130293=DIRECTION('center_axis',(0.00107025596496831,-0.999999427244995,
-7.86457232244496E-6));
#130294=DIRECTION('ref_axis',(-0.848044334090886,-0.000911792658910411,
0.529924500330465));
#130295=DIRECTION('center_axis',(-1.4081690688991E-16,-6.98296267768627E-15,
1.));
#130296=DIRECTION('ref_axis',(-1.,8.07722881720021E-31,-1.42096112075504E-16));
#130297=DIRECTION('center_axis',(-0.103509373457858,0.994628478131859,9.77058599509235E-6));
#130298=DIRECTION('ref_axis',(0.869943071290751,0.0905383273446241,-0.484769908301715));
#130299=DIRECTION('center_axis',(0.00102464802302249,-0.999999475000345,
9.77051621741992E-6));
#130300=DIRECTION('ref_axis',(0.874648786634666,0.000891471298443714,-0.484756336026081));
#130301=DIRECTION('center_axis',(-1.4081690688991E-16,-6.98296267768627E-15,
1.));
#130302=DIRECTION('ref_axis',(-1.,8.24049048117772E-31,-1.37719829560012E-16));
#130303=DIRECTION('center_axis',(0.10711218892574,-0.99424694047991,-1.81624798142884E-5));
#130304=DIRECTION('ref_axis',(0.860268013667682,0.0926692157698502,0.501349539851053));
#130305=DIRECTION('center_axis',(0.00259829454877957,0.999996624262643,
-1.81316452223945E-5));
#130306=DIRECTION('ref_axis',(0.866978573811375,-0.00224363754548925,0.498340364251741));
#130307=DIRECTION('center_axis',(-1.4081690688991E-16,-6.98296267768627E-15,
1.));
#130308=DIRECTION('ref_axis',(-1.,8.26087817385229E-31,-1.38060560438432E-16));
#130309=DIRECTION('center_axis',(0.107125623152397,-0.99424549308618,-1.84940568669125E-5));
#130310=DIRECTION('ref_axis',(0.86199199692613,0.0928851544032709,-0.498339387693551));
#130311=DIRECTION('center_axis',(0.00261180600212697,0.999996589057285,
-1.85257108462124E-5));
#130312=DIRECTION('ref_axis',(0.865242466401146,-0.00226914104442312,-0.501348506864219));
#130313=DIRECTION('center_axis',(0.,-6.98296267768627E-15,1.));
#130314=DIRECTION('ref_axis',(-1.,0.,0.));
#130315=DIRECTION('',(1.,0.,0.));
#130316=DIRECTION('center_axis',(0.,6.98296267768627E-15,-1.));
#130317=DIRECTION('ref_axis',(-1.,-2.87680990140871E-12,-2.00886561723353E-26));
#130318=DIRECTION('',(-1.,0.,0.));
#130319=DIRECTION('center_axis',(0.,-6.98296267768627E-15,1.));
#130320=DIRECTION('ref_axis',(-1.,0.,0.));
#130321=DIRECTION('center_axis',(0.,-1.,-6.98296267768627E-15));
#130322=DIRECTION('ref_axis',(0.,6.98296267768627E-15,-1.));
#130323=DIRECTION('center_axis',(5.53227016421295E-17,-1.,-7.21882542163455E-15));
#130324=DIRECTION('ref_axis',(0.874651456243689,-3.45095442585563E-15,0.484752338922459));
#130325=DIRECTION('',(-0.529924709392052,5.88254176989232E-15,-0.848044693619239));
#130326=DIRECTION('',(1.,0.,0.));
#130327=DIRECTION('',(-0.529924185123396,-5.88254404234737E-15,0.84804502122311));
#130328=DIRECTION('center_axis',(-5.53239299512741E-17,-1.,-7.21882753539534E-15));
#130329=DIRECTION('ref_axis',(0.874649580953124,3.45097890568783E-15,-0.484755722543349));
#130330=DIRECTION('',(-1.,9.83319205199467E-31,-1.40816906889911E-16));
#130331=DIRECTION('',(-0.500005012714979,6.05598756357692E-15,-0.866022509672753));
#130332=DIRECTION('center_axis',(9.46835262113691E-7,0.999999999998207,
-1.63998885887388E-6));
#130333=DIRECTION('ref_axis',(0.866072335962825,-1.66725164348147E-10,0.499918702270574));
#130334=DIRECTION('',(-1.,9.83319205199467E-31,-1.40816906889911E-16));
#130335=DIRECTION('center_axis',(-9.46924648784811E-7,0.999999999998207,
-1.64014403517076E-6));
#130336=DIRECTION('ref_axis',(0.866043284546741,5.65134626076186E-11,-0.499969028332249));
#130337=DIRECTION('',(-0.500005169296822,-6.05598693139308E-15,0.866022419268956));
#130338=DIRECTION('',(-1.,9.83319205199467E-31,-1.40816906889911E-16));
#130339=DIRECTION('center_axis',(0.,-1.,-6.98296267768627E-15));
#130340=DIRECTION('ref_axis',(0.,6.98296267768627E-15,-1.));
#130341=DIRECTION('center_axis',(2.5057754547737E-16,1.,7.42579288178415E-15));
#130342=DIRECTION('ref_axis',(0.874649580936334,3.38052804894766E-15,-0.484755722573643));
#130343=DIRECTION('',(0.529924185123401,5.93414530587678E-15,-0.848045021223107));
#130344=DIRECTION('',(-1.,0.,0.));
#130345=DIRECTION('',(0.529924709392047,-5.93414301348781E-15,0.848044693619242));
#130346=DIRECTION('center_axis',(-2.50576144038582E-16,1.,7.42579081637246E-15));
#130347=DIRECTION('ref_axis',(0.874651456263127,-3.38050267703688E-15,0.484752338887387));
#130348=DIRECTION('',(1.,-9.83319205199467E-31,1.40816906889911E-16));
#130349=DIRECTION('',(0.500005169296811,5.91835086477038E-15,-0.866022419268963));
#130350=DIRECTION('center_axis',(-9.4705535579882E-7,-0.999999999998206,
-1.64037044329868E-6));
#130351=DIRECTION('ref_axis',(0.866072438648831,-1.66970090552065E-10,-0.499918524374589));
#130352=DIRECTION('',(1.,-9.83319205199467E-31,1.40816906889911E-16));
#130353=DIRECTION('center_axis',(9.46713286859869E-7,-0.999999999998207,
-1.63977760307947E-6));
#130354=DIRECTION('ref_axis',(0.8660431783397,5.62673641619407E-11,0.499969212303389));
#130355=DIRECTION('',(0.500005012714967,-5.9183514825864E-15,0.86602250967276));
#130356=DIRECTION('',(1.,-9.83319205199467E-31,1.40816906889911E-16));
#130357=DIRECTION('center_axis',(1.,0.,0.));
#130358=DIRECTION('ref_axis',(0.,-6.97886326506453E-15,1.));
#130359=DIRECTION('center_axis',(-1.,0.,0.));
#130360=DIRECTION('ref_axis',(0.,6.97886326506453E-15,-1.));
#130361=DIRECTION('center_axis',(-0.500005014362137,6.20016534342884E-15,
-0.866022508721753));
#130362=DIRECTION('ref_axis',(9.79094323195944E-13,-1.,-5.63853427197664E-13));
#130363=DIRECTION('center_axis',(-0.86601822301453,3.004221614602E-5,-0.500012436349559));
#130364=DIRECTION('ref_axis',(0.500012217441046,0.000989701298603201,-0.866017784402277));
#130365=DIRECTION('center_axis',(0.500005023014372,1.39506795850222E-14,
0.866022503726316));
#130366=DIRECTION('ref_axis',(-0.866022503726316,-3.41480999208039E-15,
0.500005023014372));
#130367=DIRECTION('center_axis',(1.,0.,0.));
#130368=DIRECTION('ref_axis',(0.,-6.82961998416066E-15,1.));
#130369=DIRECTION('center_axis',(-1.,9.83319205199467E-31,-1.4081690688991E-16));
#130370=DIRECTION('ref_axis',(1.4081690688991E-16,6.82961998416066E-15,
-1.));
#130371=DIRECTION('center_axis',(-1.,0.,0.));
#130372=DIRECTION('ref_axis',(0.,6.82961998416066E-15,-1.));
#130373=DIRECTION('center_axis',(-1.,9.83319205199467E-31,-1.4081690688991E-16));
#130374=DIRECTION('ref_axis',(1.4081690688991E-16,6.82961998416066E-15,
-1.));
#130375=DIRECTION('center_axis',(1.,0.,0.));
#130376=DIRECTION('ref_axis',(0.,-6.82961998416066E-15,1.));
#130377=DIRECTION('center_axis',(-0.529924213265765,-5.92186660939952E-15,
0.848045003637578));
#130378=DIRECTION('ref_axis',(-0.848045003637578,3.84166124109038E-15,-0.529924213265765));
#130379=DIRECTION('center_axis',(0.500005158533463,6.04740227518902E-15,
-0.866022425483271));
#130380=DIRECTION('ref_axis',(0.866022425483271,-3.41480999208032E-15,0.500005158533463));
#130381=DIRECTION('center_axis',(0.529924185004323,2.16250629064169E-8,
-0.848045021297516));
#130382=DIRECTION('ref_axis',(0.848037146343375,0.00430950302668586,0.529919264233193));
#130383=DIRECTION('center_axis',(-0.529924157141051,-5.92186685429947E-15,
0.848045038708645));
#130384=DIRECTION('ref_axis',(-0.848045038708645,3.84166124109037E-15,-0.529924157141051));
#130385=DIRECTION('center_axis',(0.500005172385372,1.05114548020227E-8,
-0.866022417485757));
#130386=DIRECTION('ref_axis',(0.866013458679463,0.00454855867658242,0.5));
#130387=DIRECTION('center_axis',(0.866037336481667,-3.44576747032758E-5,
-0.499979330205167));
#130388=DIRECTION('ref_axis',(0.499979069431688,-0.000963977562132558,0.866036951219452));
#130389=DIRECTION('center_axis',(-0.00024249581833115,0.999999970597889,
6.99630157351179E-15));
#130390=DIRECTION('ref_axis',(0.999999970597889,0.00024249581833115,9.21890050058242E-32));
#130391=DIRECTION('center_axis',(-1.,9.83319205199467E-31,-1.4081690688991E-16));
#130392=DIRECTION('ref_axis',(1.4081690688991E-16,6.82961998416066E-15,
-1.));
#130393=DIRECTION('center_axis',(1.,0.,0.));
#130394=DIRECTION('ref_axis',(0.,-6.82961998416066E-15,1.));
#130395=DIRECTION('center_axis',(0.,-6.98296267768627E-15,1.));
#130396=DIRECTION('ref_axis',(1.,1.22464679914735E-16,0.));
#130397=DIRECTION('center_axis',(0.000242495818331158,0.999999970597889,
6.98296247237242E-15));
#130398=DIRECTION('ref_axis',(0.999999970597889,-0.000242495818331158,-5.20911529687998E-32));
#130399=DIRECTION('center_axis',(0.529924676825566,1.14592471176548E-14,
0.848044713969328));
#130400=DIRECTION('ref_axis',(-0.848044713969328,-3.84166124109036E-15,
0.529924676825566));
#130401=DIRECTION('center_axis',(0.529924157141051,5.92186685429947E-15,
-0.848045038708645));
#130402=DIRECTION('ref_axis',(0.848045038708645,-3.84166124109037E-15,0.529924157141051));
#130403=DIRECTION('center_axis',(0.529924709439994,-2.52126420968272E-8,
0.848044693589281));
#130404=DIRECTION('ref_axis',(-0.848035979777037,-0.00453325469613692,0.529919264233204));
#130405=DIRECTION('center_axis',(0.529924742154432,-3.48753411745471E-14,
0.848044673146739));
#130406=DIRECTION('ref_axis',(-0.848044673146739,-3.84166124109014E-15,
0.529924742154432));
#130407=DIRECTION('center_axis',(-0.529924185162661,-2.16945438508739E-8,
0.848045021198574));
#130408=DIRECTION('ref_axis',(0.848037146343336,-0.00430950303668575,0.529919264233174));
#130409=DIRECTION('center_axis',(0.52992421326579,5.92186660939942E-15,
-0.848045003637563));
#130410=DIRECTION('ref_axis',(0.848045003637563,-3.84166124109038E-15,0.52992421326579));
#130411=DIRECTION('center_axis',(-0.000258180127964207,0.99999996667151,
6.95551716657602E-15));
#130412=DIRECTION('ref_axis',(0.99999996667151,0.000258180127964207,-1.33844997483071E-32));
#130413=DIRECTION('center_axis',(1.,0.,0.));
#130414=DIRECTION('ref_axis',(0.,-6.82961998416066E-15,1.));
#130415=DIRECTION('center_axis',(0.,-6.98296267768627E-15,1.));
#130416=DIRECTION('ref_axis',(1.,1.22464679914735E-16,0.));
#130417=DIRECTION('center_axis',(0.000258180127964191,0.99999996667151,
6.98372952115933E-15));
#130418=DIRECTION('ref_axis',(0.99999996667151,-0.000258180127964191,3.65206484909203E-32));
#130419=DIRECTION('center_axis',(1.,-9.83319205199467E-31,1.4081690688991E-16));
#130420=DIRECTION('ref_axis',(-1.4081690688991E-16,-6.82961998416066E-15,
1.));
#130421=DIRECTION('center_axis',(0.866018223015094,3.00422153149717E-5,
0.500012436348582));
#130422=DIRECTION('ref_axis',(0.500012217440065,-0.000989701305507211,-0.866017784402835));
#130423=DIRECTION('center_axis',(-0.529924742154432,-2.30316125713584E-14,
-0.848044673146739));
#130424=DIRECTION('ref_axis',(0.848044673146739,3.8416612410906E-15,-0.529924742154432));
#130425=DIRECTION('center_axis',(-0.50000500959944,1.0113261475945E-8,-0.866022511471535));
#130426=DIRECTION('ref_axis',(-0.866013834616175,0.0044764107713436,0.499999999999996));
#130427=DIRECTION('center_axis',(0.50000502301429,-6.04740282155761E-15,
0.866022503726363));
#130428=DIRECTION('ref_axis',(-0.866022503726363,-3.41480999208032E-15,
0.50000502301429));
#130429=DIRECTION('center_axis',(-0.529924709245859,2.52852559485652E-8,
-0.848044693710592));
#130430=DIRECTION('ref_axis',(-0.848035979777086,0.00453325468302945,0.529919264233239));
#130431=DIRECTION('center_axis',(-0.529924676825566,5.92186458665694E-15,
-0.848044713969328));
#130432=DIRECTION('ref_axis',(0.848044713969328,3.84166124109038E-15,-0.529924676825566));
#130433=DIRECTION('center_axis',(1.,0.,0.));
#130434=DIRECTION('ref_axis',(0.,-6.82961998416066E-15,1.));
#130435=DIRECTION('center_axis',(-1.,0.,0.));
#130436=DIRECTION('ref_axis',(0.,6.82961998416066E-15,-1.));
#130437=DIRECTION('center_axis',(1.,-9.83319205199467E-31,1.4081690688991E-16));
#130438=DIRECTION('ref_axis',(-1.4081690688991E-16,-6.82961998416066E-15,
1.));
#130439=DIRECTION('center_axis',(1.,-3.81527851617387E-28,5.46369598732844E-14));
#130440=DIRECTION('ref_axis',(-5.46369598732844E-14,-6.82961998416066E-15,
1.));
#130441=DIRECTION('center_axis',(1.,-9.83319205199467E-31,1.4081690688991E-16));
#130442=DIRECTION('ref_axis',(-1.4081690688991E-16,-6.82961998416066E-15,
1.));
#130443=DIRECTION('center_axis',(-0.866037336481684,-3.44576748086449E-5,
0.499979330205139));
#130444=DIRECTION('ref_axis',(0.499979069431657,0.000963977566348111,0.866036951219465));
#130445=DIRECTION('center_axis',(0.500005158533422,6.04740227518918E-15,
-0.866022425483294));
#130446=DIRECTION('ref_axis',(0.866022425483294,-3.41480999208032E-15,0.500005158533422));
#130447=DIRECTION('center_axis',(0.500005167509865,6.31729921158743E-15,
-0.866022420300671));
#130448=DIRECTION('ref_axis',(-5.94450122015092E-12,1.,-3.41808820158678E-12));
#130449=DIRECTION('center_axis',(-7.71409749859041E-19,-6.96824330280696E-15,
1.));
#130450=DIRECTION('ref_axis',(0.,-1.,-6.96824330280696E-15));
#130451=DIRECTION('',(0.994521895368273,0.104528463267654,7.29146948004066E-16));
#130452=DIRECTION('center_axis',(7.71409749859041E-19,6.96824330280696E-15,
-1.));
#130453=DIRECTION('ref_axis',(-1.08459293348099E-36,-1.,-6.96824330280696E-15));
#130454=DIRECTION('',(-0.994521895368273,-0.104528463267654,-7.29146948004066E-16));
#130455=DIRECTION('center_axis',(-7.71409749859041E-19,-6.96824330280696E-15,
1.));
#130456=DIRECTION('ref_axis',(2.55974201233206E-36,-1.,-6.96824330280696E-15));
#130457=DIRECTION('center_axis',(0.104528463267654,-0.994521895368273,-6.92998990261915E-15));
#130458=DIRECTION('ref_axis',(7.71409749859066E-19,6.96824330280696E-15,
-1.));
#130459=DIRECTION('center_axis',(0.104528463267637,-0.994521895368275,1.90905987588518E-14));
#130460=DIRECTION('ref_axis',(0.869860024050105,0.0914259726159642,0.48475233892244));
#130461=DIRECTION('',(-0.527021726387053,-0.0553922155203021,-0.848044693619247));
#130462=DIRECTION('',(0.994521895368273,0.104528463267654,7.29146948004067E-16));
#130463=DIRECTION('',(-0.527021204990394,-0.0553921607193182,0.848045021223118));
#130464=DIRECTION('center_axis',(0.10452846326765,-0.994521895368274,-1.18885524848236E-14));
#130465=DIRECTION('ref_axis',(0.869858159031309,0.0914257765945981,-0.48475572254563));
#130466=DIRECTION('',(-0.994521895368273,-0.104528463267654,-8.69963854893977E-16));
#130467=DIRECTION('',(-0.497265932938934,-0.05226475560521,-0.866022509672756));
#130468=DIRECTION('center_axis',(-0.104527521619063,0.994521994337725,-1.63998885964307E-6));
#130469=DIRECTION('ref_axis',(0.861327901105178,0.0905292101910039,0.499918702270621));
#130470=DIRECTION('',(-0.994521895368273,-0.104528463267654,-8.69963854893977E-16));
#130471=DIRECTION('center_axis',(-0.104529405004769,0.994521796385911,-1.6401440381083E-6));
#130472=DIRECTION('ref_axis',(0.861299008814395,0.0905261737133511,-0.499969028328917));
#130473=DIRECTION('',(-0.497266088663003,-0.0522647719724915,0.86602241926896));
#130474=DIRECTION('',(-0.994521895368273,-0.104528463267654,-8.69963854893977E-16));
#130475=DIRECTION('center_axis',(0.104528463267654,-0.994521895368273,-6.92998990261915E-15));
#130476=DIRECTION('ref_axis',(7.71409749859066E-19,6.96824330280696E-15,
-1.));
#130477=DIRECTION('center_axis',(-0.104528463267662,0.994521895368273,-4.47974441404753E-15));
#130478=DIRECTION('ref_axis',(0.869858159016179,0.0914257765930096,-0.484755722573081));
#130479=DIRECTION('',(0.527021204990417,0.0553921607193179,-0.848045021223103));
#130480=DIRECTION('',(-0.994521895368273,-0.104528463267654,-7.29146948004067E-16));
#130481=DIRECTION('',(0.527021726387063,0.0553922155203017,0.848044693619241));
#130482=DIRECTION('center_axis',(-0.104528463267657,0.994521895368273,1.39216640785751E-14));
#130483=DIRECTION('ref_axis',(0.869860024068681,0.0914259726179182,0.484752338888738));
#130484=DIRECTION('',(0.994521895368273,0.104528463267654,8.69963854893977E-16));
#130485=DIRECTION('',(0.497266088663018,0.052264771972485,-0.866022419268951));
#130486=DIRECTION('center_axis',(0.104527521400192,-0.994521994360729,-1.64037041421999E-6));
#130487=DIRECTION('ref_axis',(0.861328003227311,0.0905292209242257,-0.49991852437703));
#130488=DIRECTION('',(0.994521895368273,0.104528463267654,8.69963854893977E-16));
#130489=DIRECTION('center_axis',(0.10452940479455,-0.994521796408007,-1.63977758816116E-6));
#130490=DIRECTION('ref_axis',(0.861298903188812,0.0905261626114036,0.49996921230072));
#130491=DIRECTION('',(0.497265932938937,0.0522647556052066,0.866022509672755));
#130492=DIRECTION('',(0.994521895368273,0.104528463267654,8.69963854893977E-16));
#130493=DIRECTION('center_axis',(-3.07718727278886E-18,-6.95368519647906E-15,
1.));
#130494=DIRECTION('ref_axis',(0.,-1.,-6.95368519647906E-15));
#130495=DIRECTION('',(0.978147600733805,0.20791169081776,1.44876238996227E-15));
#130496=DIRECTION('center_axis',(3.07718727278886E-18,6.95368519647906E-15,
-1.));
#130497=DIRECTION('ref_axis',(2.06146211212399E-12,-1.,-6.95368519647905E-15));
#130498=DIRECTION('',(-0.978147600733805,-0.20791169081776,-1.44876238996227E-15));
#130499=DIRECTION('center_axis',(-3.07718727278886E-18,-6.95368519647906E-15,
1.));
#130500=DIRECTION('ref_axis',(1.06288922528842E-35,-1.,-6.95368519647906E-15));
#130501=DIRECTION('center_axis',(0.20791169081776,-0.978147600733806,-6.80109070798532E-15));
#130502=DIRECTION('ref_axis',(3.07718727278892E-18,6.95368519647906E-15,
-1.));
#130503=DIRECTION('center_axis',(0.207911690817738,-0.97814760073381,3.2805505448422E-14));
#130504=DIRECTION('ref_axis',(0.855538223403851,0.181850263143999,0.484752338921063));
#130505=DIRECTION('',(-0.518344583061401,-0.110177542335806,-0.848044693619236));
#130506=DIRECTION('',(0.978147600733806,0.20791169081776,1.44876238996227E-15));
#130507=DIRECTION('',(-0.518344070249267,-0.110177433334231,0.848045021223109));
#130508=DIRECTION('center_axis',(0.207911690817745,-0.978147600733809,-5.5135315871643E-14));
#130509=DIRECTION('ref_axis',(0.855536389092617,0.181849873249127,-0.48475572254244));
#130510=DIRECTION('',(-0.978147600733806,-0.20791169081776,-1.58957929685218E-15));
#130511=DIRECTION('',(-0.489078703542047,-0.103956887610915,-0.866022509672747));
#130512=DIRECTION('center_axis',(-0.207910764672755,0.97814779759017,-1.63998884845435E-6));
#130513=DIRECTION('ref_axis',(0.847146577517719,0.180066563577246,0.499918702272176));
#130514=DIRECTION('',(-0.978147600733806,-0.20791169081776,-1.58957929685218E-15));
#130515=DIRECTION('center_axis',(-0.207912617049438,0.978147403855351,-1.64014399912025E-6));
#130516=DIRECTION('ref_axis',(0.847118160900897,0.180060523667102,-0.499969028329366));
#130517=DIRECTION('',(-0.489078856702207,-0.10395692016612,0.866022419268945));
#130518=DIRECTION('',(-0.978147600733806,-0.20791169081776,-1.58957929685218E-15));
#130519=DIRECTION('center_axis',(0.20791169081776,-0.978147600733806,-6.80109070798532E-15));
#130520=DIRECTION('ref_axis',(3.07718727278892E-18,6.95368519647906E-15,
-1.));
#130521=DIRECTION('center_axis',(-0.207911690817755,0.978147600733807,2.12270966081019E-14));
#130522=DIRECTION('ref_axis',(0.855536389075087,0.181849873245393,-0.484755722574778));
#130523=DIRECTION('',(0.518344070249257,0.110177433334232,-0.848045021223115));
#130524=DIRECTION('',(-0.978147600733806,-0.20791169081776,-1.44876238996227E-15));
#130525=DIRECTION('',(0.518344583061396,0.110177542335808,0.848044693619239));
#130526=DIRECTION('center_axis',(-0.207911690817758,0.978147600733806,-5.58244945724969E-15));
#130527=DIRECTION('ref_axis',(0.855538223421779,0.181850263147814,0.48475233888799));
#130528=DIRECTION('',(0.978147600733806,0.20791169081776,1.58957929685218E-15));
#130529=DIRECTION('',(0.489078856702179,0.10395692016613,-0.86602241926896));
#130530=DIRECTION('center_axis',(0.207910764457463,-0.978147797635931,-1.64037042063166E-6));
#130531=DIRECTION('ref_axis',(0.847146677960003,0.180066584926648,-0.499918524375908));
#130532=DIRECTION('',(0.978147600733806,0.20791169081776,1.58957929685218E-15));
#130533=DIRECTION('center_axis',(0.207912616842675,-0.978147403899301,-1.63977751440231E-6));
#130534=DIRECTION('ref_axis',(0.847118057016758,0.180060501585604,0.499969212297011));
#130535=DIRECTION('',(0.489078703542037,0.103956887610914,0.866022509672752));
#130536=DIRECTION('',(0.978147600733806,0.20791169081776,1.58957929685218E-15));
#130537=DIRECTION('center_axis',(-6.89206998773325E-18,-6.93944786036197E-15,
1.));
#130538=DIRECTION('ref_axis',(0.,-1.,-6.93944786036197E-15));
#130539=DIRECTION('',(0.951056516295153,0.309016994374948,2.15096206850332E-15));
#130540=DIRECTION('center_axis',(6.89206998773325E-18,6.93944786036197E-15,
-1.));
#130541=DIRECTION('ref_axis',(-6.04138961080025E-12,-1.,-6.93944786036201E-15));
#130542=DIRECTION('',(-0.951056516295153,-0.309016994374948,-2.15096206850332E-15));
#130543=DIRECTION('center_axis',(-6.89206998773325E-18,-6.93944786036197E-15,
1.));
#130544=DIRECTION('ref_axis',(-2.36830503925458E-35,-1.,-6.93944786036197E-15));
#130545=DIRECTION('center_axis',(0.309016994374948,-0.951056516295153,-6.59767734033508E-15));
#130546=DIRECTION('ref_axis',(6.89206998773322E-18,6.93944786036197E-15,
-1.));
#130547=DIRECTION('center_axis',(0.309016994374975,-0.951056516295145,-5.00352877217599E-14));
#130548=DIRECTION('ref_axis',(0.831842966947628,0.270282164134104,0.484752338922417));
#130549=DIRECTION('',(-0.503988348013119,-0.163755740941345,-0.848044693619245));
#130550=DIRECTION('',(0.951056516295153,0.309016994374948,2.15096206850332E-15));
#130551=DIRECTION('',(-0.503987849403997,-0.163755578933432,0.848045021223113));
#130552=DIRECTION('center_axis',(0.309016994374943,-0.951056516295155,-1.8608169106679E-14));
#130553=DIRECTION('ref_axis',(0.831841183440077,0.270281584637376,-0.484755722543759));
#130554=DIRECTION('',(-0.951056516295153,-0.309016994374948,-2.29177897539323E-15));
#130555=DIRECTION('',(-0.47553302552285,-0.154510046201597,-0.866022509672736));
#130556=DIRECTION('center_axis',(-0.30901609388053,0.951056808881641,-1.63998886386027E-6));
#130557=DIRECTION('ref_axis',(0.823683738752015,0.26763107001197,0.499918702270429));
#130558=DIRECTION('',(-0.951056516295153,-0.309016994374948,-2.29177897539323E-15));
#130559=DIRECTION('center_axis',(-0.30901789495323,0.951056223677646,-1.64014403819393E-6));
#130560=DIRECTION('ref_axis',(0.823656109144305,0.267622092842945,-0.499969028332382));
#130561=DIRECTION('',(-0.475533174441002,-0.154510094588054,0.866022419268955));
#130562=DIRECTION('',(-0.951056516295153,-0.309016994374948,-2.29177897539323E-15));
#130563=DIRECTION('center_axis',(0.309016994374948,-0.951056516295153,-6.59767734033508E-15));
#130564=DIRECTION('ref_axis',(6.89206998773322E-18,6.93944786036197E-15,
-1.));
#130565=DIRECTION('center_axis',(-0.309016994374928,0.95105651629516,3.79055296573235E-14));
#130566=DIRECTION('ref_axis',(0.831841183424877,0.270281584632433,-0.484755722572598));
#130567=DIRECTION('',(0.503987849404017,0.163755578933437,-0.848045021223101));
#130568=DIRECTION('',(-0.951056516295153,-0.309016994374948,-2.15096206850332E-15));
#130569=DIRECTION('',(0.503988348013119,0.163755740941342,0.848044693619245));
#130570=DIRECTION('center_axis',(-0.309016994374936,0.951056516295157,-1.18540902055188E-14));
#130571=DIRECTION('ref_axis',(0.831842966965641,0.27028216413995,0.484752338888245));
#130572=DIRECTION('',(0.951056516295153,0.309016994374948,2.29177897539323E-15));
#130573=DIRECTION('',(0.475533174441018,0.154510094588057,-0.866022419268946));
#130574=DIRECTION('center_axis',(0.309016093671233,-0.951056808949645,-1.64037046624666E-6));
#130575=DIRECTION('ref_axis',(0.823683836411332,0.267631101743181,-0.499918524376164));
#130576=DIRECTION('',(0.951056516295153,0.309016994374948,2.29177897539323E-15));
#130577=DIRECTION('center_axis',(0.309017894752258,-0.951056223742947,-1.639777670527E-6));
#130578=DIRECTION('ref_axis',(0.823656008138232,0.267622060023833,0.49996921229851));
#130579=DIRECTION('',(0.475533025522778,0.154510046201593,0.866022509672777));
#130580=DIRECTION('',(0.951056516295153,0.309016994374948,2.29177897539323E-15));
#130581=DIRECTION('center_axis',(-1.21742612413517E-17,-6.92568728168955E-15,
1.));
#130582=DIRECTION('ref_axis',(0.,-1.,-6.92568728168955E-15));
#130583=DIRECTION('',(0.913545457642601,0.406736643075801,2.82805253700437E-15));
#130584=DIRECTION('center_axis',(1.21742612413517E-17,6.92568728168955E-15,
-1.));
#130585=DIRECTION('ref_axis',(-3.11436113529516E-35,-1.,-6.92568728168955E-15));
#130586=DIRECTION('',(-0.913545457642601,-0.406736643075801,-2.82805253700437E-15));
#130587=DIRECTION('center_axis',(-1.21742612413517E-17,-6.92568728168955E-15,
1.));
#130588=DIRECTION('ref_axis',(-3.04711942787957E-35,-1.,-6.92568728168955E-15));
#130589=DIRECTION('center_axis',(0.406736643075801,-0.913545457642601,-6.32197843909138E-15));
#130590=DIRECTION('ref_axis',(1.21742612413516E-17,6.92568728168955E-15,
-1.));
#130591=DIRECTION('center_axis',(0.406736643075802,-0.9135454576426,1.92973561461327E-15));
#130592=DIRECTION('ref_axis',(0.799033864871343,0.355752797173669,0.484752338923573));
#130593=DIRECTION('',(-0.484110311157683,-0.21553979738103,-0.848044693619243));
#130594=DIRECTION('',(0.913545457642601,0.406736643075801,2.82805253700437E-15));
#130595=DIRECTION('',(-0.484109832214428,-0.215539584141767,0.848045021223115));
#130596=DIRECTION('center_axis',(0.406736643075783,-0.913545457642609,-5.80299199549056E-14));
#130597=DIRECTION('ref_axis',(0.799032151707775,0.355752034424116,-0.484755722545228));
#130598=DIRECTION('',(-0.913545457642601,-0.406736643075801,-2.96886944389428E-15));
#130599=DIRECTION('',(-0.456777308164342,-0.20337036039276,-0.866022509672732));
#130600=DIRECTION('center_axis',(-0.40673577809802,0.913545842753558,-1.63998889148739E-6));
#130601=DIRECTION('ref_axis',(0.791196448577878,0.352263354438628,0.499918702268077));
#130602=DIRECTION('',(-0.913545457642601,-0.406736643075801,-2.96886944389428E-15));
#130603=DIRECTION('center_axis',(-0.406737508133751,0.913545072492024,-1.6401440001529E-6));
#130604=DIRECTION('ref_axis',(0.791169908694268,0.352251538365472,-0.499969028336619));
#130605=DIRECTION('',(-0.45677745120893,-0.203370424080359,0.866022419268952));
#130606=DIRECTION('',(-0.913545457642601,-0.406736643075801,-2.96886944389428E-15));
#130607=DIRECTION('center_axis',(0.406736643075801,-0.913545457642601,-6.32197843909138E-15));
#130608=DIRECTION('ref_axis',(1.21742612413516E-17,6.92568728168955E-15,
-1.));
#130609=DIRECTION('center_axis',(-0.406736643075821,0.913545457642592,-5.01731374373314E-14));
#130610=DIRECTION('ref_axis',(0.799032151693526,0.355752034417755,-0.484755722573383));
#130611=DIRECTION('',(0.484109832214453,0.215539584141773,-0.848045021223098));
#130612=DIRECTION('',(-0.913545457642601,-0.406736643075801,-2.82805253700437E-15));
#130613=DIRECTION('',(0.484110311157685,0.215539797381037,0.84804469361924));
#130614=DIRECTION('center_axis',(-0.406736643075817,0.913545457642593,4.39704043669841E-14));
#130615=DIRECTION('ref_axis',(0.799033864889297,0.355752797181655,0.484752338888119));
#130616=DIRECTION('',(0.9135454576426,0.406736643075801,2.96886944389428E-15));
#130617=DIRECTION('',(0.45677745120893,0.203370424080376,-0.866022419268948));
#130618=DIRECTION('center_axis',(0.406735777896989,-0.913545842843062,-1.64037036589386E-6));
#130619=DIRECTION('ref_axis',(0.791196542384911,0.352263396203918,-0.499918524374765));
#130620=DIRECTION('',(0.913545457642601,0.406736643075801,2.96886944389428E-15));
#130621=DIRECTION('center_axis',(0.406737507940689,-0.913545072577981,-1.63977759702633E-6));
#130622=DIRECTION('ref_axis',(0.791169811673513,0.352251495168791,0.499969212299967));
#130623=DIRECTION('',(0.45677730816427,0.203370360392743,0.866022509672774));
#130624=DIRECTION('',(0.913545457642601,0.406736643075801,2.96886944389428E-15));
#130625=DIRECTION('center_axis',(-1.88658882409001E-17,-6.91255422424131E-15,
1.));
#130626=DIRECTION('ref_axis',(0.,-1.,-6.91255422424131E-15));
#130627=DIRECTION('',(0.866025403784438,0.500000000000001,3.47261545060224E-15));
#130628=DIRECTION('center_axis',(1.88658882409001E-17,6.91255422424131E-15,
-1.));
#130629=DIRECTION('ref_axis',(3.83604259468484E-12,-1.,-6.91255422424124E-15));
#130630=DIRECTION('',(-0.866025403784438,-0.500000000000001,-3.47261545060224E-15));
#130631=DIRECTION('center_axis',(-1.88658882409001E-17,-6.91255422424131E-15,
1.));
#130632=DIRECTION('ref_axis',(-1.77724617242827E-35,-1.,-6.91255422424131E-15));
#130633=DIRECTION('center_axis',(0.500000000000001,-0.866025403784438,-5.97701461910995E-15));
#130634=DIRECTION('ref_axis',(1.88658882408999E-17,6.91255422424131E-15,
-1.));
#130635=DIRECTION('center_axis',(0.500000000000029,-0.866025403784422,-5.32055676600525E-14));
#130636=DIRECTION('ref_axis',(0.757470380563957,0.437325728121773,0.484752338922729));
#130637=DIRECTION('',(-0.458928260426595,-0.264962354696009,-0.848044693619249));
#130638=DIRECTION('',(0.866025403784438,0.500000000000001,3.47261545060224E-15));
#130639=DIRECTION('',(-0.458927806396613,-0.264962092561708,0.848045021223115));
#130640=DIRECTION('center_axis',(0.500000000000022,-0.866025403784426,2.06757434518667E-14));
#130641=DIRECTION('ref_axis',(0.757468756514555,0.437324790476423,-0.484755722543887));
#130642=DIRECTION('',(-0.866025403784438,-0.500000000000001,-3.61343235749215E-15));
#130643=DIRECTION('',(-0.433017043030787,-0.250002506357499,-0.866022509672723));
#130644=DIRECTION('center_axis',(-0.499999180015709,0.86602587720052,-1.63998889217594E-6));
#130645=DIRECTION('ref_axis',(0.750040644542496,0.433036167837267,0.499918702269771));
#130646=DIRECTION('',(-0.866025403784438,-0.500000000000001,-3.61343235749215E-15));
#130647=DIRECTION('center_axis',(-0.500000820059939,0.866024930320542,-1.64014409121096E-6));
#130648=DIRECTION('ref_axis',(0.750015485167105,0.433021642322879,-0.499969028330305));
#130649=DIRECTION('',(-0.433017178634592,-0.25000258464845,0.866022419268943));
#130650=DIRECTION('',(-0.866025403784438,-0.500000000000001,-3.61343235749215E-15));
#130651=DIRECTION('center_axis',(0.500000000000001,-0.866025403784438,-5.97701461910995E-15));
#130652=DIRECTION('ref_axis',(1.88658882408999E-17,6.91255422424131E-15,
-1.));
#130653=DIRECTION('center_axis',(-0.499999999999999,0.866025403784439,1.32324758076477E-14));
#130654=DIRECTION('ref_axis',(0.757468756499566,0.437324790467762,-0.484755722575123));
#130655=DIRECTION('',(0.458927806396622,0.264962092561705,-0.848045021223111));
#130656=DIRECTION('',(-0.866025403784438,-0.500000000000001,-3.47261545060224E-15));
#130657=DIRECTION('',(0.458928260426604,0.26496235469602,0.848044693619241));
#130658=DIRECTION('center_axis',(-0.500000000000014,0.866025403784431,3.62514619075765E-14));
#130659=DIRECTION('ref_axis',(0.75747038058095,0.437325728131575,0.484752338887332));
#130660=DIRECTION('',(0.866025403784438,0.500000000000001,3.61343235749215E-15));
#130661=DIRECTION('',(0.433017178634604,0.25000258464844,-0.866022419268939));
#130662=DIRECTION('center_axis',(0.499999179825138,-0.866025877310545,-1.64037034781974E-6));
#130663=DIRECTION('ref_axis',(0.750040733469403,0.433036219178925,-0.499918524377625));
#130664=DIRECTION('',(0.866025403784438,0.500000000000001,3.61343235749215E-15));
#130665=DIRECTION('center_axis',(0.500000819876823,-0.866024930426264,-1.63977751905006E-6));
#130666=DIRECTION('ref_axis',(0.750015393191207,0.433021589220285,0.499969212297495));
#130667=DIRECTION('',(0.433017043030726,0.250002506357484,0.866022509672758));
#130668=DIRECTION('',(0.866025403784438,0.500000000000001,3.61343235749215E-15));
#130669=DIRECTION('center_axis',(-2.68936361206584E-17,-6.90019257654293E-15,
1.));
#130670=DIRECTION('ref_axis',(0.,-1.,-6.90019257654294E-15));
#130671=DIRECTION('',(0.809016994374947,0.587785252292474,4.07758884313209E-15));
#130672=DIRECTION('center_axis',(2.68936361206584E-17,6.90019257654293E-15,
-1.));
#130673=DIRECTION('ref_axis',(-1.21098210448278E-35,-1.,-6.90019257654293E-15));
#130674=DIRECTION('',(-0.809016994374947,-0.587785252292474,-4.07758884313209E-15));
#130675=DIRECTION('center_axis',(-2.68936361206584E-17,-6.90019257654293E-15,
1.));
#130676=DIRECTION('ref_axis',(3.73887388675131E-35,-1.,-6.90019257654293E-15));
#130677=DIRECTION('center_axis',(0.587785252292474,-0.809016994374947,-5.56656537619084E-15));
#130678=DIRECTION('ref_axis',(2.6893636120658E-17,6.90019257654294E-15,
-1.));
#130679=DIRECTION('center_axis',(0.587785252292488,-0.809016994374937,-2.2605474342611E-14));
#130680=DIRECTION('ref_axis',(0.707607892256329,0.514107226876464,0.484752338921584));
#130681=DIRECTION('',(-0.428718095637387,-0.311481929006017,-0.848044693619235));
#130682=DIRECTION('',(0.809016994374947,0.587785252292474,4.07758884313209E-15));
#130683=DIRECTION('',(-0.428717671495138,-0.311481620848666,0.848045021223092));
#130684=DIRECTION('center_axis',(0.587785252292496,-0.809016994374931,6.42326429904636E-14));
#130685=DIRECTION('ref_axis',(0.707606375113785,0.514106124607871,-0.484755722543847));
#130686=DIRECTION('',(-0.809016994374947,-0.587785252292474,-4.21840575002201E-15));
#130687=DIRECTION('',(-0.404512552559103,-0.293895572546151,-0.86602250967275));
#130688=DIRECTION('center_axis',(-0.587784486285606,0.809017550909297,-1.63998889613513E-6));
#130689=DIRECTION('ref_axis',(0.700667238250726,0.509064546363162,0.499918702268848));
#130690=DIRECTION('',(-0.809016994374947,-0.587785252292474,-4.21840575002201E-15));
#130691=DIRECTION('center_axis',(-0.587786018369567,0.809016437785142,-1.6401440982681E-6));
#130692=DIRECTION('ref_axis',(0.700643735030324,0.509047470549884,-0.499969028330278));
#130693=DIRECTION('',(-0.404512679236431,-0.293895664582696,0.866022419268959));
#130694=DIRECTION('',(-0.809016994374947,-0.587785252292474,-4.21840575002201E-15));
#130695=DIRECTION('center_axis',(0.587785252292474,-0.809016994374947,-5.56656537619084E-15));
#130696=DIRECTION('ref_axis',(2.6893636120658E-17,6.90019257654294E-15,
-1.));
#130697=DIRECTION('center_axis',(-0.587785252292482,0.809016994374941,-9.09732711775792E-15));
#130698=DIRECTION('ref_axis',(0.707606375100825,0.514106124598469,-0.484755722572735));
#130699=DIRECTION('',(0.428717671495133,0.311481620848643,-0.848045021223103));
#130700=DIRECTION('',(-0.809016994374947,-0.587785252292474,-4.07758884313209E-15));
#130701=DIRECTION('',(0.428718095637375,0.311481929006018,0.848044693619241));
#130702=DIRECTION('center_axis',(-0.587785252292472,0.809016994374949,2.06757387305573E-15));
#130703=DIRECTION('ref_axis',(0.707607892271538,0.514107226887505,0.484752338887674));
#130704=DIRECTION('',(0.809016994374947,0.587785252292474,4.21840575002201E-15));
#130705=DIRECTION('',(0.404512679236465,0.293895664582661,-0.866022419268954));
#130706=DIRECTION('center_axis',(0.587784486107541,-0.809017551038668,-1.64037047777937E-6));
#130707=DIRECTION('ref_axis',(0.700667321324406,0.509064606719412,-0.499918524375414));
#130708=DIRECTION('',(0.809016994374947,0.587785252292474,4.21840575002201E-15));
#130709=DIRECTION('center_axis',(0.587786018198601,-0.809016437909357,-1.63977768550205E-6));
#130710=DIRECTION('ref_axis',(0.700643649108103,0.509047408123459,0.499969212299387));
#130711=DIRECTION('',(0.404512552559084,0.293895572546173,0.866022509672752));
#130712=DIRECTION('',(0.809016994374947,0.587785252292474,4.21840575002201E-15));
#130713=DIRECTION('center_axis',(-3.61695511949416E-17,-6.88873777539344E-15,
1.));
#130714=DIRECTION('ref_axis',(0.,-1.,-6.88873777539344E-15));
#130715=DIRECTION('',(0.743144825477393,0.669130606358859,4.63634449950655E-15));
#130716=DIRECTION('center_axis',(3.61695511949416E-17,6.88873777539344E-15,
-1.));
#130717=DIRECTION('ref_axis',(6.85846605685609E-35,-1.,-6.88873777539344E-15));
#130718=DIRECTION('',(-0.743144825477393,-0.669130606358859,-4.63634449950655E-15));
#130719=DIRECTION('center_axis',(-3.61695511949416E-17,-6.88873777539344E-15,
1.));
#130720=DIRECTION('ref_axis',(-9.8293973350875E-35,-1.,-6.88873777539344E-15));
#130721=DIRECTION('center_axis',(0.669130606358859,-0.743144825477393,-5.09512767813149E-15));
#130722=DIRECTION('ref_axis',(3.61695511949414E-17,6.88873777539344E-15,
-1.));
#130723=DIRECTION('center_axis',(0.669130606358863,-0.74314482547739,2.56379160227189E-14));
#130724=DIRECTION('ref_axis',(0.649992703803497,0.585256059268782,0.484752338923078));
#130725=DIRECTION('',(-0.393810805677315,-0.354588842120017,-0.848044693619251));
#130726=DIRECTION('',(0.743144825477393,0.669130606358859,4.63634449950655E-15));
#130727=DIRECTION('',(-0.393810416069769,-0.354588491315852,0.848045021223109));
#130728=DIRECTION('center_axis',(0.669130606358859,-0.743144825477393,4.41082526973097E-15));
#130729=DIRECTION('ref_axis',(0.649991310190666,0.585254804454127,-0.484755722544853));
#130730=DIRECTION('',(-0.743144825477393,-0.669130606358859,-4.77716140639646E-15));
#130731=DIRECTION('',(-0.3715761379119,-0.334568657340434,-0.866022509672754));
#130732=DIRECTION('center_axis',(-0.669129902721922,0.743145459032525,-1.63998885774954E-6));
#130733=DIRECTION('ref_axis',(0.643617175072105,0.579515507190106,0.499918702269076));
#130734=DIRECTION('',(-0.743144825477393,-0.669130606358859,-4.77716140639646E-15));
#130735=DIRECTION('center_axis',(-0.669131310059706,0.743144191859892,-1.64014388379194E-6));
#130736=DIRECTION('ref_axis',(0.64359558551269,0.579496068163846,-0.499969028331978));
#130737=DIRECTION('',(-0.371576254274913,-0.33456876211417,0.866022419268934));
#130738=DIRECTION('',(-0.743144825477393,-0.669130606358859,-4.77716140639646E-15));
#130739=DIRECTION('center_axis',(0.669130606358859,-0.743144825477393,-5.09512767813149E-15));
#130740=DIRECTION('ref_axis',(3.61695511949414E-17,6.88873777539344E-15,
-1.));
#130741=DIRECTION('center_axis',(-0.669130606358859,0.743144825477393,-3.225415978114E-14));
#130742=DIRECTION('ref_axis',(0.649991310179485,0.585254804444041,-0.484755722572022));
#130743=DIRECTION('',(0.393810416069769,0.354588491315851,-0.84804502122311));
#130744=DIRECTION('',(-0.743144825477393,-0.669130606358859,-4.63634449950655E-15));
#130745=DIRECTION('',(0.393810805677318,0.354588842120046,0.848044693619238));
#130746=DIRECTION('center_axis',(-0.669130606358895,0.743144825477361,1.30119315744295E-13));
#130747=DIRECTION('ref_axis',(0.649992703818358,0.585256059282112,0.484752338887059));
#130748=DIRECTION('',(0.743144825477393,0.669130606358859,4.77716140639646E-15));
#130749=DIRECTION('',(0.371576254274905,0.334568762114163,-0.86602241926894));
#130750=DIRECTION('center_axis',(0.66912990255837,-0.743145459179787,-1.64037045350906E-6));
#130751=DIRECTION('ref_axis',(0.643617251380043,0.579515575897775,-0.499918524379592));
#130752=DIRECTION('',(0.743144825477393,0.669130606358859,4.77716140639646E-15));
#130753=DIRECTION('center_axis',(0.669131309902701,-0.743144192001261,-1.63977754710756E-6));
#130754=DIRECTION('ref_axis',(0.643595506588125,0.579495997099558,0.499969212297282));
#130755=DIRECTION('',(0.371576137911895,0.334568657340433,0.866022509672757));
#130756=DIRECTION('',(0.743144825477393,0.669130606358859,4.77716140639646E-15));
#130757=DIRECTION('center_axis',(-4.6592004597086E-17,-6.8783153219913E-15,
1.));
#130758=DIRECTION('ref_axis',(0.,-1.,-6.8783153219913E-15));
#130759=DIRECTION('',(0.669130606358857,0.743144825477395,5.14276057582724E-15));
#130760=DIRECTION('center_axis',(4.6592004597086E-17,6.8783153219913E-15,
-1.));
#130761=DIRECTION('ref_axis',(3.5473846082823E-12,-1.,-6.87831532199113E-15));
#130762=DIRECTION('',(-0.669130606358857,-0.743144825477395,-5.14276057582724E-15));
#130763=DIRECTION('center_axis',(-4.6592004597086E-17,-6.8783153219913E-15,
1.));
#130764=DIRECTION('ref_axis',(7.23989575295994E-35,-1.,-6.8783153219913E-15));
#130765=DIRECTION('center_axis',(0.743144825477395,-0.669130606358857,-4.56786669500651E-15));
#130766=DIRECTION('ref_axis',(4.65920045970859E-17,6.8783153219913E-15,
-1.));
#130767=DIRECTION('center_axis',(0.743144825477392,-0.66913060635886,4.24541835214864E-14));
#130768=DIRECTION('ref_axis',(0.585256059269044,0.649992703803843,0.484752338922299));
#130769=DIRECTION('',(-0.354588842120053,-0.393810805677299,-0.848044693619244));
#130770=DIRECTION('',(0.669130606358857,0.743144825477395,5.14276057582724E-15));
#130771=DIRECTION('',(-0.354588491315835,-0.393810416069765,0.848045021223118));
#130772=DIRECTION('center_axis',(0.743144825477363,-0.669130606358893,-8.68381224978382E-14));
#130773=DIRECTION('ref_axis',(0.585254804454296,0.649991310190854,-0.484755722544398));
#130774=DIRECTION('',(-0.669130606358857,-0.743144825477395,-5.28357748271715E-15));
#130775=DIRECTION('',(-0.334568657340461,-0.371576137911926,-0.866022509672733));
#130776=DIRECTION('center_axis',(-0.743144191919596,0.669131309993398,-1.6399889042252E-6));
#130777=DIRECTION('ref_axis',(0.579515507436744,0.643617174847681,0.499918702272102));
#130778=DIRECTION('',(-0.669130606358857,-0.743144825477395,-5.28357748271715E-15));
#130779=DIRECTION('center_axis',(-0.743145459092377,0.669129902655449,-1.64014418399028E-6));
#130780=DIRECTION('ref_axis',(0.579496068079923,0.643595585588318,-0.499969028331896));
#130781=DIRECTION('',(-0.334568762114163,-0.371576254274904,0.86602241926894));
#130782=DIRECTION('',(-0.669130606358857,-0.743144825477395,-5.28357748271715E-15));
#130783=DIRECTION('center_axis',(0.743144825477395,-0.669130606358857,-4.56786669500651E-15));
#130784=DIRECTION('ref_axis',(4.65920045970859E-17,6.8783153219913E-15,
-1.));
#130785=DIRECTION('center_axis',(-0.743144825477411,0.66913060635884,-6.75407619348667E-14));
#130786=DIRECTION('ref_axis',(0.585254804443858,0.649991310179243,-0.484755722572568));
#130787=DIRECTION('',(0.354588491315848,0.393810416069791,-0.848045021223101));
#130788=DIRECTION('',(-0.669130606358857,-0.743144825477395,-5.14276057582724E-15));
#130789=DIRECTION('',(0.354588842120031,0.393810805677304,0.84804469361925));
#130790=DIRECTION('center_axis',(-0.743144825477382,0.669130606358872,-2.1227091763372E-14));
#130791=DIRECTION('ref_axis',(0.585256059281954,0.649992703818144,0.484752338887536));
#130792=DIRECTION('',(0.669130606358857,0.743144825477395,5.28357748271715E-15));
#130793=DIRECTION('',(0.334568762114167,0.371576254274874,-0.866022419268952));
#130794=DIRECTION('center_axis',(0.743144191772429,-0.669131310156843,-1.64037028413086E-6));
#130795=DIRECTION('ref_axis',(0.579515576147915,0.643617251158851,-0.499918524374397));
#130796=DIRECTION('',(0.669130606358857,0.743144825477395,5.28357748271715E-15));
#130797=DIRECTION('center_axis',(0.743145458950857,-0.669129902812624,-1.63977741490995E-6));
#130798=DIRECTION('ref_axis',(0.57949599701582,0.643595506663342,0.499969212297514));
#130799=DIRECTION('',(0.334568657340468,0.37157613791193,0.866022509672728));
#130800=DIRECTION('',(0.669130606358857,0.743144825477395,5.28357748271715E-15));
#130801=DIRECTION('center_axis',(-5.8046805746579E-17,-6.86903940691701E-15,
1.));
#130802=DIRECTION('ref_axis',(0.,-1.,-6.86903940691702E-15));
#130803=DIRECTION('',(0.587785252292471,0.809016994374949,5.59128867158761E-15));
#130804=DIRECTION('center_axis',(5.8046805746579E-17,6.86903940691701E-15,
-1.));
#130805=DIRECTION('ref_axis',(1.68321743785256E-34,-1.,-6.86903940691701E-15));
#130806=DIRECTION('',(-0.587785252292471,-0.809016994374949,-5.59128867158761E-15));
#130807=DIRECTION('center_axis',(-5.8046805746579E-17,-6.86903940691701E-15,
1.));
#130808=DIRECTION('ref_axis',(-2.17707695431367E-35,-1.,-6.86903940691701E-15));
#130809=DIRECTION('center_axis',(0.809016994374949,-0.587785252292471,-3.99055920848348E-15));
#130810=DIRECTION('ref_axis',(5.80468057465793E-17,6.86903940691702E-15,
-1.));
#130811=DIRECTION('center_axis',(0.809016994374951,-0.587785252292468,-1.46108553677859E-14));
#130812=DIRECTION('ref_axis',(0.514107226876147,0.707607892255898,0.484752338922551));
#130813=DIRECTION('',(-0.311481929006009,-0.428718095637372,-0.848044693619246));
#130814=DIRECTION('',(0.587785252292471,0.809016994374949,5.59128867158761E-15));
#130815=DIRECTION('',(-0.311481620848641,-0.428717671495144,0.848045021223099));
#130816=DIRECTION('center_axis',(0.809016994374939,-0.587785252292485,-3.92839125585453E-14));
#130817=DIRECTION('ref_axis',(0.514106124607336,0.707606375113047,-0.48475572254549));
#130818=DIRECTION('',(-0.587785252292471,-0.809016994374949,-5.73210557847752E-15));
#130819=DIRECTION('',(-0.293895572546214,-0.404512552559082,-0.866022509672739));
#130820=DIRECTION('center_axis',(-0.809016437837686,0.587786018297248,-1.63998888511843E-6));
#130821=DIRECTION('ref_axis',(0.509064546633241,0.7006672380552,0.499918702267869));
#130822=DIRECTION('',(-0.587785252292471,-0.809016994374949,-5.73210557847752E-15));
#130823=DIRECTION('center_axis',(-0.809017550961786,0.587784486213361,-1.64014389411998E-6));
#130824=DIRECTION('ref_axis',(0.509047470457493,0.700643735095407,-0.499969028333141));
#130825=DIRECTION('',(-0.293895664582667,-0.404512679236475,0.866022419268948));
#130826=DIRECTION('',(-0.587785252292471,-0.809016994374949,-5.73210557847752E-15));
#130827=DIRECTION('center_axis',(0.809016994374949,-0.587785252292471,-3.99055920848348E-15));
#130828=DIRECTION('ref_axis',(5.80468057465793E-17,6.86903940691702E-15,
-1.));
#130829=DIRECTION('center_axis',(-0.80901699437496,0.587785252292456,-5.37569329685675E-14));
#130830=DIRECTION('ref_axis',(0.514106124598334,0.707606375100633,-0.484755722573158));
#130831=DIRECTION('',(0.311481620848638,0.428717671495152,-0.848045021223095));
#130832=DIRECTION('',(-0.587785252292471,-0.809016994374949,-5.59128867158761E-15));
#130833=DIRECTION('',(0.311481929006021,0.428718095637366,0.848044693619245));
#130834=DIRECTION('center_axis',(-0.809016994374947,0.587785252292474,1.47486936277971E-14));
#130835=DIRECTION('ref_axis',(0.514107226887317,0.70760789227126,0.48475233888828));
#130836=DIRECTION('',(0.587785252292471,0.809016994374949,5.73210557847752E-15));
#130837=DIRECTION('',(0.293895664582692,0.40451267923646,-0.866022419268946));
#130838=DIRECTION('center_axis',(0.809016437708317,-0.587786018475307,-1.6403705029113E-6));
#130839=DIRECTION('ref_axis',(0.509064606990388,0.700667321129299,-0.499918524372936));
#130840=DIRECTION('',(0.587785252292471,0.809016994374949,5.73210557847752E-15));
#130841=DIRECTION('center_axis',(0.809017550837637,-0.587784486384239,-1.6397776906657E-6));
#130842=DIRECTION('ref_axis',(0.509047408032981,0.700643649175039,0.499969212297706));
#130843=DIRECTION('',(0.293895572546198,0.40451255255907,0.86602250967275));
#130844=DIRECTION('',(0.587785252292471,0.809016994374949,5.73210557847752E-15));
#130845=DIRECTION('center_axis',(-7.04084534449555E-17,-6.86101165903726E-15,
1.));
#130846=DIRECTION('ref_axis',(0.,-1.,-6.86101165903726E-15));
#130847=DIRECTION('',(0.499999999999998,0.86602540378444,5.97701461910997E-15));
#130848=DIRECTION('center_axis',(7.04084534449556E-17,6.86101165903726E-15,
-1.));
#130849=DIRECTION('ref_axis',(1.24809821036928E-34,-1.,-6.86101165903726E-15));
#130850=DIRECTION('',(-0.499999999999998,-0.86602540378444,-5.97701461910997E-15));
#130851=DIRECTION('center_axis',(-7.04084534449556E-17,-6.86101165903726E-15,
1.));
#130852=DIRECTION('ref_axis',(-7.43397775866882E-35,-1.,-6.86101165903726E-15));
#130853=DIRECTION('center_axis',(0.86602540378444,-0.499999999999998,-3.36953032019411E-15));
#130854=DIRECTION('ref_axis',(7.04084534449556E-17,6.86101165903726E-15,
-1.));
#130855=DIRECTION('center_axis',(0.866025403784421,-0.50000000000003,5.81677449547759E-14));
#130856=DIRECTION('ref_axis',(0.437325728121601,0.757470380563662,0.484752338923344));
#130857=DIRECTION('',(-0.264962354696014,-0.458928260426592,-0.848044693619249));
#130858=DIRECTION('',(0.499999999999998,0.86602540378444,5.97701461910997E-15));
#130859=DIRECTION('',(-0.264962092561698,-0.458927806396633,0.848045021223108));
#130860=DIRECTION('center_axis',(0.86602540378445,-0.49999999999998,3.34947043920223E-14));
#130861=DIRECTION('ref_axis',(0.437324790476197,0.757468756514194,-0.484755722544655));
#130862=DIRECTION('',(-0.499999999999998,-0.86602540378444,-6.11783152599987E-15));
#130863=DIRECTION('',(-0.250002506357479,-0.433017043030743,-0.866022509672751));
#130864=DIRECTION('center_axis',(-0.866024930365256,0.500000819982492,-1.63998893916804E-6));
#130865=DIRECTION('ref_axis',(0.433036168126024,0.750040644375844,0.499918702269678));
#130866=DIRECTION('',(-0.499999999999998,-0.86602540378444,-6.11783152599987E-15));
#130867=DIRECTION('center_axis',(-0.866025877245197,0.499999179938324,-1.64014403630087E-6));
#130868=DIRECTION('ref_axis',(0.433021642223467,0.750015485220938,-0.499969028335648));
#130869=DIRECTION('',(-0.250002584648417,-0.433017178634595,0.866022419268951));
#130870=DIRECTION('',(-0.499999999999998,-0.86602540378444,-6.11783152599987E-15));
#130871=DIRECTION('center_axis',(0.86602540378444,-0.499999999999998,-3.36953032019411E-15));
#130872=DIRECTION('ref_axis',(7.04084534449556E-17,6.86101165903726E-15,
-1.));
#130873=DIRECTION('center_axis',(-0.86602540378442,0.500000000000033,5.65136987618391E-14));
#130874=DIRECTION('ref_axis',(0.43732479046754,0.757468756499181,-0.484755722575925));
#130875=DIRECTION('',(0.264962092561698,0.458927806396633,-0.848045021223108));
#130876=DIRECTION('',(-0.499999999999998,-0.86602540378444,-5.97701461910997E-15));
#130877=DIRECTION('',(0.264962354696018,0.458928260426587,0.84804469361925));
#130878=DIRECTION('center_axis',(-0.866025403784437,0.500000000000003,2.48108864766678E-15));
#130879=DIRECTION('ref_axis',(0.437325728131431,0.757470380580684,0.484752338887877));
#130880=DIRECTION('',(0.499999999999998,0.86602540378444,6.11783152599988E-15));
#130881=DIRECTION('',(0.250002584648414,0.43301717863459,-0.866022419268954));
#130882=DIRECTION('center_axis',(0.866024930255218,-0.500000820173081,-1.64037040324638E-6));
#130883=DIRECTION('ref_axis',(0.433036219468666,0.750040733303334,-0.499918524375804));
#130884=DIRECTION('',(0.499999999999998,0.86602540378444,6.11783152599987E-15));
#130885=DIRECTION('center_axis',(0.866025877139533,-0.499999180121342,-1.63977762112504E-6));
#130886=DIRECTION('ref_axis',(0.433021589122546,0.750015393246993,0.499969212298461));
#130887=DIRECTION('',(0.250002506357474,0.433017043030739,0.866022509672755));
#130888=DIRECTION('',(0.499999999999998,0.86602540378444,6.11783152599987E-15));
#130889=DIRECTION('center_axis',(-8.35415108931911E-17,-6.85432003203771E-15,
1.));
#130890=DIRECTION('ref_axis',(0.,-1.,-6.85432003203771E-15));
#130891=DIRECTION('',(0.406736643075798,0.913545457642602,6.29571232419492E-15));
#130892=DIRECTION('center_axis',(8.35415108931911E-17,6.85432003203771E-15,
-1.));
#130893=DIRECTION('ref_axis',(1.65551687784934E-34,-1.,-6.85432003203771E-15));
#130894=DIRECTION('',(-0.406736643075798,-0.913545457642602,-6.29571232419492E-15));
#130895=DIRECTION('center_axis',(-8.35415108931911E-17,-6.85432003203771E-15,
1.));
#130896=DIRECTION('ref_axis',(-3.34580098672039E-35,-1.,-6.85432003203771E-15));
#130897=DIRECTION('center_axis',(0.913545457642602,-0.406736643075798,-2.71158415259714E-15));
#130898=DIRECTION('ref_axis',(8.35415108931909E-17,6.85432003203771E-15,
-1.));
#130899=DIRECTION('center_axis',(0.913545457642599,-0.406736643075804,8.27029549119894E-16));
#130900=DIRECTION('ref_axis',(0.355752797174059,0.799033864872216,0.484752338921848));
#130901=DIRECTION('',(-0.215539797381028,-0.48411031115768,-0.848044693619246));
#130902=DIRECTION('',(0.406736643075798,0.913545457642602,6.29571232419492E-15));
#130903=DIRECTION('',(-0.215539584141774,-0.484109832214441,0.848045021223105));
#130904=DIRECTION('center_axis',(0.913545457642602,-0.406736643075797,6.89191448395568E-16));
#130905=DIRECTION('ref_axis',(0.355752034424597,0.79903215170889,-0.484755722543036));
#130906=DIRECTION('',(-0.406736643075798,-0.913545457642602,-6.43652923108483E-15));
#130907=DIRECTION('',(-0.203370360392777,-0.45677730816434,-0.866022509672729));
#130908=DIRECTION('center_axis',(-0.913545072528373,0.406737508052111,-1.63998884914257E-6));
#130909=DIRECTION('ref_axis',(0.352263354743096,0.791196448441969,0.499918702268634));
#130910=DIRECTION('',(-0.406736643075798,-0.913545457642602,-6.43652923108483E-15));
#130911=DIRECTION('center_axis',(-0.91354584278991,0.406735778016372,-1.64014401684982E-6));
#130912=DIRECTION('ref_axis',(0.352251538263059,0.791169908742093,-0.499969028333092));
#130913=DIRECTION('',(-0.203370424080347,-0.456777451208944,0.866022419268947));
#130914=DIRECTION('',(-0.406736643075798,-0.913545457642602,-6.43652923108483E-15));
#130915=DIRECTION('center_axis',(0.913545457642602,-0.406736643075798,-2.71158415259714E-15));
#130916=DIRECTION('ref_axis',(8.35415108931909E-17,6.85432003203771E-15,
-1.));
#130917=DIRECTION('center_axis',(-0.913545457642604,0.406736643075794,-2.48108921393404E-15));
#130918=DIRECTION('ref_axis',(0.355752034417932,0.799032151693926,-0.484755722572594));
#130919=DIRECTION('',(0.215539584141771,0.484109832214462,-0.848045021223094));
#130920=DIRECTION('',(-0.406736643075798,-0.913545457642602,-6.29571232419492E-15));
#130921=DIRECTION('',(0.215539797381042,0.484110311157681,0.848044693619241));
#130922=DIRECTION('center_axis',(-0.913545457642596,0.40673664307581,-1.51622084024078E-14));
#130923=DIRECTION('ref_axis',(0.355752797181947,0.799033864889936,0.48475233888685));
#130924=DIRECTION('',(0.406736643075798,0.913545457642602,6.43652923108483E-15));
#130925=DIRECTION('',(0.203370424080339,0.456777451208961,-0.866022419268941));
#130926=DIRECTION('center_axis',(0.913545072438839,-0.406737508253204,-1.64037044800086E-6));
#130927=DIRECTION('ref_axis',(0.352263396508499,0.79119654224795,-0.499918524376906));
#130928=DIRECTION('',(0.406736643075798,0.913545457642602,6.43652923108483E-15));
#130929=DIRECTION('center_axis',(0.913545842703945,-0.406735778209453,-1.63977757413235E-6));
#130930=DIRECTION('ref_axis',(0.352251495067333,0.791169811722332,0.499969212294195));
#130931=DIRECTION('',(0.203370360392769,0.456777308164283,0.866022509672761));
#130932=DIRECTION('',(0.406736643075798,0.913545457642602,6.43652923108483E-15));
#130933=DIRECTION('center_axis',(-9.73020895656139E-17,-6.84903784078409E-15,
1.));
#130934=DIRECTION('ref_axis',(0.,-1.,-6.84903784078409E-15));
#130935=DIRECTION('',(0.309016994374945,0.951056516295154,6.54389006809377E-15));
#130936=DIRECTION('center_axis',(9.73020895656139E-17,6.84903784078409E-15,
-1.));
#130937=DIRECTION('ref_axis',(-3.21147635721861E-34,-1.,-6.84903784078409E-15));
#130938=DIRECTION('',(-0.309016994374945,-0.951056516295154,-6.54389006809377E-15));
#130939=DIRECTION('center_axis',(-9.73020895656139E-17,-6.84903784078409E-15,
1.));
#130940=DIRECTION('ref_axis',(1.61937966168246E-34,-1.,-6.84903784078409E-15));
#130941=DIRECTION('center_axis',(0.951056516295154,-0.309016994374945,-2.02392930158885E-15));
#130942=DIRECTION('ref_axis',(9.73020895656142E-17,6.84903784078409E-15,
-1.));
#130943=DIRECTION('center_axis',(0.951056516295153,-0.30901699437495,1.32324727859198E-14));
#130944=DIRECTION('ref_axis',(0.270282164134238,0.831842966948057,0.484752338921605));
#130945=DIRECTION('',(-0.163755740941347,-0.503988348013117,-0.848044693619246));
#130946=DIRECTION('',(0.309016994374945,0.951056516295154,6.54389006809377E-15));
#130947=DIRECTION('',(-0.163755578933429,-0.50398784940401,0.848045021223106));
#130948=DIRECTION('center_axis',(0.951056516295158,-0.309016994374936,1.46108587059839E-14));
#130949=DIRECTION('ref_axis',(0.270281584637381,0.831841183440119,-0.484755722543684));
#130950=DIRECTION('',(-0.309016994374945,-0.951056516295154,-6.68470697498368E-15));
#130951=DIRECTION('',(-0.154510046201584,-0.47553302552284,-0.866022509672744));
#130952=DIRECTION('center_axis',(-0.951056223705258,0.309017894868251,-1.63998889432737E-6));
#130953=DIRECTION('ref_axis',(0.26763107032928,0.823683738649504,0.499918702269459));
#130954=DIRECTION('',(-0.309016994374945,-0.951056516295154,-6.68470697498368E-15));
#130955=DIRECTION('center_axis',(-0.951056808909242,0.309016093795583,-1.6401439545386E-6));
#130956=DIRECTION('ref_axis',(0.267622092735265,0.823656109178587,-0.499969028333544));
#130957=DIRECTION('',(-0.154510094588056,-0.475533174441008,0.866022419268952));
#130958=DIRECTION('',(-0.309016994374945,-0.951056516295154,-6.68470697498368E-15));
#130959=DIRECTION('center_axis',(0.951056516295154,-0.309016994374945,-2.02392930158885E-15));
#130960=DIRECTION('ref_axis',(9.73020895656142E-17,6.84903784078409E-15,
-1.));
#130961=DIRECTION('center_axis',(-0.951056516295147,0.309016994374967,3.33568660984485E-14));
#130962=DIRECTION('ref_axis',(0.270281584632204,0.83184118342417,-0.484755722573938));
#130963=DIRECTION('',(0.16375557893343,0.503987849404014,-0.848045021223103));
#130964=DIRECTION('',(-0.309016994374945,-0.951056516295154,-6.54389006809377E-15));
#130965=DIRECTION('',(0.16375574094134,0.503988348013127,0.848044693619241));
#130966=DIRECTION('center_axis',(-0.951056516295154,0.309016994374946,5.7892068445558E-15));
#130967=DIRECTION('ref_axis',(0.270282164140123,0.831842966966152,0.484752338887273));
#130968=DIRECTION('',(0.309016994374945,0.951056516295154,6.68470697498368E-15));
#130969=DIRECTION('',(0.154510094588052,0.47553317444103,-0.86602241926894));
#130970=DIRECTION('center_axis',(0.951056223637263,-0.309017895077515,-1.64037034454954E-6));
#130971=DIRECTION('ref_axis',(0.267631102061259,0.823683836309653,-0.499918524373411));
#130972=DIRECTION('',(0.309016994374945,0.951056516295154,6.68470697498368E-15));
#130973=DIRECTION('center_axis',(0.951056808843944,-0.30901609399655,-1.63977759461637E-6));
#130974=DIRECTION('ref_axis',(0.267622059916621,0.823656008172419,0.499969212299579));
#130975=DIRECTION('',(0.154510046201588,0.475533025522823,0.866022509672753));
#130976=DIRECTION('',(0.309016994374945,0.951056516295154,6.68470697498368E-15));
#130977=DIRECTION('center_axis',(-1.11539425682703E-16,-6.84522295806915E-15,
1.));
#130978=DIRECTION('ref_axis',(0.,-1.,-6.84522295806915E-15));
#130979=DIRECTION('',(0.207911690817756,0.978147600733806,6.71882876350984E-15));
#130980=DIRECTION('center_axis',(1.11539425682703E-16,6.84522295806915E-15,
-1.));
#130981=DIRECTION('ref_axis',(-2.39543546274231E-35,-1.,-6.84522295806915E-15));
#130982=DIRECTION('',(-0.207911690817756,-0.978147600733806,-6.71882876350984E-15));
#130983=DIRECTION('center_axis',(-1.11539425682703E-16,-6.84522295806915E-15,
1.));
#130984=DIRECTION('ref_axis',(-2.39876940632517E-34,-1.,-6.84522295806915E-15));
#130985=DIRECTION('center_axis',(0.978147600733806,-0.207911690817756,-1.31409985761792E-15));
#130986=DIRECTION('ref_axis',(1.11539425682703E-16,6.84522295806915E-15,
-1.));
#130987=DIRECTION('center_axis',(0.978147600733806,-0.207911690817757,1.03378693639992E-14));
#130988=DIRECTION('ref_axis',(0.181850263143883,0.855538223403326,0.484752338922033));
#130989=DIRECTION('',(-0.110177542335811,-0.518344583061382,-0.848044693619247));
#130990=DIRECTION('',(0.207911690817756,0.978147600733806,6.71882876350984E-15));
#130991=DIRECTION('',(-0.110177433334227,-0.518344070249277,0.848045021223104));
#130992=DIRECTION('center_axis',(0.978147600733807,-0.207911690817751,-2.06757434518653E-16));
#130993=DIRECTION('ref_axis',(0.181849873248985,0.85553638909205,-0.484755722543494));
#130994=DIRECTION('',(-0.207911690817756,-0.978147600733806,-6.85964567039975E-15));
#130995=DIRECTION('',(-0.103956887610937,-0.48907870354206,-0.866022509672737));
#130996=DIRECTION('center_axis',(-0.978147403873936,0.207912616962008,-1.6399888600733E-6));
#130997=DIRECTION('ref_axis',(0.180066563903243,0.847146577447699,0.49991870227341));
#130998=DIRECTION('',(-0.207911690817756,-0.978147600733806,-6.85964567039975E-15));
#130999=DIRECTION('center_axis',(-0.978147797608753,0.207910764585331,-1.64014399602197E-6));
#131000=DIRECTION('ref_axis',(0.180060523556148,0.847118160922542,-0.499969028332651));
#131001=DIRECTION('',(-0.103956920166139,-0.489078856702179,0.866022419268959));
#131002=DIRECTION('',(-0.207911690817756,-0.978147600733806,-6.85964567039975E-15));
#131003=DIRECTION('center_axis',(0.978147600733806,-0.207911690817756,-1.31409985761792E-15));
#131004=DIRECTION('ref_axis',(1.11539425682703E-16,6.84522295806915E-15,
-1.));
#131005=DIRECTION('center_axis',(-0.978147600733803,0.20791169081777,9.51084198674763E-15));
#131006=DIRECTION('ref_axis',(0.181849873245726,0.855536389076659,-0.484755722571879));
#131007=DIRECTION('',(0.110177433334223,0.518344070249286,-0.848045021223099));
#131008=DIRECTION('',(-0.207911690817756,-0.978147600733806,-6.71882876350983E-15));
#131009=DIRECTION('',(0.110177542335811,0.518344583061368,0.848044693619255));
#131010=DIRECTION('center_axis',(-0.978147600733808,0.20791169081775,3.79055210060189E-15));
#131011=DIRECTION('ref_axis',(0.18185026314782,0.855538223421847,0.484752338887868));
#131012=DIRECTION('',(0.207911690817756,0.978147600733806,6.85964567039975E-15));
#131013=DIRECTION('',(0.103956920166119,0.489078856702167,-0.866022419268968));
#131014=DIRECTION('center_axis',(0.978147403828172,-0.207912617177303,-1.64037042906602E-6));
#131015=DIRECTION('ref_axis',(0.180066585253188,0.847146677890037,-0.499918524376853));
#131016=DIRECTION('',(0.207911690817756,0.978147600733806,6.85964567039975E-15));
#131017=DIRECTION('center_axis',(0.978147797564806,-0.207910764792088,-1.63977754134118E-6));
#131018=DIRECTION('ref_axis',(0.18006050147535,0.847118057039365,0.499969212298413));
#131019=DIRECTION('',(0.103956887610919,0.489078703542023,0.86602250967276));
#131020=DIRECTION('',(0.207911690817756,0.978147600733806,6.85964567039975E-15));
#131021=DIRECTION('center_axis',(-1.26097532010604E-16,-6.84291718054622E-15,
1.));
#131022=DIRECTION('ref_axis',(0.,-1.,-6.84291718054622E-15));
#131023=DIRECTION('',(0.10452846326765,0.994521895368274,6.81861174548786E-15));
#131024=DIRECTION('center_axis',(1.26097532010604E-16,6.84291718054622E-15,
-1.));
#131025=DIRECTION('ref_axis',(-3.1783372781003E-34,-1.,-6.84291718054621E-15));
#131026=DIRECTION('',(-0.10452846326765,-0.994521895368274,-6.81861174548786E-15));
#131027=DIRECTION('center_axis',(-1.26097532010604E-16,-6.84291718054622E-15,
1.));
#131028=DIRECTION('ref_axis',(3.64495957293817E-34,-1.,-6.84291718054622E-15));
#131029=DIRECTION('center_axis',(0.994521895368274,-0.10452846326765,-5.89872860613851E-16));
#131030=DIRECTION('ref_axis',(1.26097532010604E-16,6.84291718054622E-15,
-1.));
#131031=DIRECTION('center_axis',(0.994521895368275,-0.10452846326764,-2.22608786971444E-14));
#131032=DIRECTION('ref_axis',(0.0914259726159116,0.869860024049565,0.484752338923418));
#131033=DIRECTION('',(-0.0553922155203051,-0.527021726387053,-0.848044693619247));
#131034=DIRECTION('',(0.10452846326765,0.994521895368274,6.81861174548786E-15));
#131035=DIRECTION('',(-0.0553921607193105,-0.527021204990399,0.848045021223115));
#131036=DIRECTION('center_axis',(0.994521895368273,-0.104528463267657,-1.44041012714673E-14));
#131037=DIRECTION('ref_axis',(0.0914257765946934,0.86985815903228,-0.48475572254387));
#131038=DIRECTION('',(-0.10452846326765,-0.994521895368274,-6.95942865237777E-15));
#131039=DIRECTION('',(-0.0522647556052144,-0.497265932938934,-0.866022509672756));
#131040=DIRECTION('center_axis',(-0.994521796395255,0.104529404915866,-1.63998886226799E-6));
#131041=DIRECTION('ref_axis',(0.090529210522719,0.861327901071179,0.499918702269129));
#131042=DIRECTION('',(-0.10452846326765,-0.994521895368274,-6.95942865237777E-15));
#131043=DIRECTION('center_axis',(-0.994521994347068,0.104527521530168,-1.64014403750577E-6));
#131044=DIRECTION('ref_axis',(0.0905261736004185,0.861299008821256,-0.499969028337546));
#131045=DIRECTION('',(-0.0522647719724818,-0.49726608866303,0.866022419268945));
#131046=DIRECTION('',(-0.10452846326765,-0.994521895368274,-6.95942865237777E-15));
#131047=DIRECTION('center_axis',(0.994521895368274,-0.10452846326765,-5.89872860613851E-16));
#131048=DIRECTION('ref_axis',(1.26097532010604E-16,6.84291718054622E-15,
-1.));
#131049=DIRECTION('center_axis',(-0.994521895368273,0.104528463267658,6.61623790382405E-15));
#131050=DIRECTION('ref_axis',(0.0914257765928784,0.869858159014973,-0.484755722575269));
#131051=DIRECTION('',(0.0553921607193085,0.527021204990422,-0.848045021223101));
#131052=DIRECTION('',(-0.10452846326765,-0.994521895368274,-6.81861174548786E-15));
#131053=DIRECTION('',(0.0553922155203075,0.527021726387058,0.848044693619244));
#131054=DIRECTION('center_axis',(-0.994521895368274,0.104528463267647,9.13178460599565E-15));
#131055=DIRECTION('ref_axis',(0.0914259726180026,0.86986002406946,0.484752338887324));
#131056=DIRECTION('',(0.10452846326765,0.994521895368274,6.95942865237777E-15));
#131057=DIRECTION('',(0.0522647719724739,0.497266088663004,-0.86602241926896));
#131058=DIRECTION('center_axis',(0.994521796372252,-0.104529405134716,-1.6403703829347E-6));
#131059=DIRECTION('ref_axis',(0.0905292212565932,0.861328003194837,-0.499918524372793));
#131060=DIRECTION('',(0.10452846326765,0.994521895368274,6.95942865237777E-15));
#131061=DIRECTION('center_axis',(0.994521994324978,-0.104527521740355,-1.63977761557319E-6));
#131062=DIRECTION('ref_axis',(0.0905261624997722,0.861298903203399,0.499969212295804));
#131063=DIRECTION('',(0.0522647556052142,0.497265932938926,0.866022509672761));
#131064=DIRECTION('',(0.10452846326765,0.994521895368274,6.95942865237777E-15));
#131065=DIRECTION('center_axis',(-1.40816906889911E-16,-6.84214577079636E-15,
1.));
#131066=DIRECTION('ref_axis',(-1.,9.8331920519947E-31,-1.40816906889911E-16));
#131067=DIRECTION('',(-3.49148133884313E-15,1.,6.84214577079636E-15));
#131068=DIRECTION('center_axis',(1.40816906889911E-16,6.84214577079636E-15,
-1.));
#131069=DIRECTION('ref_axis',(-1.,1.19595411430356E-30,-1.40816906889911E-16));
#131070=DIRECTION('',(3.49148133884313E-15,-1.,-6.84214577079636E-15));
#131071=DIRECTION('center_axis',(-1.40816906889911E-16,-6.84214577079636E-15,
1.));
#131072=DIRECTION('ref_axis',(-1.,8.43631878914075E-31,-1.40816906889911E-16));
#131073=DIRECTION('center_axis',(1.,3.49148133884313E-15,1.40816906889935E-16));
#131074=DIRECTION('ref_axis',(1.40816906889911E-16,6.84214577079636E-15,
-1.));
#131075=DIRECTION('center_axis',(1.,3.44043747061122E-15,3.3107378020012E-16));
#131076=DIRECTION('ref_axis',(-3.16967243309519E-15,0.87465145624433,0.484752338921301));
#131077=DIRECTION('',(1.96084725663078E-15,-0.52992470939204,-0.848044693619247));
#131078=DIRECTION('',(-3.49148133884313E-15,1.,6.84214577079636E-15));
#131079=DIRECTION('',(1.75444295999835E-15,-0.529924185123399,0.848045021223108));
#131080=DIRECTION('center_axis',(1.,3.58452992681197E-15,2.19445148712543E-16));
#131081=DIRECTION('ref_axis',(-3.02883030677592E-15,0.874649580952794,-0.484755722543945));
#131082=DIRECTION('',(3.49148133884313E-15,-1.,-6.98296267768627E-15));
#131083=DIRECTION('',(1.92690513386524E-15,-0.500005012715014,-0.866022509672733));
#131084=DIRECTION('center_axis',(-0.999999999998207,9.46835254807534E-7,
-1.639988859514E-6));
#131085=DIRECTION('ref_axis',(1.66718524320421E-10,0.866072335964842,0.49991870226708));
#131086=DIRECTION('',(3.49148133884313E-15,-1.,-6.98296267768627E-15));
#131087=DIRECTION('center_axis',(-0.999999999998207,-9.46924665087402E-7,
-1.64014406431857E-6));
#131088=DIRECTION('ref_axis',(-5.65130087085307E-11,0.866043284546834,-0.499969028332087));
#131089=DIRECTION('',(1.51399673284832E-15,-0.50000516929684,0.866022419268946));
#131090=DIRECTION('',(3.49148133884313E-15,-1.,-6.98296267768627E-15));
#131091=DIRECTION('center_axis',(1.,3.49148133884313E-15,1.40816906889935E-16));
#131092=DIRECTION('ref_axis',(1.40816906889911E-16,6.84214577079636E-15,
-1.));
#131093=DIRECTION('center_axis',(-1.,-3.31723128487435E-15,2.6278067191977E-16));
#131094=DIRECTION('ref_axis',(-3.02879938767599E-15,0.874649580935239,-0.48475572257562));
#131095=DIRECTION('',(-1.702841696469E-15,0.529924185123403,-0.848045021223106));
#131096=DIRECTION('',(3.49148133884313E-15,-1.,-6.84214577079636E-15));
#131097=DIRECTION('',(-1.90924601303524E-15,0.52992470939203,0.848044693619253));
#131098=DIRECTION('center_axis',(-1.,-3.24518402866521E-15,-5.38039174125174E-16));
#131099=DIRECTION('ref_axis',(-3.09922068458486E-15,0.874651456263469,0.48475233888677));
#131100=DIRECTION('',(-3.49148133884313E-15,1.,6.98296267768627E-15));
#131101=DIRECTION('',(-1.6516327994709E-15,0.50000516929684,-0.866022419268946));
#131102=DIRECTION('center_axis',(0.999999999998206,-9.47055338026444E-7,
-1.64037041142286E-6));
#131103=DIRECTION('ref_axis',(1.6697062825775E-10,0.866072438647394,-0.499918524377079));
#131104=DIRECTION('',(-3.49148133884313E-15,1.,6.98296267768627E-15));
#131105=DIRECTION('center_axis',(0.999999999998207,9.46713294510181E-7,
-1.63977760303538E-6));
#131106=DIRECTION('ref_axis',(-5.62740263084214E-11,0.866043178343555,0.499969212296711));
#131107=DIRECTION('',(-1.92690513386528E-15,0.500005012714987,0.866022509672748));
#131108=DIRECTION('',(-3.49148133884313E-15,1.,6.98296267768627E-15));
#131109=DIRECTION('center_axis',(-1.55536281769218E-16,-6.84291718054622E-15,
1.));
#131110=DIRECTION('ref_axis',(-1.,1.08610405062054E-30,-1.55536281769218E-16));
#131111=DIRECTION('',(-0.104528463267657,0.994521895368273,6.78917299572924E-15));
#131112=DIRECTION('center_axis',(1.55536281769218E-16,6.84291718054622E-15,
-1.));
#131113=DIRECTION('ref_axis',(-1.,1.15501815782576E-30,-1.55536281769218E-16));
#131114=DIRECTION('',(0.104528463267657,-0.994521895368273,-6.78917299572924E-15));
#131115=DIRECTION('center_axis',(-1.55536281769218E-16,-6.84291718054622E-15,
1.));
#131116=DIRECTION('ref_axis',(-1.,1.26143365054205E-30,-1.55536281769218E-16));
#131117=DIRECTION('center_axis',(0.994521895368273,0.104528463267657,8.69963854894001E-16));
#131118=DIRECTION('ref_axis',(1.55536281769218E-16,6.84291718054622E-15,
-1.));
#131119=DIRECTION('center_axis',(0.994521895368273,0.10452846326766,-6.61623639296017E-15));
#131120=DIRECTION('ref_axis',(0.0914259726160256,-0.869860024050614,-0.484752338921515));
#131121=DIRECTION('',(0.0553922155203091,-0.527021726387057,-0.848044693619244));
#131122=DIRECTION('',(-0.104528463267657,0.994521895368273,6.78917299572924E-15));
#131123=DIRECTION('',(0.0553921607193154,-0.527021204990399,0.848045021223115));
#131124=DIRECTION('center_axis',(0.994521895368271,0.104528463267677,4.04899975932421E-14));
#131125=DIRECTION('ref_axis',(0.0914257765946187,-0.869858159031526,0.484755722545237));
#131126=DIRECTION('',(0.104528463267657,-0.994521895368273,-6.92998990261915E-15));
#131127=DIRECTION('',(0.0522647556052223,-0.497265932938961,-0.86602250967274));
#131128=DIRECTION('center_axis',(-0.994521994337723,-0.104527521619084,
-1.63998884823934E-6));
#131129=DIRECTION('ref_axis',(0.0905292101911854,-0.861327901106789,-0.499918702267812));
#131130=DIRECTION('',(0.104528463267657,-0.994521895368273,-6.92998990261915E-15));
#131131=DIRECTION('center_axis',(-0.994521796385912,-0.104529405004756,
-1.64014403298725E-6));
#131132=DIRECTION('ref_axis',(0.0905261737132939,-0.861299008813934,0.499969028329721));
#131133=DIRECTION('',(0.0522647719724805,-0.497266088663018,0.866022419268952));
#131134=DIRECTION('',(0.104528463267657,-0.994521895368273,-6.92998990261915E-15));
#131135=DIRECTION('center_axis',(0.994521895368273,0.104528463267657,8.69963854894001E-16));
#131136=DIRECTION('ref_axis',(1.55536281769218E-16,6.84291718054622E-15,
-1.));
#131137=DIRECTION('center_axis',(-0.994521895368273,-0.104528463267655,
3.58379553123804E-15));
#131138=DIRECTION('ref_axis',(0.0914257765929169,-0.869858159015314,0.484755722574649));
#131139=DIRECTION('',(-0.0553921607193138,0.527021204990413,-0.848045021223107));
#131140=DIRECTION('',(0.104528463267657,-0.994521895368273,-6.78917299572924E-15));
#131141=DIRECTION('',(-0.0553922155203088,0.527021726387043,0.848044693619253));
#131142=DIRECTION('center_axis',(-0.994521895368272,-0.104528463267666,
1.06480054462366E-14));
#131143=DIRECTION('ref_axis',(0.091425972617933,-0.869860024068733,-0.484752338888641));
#131144=DIRECTION('',(-0.104528463267657,0.994521895368273,6.92998990261915E-15));
#131145=DIRECTION('',(-0.0522647719724874,0.497266088663041,-0.866022419268938));
#131146=DIRECTION('center_axis',(0.994521994360729,0.104527521400187,-1.64037042071753E-6));
#131147=DIRECTION('ref_axis',(0.0905292209241164,-0.861328003226279,0.499918524378826));
#131148=DIRECTION('',(-0.104528463267657,0.994521895368273,6.92998990261915E-15));
#131149=DIRECTION('center_axis',(0.994521796408008,0.10452940479454,-1.63977756432044E-6));
#131150=DIRECTION('ref_axis',(0.0905261626117495,-0.861298903192075,-0.499969212295037));
#131151=DIRECTION('',(-0.0522647556052286,0.497265932938937,0.866022509672754));
#131152=DIRECTION('',(-0.104528463267657,0.994521895368273,6.92998990261915E-15));
#131153=DIRECTION('center_axis',(-1.70094388097119E-16,-6.84522295806915E-15,
1.));
#131154=DIRECTION('ref_axis',(-1.,1.18776276376607E-30,-1.70094388097119E-16));
#131155=DIRECTION('',(-0.207911690817763,0.978147600733805,6.66027380109541E-15));
#131156=DIRECTION('center_axis',(1.70094388097119E-16,6.84522295806915E-15,
-1.));
#131157=DIRECTION('ref_axis',(-1.,1.16019143467152E-30,-1.70094388097119E-16));
#131158=DIRECTION('',(0.207911690817763,-0.978147600733805,-6.66027380109541E-15));
#131159=DIRECTION('center_axis',(-1.70094388097119E-16,-6.84522295806915E-15,
1.));
#131160=DIRECTION('ref_axis',(-1.,1.26050675734334E-30,-1.70094388097119E-16));
#131161=DIRECTION('center_axis',(0.978147600733805,0.207911690817763,1.58957929685221E-15));
#131162=DIRECTION('ref_axis',(1.70094388097119E-16,6.84522295806915E-15,
-1.));
#131163=DIRECTION('center_axis',(0.978147600733804,0.207911690817767,-2.12270917607467E-14));
#131164=DIRECTION('ref_axis',(0.181850263143777,-0.855538223402809,-0.484752338922984));
#131165=DIRECTION('',(0.110177542335814,-0.518344583061392,-0.848044693619241));
#131166=DIRECTION('',(-0.207911690817763,0.978147600733805,6.66027380109541E-15));
#131167=DIRECTION('',(0.110177433334229,-0.518344070249262,0.848045021223113));
#131168=DIRECTION('center_axis',(0.978147600733799,0.207911690817789,5.18271969193474E-14));
#131169=DIRECTION('ref_axis',(0.181849873249002,-0.855536389092088,0.484755722543421));
#131170=DIRECTION('',(0.207911690817763,-0.978147600733805,-6.80109070798532E-15));
#131171=DIRECTION('',(0.103956887610948,-0.489078703542072,-0.866022509672728));
#131172=DIRECTION('center_axis',(-0.97814779759017,-0.207910764672759,-1.63998884285995E-6));
#131173=DIRECTION('ref_axis',(0.180066563577228,-0.847146577517634,-0.499918702272328));
#131174=DIRECTION('',(0.207911690817763,-0.978147600733805,-6.80109070798532E-15));
#131175=DIRECTION('center_axis',(-0.97814740385534,-0.207912617049492,-1.6401440806252E-6));
#131176=DIRECTION('ref_axis',(0.180060523666301,-0.847118160897096,0.499969028336096));
#131177=DIRECTION('',(0.103956920166122,-0.48907885670218,0.866022419268961));
#131178=DIRECTION('',(0.207911690817763,-0.978147600733805,-6.80109070798532E-15));
#131179=DIRECTION('center_axis',(0.978147600733805,0.207911690817763,1.58957929685221E-15));
#131180=DIRECTION('ref_axis',(1.70094388097119E-16,6.84522295806915E-15,
-1.));
#131181=DIRECTION('center_axis',(-0.978147600733801,-0.207911690817782,
-2.26054795047341E-14));
#131182=DIRECTION('ref_axis',(0.181849873245555,-0.855536389075835,0.484755722573397));
#131183=DIRECTION('',(-0.110177433334229,0.518344070249272,-0.848045021223107));
#131184=DIRECTION('',(0.207911690817763,-0.978147600733805,-6.66027380109541E-15));
#131185=DIRECTION('',(-0.110177542335816,0.518344583061377,0.84804469361925));
#131186=DIRECTION('center_axis',(-0.978147600733805,-0.207911690817762,
9.0284059123426E-15));
#131187=DIRECTION('ref_axis',(0.181850263147824,-0.855538223421843,-0.484752338887874));
#131188=DIRECTION('',(-0.207911690817763,0.978147600733805,6.80109070798532E-15));
#131189=DIRECTION('',(-0.10395692016612,0.489078856702206,-0.866022419268946));
#131190=DIRECTION('center_axis',(0.978147797635921,0.20791076445751,-1.64037035642678E-6));
#131191=DIRECTION('ref_axis',(0.180066584926945,-0.847146677961353,0.499918524373514));
#131192=DIRECTION('',(-0.207911690817763,0.978147600733805,6.80109070798532E-15));
#131193=DIRECTION('center_axis',(0.978147403899296,0.207912616842697,-1.63977756113648E-6));
#131194=DIRECTION('ref_axis',(0.180060501585272,-0.847118057015218,-0.49996921229974));
#131195=DIRECTION('',(-0.103956887610925,0.489078703542011,0.866022509672765));
#131196=DIRECTION('',(-0.207911690817763,0.978147600733805,6.80109070798532E-15));
#131197=DIRECTION('center_axis',(-1.84331724214208E-16,-6.84903784078409E-15,
1.));
#131198=DIRECTION('ref_axis',(-1.,1.28718155050137E-30,-1.84331724214208E-16));
#131199=DIRECTION('',(-0.309016994374951,0.951056516295152,6.45686043344516E-15));
#131200=DIRECTION('center_axis',(1.84331724214208E-16,6.84903784078409E-15,
-1.));
#131201=DIRECTION('ref_axis',(-1.,1.16316872187192E-30,-1.84331724214208E-16));
#131202=DIRECTION('',(0.309016994374951,-0.951056516295152,-6.45686043344516E-15));
#131203=DIRECTION('center_axis',(-1.84331724214208E-16,-6.84903784078409E-15,
1.));
#131204=DIRECTION('ref_axis',(-1.,1.25738374682677E-30,-1.84331724214208E-16));
#131205=DIRECTION('center_axis',(0.951056516295152,0.309016994374951,2.29177897539325E-15));
#131206=DIRECTION('ref_axis',(1.84331724214208E-16,6.84903784078409E-15,
-1.));
#131207=DIRECTION('center_axis',(0.951056516295154,0.309016994374946,2.1778444793492E-14));
#131208=DIRECTION('ref_axis',(0.270282164134052,-0.831842966947439,-0.484752338922769));
#131209=DIRECTION('',(0.163755740941359,-0.503988348013111,-0.848044693619247));
#131210=DIRECTION('',(-0.309016994374951,0.951056516295152,6.45686043344516E-15));
#131211=DIRECTION('',(0.163755578933428,-0.50398784940402,0.848045021223101));
#131212=DIRECTION('center_axis',(0.951056516295148,0.309016994374966,3.11514534674777E-14));
#131213=DIRECTION('ref_axis',(0.270281584637533,-0.831841183440571,0.484755722542823));
#131214=DIRECTION('',(0.309016994374951,-0.951056516295152,-6.59767734033507E-15));
#131215=DIRECTION('',(0.154510046201604,-0.475533025522845,-0.866022509672738));
#131216=DIRECTION('center_axis',(-0.951056808881636,-0.309016093880544,
-1.63998884845428E-6));
#131217=DIRECTION('ref_axis',(0.267631070012316,-0.823683738753064,-0.499918702268516));
#131218=DIRECTION('',(0.309016994374951,-0.951056516295152,-6.59767734033507E-15));
#131219=DIRECTION('center_axis',(-0.951056223677648,-0.309017894953224,
-1.64014399102986E-6));
#131220=DIRECTION('ref_axis',(0.267622092843757,-0.823656109146745,0.499969028327929));
#131221=DIRECTION('',(0.154510094588035,-0.475533174441031,0.866022419268943));
#131222=DIRECTION('',(0.309016994374951,-0.951056516295152,-6.59767734033507E-15));
#131223=DIRECTION('center_axis',(0.951056516295152,0.309016994374951,2.29177897539325E-15));
#131224=DIRECTION('ref_axis',(1.84331724214208E-16,6.84903784078409E-15,
-1.));
#131225=DIRECTION('center_axis',(-0.95105651629515,-0.309016994374958,-7.85678251079127E-15));
#131226=DIRECTION('ref_axis',(0.270281584632399,-0.831841183424754,0.484755722572828));
#131227=DIRECTION('',(-0.163755578933429,0.50398784940401,-0.848045021223106));
#131228=DIRECTION('',(0.309016994374951,-0.951056516295152,-6.45686043344516E-15));
#131229=DIRECTION('',(-0.16375574094135,0.503988348013116,0.848044693619245));
#131230=DIRECTION('center_axis',(-0.951056516295163,-0.30901699437492,-6.57488491631666E-14));
#131231=DIRECTION('ref_axis',(0.270282164140199,-0.831842966966367,-0.484752338886862));
#131232=DIRECTION('',(-0.309016994374951,0.951056516295152,6.59767734033507E-15));
#131233=DIRECTION('',(-0.15451009458806,0.475533174441019,-0.866022419268945));
#131234=DIRECTION('center_axis',(0.951056808949647,0.309016093671226,-1.64037043810308E-6));
#131235=DIRECTION('ref_axis',(0.267631101743103,-0.823683836411159,0.499918524376491));
#131236=DIRECTION('',(-0.309016994374951,0.951056516295152,6.59767734033507E-15));
#131237=DIRECTION('center_axis',(0.951056223742945,0.309017894752262,-1.6397776367882E-6));
#131238=DIRECTION('ref_axis',(0.267622060023681,-0.823656008137699,-0.499969212299469));
#131239=DIRECTION('',(-0.154510046201599,0.475533025522804,0.866022509672762));
#131240=DIRECTION('',(-0.309016994374951,0.951056516295152,6.59767734033507E-15));
#131241=DIRECTION('center_axis',(-1.98092302886631E-16,-6.85432003203771E-15,
1.));
#131242=DIRECTION('ref_axis',(-1.,1.38327115779427E-30,-1.98092302886631E-16));
#131243=DIRECTION('',(-0.406736643075804,0.913545457642599,6.18116153220146E-15));
#131244=DIRECTION('center_axis',(1.98092302886631E-16,6.85432003203771E-15,
-1.));
#131245=DIRECTION('ref_axis',(-1.,1.55513534684527E-30,-1.98092302886631E-16));
#131246=DIRECTION('',(0.406736643075804,-0.913545457642599,-6.18116153220146E-15));
#131247=DIRECTION('center_axis',(-1.98092302886631E-16,-6.85432003203771E-15,
1.));
#131248=DIRECTION('ref_axis',(-1.,1.25098969931104E-30,-1.98092302886631E-16));
#131249=DIRECTION('center_axis',(0.913545457642599,0.406736643075804,2.9688694438943E-15));
#131250=DIRECTION('ref_axis',(1.98092302886631E-16,6.85432003203771E-15,
-1.));
#131251=DIRECTION('center_axis',(0.913545457642599,0.406736643075804,-8.27029549119878E-16));
#131252=DIRECTION('ref_axis',(0.355752797173898,-0.799033864871854,-0.484752338922563));
#131253=DIRECTION('',(0.21553979738105,-0.484110311157671,-0.848044693619245));
#131254=DIRECTION('',(-0.406736643075804,0.913545457642599,6.18116153220146E-15));
#131255=DIRECTION('',(0.215539584141765,-0.484109832214438,0.848045021223109));
#131256=DIRECTION('center_axis',(0.913545457642593,0.406736643075818,2.34325092454483E-14));
#131257=DIRECTION('ref_axis',(0.355752034424608,-0.799032151708895,0.484755722543021));
#131258=DIRECTION('',(0.406736643075804,-0.913545457642599,-6.32197843909137E-15));
#131259=DIRECTION('',(0.20337036039278,-0.456777308164312,-0.866022509672743));
#131260=DIRECTION('center_axis',(-0.913545842753553,-0.406735778098031,
-1.6399888567167E-6));
#131261=DIRECTION('ref_axis',(0.352263354438044,-0.791196448576584,-0.499918702270538));
#131262=DIRECTION('',(0.406736643075804,-0.913545457642599,-6.32197843909137E-15));
#131263=DIRECTION('center_axis',(-0.91354507249199,-0.406737508133826,-1.6401440824322E-6));
#131264=DIRECTION('ref_axis',(0.352251538367414,-0.791169908698556,0.499969028328464));
#131265=DIRECTION('',(0.203370424080347,-0.456777451208943,0.866022419268948));
#131266=DIRECTION('',(0.406736643075804,-0.913545457642599,-6.32197843909137E-15));
#131267=DIRECTION('center_axis',(0.913545457642599,0.406736643075804,2.9688694438943E-15));
#131268=DIRECTION('ref_axis',(1.98092302886631E-16,6.85432003203771E-15,
-1.));
#131269=DIRECTION('center_axis',(-0.913545457642582,-0.406736643075842,
-7.44326764180192E-14));
#131270=DIRECTION('ref_axis',(0.355752034418312,-0.799032151694757,0.484755722570946));
#131271=DIRECTION('',(-0.21553958414177,0.484109832214447,-0.848045021223103));
#131272=DIRECTION('',(0.406736643075804,-0.913545457642599,-6.18116153220146E-15));
#131273=DIRECTION('',(-0.215539797381043,0.484110311157669,0.848044693619248));
#131274=DIRECTION('center_axis',(-0.913545457642587,-0.406736643075831,
3.94217418462606E-14));
#131275=DIRECTION('ref_axis',(0.355752797181838,-0.799033864889671,-0.484752338887366));
#131276=DIRECTION('',(-0.406736643075804,0.913545457642599,6.32197843909137E-15));
#131277=DIRECTION('',(-0.203370424080351,0.456777451208949,-0.866022419268944));
#131278=DIRECTION('center_axis',(0.913545842843072,0.406735777896966,-1.64037044955031E-6));
#131279=DIRECTION('ref_axis',(0.352263396204226,-0.791196542385554,0.499918524373531));
#131280=DIRECTION('',(-0.406736643075804,0.913545457642599,6.32197843909137E-15));
#131281=DIRECTION('center_axis',(0.913545072577991,0.406737507940666,-1.63977755898457E-6));
#131282=DIRECTION('ref_axis',(0.352251495169288,-0.791169811674637,-0.499969212297838));
#131283=DIRECTION('',(-0.203370360392795,0.456777308164266,0.866022509672764));
#131284=DIRECTION('',(-0.406736643075804,0.913545457642599,6.32197843909137E-15));
#131285=DIRECTION('center_axis',(-2.11225360334866E-16,-6.86101165903726E-15,
1.));
#131286=DIRECTION('ref_axis',(-1.,1.4749788077992E-30,-2.11225360334866E-16));
#131287=DIRECTION('',(-0.500000000000004,0.866025403784436,5.83619771222003E-15));
#131288=DIRECTION('center_axis',(2.11225360334866E-16,6.86101165903726E-15,
-1.));
#131289=DIRECTION('ref_axis',(-1.,1.55053706533811E-30,-2.11225360334866E-16));
#131290=DIRECTION('',(0.500000000000004,-0.866025403784436,-5.83619771222003E-15));
#131291=DIRECTION('center_axis',(-2.11225360334866E-16,-6.86101165903726E-15,
1.));
#131292=DIRECTION('ref_axis',(-1.,1.6579053986113E-30,-2.11225360334866E-16));
#131293=DIRECTION('center_axis',(0.866025403784436,0.500000000000004,3.61343235749217E-15));
#131294=DIRECTION('ref_axis',(2.11225360334867E-16,6.86101165903726E-15,
-1.));
#131295=DIRECTION('center_axis',(0.866025403784404,0.500000000000061,-7.33299533553082E-14));
#131296=DIRECTION('ref_axis',(0.437325728121665,-0.757470380563725,-0.484752338923188));
#131297=DIRECTION('',(0.264962354696018,-0.458928260426587,-0.84804469361925));
#131298=DIRECTION('',(-0.500000000000004,0.866025403784436,5.83619771222003E-15));
#131299=DIRECTION('',(0.264962092561705,-0.458927806396622,0.848045021223111));
#131300=DIRECTION('center_axis',(0.866025403784435,0.500000000000007,2.46730538525601E-14));
#131301=DIRECTION('ref_axis',(0.437324790476593,-0.757468756514882,0.484755722543223));
#131302=DIRECTION('',(0.500000000000004,-0.866025403784436,-5.97701461910994E-15));
#131303=DIRECTION('',(0.250002506357502,-0.433017043030757,-0.866022509672737));
#131304=DIRECTION('center_axis',(-0.866025877200505,-0.499999180015734,
-1.63998885809397E-6));
#131305=DIRECTION('ref_axis',(0.433036167836597,-0.750040644541319,-0.499918702272117));
#131306=DIRECTION('',(0.500000000000004,-0.866025403784436,-5.97701461910994E-15));
#131307=DIRECTION('center_axis',(-0.866024930320587,-0.50000082005986,-1.64014391649668E-6));
#131308=DIRECTION('ref_axis',(0.433021642321137,-0.750015485164071,0.499969028336364));
#131309=DIRECTION('',(0.250002584648427,-0.433017178634617,0.866022419268937));
#131310=DIRECTION('',(0.500000000000004,-0.866025403784436,-5.97701461910994E-15));
#131311=DIRECTION('center_axis',(0.866025403784436,0.500000000000004,3.61343235749217E-15));
#131312=DIRECTION('ref_axis',(2.11225360334867E-16,6.86101165903726E-15,
-1.));
#131313=DIRECTION('center_axis',(-0.866025403784421,-0.50000000000003,-5.320557980992E-14));
#131314=DIRECTION('ref_axis',(0.437324790468157,-0.757468756500253,0.484755722573692));
#131315=DIRECTION('',(-0.264962092561701,0.458927806396626,-0.84804502122311));
#131316=DIRECTION('',(0.500000000000004,-0.866025403784436,-5.83619771222003E-15));
#131317=DIRECTION('',(-0.264962354696035,0.45892826042661,0.848044693619233));
#131318=DIRECTION('center_axis',(-0.866025403784439,-0.5,-2.48108864766685E-14));
#131319=DIRECTION('ref_axis',(0.437325728131541,-0.75747038058086,-0.484752338887502));
#131320=DIRECTION('',(-0.500000000000004,0.866025403784436,5.97701461910994E-15));
#131321=DIRECTION('',(-0.250002584648417,0.433017178634595,-0.866022419268951));
#131322=DIRECTION('center_axis',(0.86602587731055,0.499999179825129,-1.64037040961549E-6));
#131323=DIRECTION('ref_axis',(0.433036219180504,-0.750040733472094,0.49991852437222));
#131324=DIRECTION('',(-0.500000000000004,0.866025403784436,5.97701461910994E-15));
#131325=DIRECTION('center_axis',(0.866024930426257,0.500000819876835,-1.6397775689687E-6));
#131326=DIRECTION('ref_axis',(0.433021589219912,-0.750015393190588,-0.499969212298748));
#131327=DIRECTION('',(-0.250002506357468,0.433017043030729,0.866022509672762));
#131328=DIRECTION('',(-0.500000000000004,0.866025403784436,5.97701461910994E-15));
#131329=DIRECTION('center_axis',(-2.23587008033243E-16,-6.86903940691702E-15,
1.));
#131330=DIRECTION('ref_axis',(-1.,1.56129973231167E-30,-2.23587008033243E-16));
#131331=DIRECTION('',(-0.587785252292477,0.809016994374945,5.42574846930092E-15));
#131332=DIRECTION('center_axis',(2.23587008033243E-16,6.86903940691702E-15,
-1.));
#131333=DIRECTION('ref_axis',(-1.,2.1582735598713E-13,-2.2358700803176E-16));
#131334=DIRECTION('',(0.587785252292477,-0.809016994374945,-5.42574846930092E-15));
#131335=DIRECTION('center_axis',(-2.23587008033243E-16,-6.86903940691702E-15,
1.));
#131336=DIRECTION('ref_axis',(-1.,1.69233669110578E-30,-2.23587008033243E-16));
#131337=DIRECTION('center_axis',(0.809016994374945,0.587785252292477,4.21840575002203E-15));
#131338=DIRECTION('ref_axis',(2.23587008033243E-16,6.86903940691702E-15,
-1.));
#131339=DIRECTION('center_axis',(0.809016994374947,0.587785252292474,1.54378849169051E-14));
#131340=DIRECTION('ref_axis',(0.514107226876102,-0.707607892255824,-0.484752338922705));
#131341=DIRECTION('',(0.311481929006018,-0.428718095637362,-0.848044693619248));
#131342=DIRECTION('',(-0.587785252292477,0.809016994374945,5.42574846930092E-15));
#131343=DIRECTION('',(0.311481620848644,-0.428717671495135,0.848045021223102));
#131344=DIRECTION('center_axis',(0.809016994374931,0.587785252292496,3.47352489991332E-14));
#131345=DIRECTION('ref_axis',(0.514106124607984,-0.707606375113916,0.484755722543533));
#131346=DIRECTION('',(0.587785252292477,-0.809016994374945,-5.56656537619083E-15));
#131347=DIRECTION('',(0.29389557254618,-0.404512552559093,-0.866022509672745));
#131348=DIRECTION('center_axis',(-0.809017550909332,-0.587784486285558,
-1.63998894398804E-6));
#131349=DIRECTION('ref_axis',(0.509064546361577,-0.70066723824859,-0.499918702273455));
#131350=DIRECTION('',(0.587785252292477,-0.809016994374945,-5.56656537619083E-15));
#131351=DIRECTION('center_axis',(-0.80901643778517,-0.587786018369528,-1.64014399843157E-6));
#131352=DIRECTION('ref_axis',(0.509047470549497,-0.700643735029776,0.49996902833144));
#131353=DIRECTION('',(0.293895664582661,-0.404512679236465,0.866022419268955));
#131354=DIRECTION('',(0.587785252292477,-0.809016994374945,-5.56656537619083E-15));
#131355=DIRECTION('center_axis',(0.809016994374945,0.587785252292477,4.21840575002203E-15));
#131356=DIRECTION('ref_axis',(2.23587008033243E-16,6.86903940691702E-15,
-1.));
#131357=DIRECTION('center_axis',(-0.809016994374898,-0.587785252292541,
-1.25984196751993E-13));
#131358=DIRECTION('ref_axis',(0.514106124597603,-0.70760637509962,0.484755722575412));
#131359=DIRECTION('',(-0.311481620848633,0.428717671495124,-0.848045021223112));
#131360=DIRECTION('',(0.587785252292477,-0.809016994374945,-5.42574846930092E-15));
#131361=DIRECTION('',(-0.311481929006027,0.428718095637352,0.84804469361925));
#131362=DIRECTION('center_axis',(-0.80901699437497,-0.587785252292442,-5.73407154127436E-14));
#131363=DIRECTION('ref_axis',(0.514107226887343,-0.707607892271321,-0.484752338888164));
#131364=DIRECTION('',(-0.587785252292477,0.809016994374945,5.56656537619083E-15));
#131365=DIRECTION('',(-0.293895664582678,0.404512679236454,-0.866022419268954));
#131366=DIRECTION('center_axis',(0.809017551038645,0.587784486107572,-1.64037042941065E-6));
#131367=DIRECTION('ref_axis',(0.509064606719126,-0.700667321323996,0.49991852437628));
#131368=DIRECTION('',(-0.587785252292477,0.809016994374945,5.56656537619083E-15));
#131369=DIRECTION('center_axis',(0.80901643790939,0.587786018198556,-1.63977758015677E-6));
#131370=DIRECTION('ref_axis',(0.509047408125087,-0.700643649110335,-0.499969212294602));
#131371=DIRECTION('',(-0.293895572546205,0.40451255255908,0.866022509672743));
#131372=DIRECTION('',(-0.587785252292477,0.809016994374945,5.56656537619083E-15));
#131373=DIRECTION('center_axis',(-2.35041809182736E-16,-6.8783153219913E-15,
1.));
#131374=DIRECTION('ref_axis',(-1.,1.6412881812189E-30,-2.35041809182736E-16));
#131375=DIRECTION('',(-0.669130606358862,0.743144825477391,4.95431077124156E-15));
#131376=DIRECTION('center_axis',(2.35041809182736E-16,6.8783153219913E-15,
-1.));
#131377=DIRECTION('ref_axis',(-1.,1.57191309186665E-30,-2.35041809182736E-16));
#131378=DIRECTION('',(0.669130606358862,-0.743144825477391,-4.95431077124156E-15));
#131379=DIRECTION('center_axis',(-2.35041809182736E-16,-6.8783153219913E-15,
1.));
#131380=DIRECTION('ref_axis',(-1.,1.6700863880665E-30,-2.35041809182736E-16));
#131381=DIRECTION('center_axis',(0.743144825477391,0.669130606358862,4.77716140639648E-15));
#131382=DIRECTION('ref_axis',(2.35041809182736E-16,6.8783153219913E-15,
-1.));
#131383=DIRECTION('center_axis',(0.743144825477429,0.669130606358819,1.07238164869218E-13));
#131384=DIRECTION('ref_axis',(0.585256059269502,-0.649992703804315,-0.484752338921114));
#131385=DIRECTION('',(0.354588842120036,-0.393810805677314,-0.848044693619244));
#131386=DIRECTION('',(-0.669130606358862,0.743144825477391,4.95431077124156E-15));
#131387=DIRECTION('',(0.354588491315835,-0.393810416069778,0.848045021223112));
#131388=DIRECTION('center_axis',(0.743144825477371,0.669130606358884,3.96974274275828E-14));
#131389=DIRECTION('ref_axis',(0.585254804454859,-0.649991310191462,0.484755722542903));
#131390=DIRECTION('',(0.669130606358862,-0.743144825477391,-5.09512767813147E-15));
#131391=DIRECTION('',(0.334568657340445,-0.371576137911944,-0.866022509672731));
#131392=DIRECTION('center_axis',(-0.743145459032541,-0.669129902721903,
-1.63998892591404E-6));
#131393=DIRECTION('ref_axis',(0.579515507190066,-0.643617175072043,-0.499918702269203));
#131394=DIRECTION('',(0.669130606358862,-0.743144825477391,-5.09512767813147E-15));
#131395=DIRECTION('center_axis',(-0.743144191859853,-0.669131310059748,
-1.64014385074246E-6));
#131396=DIRECTION('ref_axis',(0.579496068163196,-0.64359558551187,0.499969028333786));
#131397=DIRECTION('',(0.334568762114132,-0.371576254274909,0.866022419268951));
#131398=DIRECTION('',(0.669130606358862,-0.743144825477391,-5.09512767813147E-15));
#131399=DIRECTION('center_axis',(0.743144825477391,0.669130606358862,4.77716140639648E-15));
#131400=DIRECTION('ref_axis',(2.35041809182736E-16,6.8783153219913E-15,
-1.));
#131401=DIRECTION('center_axis',(-0.743144825477371,-0.669130606358884,
-6.75407619348696E-14));
#131402=DIRECTION('ref_axis',(0.585254804443369,-0.649991310178721,0.484755722573859));
#131403=DIRECTION('',(-0.354588491315836,0.39381041606978,-0.848045021223111));
#131404=DIRECTION('',(0.669130606358862,-0.743144825477391,-4.95431077124156E-15));
#131405=DIRECTION('',(-0.354588842120062,0.393810805677293,0.848044693619243));
#131406=DIRECTION('center_axis',(-0.743144825477435,-0.669130606358813,
-9.70381337754059E-14));
#131407=DIRECTION('ref_axis',(0.585256059282122,-0.649992703818349,-0.484752338887059));
#131408=DIRECTION('',(-0.669130606358862,0.743144825477391,5.09512767813147E-15));
#131409=DIRECTION('',(-0.334568762114163,0.371576254274904,-0.86602241926894));
#131410=DIRECTION('center_axis',(0.743145459179803,0.669129902558351,-1.64037053045256E-6));
#131411=DIRECTION('ref_axis',(0.579515575900153,-0.643617251382659,0.499918524373468));
#131412=DIRECTION('',(-0.669130606358862,0.743144825477391,5.09512767813147E-15));
#131413=DIRECTION('center_axis',(0.743144192001209,0.669131309902759,-1.63977761596072E-6));
#131414=DIRECTION('ref_axis',(0.579495997099647,-0.643595506588175,-0.499969212297114));
#131415=DIRECTION('',(-0.334568657340465,0.371576137911926,0.866022509672731));
#131416=DIRECTION('',(-0.669130606358862,0.743144825477391,5.09512767813147E-15));
#131417=DIRECTION('center_axis',(-2.4546426258488E-16,-6.88873777539344E-15,
1.));
#131418=DIRECTION('ref_axis',(-1.,1.714067784336E-30,-2.4546426258488E-16));
#131419=DIRECTION('',(-0.743144825477398,0.669130606358854,4.42704978811658E-15));
#131420=DIRECTION('center_axis',(2.4546426258488E-16,6.88873777539344E-15,
-1.));
#131421=DIRECTION('ref_axis',(-1.,1.54864157893911E-30,-2.4546426258488E-16));
#131422=DIRECTION('',(0.743144825477398,-0.669130606358854,-4.42704978811658E-15));
#131423=DIRECTION('center_axis',(-2.4546426258488E-16,-6.88873777539344E-15,
1.));
#131424=DIRECTION('ref_axis',(-1.,1.6912719677966E-30,-2.4546426258488E-16));
#131425=DIRECTION('center_axis',(0.669130606358854,0.743144825477398,5.28357748271717E-15));
#131426=DIRECTION('ref_axis',(2.4546426258488E-16,6.88873777539344E-15,
-1.));
#131427=DIRECTION('center_axis',(0.669130606358848,0.743144825477403,-9.09732504031885E-15));
#131428=DIRECTION('ref_axis',(0.649992703803272,-0.585256059268544,-0.484752338923668));
#131429=DIRECTION('',(0.393810805677323,-0.354588842120038,-0.848044693619239));
#131430=DIRECTION('',(-0.743144825477398,0.669130606358854,4.42704978811658E-15));
#131431=DIRECTION('',(0.393810416069788,-0.354588491315845,0.848045021223103));
#131432=DIRECTION('center_axis',(0.669130606358885,0.74314482547737,-4.46596058560287E-14));
#131433=DIRECTION('ref_axis',(0.649991310190434,-0.585254804453932,0.4847557225454));
#131434=DIRECTION('',(0.743144825477398,-0.669130606358854,-4.56786669500649E-15));
#131435=DIRECTION('',(0.371576137911948,-0.334568657340484,-0.866022509672714));
#131436=DIRECTION('center_axis',(-0.669131309993376,-0.743144191919616,
-1.63998892143862E-6));
#131437=DIRECTION('ref_axis',(0.643617174848185,-0.579515507437152,-0.499918702270981));
#131438=DIRECTION('',(0.743144825477398,-0.669130606358854,-4.56786669500649E-15));
#131439=DIRECTION('center_axis',(-0.669129902655549,-0.743145459092287,
-1.64014392097245E-6));
#131440=DIRECTION('ref_axis',(0.643595585587833,-0.579496068079466,0.499969028333048));
#131441=DIRECTION('',(0.371576254274914,-0.334568762114171,0.866022419268933));
#131442=DIRECTION('',(0.743144825477398,-0.669130606358854,-4.56786669500649E-15));
#131443=DIRECTION('center_axis',(0.669130606358854,0.743144825477398,5.28357748271717E-15));
#131444=DIRECTION('ref_axis',(2.4546426258488E-16,6.88873777539344E-15,
-1.));
#131445=DIRECTION('center_axis',(-0.669130606358856,-0.743144825477396,
2.3156832663386E-14));
#131446=DIRECTION('ref_axis',(0.649991310178511,-0.585254804443164,0.484755722574387));
#131447=DIRECTION('',(-0.393810416069763,0.35458849131586,-0.848045021223108));
#131448=DIRECTION('',(0.743144825477398,-0.669130606358854,-4.42704978811658E-15));
#131449=DIRECTION('',(-0.393810805677305,0.354588842120013,0.848044693619257));
#131450=DIRECTION('center_axis',(-0.669130606358852,-0.7431448254774,-1.18540902055189E-14));
#131451=DIRECTION('ref_axis',(0.649992703818265,-0.585256059282037,-0.484752338887274));
#131452=DIRECTION('',(-0.743144825477398,0.669130606358854,4.56786669500649E-15));
#131453=DIRECTION('',(-0.3715762542749,0.334568762114124,-0.866022419268957));
#131454=DIRECTION('center_axis',(0.669131310156853,0.743144191772419,-1.64037024591789E-6));
#131455=DIRECTION('ref_axis',(0.643617251157576,-0.579515576146809,0.499918524377321));
#131456=DIRECTION('',(-0.743144825477398,0.669130606358854,4.56786669500649E-15));
#131457=DIRECTION('center_axis',(0.669129902812627,0.743145458950854,-1.63977753884496E-6));
#131458=DIRECTION('ref_axis',(0.643595506662832,-0.57949599701545,-0.4999692122986));
#131459=DIRECTION('',(-0.371576137911895,0.334568657340398,0.86602250967277));
#131460=DIRECTION('',(-0.743144825477398,0.669130606358854,4.56786669500649E-15));
#131461=DIRECTION('center_axis',(-2.54740177659163E-16,-6.90019257654294E-15,
1.));
#131462=DIRECTION('ref_axis',(-1.,1.77884115310111E-30,-2.54740177659163E-16));
#131463=DIRECTION('',(-0.80901699437495,0.587785252292469,3.84974230159355E-15));
#131464=DIRECTION('center_axis',(2.54740177659163E-16,6.90019257654294E-15,
-1.));
#131465=DIRECTION('ref_axis',(-1.,-1.4388490399142E-13,-2.54740177660156E-16));
#131466=DIRECTION('',(0.80901699437495,-0.587785252292469,-3.84974230159355E-15));
#131467=DIRECTION('center_axis',(-2.54740177659163E-16,-6.90019257654294E-15,
1.));
#131468=DIRECTION('ref_axis',(-1.,1.65392111781157E-30,-2.54740177659163E-16));
#131469=DIRECTION('center_axis',(0.587785252292469,0.80901699437495,5.73210557847753E-15));
#131470=DIRECTION('ref_axis',(2.54740177659164E-16,6.90019257654294E-15,
-1.));
#131471=DIRECTION('center_axis',(0.587785252292465,0.809016994374953,-2.72919751209577E-14));
#131472=DIRECTION('ref_axis',(0.707607892255939,-0.51410722687618,-0.484752338922456));
#131473=DIRECTION('',(0.428718095637376,-0.311481929006005,-0.848044693619245));
#131474=DIRECTION('',(-0.80901699437495,0.587785252292469,3.84974230159355E-15));
#131475=DIRECTION('',(0.428717671495123,-0.311481620848632,0.848045021223112));
#131476=DIRECTION('center_axis',(0.587785252292479,0.809016994374943,-1.0613548305292E-14));
#131477=DIRECTION('ref_axis',(0.707606375113318,-0.514106124607541,0.484755722544878));
#131478=DIRECTION('',(0.80901699437495,-0.587785252292469,-3.99055920848346E-15));
#131479=DIRECTION('',(0.40451255255906,-0.293895572546216,-0.866022509672749));
#131480=DIRECTION('center_axis',(-0.587786018297275,-0.809016437837666,
-1.63998894467645E-6));
#131481=DIRECTION('ref_axis',(0.700667238054855,-0.509064546632989,-0.49991870226861));
#131482=DIRECTION('',(0.80901699437495,-0.587785252292469,-3.99055920848346E-15));
#131483=DIRECTION('center_axis',(-0.587784486213231,-0.80901755096188,-1.64014414198988E-6));
#131484=DIRECTION('ref_axis',(0.700643735095494,-0.509047470457538,0.499969028332974));
#131485=DIRECTION('',(0.404512679236436,-0.293895664582665,0.866022419268967));
#131486=DIRECTION('',(0.80901699437495,-0.587785252292469,-3.99055920848346E-15));
#131487=DIRECTION('center_axis',(0.587785252292469,0.80901699437495,5.73210557847753E-15));
#131488=DIRECTION('ref_axis',(2.54740177659164E-16,6.90019257654294E-15,
-1.));
#131489=DIRECTION('center_axis',(-0.58778525229251,-0.809016994374921,1.17438222792872E-13));
#131490=DIRECTION('ref_axis',(0.707606375100373,-0.514106124598113,0.484755722573772));
#131491=DIRECTION('',(-0.428717671495135,0.311481620848657,-0.848045021223097));
#131492=DIRECTION('',(0.80901699437495,-0.587785252292469,-3.84974230159355E-15));
#131493=DIRECTION('',(-0.428718095637387,0.311481929006017,0.848044693619235));
#131494=DIRECTION('center_axis',(-0.587785252292488,-0.809016994374937,
-2.37081804110383E-14));
#131495=DIRECTION('ref_axis',(0.707607892271278,-0.514107226887325,-0.484752338888244));
#131496=DIRECTION('',(-0.80901699437495,0.587785252292469,3.99055920848346E-15));
#131497=DIRECTION('',(-0.404512679236475,0.293895664582667,-0.866022419268948));
#131498=DIRECTION('center_axis',(0.58778601847531,0.809016437708315,-1.64037048156678E-6));
#131499=DIRECTION('ref_axis',(0.700667321127577,-0.509064606989155,0.499918524376605));
#131500=DIRECTION('',(-0.80901699437495,0.587785252292469,3.99055920848346E-15));
#131501=DIRECTION('center_axis',(0.587784486384294,0.809017550837597,-1.63977761045217E-6));
#131502=DIRECTION('ref_axis',(0.700643649175082,-0.509047408033036,-0.49996921229759));
#131503=DIRECTION('',(-0.404512552559104,0.293895572546197,0.866022509672734));
#131504=DIRECTION('',(-0.80901699437495,0.587785252292469,3.99055920848346E-15));
#131505=DIRECTION('center_axis',(-2.62767925538921E-16,-6.91255422424131E-15,
1.));
#131506=DIRECTION('ref_axis',(-1.,1.83489861693133E-30,-2.62767925538921E-16));
#131507=DIRECTION('',(-0.866025403784441,0.499999999999995,3.22871341330418E-15));
#131508=DIRECTION('center_axis',(2.62767925538921E-16,6.91255422424131E-15,
-1.));
#131509=DIRECTION('ref_axis',(-1.,-1.19904086659517E-13,-2.6276792553975E-16));
#131510=DIRECTION('',(0.866025403784441,-0.499999999999995,-3.22871341330418E-15));
#131511=DIRECTION('center_axis',(-2.62767925538921E-16,-6.91255422424131E-15,
1.));
#131512=DIRECTION('ref_axis',(-1.,1.65859733677587E-30,-2.62767925538921E-16));
#131513=DIRECTION('center_axis',(0.499999999999995,0.866025403784442,6.11783152599989E-15));
#131514=DIRECTION('ref_axis',(2.62767925538921E-16,6.91255422424131E-15,
-1.));
#131515=DIRECTION('center_axis',(0.499999999999996,0.866025403784441,3.41838880302928E-14));
#131516=DIRECTION('ref_axis',(0.757470380564982,-0.437325728122336,-0.484752338920618));
#131517=DIRECTION('',(0.458928260426605,-0.264962354696014,-0.848044693619242));
#131518=DIRECTION('',(-0.866025403784442,0.499999999999995,3.22871341330418E-15));
#131519=DIRECTION('',(0.458927806396632,-0.264962092561704,0.848045021223106));
#131520=DIRECTION('center_axis',(0.499999999999982,0.866025403784449,3.4597410709456E-14));
#131521=DIRECTION('ref_axis',(0.757468756515396,-0.437324790476894,0.484755722542148));
#131522=DIRECTION('',(0.866025403784442,-0.499999999999995,-3.36953032019409E-15));
#131523=DIRECTION('',(0.43301704303075,-0.250002506357463,-0.866022509672752));
#131524=DIRECTION('center_axis',(-0.500000819982456,-0.866024930365277,
-1.63998877357693E-6));
#131525=DIRECTION('ref_axis',(0.75004064437554,-0.433036168125902,-0.49991870227024));
#131526=DIRECTION('',(0.866025403784442,-0.499999999999995,-3.36953032019409E-15));
#131527=DIRECTION('center_axis',(-0.4999991799383,-0.866025877245211,-1.64014404112045E-6));
#131528=DIRECTION('ref_axis',(0.75001548522118,-0.433021642223581,0.499969028335187));
#131529=DIRECTION('',(0.433017178634605,-0.250002584648423,0.866022419268944));
#131530=DIRECTION('',(0.866025403784442,-0.499999999999995,-3.36953032019409E-15));
#131531=DIRECTION('center_axis',(0.499999999999995,0.866025403784442,6.11783152599989E-15));
#131532=DIRECTION('ref_axis',(2.62767925538921E-16,6.91255422424131E-15,
-1.));
#131533=DIRECTION('center_axis',(-0.500000000000014,-0.866025403784431,
5.2378550071941E-14));
#131534=DIRECTION('ref_axis',(0.757468756500337,-0.437324790468187,0.484755722573535));
#131535=DIRECTION('',(-0.458927806396645,0.264962092561697,-0.848045021223101));
#131536=DIRECTION('',(0.866025403784442,-0.499999999999995,-3.22871341330418E-15));
#131537=DIRECTION('',(-0.458928260426594,0.264962354696015,0.848044693619248));
#131538=DIRECTION('center_axis',(-0.5,-0.866025403784439,-4.50731104326131E-14));
#131539=DIRECTION('ref_axis',(0.757470380581421,-0.437325728131826,-0.484752338886368));
#131540=DIRECTION('',(-0.866025403784442,0.499999999999995,3.36953032019409E-15));
#131541=DIRECTION('',(-0.433017178634586,0.250002584648412,-0.866022419268957));
#131542=DIRECTION('center_axis',(0.500000820173086,0.866024930255215,-1.64037043715635E-6));
#131543=DIRECTION('ref_axis',(0.750040733300453,-0.433036219466989,0.499918524381581));
#131544=DIRECTION('',(-0.866025403784442,0.499999999999995,3.36953032019409E-15));
#131545=DIRECTION('center_axis',(0.499999180121306,0.866025877139554,-1.63977767534645E-6));
#131546=DIRECTION('ref_axis',(0.750015393247303,-0.433021589122715,-0.499969212297849));
#131547=DIRECTION('',(-0.433017043030757,0.250002506357464,0.866022509672748));
#131548=DIRECTION('',(-0.866025403784442,0.499999999999995,3.36953032019409E-15));
#131549=DIRECTION('center_axis',(-2.6945955253847E-16,-6.92568728168955E-15,
1.));
#131550=DIRECTION('ref_axis',(-1.,1.88162599852217E-30,-2.6945955253847E-16));
#131551=DIRECTION('',(-0.913545457642603,0.406736643075795,2.57076724570721E-15));
#131552=DIRECTION('center_axis',(2.6945955253847E-16,6.92568728168955E-15,
-1.));
#131553=DIRECTION('ref_axis',(-1.,4.79616346638067E-14,-2.69459552538137E-16));
#131554=DIRECTION('',(0.913545457642603,-0.406736643075795,-2.57076724570721E-15));
#131555=DIRECTION('center_axis',(-2.6945955253847E-16,-6.92568728168955E-15,
1.));
#131556=DIRECTION('ref_axis',(-1.,2.07166276942212E-30,-2.6945955253847E-16));
#131557=DIRECTION('center_axis',(0.406736643075795,0.913545457642603,6.43652923108484E-15));
#131558=DIRECTION('ref_axis',(2.6945955253847E-16,6.92568728168955E-15,
-1.));
#131559=DIRECTION('center_axis',(0.406736643075755,0.913545457642621,-7.60867185190334E-14));
#131560=DIRECTION('ref_axis',(0.799033864872018,-0.355752797173961,-0.484752338922246));
#131561=DIRECTION('',(0.484110311157685,-0.215539797381024,-0.848044693619243));
#131562=DIRECTION('',(-0.913545457642603,0.406736643075795,2.5707672457072E-15));
#131563=DIRECTION('',(0.484109832214428,-0.21553958414178,0.848045021223111));
#131564=DIRECTION('center_axis',(0.406736643075769,0.913545457642615,5.37569329748505E-14));
#131565=DIRECTION('ref_axis',(0.799032151707873,-0.355752034424143,0.484755722545047));
#131566=DIRECTION('',(0.913545457642603,-0.406736643075795,-2.71158415259712E-15));
#131567=DIRECTION('',(0.456777308164332,-0.203370360392738,-0.866022509672742));
#131568=DIRECTION('center_axis',(-0.406737508052088,-0.913545072528383,
-1.63998878579854E-6));
#131569=DIRECTION('ref_axis',(0.791196448440653,-0.352263354742521,-0.499918702271121));
#131570=DIRECTION('',(0.913545457642603,-0.406736643075795,-2.71158415259712E-15));
#131571=DIRECTION('center_axis',(-0.406735778016336,-0.913545842789926,
-1.6401440662521E-6));
#131572=DIRECTION('ref_axis',(0.791169908742451,-0.352251538263208,0.499969028332421));
#131573=DIRECTION('',(0.456777451208934,-0.203370424080325,0.866022419268958));
#131574=DIRECTION('',(0.913545457642603,-0.406736643075795,-2.71158415259712E-15));
#131575=DIRECTION('center_axis',(0.406736643075795,0.913545457642603,6.43652923108484E-15));
#131576=DIRECTION('ref_axis',(2.6945955253847E-16,6.92568728168955E-15,
-1.));
#131577=DIRECTION('center_axis',(-0.406736643075775,-0.913545457642612,
-2.39838624013607E-14));
#131578=DIRECTION('ref_axis',(0.799032151693213,-0.355752034417607,0.484755722574007));
#131579=DIRECTION('',(-0.48410983221445,0.215539584141779,-0.848045021223099));
#131580=DIRECTION('',(0.913545457642603,-0.406736643075795,-2.5707672457072E-15));
#131581=DIRECTION('',(-0.484110311157682,0.21553979738103,0.848044693619243));
#131582=DIRECTION('center_axis',(-0.40673664307581,-0.913545457642596,-1.53000466606117E-14));
#131583=DIRECTION('ref_axis',(0.799033864890076,-0.35575279718201,-0.484752338886573));
#131584=DIRECTION('',(-0.913545457642603,0.406736643075795,2.71158415259712E-15));
#131585=DIRECTION('',(-0.456777451208944,0.203370424080347,-0.866022419268947));
#131586=DIRECTION('center_axis',(0.406737508253247,0.91354507243882,-1.6403705445672E-6));
#131587=DIRECTION('ref_axis',(0.791196542249301,-0.352263396509092,0.49991852437435));
#131588=DIRECTION('',(-0.913545457642603,0.406736643075795,2.71158415259712E-15));
#131589=DIRECTION('center_axis',(0.406735778209435,0.913545842703954,-1.63977762938691E-6));
#131590=DIRECTION('ref_axis',(0.791169811721884,-0.352251495067145,-0.499969212295037));
#131591=DIRECTION('',(-0.456777308164335,0.203370360392759,0.866022509672736));
#131592=DIRECTION('',(-0.913545457642603,0.406736643075795,2.71158415259712E-15));
#131593=DIRECTION('center_axis',(-2.74741743792088E-16,-6.93944786036197E-15,
1.));
#131594=DIRECTION('ref_axis',(-1.,1.91851134290259E-30,-2.74741743792088E-16));
#131595=DIRECTION('',(-0.951056516295155,0.309016994374942,1.88311239469892E-15));
#131596=DIRECTION('center_axis',(2.74741743792088E-16,6.93944786036197E-15,
-1.));
#131597=DIRECTION('ref_axis',(-1.,3.5527136788005E-14,-2.74741743791841E-16));
#131598=DIRECTION('',(0.951056516295155,-0.309016994374942,-1.88311239469892E-15));
#131599=DIRECTION('center_axis',(-2.74741743792088E-16,-6.93944786036197E-15,
1.));
#131600=DIRECTION('ref_axis',(-1.,2.10828553426994E-30,-2.74741743792088E-16));
#131601=DIRECTION('center_axis',(0.309016994374942,0.951056516295155,6.68470697498369E-15));
#131602=DIRECTION('ref_axis',(2.74741743792088E-16,6.93944786036197E-15,
-1.));
#131603=DIRECTION('center_axis',(0.309016994374954,0.951056516295151,2.34325038917348E-14));
#131604=DIRECTION('ref_axis',(0.831842966947239,-0.270282164133971,-0.484752338923158));
#131605=DIRECTION('',(0.503988348013129,-0.163755740941344,-0.848044693619239));
#131606=DIRECTION('',(-0.951056516295155,0.309016994374942,1.88311239469892E-15));
#131607=DIRECTION('',(0.503987849404003,-0.163755578933424,0.848045021223111));
#131608=DIRECTION('center_axis',(0.309016994374937,0.951056516295157,9.51084198785806E-15));
#131609=DIRECTION('ref_axis',(0.83184118343951,-0.270281584637182,0.484755722544839));
#131610=DIRECTION('',(0.951056516295155,-0.309016994374942,-2.02392930158883E-15));
#131611=DIRECTION('',(0.475533025522856,-0.154510046201578,-0.866022509672736));
#131612=DIRECTION('center_axis',(-0.309017894868182,-0.95105622370528,-1.63998878906873E-6));
#131613=DIRECTION('ref_axis',(0.823683738647416,-0.26763107032859,-0.499918702273269));
#131614=DIRECTION('',(0.951056516295155,-0.309016994374942,-2.02392930158883E-15));
#131615=DIRECTION('center_axis',(-0.309016093795536,-0.951056808909257,
-1.64014398896477E-6));
#131616=DIRECTION('ref_axis',(0.823656109179533,-0.267622092735545,0.499969028331835));
#131617=DIRECTION('',(0.475533174441014,-0.154510094588067,0.866022419268946));
#131618=DIRECTION('',(0.951056516295155,-0.309016994374942,-2.02392930158883E-15));
#131619=DIRECTION('center_axis',(0.309016994374942,0.951056516295155,6.68470697498369E-15));
#131620=DIRECTION('ref_axis',(2.74741743792088E-16,6.93944786036197E-15,
-1.));
#131621=DIRECTION('center_axis',(-0.309016994374951,-0.951056516295152,
3.72163382090124E-15));
#131622=DIRECTION('ref_axis',(0.831841183423651,-0.270281584632036,0.484755722574922));
#131623=DIRECTION('',(-0.503987849404007,0.163755578933431,-0.848045021223107));
#131624=DIRECTION('',(0.951056516295155,-0.309016994374942,-1.88311239469892E-15));
#131625=DIRECTION('',(-0.503988348013115,0.163755740941334,0.848044693619249));
#131626=DIRECTION('center_axis',(-0.309016994374943,-0.951056516295155,
-1.51622084024086E-14));
#131627=DIRECTION('ref_axis',(0.831842966966906,-0.270282164140354,-0.48475233888585));
#131628=DIRECTION('',(-0.951056516295155,0.309016994374942,2.02392930158883E-15));
#131629=DIRECTION('',(-0.475533174441028,0.154510094588078,-0.866022419268937));
#131630=DIRECTION('center_axis',(0.30901789507753,0.951056223637258,-1.64037039627468E-6));
#131631=DIRECTION('ref_axis',(0.823683836309039,-0.267631102061046,0.499918524374537));
#131632=DIRECTION('',(-0.951056516295155,0.309016994374942,2.02392930158883E-15));
#131633=DIRECTION('center_axis',(0.309016093996548,0.951056808843945,-1.63977760305072E-6));
#131634=DIRECTION('ref_axis',(0.823656008173282,-0.267622059916903,-0.499969212298005));
#131635=DIRECTION('',(-0.475533025522834,0.154510046201571,0.86602250967275));
#131636=DIRECTION('',(-0.951056516295155,0.309016994374942,2.02392930158883E-15));
#131637=DIRECTION('center_axis',(-2.78556626507032E-16,-6.95368519647906E-15,
1.));
#131638=DIRECTION('ref_axis',(-1.,1.9451505265208E-30,-2.78556626507032E-16));
#131639=DIRECTION('',(-0.978147600733807,0.207911690817753,1.17328295072798E-15));
#131640=DIRECTION('center_axis',(2.78556626507032E-16,6.95368519647906E-15,
-1.));
#131641=DIRECTION('ref_axis',(-1.,1.15463194561016E-14,-2.78556626506952E-16));
#131642=DIRECTION('',(0.978147600733807,-0.207911690817753,-1.17328295072798E-15));
#131643=DIRECTION('center_axis',(-2.78556626507032E-16,-6.95368519647906E-15,
1.));
#131644=DIRECTION('ref_axis',(-1.,2.08376587424813E-30,-2.78556626507032E-16));
#131645=DIRECTION('center_axis',(0.207911690817753,0.978147600733807,6.85964567039975E-15));
#131646=DIRECTION('ref_axis',(2.78556626507032E-16,6.95368519647906E-15,
-1.));
#131647=DIRECTION('center_axis',(0.207911690817757,0.978147600733806,1.02000311058128E-14));
#131648=DIRECTION('ref_axis',(0.855538223403065,-0.181850263143827,-0.484752338922514));
#131649=DIRECTION('',(0.518344583061388,-0.110177542335806,-0.848044693619244));
#131650=DIRECTION('',(-0.978147600733807,0.207911690817753,1.17328295072798E-15));
#131651=DIRECTION('',(0.518344070249267,-0.110177433334231,0.848045021223109));
#131652=DIRECTION('center_axis',(0.207911690817748,0.978147600733808,1.44730204163055E-14));
#131653=DIRECTION('ref_axis',(0.855536389092135,-0.181849873249007,0.484755722543334));
#131654=DIRECTION('',(0.978147600733807,-0.207911690817753,-1.3140998576179E-15));
#131655=DIRECTION('',(0.489078703542099,-0.103956887610937,-0.866022509672714));
#131656=DIRECTION('center_axis',(-0.207912616961996,-0.978147403873938,
-1.63998882728223E-6));
#131657=DIRECTION('ref_axis',(0.847146577450082,-0.180066563903755,-0.499918702269186));
#131658=DIRECTION('',(0.978147600733807,-0.207911690817753,-1.3140998576179E-15));
#131659=DIRECTION('center_axis',(-0.207910764585316,-0.978147797608756,
-1.64014404456341E-6));
#131660=DIRECTION('ref_axis',(0.847118160920355,-0.180060523555695,0.49996902833652));
#131661=DIRECTION('',(0.489078856702179,-0.10395692016613,0.86602241926896));
#131662=DIRECTION('',(0.978147600733807,-0.207911690817753,-1.3140998576179E-15));
#131663=DIRECTION('center_axis',(0.207911690817753,0.978147600733807,6.85964567039975E-15));
#131664=DIRECTION('ref_axis',(2.78556626507032E-16,6.95368519647906E-15,
-1.));
#131665=DIRECTION('center_axis',(-0.207911690817752,-0.978147600733807,
2.89460408292303E-15));
#131666=DIRECTION('ref_axis',(0.855536389075788,-0.181849873245528,0.48475572257349));
#131667=DIRECTION('',(-0.518344070249267,0.110177433334231,-0.848045021223109));
#131668=DIRECTION('',(0.978147600733807,-0.207911690817753,-1.17328295072798E-15));
#131669=DIRECTION('',(-0.518344583061402,0.110177542335803,0.848044693619236));
#131670=DIRECTION('center_axis',(-0.207911690817764,-0.978147600733805,
-2.43973717020567E-14));
#131671=DIRECTION('ref_axis',(0.855538223422352,-0.181850263147927,-0.484752338886936));
#131672=DIRECTION('',(-0.978147600733807,0.207911690817753,1.3140998576179E-15));
#131673=DIRECTION('',(-0.489078856702203,0.103956920166127,-0.866022419268947));
#131674=DIRECTION('center_axis',(0.207912617177298,0.978147403828173,-1.64037041701691E-6));
#131675=DIRECTION('ref_axis',(0.84714667788718,-0.180066585252583,0.499918524381912));
#131676=DIRECTION('',(-0.978147600733807,0.207911690817753,1.3140998576179E-15));
#131677=DIRECTION('center_axis',(0.207910764792091,0.978147797564805,-1.63977752223453E-6));
#131678=DIRECTION('ref_axis',(0.847118057038102,-0.180060501475074,-0.499969212300654));
#131679=DIRECTION('',(-0.489078703542011,0.103956887610907,0.866022509672768));
#131680=DIRECTION('',(-0.978147600733807,0.207911690817753,1.3140998576179E-15));
#131681=DIRECTION('center_axis',(-2.80862404029962E-16,-6.96824330280696E-15,
1.));
#131682=DIRECTION('ref_axis',(-1.,1.96125168490647E-30,-2.80862404029962E-16));
#131683=DIRECTION('',(-0.994521895368274,0.104528463267647,4.49055953723918E-16));
#131684=DIRECTION('center_axis',(2.80862404029962E-16,6.96824330280696E-15,
-1.));
#131685=DIRECTION('ref_axis',(-1.,2.66453525910038E-15,-2.80862404029943E-16));
#131686=DIRECTION('',(0.994521895368274,-0.104528463267647,-4.49055953723918E-16));
#131687=DIRECTION('center_axis',(-2.80862404029962E-16,-6.96824330280696E-15,
1.));
#131688=DIRECTION('ref_axis',(-1.,2.09982394861192E-30,-2.80862404029962E-16));
#131689=DIRECTION('center_axis',(0.104528463267647,0.994521895368274,6.95942865237777E-15));
#131690=DIRECTION('ref_axis',(2.80862404029962E-16,6.96824330280696E-15,
-1.));
#131691=DIRECTION('center_axis',(0.104528463267647,0.994521895368274,3.92839035831992E-15));
#131692=DIRECTION('ref_axis',(0.869860024050247,-0.0914259726159766,-0.484752338922182));
#131693=DIRECTION('',(0.527021726387053,-0.0553922155202972,-0.848044693619247));
#131694=DIRECTION('',(-0.994521895368274,0.104528463267647,4.49055953723918E-16));
#131695=DIRECTION('',(0.527021204990422,-0.0553921607193138,0.8480450212231));
#131696=DIRECTION('center_axis',(0.104528463267653,0.994521895368273,1.72297862098881E-15));
#131697=DIRECTION('ref_axis',(0.869858159032045,-0.0914257765946727,0.484755722544297));
#131698=DIRECTION('',(0.994521895368274,-0.104528463267647,-5.89872860613828E-16));
#131699=DIRECTION('',(0.497265932938961,-0.0522647556052135,-0.866022509672741));
#131700=DIRECTION('center_axis',(-0.104529404915856,-0.994521796395256,
-1.63998887823304E-6));
#131701=DIRECTION('ref_axis',(0.861327901070945,-0.0905292105226773,-0.499918702269541));
#131702=DIRECTION('',(0.994521895368274,-0.104528463267647,-5.89872860613828E-16));
#131703=DIRECTION('center_axis',(-0.10452752153017,-0.994521994347068,-1.64014402515561E-6));
#131704=DIRECTION('ref_axis',(0.861299008823507,-0.0905261736006502,0.499969028333625));
#131705=DIRECTION('',(0.497266088663018,-0.0522647719724938,0.866022419268951));
#131706=DIRECTION('',(0.994521895368274,-0.104528463267647,-5.89872860613828E-16));
#131707=DIRECTION('center_axis',(0.104528463267647,0.994521895368274,6.95942865237777E-15));
#131708=DIRECTION('ref_axis',(2.80862404029962E-16,6.96824330280696E-15,
-1.));
#131709=DIRECTION('center_axis',(-0.104528463267644,-0.994521895368274,
-9.02840797292685E-15));
#131710=DIRECTION('ref_axis',(0.869858159015343,-0.0914257765929128,0.484755722574599));
#131711=DIRECTION('',(-0.527021204990403,0.0553921607193145,-0.848045021223112));
#131712=DIRECTION('',(0.994521895368274,-0.104528463267647,-4.49055953723918E-16));
#131713=DIRECTION('',(-0.527021726387063,0.0553922155202998,0.848044693619241));
#131714=DIRECTION('center_axis',(-0.104528463267641,-0.994521895368275,
3.7216329714999E-15));
#131715=DIRECTION('ref_axis',(0.869860024068749,-0.0914259726179193,-0.484752338888615));
#131716=DIRECTION('',(-0.994521895368274,0.104528463267647,5.89872860613828E-16));
#131717=DIRECTION('',(-0.49726608866303,0.0522647719724906,-0.866022419268944));
#131718=DIRECTION('center_axis',(0.104529405134737,0.99452179637225,-1.6403704179208E-6));
#131719=DIRECTION('ref_axis',(0.861328003191142,-0.090529221256205,0.499918524379227));
#131720=DIRECTION('',(-0.994521895368274,0.104528463267647,5.89872860613828E-16));
#131721=DIRECTION('center_axis',(0.104527521740381,0.994521994324975,-1.6397775587696E-6));
#131722=DIRECTION('ref_axis',(0.861298903200557,-0.0905261624994676,-0.499969212300755));
#131723=DIRECTION('',(-0.497265932938963,0.0522647556052233,0.866022509672739));
#131724=DIRECTION('',(-0.994521895368274,0.104528463267647,5.89872860613828E-16));
#131725=DIRECTION('center_axis',(-2.81633813779821E-16,-6.98296267768627E-15,
1.));
#131726=DIRECTION('ref_axis',(-1.,1.96663841039893E-30,-2.81633813779821E-16));
#131727=DIRECTION('',(-1.,1.96663841039893E-30,-2.81633813779821E-16));
#131728=DIRECTION('',(1.,-1.96663841039893E-30,2.81633813779821E-16));
#131729=DIRECTION('center_axis',(0.,1.,6.98296267768627E-15));
#131730=DIRECTION('ref_axis',(2.81633813779821E-16,6.98296267768627E-15,
-1.));
#131731=DIRECTION('center_axis',(2.50576143790467E-16,1.,7.42579081592464E-15));
#131732=DIRECTION('ref_axis',(0.874651456242924,3.38050267731257E-15,-0.48475233892384));
#131733=DIRECTION('',(0.529924709392056,5.93414301348777E-15,-0.848044693619236));
#131734=DIRECTION('',(-1.,1.96663841039893E-30,-2.81633813779821E-16));
#131735=DIRECTION('',(0.529924185123406,-5.93414530587669E-15,0.848045021223104));
#131736=DIRECTION('center_axis',(-2.50577545723561E-16,1.,7.42579288222807E-15));
#131737=DIRECTION('ref_axis',(0.874649580953153,-3.38052804871796E-15,0.484755722543297));
#131738=DIRECTION('',(1.,-9.83319205199467E-31,1.40816906889911E-16));
#131739=DIRECTION('',(0.500005012714991,5.91835148258668E-15,-0.866022509672746));
#131740=DIRECTION('center_axis',(-9.46835262596884E-7,-0.999999999998207,
-1.63998887409855E-6));
#131741=DIRECTION('ref_axis',(0.866072335963508,-1.66717974320025E-10,-0.499918702269391));
#131742=DIRECTION('',(1.,-9.83319205199467E-31,1.40816906889911E-16));
#131743=DIRECTION('center_axis',(9.46924640381337E-7,-0.999999999998207,
-1.64014403445674E-6));
#131744=DIRECTION('ref_axis',(0.866043284544476,5.65065332453387E-11,0.499969028336172));
#131745=DIRECTION('',(0.50000516929686,-5.91835086477054E-15,0.866022419268935));
#131746=DIRECTION('',(1.,-9.83319205199467E-31,1.40816906889911E-16));
#131747=DIRECTION('center_axis',(0.,1.,6.98296267768627E-15));
#131748=DIRECTION('ref_axis',(2.81633813779821E-16,6.98296267768627E-15,
-1.));
#131749=DIRECTION('center_axis',(5.53239297233671E-17,-1.,-7.21882753498418E-15));
#131750=DIRECTION('ref_axis',(0.874649580936035,-3.45097890591139E-15,0.484755722574184));
#131751=DIRECTION('',(-0.529924185123415,5.88254404234729E-15,-0.848045021223098));
#131752=DIRECTION('',(1.,-1.96663841039893E-30,2.81633813779821E-16));
#131753=DIRECTION('',(-0.529924709392047,-5.88254176989226E-15,0.848044693619242));
#131754=DIRECTION('center_axis',(-5.53227018708228E-17,-1.,-7.21882542204734E-15));
#131755=DIRECTION('ref_axis',(0.874651456262773,3.45095442560608E-15,-0.484752338888025));
#131756=DIRECTION('',(-1.,9.83319205199467E-31,-1.40816906889911E-16));
#131757=DIRECTION('',(-0.50000516929686,6.05598693139311E-15,-0.866022419268935));
#131758=DIRECTION('center_axis',(9.47055349398689E-7,0.999999999998206,
-1.64037041837183E-6));
#131759=DIRECTION('ref_axis',(0.866072438647096,-1.66977002397838E-10,0.499918524377595));
#131760=DIRECTION('',(-1.,9.83319205199467E-31,-1.40816906889911E-16));
#131761=DIRECTION('center_axis',(-9.46713274170111E-7,0.999999999998207,
-1.63977756707643E-6));
#131762=DIRECTION('ref_axis',(0.866043178342101,5.62743837908293E-11,-0.499969212299229));
#131763=DIRECTION('',(-0.500005012714993,-6.05598756357666E-15,0.866022509672745));
#131764=DIRECTION('',(-1.,9.83319205199467E-31,-1.40816906889911E-16));
#131765=DIRECTION('center_axis',(-2.80862404029962E-16,-6.99768205256557E-15,
1.));
#131766=DIRECTION('ref_axis',(-1.,1.96125168490646E-30,-2.80862404029962E-16));
#131767=DIRECTION('',(-0.994521895368273,-0.104528463267661,-1.01078076178394E-15));
#131768=DIRECTION('center_axis',(2.80862404029962E-16,6.99768205256557E-15,
-1.));
#131769=DIRECTION('ref_axis',(-1.,-2.29860575018392E-12,-2.80862404046047E-16));
#131770=DIRECTION('',(0.994521895368273,0.104528463267661,1.01078076178394E-15));
#131771=DIRECTION('center_axis',(-2.80862404029962E-16,-6.99768205256557E-15,
1.));
#131772=DIRECTION('ref_axis',(-1.,2.09987333638716E-30,-2.80862404029962E-16));
#131773=DIRECTION('center_axis',(-0.104528463267661,0.994521895368273,6.92998990261915E-15));
#131774=DIRECTION('ref_axis',(2.80862404029962E-16,6.99768205256558E-15,
-1.));
#131775=DIRECTION('center_axis',(-0.104528463267665,0.994521895368272,-3.99730948741319E-15));
#131776=DIRECTION('ref_axis',(0.869860024049594,0.0914259726159237,-0.484752338923364));
#131777=DIRECTION('',(0.527021726387062,0.0553922155203198,-0.84804469361924));
#131778=DIRECTION('',(-0.994521895368273,-0.104528463267661,-1.01078076178394E-15));
#131779=DIRECTION('',(0.527021204990404,0.0553921607193099,0.848045021223112));
#131780=DIRECTION('center_axis',(-0.104528463267673,0.994521895368271,2.43973772732041E-14));
#131781=DIRECTION('ref_axis',(0.869858159031862,0.0914257765946581,0.484755722544626));
#131782=DIRECTION('',(0.994521895368273,0.104528463267661,8.69963854894025E-16));
#131783=DIRECTION('',(0.497265932938987,0.0522647556052302,-0.866022509672725));
#131784=DIRECTION('center_axis',(0.104527521619062,-0.994521994337725,-1.63998890568842E-6));
#131785=DIRECTION('ref_axis',(0.861327901104011,0.0905292101909037,-0.499918702272649));
#131786=DIRECTION('',(0.994521895368273,0.104528463267661,8.69963854894025E-16));
#131787=DIRECTION('center_axis',(0.104529405004759,-0.994521796385912,-1.6401440355691E-6));
#131788=DIRECTION('ref_axis',(0.861299008813094,0.0905261737132066,0.499969028331184));
#131789=DIRECTION('',(0.497266088663019,0.0522647719724762,0.866022419268952));
#131790=DIRECTION('',(0.994521895368273,0.104528463267661,8.69963854894025E-16));
#131791=DIRECTION('center_axis',(-0.104528463267661,0.994521895368273,6.92998990261915E-15));
#131792=DIRECTION('ref_axis',(2.80862404029962E-16,6.99768205256558E-15,
-1.));
#131793=DIRECTION('center_axis',(0.104528463267666,-0.994521895368272,-2.20541263460803E-14));
#131794=DIRECTION('ref_axis',(0.86985815901466,0.0914257765928456,0.484755722575836));
#131795=DIRECTION('',(-0.527021204990422,-0.0553921607193138,-0.8480450212231));
#131796=DIRECTION('',(0.994521895368273,0.104528463267661,1.01078076178394E-15));
#131797=DIRECTION('',(-0.527021726387058,-0.0553922155203158,0.848044693619243));
#131798=DIRECTION('center_axis',(0.10452846326766,-0.994521895368273,-7.96015941126447E-15));
#131799=DIRECTION('ref_axis',(0.869860024068839,0.0914259726179483,-0.484752338888448));
#131800=DIRECTION('',(-0.994521895368273,-0.104528463267661,-8.69963854894025E-16));
#131801=DIRECTION('',(-0.497266088663004,-0.0522647719724695,-0.866022419268961));
#131802=DIRECTION('center_axis',(-0.104527521400179,0.99452199436073,-1.64037044554758E-6));
#131803=DIRECTION('ref_axis',(0.861328003227402,0.0905292209242402,0.499918524376869));
#131804=DIRECTION('',(-0.994521895368273,-0.104528463267661,-8.69963854894025E-16));
#131805=DIRECTION('center_axis',(-0.104529404794561,0.994521796408005,-1.63977758411593E-6));
#131806=DIRECTION('ref_axis',(0.861298903191925,0.0905261626117421,-0.499969212295296));
#131807=DIRECTION('',(-0.497265932938963,-0.0522647556052321,0.866022509672738));
#131808=DIRECTION('',(-0.994521895368273,-0.104528463267661,-8.69963854894025E-16));
#131809=DIRECTION('center_axis',(-2.78556626507032E-16,-7.01224015889348E-15,
1.));
#131810=DIRECTION('ref_axis',(-1.,1.9451505265208E-30,-2.78556626507032E-16));
#131811=DIRECTION('',(-0.978147600733804,-0.207911690817766,-1.73039620374214E-15));
#131812=DIRECTION('center_axis',(2.78556626507032E-16,7.01224015889348E-15,
-1.));
#131813=DIRECTION('ref_axis',(-1.,-2.43272069155864E-12,-2.78556626524091E-16));
#131814=DIRECTION('',(0.978147600733804,0.207911690817766,1.73039620374214E-15));
#131815=DIRECTION('center_axis',(-2.78556626507032E-16,-7.01224015889348E-15,
1.));
#131816=DIRECTION('ref_axis',(-1.,2.08372909397962E-30,-2.78556626507032E-16));
#131817=DIRECTION('center_axis',(-0.207911690817766,0.978147600733804,6.80109070798531E-15));
#131818=DIRECTION('ref_axis',(2.78556626507032E-16,7.01224015889348E-15,
-1.));
#131819=DIRECTION('center_axis',(-0.207911690817786,0.9781476007338,-2.72919751209605E-14));
#131820=DIRECTION('ref_axis',(0.855538223402316,0.181850263143686,-0.48475233892389));
#131821=DIRECTION('',(0.518344583061382,0.110177542335822,-0.848044693619246));
#131822=DIRECTION('',(-0.978147600733804,-0.207911690817766,-1.73039620374214E-15));
#131823=DIRECTION('',(0.518344070249262,0.110177433334227,0.848045021223113));
#131824=DIRECTION('center_axis',(-0.207911690817754,0.978147600733807,-2.06757434518659E-14));
#131825=DIRECTION('ref_axis',(0.855536389092255,0.181849873249041,0.484755722543111));
#131826=DIRECTION('',(0.978147600733804,0.207911690817766,1.58957929685223E-15));
#131827=DIRECTION('',(0.489078703542061,0.103956887610937,-0.866022509672736));
#131828=DIRECTION('center_axis',(0.207910764672762,-0.978147797590169,-1.63998887332749E-6));
#131829=DIRECTION('ref_axis',(0.847146577520758,0.18006656357791,-0.499918702266787));
#131830=DIRECTION('',(0.978147600733804,0.207911690817766,1.58957929685223E-15));
#131831=DIRECTION('center_axis',(0.207912617049462,-0.978147403855346,-1.64014402838238E-6));
#131832=DIRECTION('ref_axis',(0.847118160900355,0.180060523666994,0.499969028330324));
#131833=DIRECTION('',(0.489078856702179,0.10395692016613,0.86602241926896));
#131834=DIRECTION('',(0.978147600733804,0.207911690817766,1.58957929685223E-15));
#131835=DIRECTION('center_axis',(-0.207911690817766,0.978147600733804,6.80109070798531E-15));
#131836=DIRECTION('ref_axis',(2.78556626507032E-16,7.01224015889348E-15,
-1.));
#131837=DIRECTION('center_axis',(0.207911690817764,-0.978147600733805,-1.32324758076486E-14));
#131838=DIRECTION('ref_axis',(0.855536389075988,0.181849873245576,0.48475572257312));
#131839=DIRECTION('',(-0.518344070249253,-0.110177433334228,-0.848045021223118));
#131840=DIRECTION('',(0.978147600733804,0.207911690817766,1.73039620374214E-15));
#131841=DIRECTION('',(-0.518344583061406,-0.11017754233582,0.848044693619231));
#131842=DIRECTION('center_axis',(0.207911690817771,-0.978147600733803,-1.60581570807317E-14));
#131843=DIRECTION('ref_axis',(0.855538223422078,0.181850263147895,-0.484752338887433));
#131844=DIRECTION('',(-0.978147600733804,-0.207911690817766,-1.58957929685223E-15));
#131845=DIRECTION('',(-0.489078856702194,-0.103956920166107,-0.866022419268955));
#131846=DIRECTION('center_axis',(-0.20791076445747,0.97814779763593,-1.64037044223425E-6));
#131847=DIRECTION('ref_axis',(0.847146677959787,0.18006658492662,0.499918524376283));
#131848=DIRECTION('',(-0.978147600733804,-0.207911690817766,-1.58957929685223E-15));
#131849=DIRECTION('center_axis',(-0.207912616842705,0.978147403899295,-1.63977754289028E-6));
#131850=DIRECTION('ref_axis',(0.847118057015926,0.180060501585439,-0.49996921229848));
#131851=DIRECTION('',(-0.489078703542037,-0.103956887610949,0.866022509672748));
#131852=DIRECTION('',(-0.978147600733804,-0.207911690817766,-1.58957929685223E-15));
#131853=DIRECTION('center_axis',(-2.74741743792087E-16,-7.02647749501056E-15,
1.));
#131854=DIRECTION('ref_axis',(-1.,1.91851134290259E-30,-2.74741743792087E-16));
#131855=DIRECTION('',(-0.951056516295151,-0.309016994374954,-2.43259588228318E-15));
#131856=DIRECTION('center_axis',(2.74741743792087E-16,7.02647749501057E-15,
-1.));
#131857=DIRECTION('ref_axis',(-1.,-2.73292499741728E-12,-2.7474174381129E-16));
#131858=DIRECTION('',(0.951056516295151,0.309016994374954,2.43259588228318E-15));
#131859=DIRECTION('center_axis',(-2.74741743792087E-16,-7.02647749501057E-15,
1.));
#131860=DIRECTION('ref_axis',(-1.,2.1085382641719E-30,-2.74741743792087E-16));
#131861=DIRECTION('center_axis',(-0.309016994374955,0.951056516295151,6.59767734033506E-15));
#131862=DIRECTION('ref_axis',(2.74741743792088E-16,7.02647749501057E-15,
-1.));
#131863=DIRECTION('center_axis',(-0.309016994374942,0.951056516295155,3.83190357758892E-14));
#131864=DIRECTION('ref_axis',(0.831842966947115,0.270282164133951,-0.484752338923381));
#131865=DIRECTION('',(0.503988348013127,0.16375574094136,-0.848044693619237));
#131866=DIRECTION('',(-0.951056516295151,-0.309016994374955,-2.43259588228318E-15));
#131867=DIRECTION('',(0.503987849404007,0.163755578933431,0.848045021223107));
#131868=DIRECTION('center_axis',(-0.309016994374941,0.951056516295156,-1.19919312020825E-14));
#131869=DIRECTION('ref_axis',(0.831841183439686,0.270281584637244,0.484755722544503));
#131870=DIRECTION('',(0.951056516295151,0.309016994374955,2.29177897539327E-15));
#131871=DIRECTION('',(0.47553302552288,0.15451004620161,-0.866022509672718));
#131872=DIRECTION('center_axis',(0.309016093880556,-0.951056808881632,-1.63998887048721E-6));
#131873=DIRECTION('ref_axis',(0.823683738754044,0.267631070012658,-0.499918702266717));
#131874=DIRECTION('',(0.951056516295151,0.309016994374955,2.29177897539327E-15));
#131875=DIRECTION('center_axis',(0.309017894953215,-0.951056223677651,-1.64014397020222E-6));
#131876=DIRECTION('ref_axis',(0.823656109144283,0.267622092842959,0.499969028332411));
#131877=DIRECTION('',(0.475533174441003,0.154510094588037,0.866022419268958));
#131878=DIRECTION('',(0.951056516295151,0.309016994374955,2.29177897539327E-15));
#131879=DIRECTION('center_axis',(-0.309016994374955,0.951056516295151,6.59767734033506E-15));
#131880=DIRECTION('ref_axis',(2.74741743792088E-16,7.02647749501057E-15,
-1.));
#131881=DIRECTION('center_axis',(0.309016994374966,-0.951056516295147,-4.13514868989001E-14));
#131882=DIRECTION('ref_axis',(0.831841183424408,0.270281584632277,0.484755722573489));
#131883=DIRECTION('',(-0.503987849403998,-0.163755578933433,-0.848045021223113));
#131884=DIRECTION('',(0.951056516295151,0.309016994374955,2.43259588228318E-15));
#131885=DIRECTION('',(-0.503988348013108,-0.163755740941352,0.84804469361925));
#131886=DIRECTION('center_axis',(0.30901699437492,-0.951056516295162,-7.37434681389843E-14));
#131887=DIRECTION('ref_axis',(0.831842966966455,0.270282164140231,-0.484752338886692));
#131888=DIRECTION('',(-0.951056516295151,-0.309016994374955,-2.29177897539327E-15));
#131889=DIRECTION('',(-0.475533174441042,-0.154510094588038,-0.866022419268936));
#131890=DIRECTION('center_axis',(-0.309016093671208,0.951056808949653,-1.6403705334645E-6));
#131891=DIRECTION('ref_axis',(0.823683836411346,0.267631101743197,0.499918524376132));
#131892=DIRECTION('',(-0.951056516295151,-0.309016994374955,-2.29177897539327E-15));
#131893=DIRECTION('center_axis',(-0.309017894752207,0.951056223742963,-1.63977755898441E-6));
#131894=DIRECTION('ref_axis',(0.823656008137761,0.26762206002369,-0.499969212299362));
#131895=DIRECTION('',(-0.475533025522815,-0.154510046201603,0.866022509672754));
#131896=DIRECTION('',(-0.951056516295151,-0.309016994374955,-2.29177897539327E-15));
#131897=DIRECTION('center_axis',(-2.69459552538469E-16,-7.04023807368299E-15,
1.));
#131898=DIRECTION('ref_axis',(-1.,1.88162599852217E-30,-2.69459552538469E-16));
#131899=DIRECTION('',(-0.913545457642598,-0.406736643075807,-3.10968635078423E-15));
#131900=DIRECTION('center_axis',(2.69459552538469E-16,7.04023807368299E-15,
-1.));
#131901=DIRECTION('ref_axis',(-1.,-1.34203759216689E-12,-2.69459552547917E-16));
#131902=DIRECTION('',(0.913545457642598,0.406736643075807,3.10968635078423E-15));
#131903=DIRECTION('center_axis',(-2.69459552538469E-16,-7.04023807368299E-15,
1.));
#131904=DIRECTION('ref_axis',(-1.,2.07139034025888E-30,-2.69459552538469E-16));
#131905=DIRECTION('center_axis',(-0.406736643075807,0.913545457642598,6.32197843909136E-15));
#131906=DIRECTION('ref_axis',(2.69459552538469E-16,7.04023807368299E-15,
-1.));
#131907=DIRECTION('center_axis',(-0.406736643075815,0.913545457642594,9.64867807306692E-15));
#131908=DIRECTION('ref_axis',(0.799033864871477,0.355752797173747,-0.484752338923296));
#131909=DIRECTION('',(0.484110311157675,0.215539797381046,-0.848044693619243));
#131910=DIRECTION('',(-0.913545457642598,-0.406736643075807,-3.10968635078423E-15));
#131911=DIRECTION('',(0.484109832214418,0.215539584141762,0.848045021223121));
#131912=DIRECTION('center_axis',(-0.406736643075818,0.913545457642593,2.68784664874263E-14));
#131913=DIRECTION('ref_axis',(0.799032151707959,0.35575203442419,0.484755722544869));
#131914=DIRECTION('',(0.913545457642598,0.406736643075807,2.96886944389432E-15));
#131915=DIRECTION('',(0.456777308164318,0.203370360392767,-0.866022509672743));
#131916=DIRECTION('center_axis',(0.406735778098062,-0.913545842753539,-1.63998876755266E-6));
#131917=DIRECTION('ref_axis',(0.791196448576301,0.352263354437902,-0.499918702271085));
#131918=DIRECTION('',(0.913545457642598,0.406736643075807,2.96886944389432E-15));
#131919=DIRECTION('center_axis',(0.406737508133866,-0.913545072491972,-1.64014417590034E-6));
#131920=DIRECTION('ref_axis',(0.791169908699022,0.352251538367612,0.499969028327587));
#131921=DIRECTION('',(0.456777451208935,0.203370424080325,0.866022419268958));
#131922=DIRECTION('',(0.913545457642598,0.406736643075807,2.96886944389432E-15));
#131923=DIRECTION('center_axis',(-0.406736643075807,0.913545457642598,6.32197843909136E-15));
#131924=DIRECTION('ref_axis',(2.69459552538469E-16,7.04023807368299E-15,
-1.));
#131925=DIRECTION('center_axis',(0.406736643075821,-0.913545457642592,-5.01731374373328E-14));
#131926=DIRECTION('ref_axis',(0.799032151694043,0.355752034417985,0.484755722572362));
#131927=DIRECTION('',(-0.484109832214425,-0.215539584141772,-0.848045021223115));
#131928=DIRECTION('',(0.913545457642598,0.406736643075807,3.10968635078423E-15));
#131929=DIRECTION('',(-0.484110311157673,-0.215539797381045,0.848044693619245));
#131930=DIRECTION('center_axis',(0.406736643075753,-0.913545457642622,-9.74516485500229E-14));
#131931=DIRECTION('ref_axis',(0.799033864889399,0.355752797181708,-0.484752338887911));
#131932=DIRECTION('',(-0.913545457642598,-0.406736643075807,-2.96886944389432E-15));
#131933=DIRECTION('',(-0.456777451208932,-0.203370424080342,-0.866022419268955));
#131934=DIRECTION('center_axis',(-0.406735777896963,0.913545842843073,-1.64037041701662E-6));
#131935=DIRECTION('ref_axis',(0.791196542384111,0.352263396203563,0.499918524376282));
#131936=DIRECTION('',(-0.913545457642598,-0.406736643075807,-2.96886944389432E-15));
#131937=DIRECTION('center_axis',(-0.406737507940739,0.913545072577959,-1.63977763214104E-6));
#131938=DIRECTION('ref_axis',(0.791169811676832,0.352251495170301,-0.499969212293651));
#131939=DIRECTION('',(-0.456777308164302,-0.203370360392813,0.86602250967274));
#131940=DIRECTION('',(-0.913545457642598,-0.406736643075807,-2.96886944389432E-15));
#131941=DIRECTION('center_axis',(-2.6276792553892E-16,-7.05337113113122E-15,
1.));
#131942=DIRECTION('ref_axis',(-1.,1.83489861693132E-30,-2.6276792553892E-16));
#131943=DIRECTION('',(-0.866025403784435,-0.500000000000007,-3.7542492643821E-15));
#131944=DIRECTION('center_axis',(2.6276792553892E-16,7.05337113113122E-15,
-1.));
#131945=DIRECTION('ref_axis',(-1.,1.96511414759077E-30,-2.6276792553892E-16));
#131946=DIRECTION('',(0.866025403784435,0.500000000000007,3.7542492643821E-15));
#131947=DIRECTION('center_axis',(-2.6276792553892E-16,-7.05337113113122E-15,
1.));
#131948=DIRECTION('ref_axis',(-1.,1.6583547235129E-30,-2.6276792553892E-16));
#131949=DIRECTION('center_axis',(-0.500000000000007,0.866025403784435,5.97701461910993E-15));
#131950=DIRECTION('ref_axis',(2.6276792553892E-16,7.05337113113122E-15,
-1.));
#131951=DIRECTION('center_axis',(-0.500000000000001,0.866025403784438,3.85947122922661E-15));
#131952=DIRECTION('ref_axis',(0.757470380563486,0.4373257281215,-0.484752338923709));
#131953=DIRECTION('',(0.458928260426603,0.264962354696026,-0.848044693619239));
#131954=DIRECTION('',(-0.866025403784435,-0.500000000000007,-3.7542492643821E-15));
#131955=DIRECTION('',(0.458927806396619,0.264962092561704,0.848045021223113));
#131956=DIRECTION('center_axis',(-0.49999999999998,0.86602540378445,-3.36325426817014E-14));
#131957=DIRECTION('ref_axis',(0.757468756514423,0.437324790476329,0.484755722544178));
#131958=DIRECTION('',(0.866025403784435,0.500000000000007,3.61343235749219E-15));
#131959=DIRECTION('',(0.433017043030755,0.250002506357519,-0.866022509672733));
#131960=DIRECTION('center_axis',(0.499999180015738,-0.866025877200503,-1.63998885396272E-6));
#131961=DIRECTION('ref_axis',(0.750040644542557,0.433036167837314,-0.499918702269639));
#131962=DIRECTION('',(0.866025403784435,0.500000000000007,3.61343235749219E-15));
#131963=DIRECTION('center_axis',(0.500000820059927,-0.866024930320548,-1.64014403113693E-6));
#131964=DIRECTION('ref_axis',(0.75001548516595,0.433021642322233,0.499969028332597));
#131965=DIRECTION('',(0.433017178634557,0.250002584648415,0.86602241926897));
#131966=DIRECTION('',(0.866025403784435,0.500000000000007,3.61343235749219E-15));
#131967=DIRECTION('center_axis',(-0.500000000000007,0.866025403784435,5.97701461910993E-15));
#131968=DIRECTION('ref_axis',(2.6276792553892E-16,7.05337113113122E-15,
-1.));
#131969=DIRECTION('center_axis',(0.499999999999989,-0.866025403784445,4.74163716440701E-14));
#131970=DIRECTION('ref_axis',(0.757468756500261,0.437324790468171,0.484755722573669));
#131971=DIRECTION('',(-0.458927806396633,-0.264962092561691,-0.848045021223109));
#131972=DIRECTION('',(0.866025403784435,0.500000000000007,3.7542492643821E-15));
#131973=DIRECTION('',(-0.458928260426587,-0.264962354696025,0.848044693619248));
#131974=DIRECTION('center_axis',(0.499999999999975,-0.866025403784453,-5.47217885068692E-14));
#131975=DIRECTION('ref_axis',(0.757470380580527,0.437325728131337,-0.484752338888207));
#131976=DIRECTION('',(-0.866025403784435,-0.500000000000007,-3.61343235749219E-15));
#131977=DIRECTION('',(-0.433017178634597,-0.250002584648401,-0.866022419268954));
#131978=DIRECTION('center_axis',(-0.499999179825182,0.866025877310519,-1.64037034334471E-6));
#131979=DIRECTION('ref_axis',(0.75004073347165,0.433036219180271,0.499918524373088));
#131980=DIRECTION('',(-0.866025403784435,-0.500000000000007,-3.61343235749219E-15));
#131981=DIRECTION('center_axis',(-0.500000819876911,0.866024930426213,-1.63977768085434E-6));
#131982=DIRECTION('ref_axis',(0.750015393190062,0.433021589219632,-0.499969212299778));
#131983=DIRECTION('',(-0.433017043030724,-0.250002506357501,0.866022509672754));
#131984=DIRECTION('',(-0.866025403784435,-0.500000000000007,-3.61343235749219E-15));
#131985=DIRECTION('center_axis',(-2.54740177659162E-16,-7.0657327788296E-15,
1.));
#131986=DIRECTION('ref_axis',(-1.,1.7788411531011E-30,-2.54740177659162E-16));
#131987=DIRECTION('',(-0.809016994374943,-0.58778525229248,-4.35922265691196E-15));
#131988=DIRECTION('center_axis',(2.54740177659162E-16,7.0657327788296E-15,
-1.));
#131989=DIRECTION('ref_axis',(-1.,-1.29496413592278E-12,-2.54740177668312E-16));
#131990=DIRECTION('',(0.809016994374943,0.58778525229248,4.35922265691196E-15));
#131991=DIRECTION('center_axis',(-2.54740177659162E-16,-7.0657327788296E-15,
1.));
#131992=DIRECTION('ref_axis',(-1.,1.65352321226724E-30,-2.54740177659162E-16));
#131993=DIRECTION('center_axis',(-0.58778525229248,0.809016994374943,5.56656537619081E-15));
#131994=DIRECTION('ref_axis',(2.54740177659162E-16,7.0657327788296E-15,
-1.));
#131995=DIRECTION('center_axis',(-0.587785252292507,0.809016994374923,-8.68381026576039E-14));
#131996=DIRECTION('ref_axis',(0.707607892255758,0.514107226876036,-0.484752338922871));
#131997=DIRECTION('',(0.42871809563737,0.311481929006034,-0.848044693619238));
#131998=DIRECTION('',(-0.809016994374943,-0.58778525229248,-4.35922265691196E-15));
#131999=DIRECTION('',(0.42871767149512,0.31148162084863,0.848045021223115));
#132000=DIRECTION('center_axis',(-0.58778525229246,0.809016994374957,-2.37081858248059E-14));
#132001=DIRECTION('ref_axis',(0.707606375114078,0.514106124608088,0.484755722543188));
#132002=DIRECTION('',(0.809016994374943,0.58778525229248,4.21840575002205E-15));
#132003=DIRECTION('',(0.404512552559089,0.293895572546202,-0.86602250967274));
#132004=DIRECTION('center_axis',(0.587784486285637,-0.809017550909275,-1.63998885809377E-6));
#132005=DIRECTION('ref_axis',(0.700667238250818,0.509064546363247,-0.499918702268632));
#132006=DIRECTION('',(0.809016994374943,0.58778525229248,4.21840575002205E-15));
#132007=DIRECTION('center_axis',(0.587786018369622,-0.809016437785102,-1.64014417882589E-6));
#132008=DIRECTION('ref_axis',(0.700643735030366,0.509047470549938,0.499969028330164));
#132009=DIRECTION('',(0.404512679236484,0.293895664582674,0.866022419268941));
#132010=DIRECTION('',(0.809016994374943,0.58778525229248,4.21840575002205E-15));
#132011=DIRECTION('center_axis',(-0.58778525229248,0.809016994374943,5.56656537619081E-15));
#132012=DIRECTION('ref_axis',(2.54740177659162E-16,7.0657327788296E-15,
-1.));
#132013=DIRECTION('center_axis',(0.587785252292496,-0.809016994374931,3.85947211056421E-15));
#132014=DIRECTION('ref_axis',(0.707606375100321,0.514106124598129,0.484755722573831));
#132015=DIRECTION('',(-0.428717671495122,-0.311481620848618,-0.848045021223118));
#132016=DIRECTION('',(0.809016994374943,0.58778525229248,4.35922265691196E-15));
#132017=DIRECTION('',(-0.428718095637371,-0.311481929006031,0.848044693619239));
#132018=DIRECTION('center_axis',(0.587785252292485,-0.809016994374939,-2.16406065379816E-14));
#132019=DIRECTION('ref_axis',(0.707607892271911,0.514107226887808,-0.484752338886809));
#132020=DIRECTION('',(-0.809016994374942,-0.58778525229248,-4.21840575002204E-15));
#132021=DIRECTION('',(-0.404512679236477,-0.293895664582651,-0.866022419268952));
#132022=DIRECTION('center_axis',(-0.587784486107578,0.809017551038641,-1.64037040754943E-6));
#132023=DIRECTION('ref_axis',(0.7006673213238,0.509064606718979,0.499918524376705));
#132024=DIRECTION('',(-0.809016994374943,-0.58778525229248,-4.21840575002205E-15));
#132025=DIRECTION('center_axis',(-0.587786018198513,0.809016437909421,-1.63977749787816E-6));
#132026=DIRECTION('ref_axis',(0.700643649108078,0.50904740812344,-0.499969212299442));
#132027=DIRECTION('',(-0.404512552559112,-0.293895572546185,0.866022509672735));
#132028=DIRECTION('',(-0.809016994374943,-0.58778525229248,-4.21840575002205E-15));
#132029=DIRECTION('center_axis',(-2.45464262584879E-16,-7.07718757997909E-15,
1.));
#132030=DIRECTION('ref_axis',(-1.,1.71406778433599E-30,-2.45464262584879E-16));
#132031=DIRECTION('',(-0.743144825477389,-0.669130606358864,-4.91797831328641E-15));
#132032=DIRECTION('center_axis',(2.45464262584879E-16,7.07718757997909E-15,
-1.));
#132033=DIRECTION('ref_axis',(-1.,7.62234719786647E-12,-2.45464262530934E-16));
#132034=DIRECTION('',(0.743144825477389,0.669130606358864,4.91797831328641E-15));
#132035=DIRECTION('center_axis',(-2.45464262584879E-16,-7.07718757997909E-15,
1.));
#132036=DIRECTION('ref_axis',(-1.,1.691840019653E-30,-2.45464262584879E-16));
#132037=DIRECTION('center_axis',(-0.669130606358865,0.743144825477389,5.09512767813145E-15));
#132038=DIRECTION('ref_axis',(2.45464262584878E-16,7.07718757997909E-15,
-1.));
#132039=DIRECTION('center_axis',(-0.66913060635884,0.743144825477411,4.41082426197315E-14));
#132040=DIRECTION('ref_axis',(0.649992703804842,0.585256059269967,-0.484752338919845));
#132041=DIRECTION('',(0.393810805677312,0.35458884212006,-0.848044693619234));
#132042=DIRECTION('',(-0.743144825477389,-0.669130606358864,-4.91797831328641E-15));
#132043=DIRECTION('',(0.393810416069775,0.354588491315832,0.848045021223115));
#132044=DIRECTION('center_axis',(-0.669130606358884,0.743144825477371,3.99731040069399E-14));
#132045=DIRECTION('ref_axis',(0.649991310190922,0.585254804454373,0.484755722544212));
#132046=DIRECTION('',(0.743144825477389,0.669130606358864,4.7771614063965E-15));
#132047=DIRECTION('',(0.371576137911922,0.334568657340493,-0.866022509672722));
#132048=DIRECTION('center_axis',(0.669129902721978,-0.743145459032475,-1.63998882521664E-6));
#132049=DIRECTION('ref_axis',(0.643617175072631,0.579515507190644,-0.499918702267776));
#132050=DIRECTION('',(0.743144825477389,0.669130606358864,4.7771614063965E-15));
#132051=DIRECTION('center_axis',(0.669131310059903,-0.743144191859714,-1.64014420739982E-6));
#132052=DIRECTION('ref_axis',(0.643595585511274,0.579496068162662,0.499969028335171));
#132053=DIRECTION('',(0.371576254274849,0.334568762114141,0.866022419268973));
#132054=DIRECTION('',(0.743144825477389,0.669130606358864,4.7771614063965E-15));
#132055=DIRECTION('center_axis',(-0.669130606358865,0.743144825477389,5.09512767813145E-15));
#132056=DIRECTION('ref_axis',(2.45464262584878E-16,7.07718757997909E-15,
-1.));
#132057=DIRECTION('center_axis',(0.669130606358884,-0.743144825477371,-6.75407619348748E-14));
#132058=DIRECTION('ref_axis',(0.649991310179477,0.58525480444405,0.484755722572022));
#132059=DIRECTION('',(-0.393810416069763,-0.354588491315834,-0.848045021223119));
#132060=DIRECTION('',(0.743144825477389,0.669130606358864,4.91797831328641E-15));
#132061=DIRECTION('',(-0.39381080567731,-0.354588842120051,0.848044693619239));
#132062=DIRECTION('center_axis',(0.669130606358841,-0.74314482547741,-5.76163919291452E-14));
#132063=DIRECTION('ref_axis',(0.64999270381715,0.585256059281061,-0.484752338889947));
#132064=DIRECTION('',(-0.743144825477389,-0.669130606358864,-4.7771614063965E-15));
#132065=DIRECTION('',(-0.371576254274891,-0.334568762114186,-0.866022419268937));
#132066=DIRECTION('center_axis',(-0.669129902558376,0.743145459179781,-1.64037043577932E-6));
#132067=DIRECTION('ref_axis',(0.643617251383537,0.579515575900918,0.49991852437145));
#132068=DIRECTION('',(-0.743144825477389,-0.669130606358864,-4.7771614063965E-15));
#132069=DIRECTION('center_axis',(-0.669131309902728,0.743144192001237,-1.63977757912426E-6));
#132070=DIRECTION('ref_axis',(0.643595506588524,0.579495997099938,-0.499969212296327));
#132071=DIRECTION('',(-0.371576137911874,-0.334568657340446,0.866022509672761));
#132072=DIRECTION('',(-0.743144825477389,-0.669130606358864,-4.7771614063965E-15));
#132073=DIRECTION('center_axis',(-2.35041809182734E-16,-7.08761003338124E-15,
1.));
#132074=DIRECTION('ref_axis',(-1.,1.64128818121889E-30,-2.35041809182734E-16));
#132075=DIRECTION('',(-0.669130606358852,-0.7431448254774,-5.42439438960709E-15));
#132076=DIRECTION('center_axis',(2.35041809182734E-16,7.08761003338124E-15,
-1.));
#132077=DIRECTION('ref_axis',(-1.,-3.73923114693753E-12,-2.35041809209237E-16));
#132078=DIRECTION('',(0.669130606358852,0.7431448254774,5.42439438960709E-15));
#132079=DIRECTION('center_axis',(-2.35041809182734E-16,-7.08761003338124E-15,
1.));
#132080=DIRECTION('ref_axis',(-1.,1.67007359059941E-30,-2.35041809182734E-16));
#132081=DIRECTION('center_axis',(-0.7431448254774,0.669130606358852,4.56786669500647E-15));
#132082=DIRECTION('ref_axis',(2.35041809182734E-16,7.08761003338124E-15,
-1.));
#132083=DIRECTION('center_axis',(-0.743144825477404,0.669130606358847,-1.40595023350398E-14));
#132084=DIRECTION('ref_axis',(0.585256059268642,0.649992703803378,-0.484752338923407));
#132085=DIRECTION('',(0.354588842120041,0.393810805677326,-0.848044693619236));
#132086=DIRECTION('',(-0.669130606358852,-0.7431448254774,-5.42439438960709E-15));
#132087=DIRECTION('',(0.354588491315847,0.393810416069763,0.848045021223114));
#132088=DIRECTION('center_axis',(-0.743144825477429,0.66913060635882,8.60110927597638E-14));
#132089=DIRECTION('ref_axis',(0.585254804454311,0.649991310190875,0.484755722544352));
#132090=DIRECTION('',(0.669130606358852,0.7431448254774,5.28357748271718E-15));
#132091=DIRECTION('',(0.334568657340462,0.371576137911927,-0.866022509672732));
#132092=DIRECTION('center_axis',(0.743144191919631,-0.669131309993359,-1.63998881333916E-6));
#132093=DIRECTION('ref_axis',(0.579515507437722,0.643617174848766,-0.499918702269571));
#132094=DIRECTION('',(0.669130606358852,0.7431448254774,5.28357748271718E-15));
#132095=DIRECTION('center_axis',(0.743145459092284,-0.669129902655552,-1.64014391615252E-6));
#132096=DIRECTION('ref_axis',(0.579496068081958,0.643595585590597,0.499969028326603));
#132097=DIRECTION('',(0.334568762114155,0.371576254274896,0.866022419268947));
#132098=DIRECTION('',(0.669130606358852,0.7431448254774,5.28357748271718E-15));
#132099=DIRECTION('center_axis',(-0.7431448254774,0.669130606358852,4.56786669500647E-15));
#132100=DIRECTION('ref_axis',(2.35041809182734E-16,7.08761003338124E-15,
-1.));
#132101=DIRECTION('center_axis',(0.743144825477371,-0.669130606358884,6.75407619348659E-14));
#132102=DIRECTION('ref_axis',(0.585254804443047,0.649991310178362,0.484755722574728));
#132103=DIRECTION('',(-0.354588491315845,-0.393810416069762,-0.848045021223115));
#132104=DIRECTION('',(0.669130606358852,0.7431448254774,5.42439438960709E-15));
#132105=DIRECTION('',(-0.35458884212002,-0.393810805677306,0.848044693619254));
#132106=DIRECTION('center_axis',(0.743144825477417,-0.669130606358833,-2.48108864766668E-15));
#132107=DIRECTION('ref_axis',(0.585256059282077,0.649992703818338,-0.484752338887127));
#132108=DIRECTION('',(-0.669130606358852,-0.7431448254774,-5.28357748271718E-15));
#132109=DIRECTION('',(-0.334568762114151,-0.371576254274926,-0.866022419268936));
#132110=DIRECTION('center_axis',(-0.743144191772371,0.669131310156907,-1.64037037088548E-6));
#132111=DIRECTION('ref_axis',(0.579515576147878,0.643617251158763,0.499918524374553));
#132112=DIRECTION('',(-0.669130606358852,-0.7431448254774,-5.28357748271718E-15));
#132113=DIRECTION('center_axis',(-0.743145458950891,0.669129902812586,-1.63977760425555E-6));
#132114=DIRECTION('ref_axis',(0.579495997016653,0.643595506664192,-0.499969212295455));
#132115=DIRECTION('',(-0.334568657340465,-0.371576137911891,0.866022509672746));
#132116=DIRECTION('',(-0.669130606358852,-0.7431448254774,-5.28357748271718E-15));
#132117=DIRECTION('center_axis',(-2.23587008033241E-16,-7.09688594845552E-15,
1.));
#132118=DIRECTION('ref_axis',(-1.,1.56129973231166E-30,-2.23587008033241E-16));
#132119=DIRECTION('',(-0.587785252292466,-0.809016994374953,-5.87292248536745E-15));
#132120=DIRECTION('center_axis',(2.23587008033241E-16,7.09688594845552E-15,
-1.));
#132121=DIRECTION('ref_axis',(-1.,-1.22390986234677E-12,-2.23587008041927E-16));
#132122=DIRECTION('',(0.587785252292466,0.809016994374953,5.87292248536745E-15));
#132123=DIRECTION('center_axis',(-2.23587008033241E-16,-7.09688594845552E-15,
1.));
#132124=DIRECTION('ref_axis',(-1.,1.69306078464668E-30,-2.23587008033241E-16));
#132125=DIRECTION('center_axis',(-0.809016994374953,0.587785252292466,3.99055920848344E-15));
#132126=DIRECTION('ref_axis',(2.23587008033241E-16,7.09688594845552E-15,
-1.));
#132127=DIRECTION('center_axis',(-0.809016994374927,0.587785252292501,5.81677449547707E-14));
#132128=DIRECTION('ref_axis',(0.514107226876486,0.707607892256365,-0.484752338921509));
#132129=DIRECTION('',(0.311481929006018,0.428718095637389,-0.848044693619234));
#132130=DIRECTION('',(-0.587785252292466,-0.809016994374953,-5.87292248536745E-15));
#132131=DIRECTION('',(0.31148162084863,0.42871767149512,0.848045021223114));
#132132=DIRECTION('center_axis',(-0.809016994374974,0.587785252292436,5.48596392922833E-14));
#132133=DIRECTION('ref_axis',(0.514106124607928,0.707606375113875,0.484755722543654));
#132134=DIRECTION('',(0.587785252292466,0.809016994374953,5.73210557847754E-15));
#132135=DIRECTION('',(0.29389557254618,0.404512552559094,-0.866022509672745));
#132136=DIRECTION('center_axis',(0.809016437837696,-0.587786018297234,-1.63998882728232E-6));
#132137=DIRECTION('ref_axis',(0.509064546633409,0.700667238055409,-0.499918702267405));
#132138=DIRECTION('',(0.587785252292466,0.809016994374953,5.73210557847754E-15));
#132139=DIRECTION('center_axis',(0.809017550961834,-0.587784486213294,-1.64014398879267E-6));
#132140=DIRECTION('ref_axis',(0.509047470456847,0.700643735094558,0.499969028334988));
#132141=DIRECTION('',(0.293895664582671,0.404512679236444,0.866022419268961));
#132142=DIRECTION('',(0.587785252292466,0.809016994374953,5.73210557847754E-15));
#132143=DIRECTION('center_axis',(-0.809016994374953,0.587785252292466,3.99055920848344E-15));
#132144=DIRECTION('ref_axis',(2.23587008033241E-16,7.09688594845552E-15,
-1.));
#132145=DIRECTION('center_axis',(0.809016994374949,-0.587785252292471,-6.67137321968949E-14));
#132146=DIRECTION('ref_axis',(0.514106124598043,0.707606375100197,0.484755722574104));
#132147=DIRECTION('',(-0.311481620848613,-0.428717671495125,-0.848045021223118));
#132148=DIRECTION('',(0.587785252292466,0.809016994374953,5.87292248536745E-15));
#132149=DIRECTION('',(-0.311481929006028,-0.428718095637371,0.84804469361924));
#132150=DIRECTION('center_axis',(0.809016994374952,-0.587785252292467,-5.23785381174101E-15));
#132151=DIRECTION('ref_axis',(0.514107226887492,0.707607892271531,-0.484752338887699));
#132152=DIRECTION('',(-0.587785252292466,-0.809016994374953,-5.73210557847754E-15));
#132153=DIRECTION('',(-0.293895664582653,-0.404512679236455,-0.866022419268962));
#132154=DIRECTION('center_axis',(-0.809016437708337,0.58778601847528,-1.6403704173616E-6));
#132155=DIRECTION('ref_axis',(0.509064606990258,0.700667321129096,0.499918524373354));
#132156=DIRECTION('',(-0.587785252292466,-0.809016994374953,-5.73210557847754E-15));
#132157=DIRECTION('center_axis',(-0.809017550837597,0.587784486384294,-1.63977757327168E-6));
#132158=DIRECTION('ref_axis',(0.50904740803245,0.700643649174308,-0.49996921229927));
#132159=DIRECTION('',(-0.293895572546189,-0.404512552559082,0.866022509672747));
#132160=DIRECTION('',(-0.587785252292466,-0.809016994374953,-5.73210557847754E-15));
#132161=DIRECTION('center_axis',(-2.11225360334865E-16,-7.10491369633528E-15,
1.));
#132162=DIRECTION('ref_axis',(-1.,1.47497880779919E-30,-2.11225360334865E-16));
#132163=DIRECTION('',(-0.499999999999992,-0.866025403784443,-6.25864843288981E-15));
#132164=DIRECTION('center_axis',(2.11225360334865E-16,7.10491369633528E-15,
-1.));
#132165=DIRECTION('ref_axis',(-1.,-2.39808173319034E-12,-2.11225360351903E-16));
#132166=DIRECTION('',(0.499999999999992,0.866025403784443,6.25864843288981E-15));
#132167=DIRECTION('center_axis',(-2.11225360334865E-16,-7.10491369633528E-15,
1.));
#132168=DIRECTION('ref_axis',(-1.,1.65745742556672E-30,-2.11225360334865E-16));
#132169=DIRECTION('center_axis',(-0.866025403784443,0.499999999999992,3.36953032019407E-15));
#132170=DIRECTION('ref_axis',(2.11225360334864E-16,7.10491369633528E-15,
-1.));
#132171=DIRECTION('center_axis',(-0.866025403784449,0.499999999999982,-2.67406220882125E-14));
#132172=DIRECTION('ref_axis',(0.437325728122339,0.757470380564956,-0.484752338920655));
#132173=DIRECTION('',(0.264962354696012,0.458928260426602,-0.848044693619244));
#132174=DIRECTION('',(-0.499999999999992,-0.866025403784443,-6.25864843288981E-15));
#132175=DIRECTION('',(0.264962092561693,0.458927806396623,0.848045021223114));
#132176=DIRECTION('center_axis',(-0.866025403784433,0.500000000000009,-2.35703475351279E-14));
#132177=DIRECTION('ref_axis',(0.437324790476303,0.757468756514376,0.484755722544276));
#132178=DIRECTION('',(0.499999999999992,0.866025403784443,6.1178315259999E-15));
#132179=DIRECTION('',(0.250002506357492,0.433017043030775,-0.866022509672731));
#132180=DIRECTION('center_axis',(0.866024930365251,-0.500000819982501,-1.6399888658402E-6));
#132181=DIRECTION('ref_axis',(0.433036168125916,0.750040644375568,-0.499918702270186));
#132182=DIRECTION('',(0.499999999999992,0.866025403784443,6.1178315259999E-15));
#132183=DIRECTION('center_axis',(0.866025877245173,-0.499999179938366,-1.64014390875047E-6));
#132184=DIRECTION('ref_axis',(0.433021642224328,0.750015485222473,0.499969028332601));
#132185=DIRECTION('',(0.250002584648419,0.433017178634634,0.866022419268931));
#132186=DIRECTION('',(0.499999999999992,0.866025403784443,6.1178315259999E-15));
#132187=DIRECTION('center_axis',(-0.866025403784443,0.499999999999992,3.36953032019407E-15));
#132188=DIRECTION('ref_axis',(2.11225360334864E-16,7.10491369633528E-15,
-1.));
#132189=DIRECTION('center_axis',(0.866025403784431,-0.500000000000014,5.26542266512672E-14));
#132190=DIRECTION('ref_axis',(0.437324790467692,0.757468756499479,0.484755722575321));
#132191=DIRECTION('',(-0.264962092561685,-0.458927806396634,-0.848045021223111));
#132192=DIRECTION('',(0.499999999999992,0.866025403784443,6.25864843288981E-15));
#132193=DIRECTION('',(-0.264962354696017,-0.458928260426612,0.848044693619237));
#132194=DIRECTION('center_axis',(0.866025403784443,-0.499999999999993,-1.46108553695935E-14));
#132195=DIRECTION('ref_axis',(0.437325728131572,0.757470380580965,-0.484752338887311));
#132196=DIRECTION('',(-0.499999999999992,-0.866025403784443,-6.1178315259999E-15));
#132197=DIRECTION('',(-0.250002584648408,-0.43301717863458,-0.866022419268961));
#132198=DIRECTION('center_axis',(-0.866024930255216,0.500000820173085,-1.6403704313039E-6));
#132199=DIRECTION('ref_axis',(0.433036219468537,0.75004073330313,0.499918524376223));
#132200=DIRECTION('',(-0.499999999999992,-0.866025403784443,-6.1178315259999E-15));
#132201=DIRECTION('center_axis',(-0.86602587713954,0.499999180121329,-1.63977762973091E-6));
#132202=DIRECTION('ref_axis',(0.433021589123383,0.75001539324846,-0.499969212295536));
#132203=DIRECTION('',(-0.25000250635749,-0.433017043030736,0.866022509672752));
#132204=DIRECTION('',(-0.499999999999992,-0.866025403784443,-6.1178315259999E-15));
#132205=DIRECTION('center_axis',(-1.98092302886629E-16,-7.11160532333482E-15,
1.));
#132206=DIRECTION('ref_axis',(-1.,1.38327115779425E-30,-1.98092302886629E-16));
#132207=DIRECTION('',(-0.406736643075792,-0.913545457642605,-6.57734613797476E-15));
#132208=DIRECTION('center_axis',(1.98092302886629E-16,7.11160532333483E-15,
-1.));
#132209=DIRECTION('ref_axis',(-1.,7.04858393874019E-12,-1.98092302836502E-16));
#132210=DIRECTION('',(0.406736643075792,0.913545457642605,6.57734613797476E-15));
#132211=DIRECTION('center_axis',(-1.98092302886629E-16,-7.11160532333483E-15,
1.));
#132212=DIRECTION('ref_axis',(-1.,1.25091873609706E-30,-1.98092302886629E-16));
#132213=DIRECTION('center_axis',(-0.913545457642605,0.406736643075792,2.7115841525971E-15));
#132214=DIRECTION('ref_axis',(1.98092302886629E-16,7.11160532333483E-15,
-1.));
#132215=DIRECTION('center_axis',(-0.913545457642619,0.40673664307576,-5.01731259799456E-14));
#132216=DIRECTION('ref_axis',(0.355752797174364,0.799033864872945,-0.484752338920422));
#132217=DIRECTION('',(0.215539797381043,0.484110311157684,-0.848044693619239));
#132218=DIRECTION('',(-0.406736643075792,-0.913545457642605,-6.57734613797476E-15));
#132219=DIRECTION('',(0.215539584141762,0.484109832214418,0.848045021223121));
#132220=DIRECTION('center_axis',(-0.91354545764262,0.406736643075758,4.31433846695598E-14));
#132221=DIRECTION('ref_axis',(0.3557520344243,0.799032151708265,0.484755722544285));
#132222=DIRECTION('',(0.406736643075792,0.913545457642605,6.43652923108485E-15));
#132223=DIRECTION('',(0.203370360392767,0.456777308164318,-0.866022509672743));
#132224=DIRECTION('center_axis',(0.913545072528379,-0.406737508052096,-1.63998882728247E-6));
#132225=DIRECTION('ref_axis',(0.352263354743371,0.791196448442592,-0.499918702267453));
#132226=DIRECTION('',(0.406736643075792,0.913545457642605,6.43652923108485E-15));
#132227=DIRECTION('center_axis',(0.913545842789922,-0.406735778016344,-1.64014405075982E-6));
#132228=DIRECTION('ref_axis',(0.352251538263023,0.791169908742036,0.499969028333208));
#132229=DIRECTION('',(0.203370424080327,0.456777451208974,0.866022419268936));
#132230=DIRECTION('',(0.406736643075792,0.913545457642605,6.43652923108485E-15));
#132231=DIRECTION('center_axis',(-0.913545457642605,0.406736643075792,2.7115841525971E-15));
#132232=DIRECTION('ref_axis',(1.98092302886629E-16,7.11160532333483E-15,
-1.));
#132233=DIRECTION('center_axis',(0.91354545764259,-0.406736643075824,5.29299032305874E-14));
#132234=DIRECTION('ref_axis',(0.35575203441772,0.799032151693445,0.484755722573542));
#132235=DIRECTION('',(-0.215539584141762,-0.484109832214432,-0.848045021223113));
#132236=DIRECTION('',(0.406736643075792,0.913545457642605,6.57734613797476E-15));
#132237=DIRECTION('',(-0.215539797381046,-0.484110311157701,0.848044693619229));
#132238=DIRECTION('center_axis',(0.913545457642612,-0.406736643075775,7.99461897581586E-15));
#132239=DIRECTION('ref_axis',(0.355752797181782,0.799033864889621,-0.484752338887492));
#132240=DIRECTION('',(-0.406736643075792,-0.913545457642605,-6.43652923108485E-15));
#132241=DIRECTION('',(-0.203370424080328,-0.456777451208907,-0.866022419268971));
#132242=DIRECTION('center_axis',(-0.913545072438836,0.406737508253211,-1.64037047915676E-6));
#132243=DIRECTION('ref_axis',(0.352263396508425,0.791196542247804,0.49991852437719));
#132244=DIRECTION('',(-0.406736643075792,-0.913545457642605,-6.43652923108485E-15));
#132245=DIRECTION('center_axis',(-0.913545842703917,0.406735778209517,-1.63977747463982E-6));
#132246=DIRECTION('ref_axis',(0.352251495066873,0.791169811721274,-0.499969212296194));
#132247=DIRECTION('',(-0.203370360392765,-0.456777308164279,0.866022509672763));
#132248=DIRECTION('',(-0.406736643075792,-0.913545457642605,-6.43652923108485E-15));
#132249=DIRECTION('center_axis',(-1.84331724214206E-16,-7.11688751458844E-15,
1.));
#132250=DIRECTION('ref_axis',(-1.,1.28718155050136E-30,-1.84331724214206E-16));
#132251=DIRECTION('',(-0.309016994374938,-0.951056516295157,-6.82552388187361E-15));
#132252=DIRECTION('center_axis',(1.84331724214206E-16,7.11688751458844E-15,
-1.));
#132253=DIRECTION('ref_axis',(-1.,9.20508114177209E-12,-1.84331724148695E-16));
#132254=DIRECTION('',(0.309016994374938,0.951056516295157,6.82552388187361E-15));
#132255=DIRECTION('center_axis',(-1.84331724214206E-16,-7.11688751458844E-15,
1.));
#132256=DIRECTION('ref_axis',(-1.,1.25755986889655E-30,-1.84331724214206E-16));
#132257=DIRECTION('center_axis',(-0.951056516295157,0.309016994374938,2.0239293015888E-15));
#132258=DIRECTION('ref_axis',(1.84331724214206E-16,7.11688751458845E-15,
-1.));
#132259=DIRECTION('center_axis',(-0.951056516295153,0.309016994374948,8.13245723301314E-15));
#132260=DIRECTION('ref_axis',(0.270282164133991,0.831842966947295,-0.484752338923049));
#132261=DIRECTION('',(0.163755740941343,0.503988348013141,-0.848044693619232));
#132262=DIRECTION('',(-0.309016994374938,-0.951056516295157,-6.82552388187361E-15));
#132263=DIRECTION('',(0.163755578933418,0.503987849403977,0.848045021223128));
#132264=DIRECTION('center_axis',(-0.951056516295156,0.309016994374941,-7.16759106331355E-15));
#132265=DIRECTION('ref_axis',(0.27028158463749,0.831841183440473,0.484755722543016));
#132266=DIRECTION('',(0.309016994374938,0.951056516295157,6.68470697498369E-15));
#132267=DIRECTION('',(0.154510046201588,0.475533025522851,-0.866022509672738));
#132268=DIRECTION('center_axis',(0.95105622370527,-0.309017894868213,-1.63998879715887E-6));
#132269=DIRECTION('ref_axis',(0.267631070329315,0.82368373864957,-0.499918702269331));
#132270=DIRECTION('',(0.309016994374938,0.951056516295157,6.68470697498369E-15));
#132271=DIRECTION('center_axis',(0.951056808909267,-0.309016093795505,-1.6401440671127E-6));
#132272=DIRECTION('ref_axis',(0.26762209273496,0.823656109177694,0.499969028335178));
#132273=DIRECTION('',(0.154510094588028,0.475533174441037,0.86602241926894));
#132274=DIRECTION('',(0.309016994374938,0.951056516295157,6.68470697498369E-15));
#132275=DIRECTION('center_axis',(-0.951056516295157,0.309016994374938,2.0239293015888E-15));
#132276=DIRECTION('ref_axis',(1.84331724214206E-16,7.11688751458845E-15,
-1.));
#132277=DIRECTION('center_axis',(0.951056516295164,-0.309016994374915,-2.46730538496772E-14));
#132278=DIRECTION('ref_axis',(0.270281584632031,0.831841183423701,0.484755722574839));
#132279=DIRECTION('',(-0.163755578933423,-0.503987849403986,-0.848045021223121));
#132280=DIRECTION('',(0.309016994374938,0.951056516295157,6.82552388187361E-15));
#132281=DIRECTION('',(-0.163755740941338,-0.503988348013147,0.84804469361923));
#132282=DIRECTION('center_axis',(0.951056516295147,-0.309016994374969,-4.41082426251915E-14));
#132283=DIRECTION('ref_axis',(0.270282164139995,0.831842966965768,-0.484752338888003));
#132284=DIRECTION('',(-0.309016994374938,-0.951056516295157,-6.68470697498369E-15));
#132285=DIRECTION('',(-0.154510094588046,-0.475533174441003,-0.866022419268957));
#132286=DIRECTION('center_axis',(-0.951056223637252,0.309017895077548,-1.64037042622575E-6));
#132287=DIRECTION('ref_axis',(0.267631102060857,0.823683836308454,0.499918524375601));
#132288=DIRECTION('',(-0.309016994374938,-0.951056516295157,-6.68470697498369E-15));
#132289=DIRECTION('center_axis',(-0.951056808843968,0.309016093996475,-1.63977771355912E-6));
#132290=DIRECTION('ref_axis',(0.267622059916434,0.823656008171873,-0.499969212300578));
#132291=DIRECTION('',(-0.154510046201585,-0.475533025522849,0.866022509672739));
#132292=DIRECTION('',(-0.309016994374938,-0.951056516295157,-6.68470697498369E-15));
#132293=DIRECTION('center_axis',(-1.70094388097117E-16,-7.12070239730339E-15,
1.));
#132294=DIRECTION('ref_axis',(-1.,1.18776276376605E-30,-1.70094388097117E-16));
#132295=DIRECTION('',(-0.207911690817749,-0.978147600733808,-7.00046257728966E-15));
#132296=DIRECTION('center_axis',(1.70094388097117E-16,7.12070239730339E-15,
-1.));
#132297=DIRECTION('ref_axis',(-1.,6.75992595233765E-12,-1.70094388048982E-16));
#132298=DIRECTION('',(0.207911690817749,0.978147600733808,7.00046257728966E-15));
#132299=DIRECTION('center_axis',(-1.70094388097117E-16,-7.12070239730339E-15,
1.));
#132300=DIRECTION('ref_axis',(-1.,1.26081367981038E-30,-1.70094388097117E-16));
#132301=DIRECTION('center_axis',(-0.978147600733808,0.207911690817749,1.31409985761787E-15));
#132302=DIRECTION('ref_axis',(1.70094388097117E-16,7.12070239730339E-15,
-1.));
#132303=DIRECTION('center_axis',(-0.97814760073381,0.20791169081774,-1.98487091788782E-14));
#132304=DIRECTION('ref_axis',(0.181850263143551,0.855538223401766,-0.484752338924911));
#132305=DIRECTION('',(0.110177542335804,0.518344583061406,-0.848044693619233));
#132306=DIRECTION('',(-0.207911690817749,-0.978147600733808,-7.00046257728966E-15));
#132307=DIRECTION('',(0.110177433334219,0.518344070249258,0.848045021223117));
#132308=DIRECTION('center_axis',(-0.97814760073381,0.20791169081774,1.2750041795317E-14));
#132309=DIRECTION('ref_axis',(0.181849873248917,0.85553638909175,0.484755722544049));
#132310=DIRECTION('',(0.207911690817749,0.978147600733808,6.85964567039975E-15));
#132311=DIRECTION('',(0.10395688761095,0.489078703542044,-0.866022509672744));
#132312=DIRECTION('center_axis',(0.978147403873936,-0.207912616962005,-1.63998886076217E-6));
#132313=DIRECTION('ref_axis',(0.180066563904181,0.84714657745213,-0.499918702265563));
#132314=DIRECTION('',(0.207911690817749,0.978147600733808,6.85964567039975E-15));
#132315=DIRECTION('center_axis',(0.978147797608756,-0.207910764585316,-1.64014401168594E-6));
#132316=DIRECTION('ref_axis',(0.180060523556231,0.847118160922957,0.499969028331919));
#132317=DIRECTION('',(0.103956920166113,0.48907885670218,0.866022419268962));
#132318=DIRECTION('',(0.207911690817749,0.978147600733808,6.85964567039975E-15));
#132319=DIRECTION('center_axis',(-0.978147600733808,0.207911690817749,1.31409985761787E-15));
#132320=DIRECTION('ref_axis',(1.70094388097117E-16,7.12070239730339E-15,
-1.));
#132321=DIRECTION('center_axis',(0.97814760073381,-0.207911690817738,-2.52244070083276E-14));
#132322=DIRECTION('ref_axis',(0.181849873245408,0.855536389075222,0.484755722574534));
#132323=DIRECTION('',(-0.110177433334222,-0.518344070249258,-0.848045021223116));
#132324=DIRECTION('',(0.207911690817749,0.978147600733808,7.00046257728966E-15));
#132325=DIRECTION('',(-0.1101775423358,-0.518344583061378,0.848044693619251));
#132326=DIRECTION('center_axis',(0.978147600733805,-0.207911690817764,-2.43284525729549E-14));
#132327=DIRECTION('ref_axis',(0.181850263147838,0.855538223421937,-0.484752338887703));
#132328=DIRECTION('',(-0.207911690817749,-0.978147600733808,-6.85964567039975E-15));
#132329=DIRECTION('',(-0.103956920166104,-0.489078856702181,-0.866022419268962));
#132330=DIRECTION('center_axis',(-0.978147403828179,0.207912617177273,-1.64037039661903E-6));
#132331=DIRECTION('ref_axis',(0.18006658525306,0.847146677889481,0.499918524377841));
#132332=DIRECTION('',(-0.207911690817749,-0.978147600733808,-6.85964567039975E-15));
#132333=DIRECTION('center_axis',(-0.978147797564812,0.207910764792059,-1.63977758902207E-6));
#132334=DIRECTION('ref_axis',(0.180060501475228,0.8471180570388,-0.499969212299415));
#132335=DIRECTION('',(-0.10395688761091,-0.489078703542053,0.866022509672744));
#132336=DIRECTION('',(-0.207911690817749,-0.978147600733808,-6.85964567039975E-15));
#132337=DIRECTION('center_axis',(-1.55536281769216E-16,-7.12300817482632E-15,
1.));
#132338=DIRECTION('ref_axis',(-1.,1.08610405062053E-30,-1.55536281769216E-16));
#132339=DIRECTION('',(-0.104528463267644,-0.994521895368274,-7.10024555926768E-15));
#132340=DIRECTION('center_axis',(1.55536281769216E-16,7.12300817482632E-15,
-1.));
#132341=DIRECTION('ref_axis',(-1.,-2.20623519453511E-12,-1.55536281784931E-16));
#132342=DIRECTION('',(0.104528463267644,0.994521895368274,7.10024555926768E-15));
#132343=DIRECTION('center_axis',(-1.55536281769216E-16,-7.12300817482632E-15,
1.));
#132344=DIRECTION('ref_axis',(-1.,1.26178375522162E-30,-1.55536281769216E-16));
#132345=DIRECTION('center_axis',(-0.994521895368274,0.104528463267644,5.89872860613804E-16));
#132346=DIRECTION('ref_axis',(1.55536281769216E-16,7.12300817482632E-15,
-1.));
#132347=DIRECTION('center_axis',(-0.994521895368273,0.104528463267655,1.83324883388259E-14));
#132348=DIRECTION('ref_axis',(0.0914259726159976,0.869860024050451,-0.484752338921813));
#132349=DIRECTION('',(0.0553922155203034,0.527021726387077,-0.848044693619232));
#132350=DIRECTION('',(-0.104528463267644,-0.994521895368274,-7.10024555926768E-15));
#132351=DIRECTION('',(0.0553921607193071,0.527021204990385,0.848045021223124));
#132352=DIRECTION('center_axis',(-0.994521895368275,0.10452846326764,2.8946040832611E-15));
#132353=DIRECTION('ref_axis',(0.0914257765947068,0.869858159032472,0.484755722543523));
#132354=DIRECTION('',(0.104528463267644,0.994521895368274,6.95942865237777E-15));
#132355=DIRECTION('',(0.0522647556052267,0.49726593293896,-0.86602250967274));
#132356=DIRECTION('center_axis',(0.994521796395256,-0.104529404915857,-1.63998886493578E-6));
#132357=DIRECTION('ref_axis',(0.0905292105226818,0.861327901070913,-0.499918702269594));
#132358=DIRECTION('',(0.104528463267644,0.994521895368274,6.95942865237777E-15));
#132359=DIRECTION('center_axis',(0.994521994347069,-0.104527521530166,-1.64014403561263E-6));
#132360=DIRECTION('ref_axis',(0.090526173600551,0.861299008822545,0.499969028335301));
#132361=DIRECTION('',(0.0522647719724817,0.497266088663029,0.866022419268946));
#132362=DIRECTION('',(0.104528463267644,0.994521895368274,6.95942865237777E-15));
#132363=DIRECTION('center_axis',(-0.994521895368274,0.104528463267644,5.89872860613804E-16));
#132364=DIRECTION('ref_axis',(1.55536281769216E-16,7.12300817482632E-15,
-1.));
#132365=DIRECTION('center_axis',(0.994521895368274,-0.104528463267644,4.4108252692159E-15));
#132366=DIRECTION('ref_axis',(0.0914257765929011,0.869858159015296,0.484755722574685));
#132367=DIRECTION('',(-0.0553921607193093,-0.527021204990427,-0.848045021223098));
#132368=DIRECTION('',(0.104528463267644,0.994521895368274,7.10024555926768E-15));
#132369=DIRECTION('',(-0.0553922155203026,-0.527021726387058,0.848044693619244));
#132370=DIRECTION('center_axis',(0.994521895368274,-0.104528463267646,-1.82635692119912E-15));
#132371=DIRECTION('ref_axis',(0.0914259726179519,0.869860024069042,-0.484752338888083));
#132372=DIRECTION('',(-0.104528463267644,-0.994521895368274,-6.95942865237777E-15));
#132373=DIRECTION('',(-0.0522647719724786,-0.497266088663041,-0.866022419268939));
#132374=DIRECTION('center_axis',(-0.994521796372249,0.104529405134747,-1.64037045376714E-6));
#132375=DIRECTION('ref_axis',(0.0905292212561143,0.861328003190363,0.499918524380586));
#132376=DIRECTION('',(-0.104528463267644,-0.994521895368274,-6.95942865237777E-15));
#132377=DIRECTION('center_axis',(-0.994521994324977,0.104527521740361,-1.63977759371224E-6));
#132378=DIRECTION('ref_axis',(0.0905261624995749,0.861298903201578,-0.499969212298977));
#132379=DIRECTION('',(-0.0522647556052255,-0.497265932938949,0.866022509672747));
#132380=DIRECTION('',(-0.104528463267644,-0.994521895368274,-6.95942865237777E-15));
#132381=DIRECTION('center_axis',(-1.40816906889909E-16,-7.12377958457618E-15,
1.));
#132382=DIRECTION('ref_axis',(0.,-1.,-7.12377958457618E-15));
#132383=DIRECTION('',(1.04744440165294E-14,-1.,-7.12377958457618E-15));
#132384=DIRECTION('',(-1.04744440165294E-14,1.,7.12377958457618E-15));
#132385=DIRECTION('center_axis',(-1.,-1.04744440165294E-14,-1.40816906889984E-16));
#132386=DIRECTION('ref_axis',(1.40816906889909E-16,7.12377958457618E-15,
-1.));
#132387=DIRECTION('center_axis',(-1.,-1.0218985244156E-14,3.06110401690858E-16));
#132388=DIRECTION('ref_axis',(-9.08643805831693E-15,0.874651456243168,-0.484752338923399));
#132389=DIRECTION('',(-5.41813057753238E-15,0.529924709392063,-0.848044693619232));
#132390=DIRECTION('',(1.04744440165294E-14,-1.,-7.12377958457618E-15));
#132391=DIRECTION('',(-5.6761389882299E-15,0.529924185123394,0.848045021223111));
#132392=DIRECTION('center_axis',(-1.,-1.05374547025195E-14,-1.67445974214903E-16));
#132393=DIRECTION('ref_axis',(-9.29775073408689E-15,0.874649580952949,0.484755722543665));
#132394=DIRECTION('',(-1.04744440165294E-14,1.,6.98296267768627E-15));
#132395=DIRECTION('',(-5.23017107763447E-15,0.500005012715,-0.866022509672741));
#132396=DIRECTION('center_axis',(0.999999999998207,-9.46835243406286E-7,
-1.63998885178633E-6));
#132397=DIRECTION('ref_axis',(1.66712506289619E-10,0.866072335963012,-0.499918702270251));
#132398=DIRECTION('',(-1.04744440165294E-14,1.,6.98296267768627E-15));
#132399=DIRECTION('center_axis',(0.999999999998207,9.46924664504057E-7,
-1.64014405074161E-6));
#132400=DIRECTION('ref_axis',(-5.65192826653378E-11,0.866043284544485,0.499969028336156));
#132401=DIRECTION('',(-5.36780659828028E-15,0.500005169296827,0.866022419268954));
#132402=DIRECTION('',(-1.04744440165294E-14,1.,6.98296267768627E-15));
#132403=DIRECTION('center_axis',(-1.,-1.04744440165294E-14,-1.40816906889984E-16));
#132404=DIRECTION('ref_axis',(1.40816906889909E-16,7.12377958457618E-15,
-1.));
#132405=DIRECTION('center_axis',(1.,1.03422010861309E-14,3.74411322160068E-16));
#132406=DIRECTION('ref_axis',(-9.22729987695407E-15,0.874649580936016,0.484755722574217));
#132407=DIRECTION('',(5.62453772470054E-15,-0.529924185123408,-0.848045021223102));
#132408=DIRECTION('',(-1.04744440165294E-14,1.,7.12377958457618E-15));
#132409=DIRECTION('',(5.41813057753242E-15,-0.529924709392054,0.848044693619238));
#132410=DIRECTION('center_axis',(1.,1.04142386870038E-14,-9.91450061389633E-17));
#132411=DIRECTION('ref_axis',(-9.15688980707246E-15,0.874651456262926,-0.484752338887749));
#132412=DIRECTION('',(1.04744440165294E-14,-1.,-6.98296267768627E-15));
#132413=DIRECTION('',(5.50544266490299E-15,-0.50000516929684,-0.866022419268946));
#132414=DIRECTION('center_axis',(-0.999999999998206,9.47055339204534E-7,
-1.64037042584766E-6));
#132415=DIRECTION('ref_axis',(1.66964440532393E-10,0.866072438648236,0.499918524375621));
#132416=DIRECTION('',(1.04744440165294E-14,-1.,-6.98296267768627E-15));
#132417=DIRECTION('center_axis',(-0.999999999998207,-9.46713291890296E-7,
-1.63977758665962E-6));
#132418=DIRECTION('ref_axis',(-5.62799362796097E-11,0.866043178341318,-0.499969212300586));
#132419=DIRECTION('',(5.09253499664396E-15,-0.500005012714988,0.866022509672748));
#132420=DIRECTION('',(1.04744440165294E-14,-1.,-6.98296267768627E-15));
#132421=DIRECTION('center_axis',(-1.26097532010602E-16,-7.12300817482632E-15,
1.));
#132422=DIRECTION('ref_axis',(0.,-1.,-7.12300817482632E-15));
#132423=DIRECTION('',(0.104528463267664,-0.994521895368272,-7.07080680950905E-15));
#132424=DIRECTION('center_axis',(1.26097532010602E-16,7.12300817482632E-15,
-1.));
#132425=DIRECTION('ref_axis',(1.94422256072357E-12,-1.,-7.12300817482607E-15));
#132426=DIRECTION('',(-0.104528463267664,0.994521895368272,7.07080680950905E-15));
#132427=DIRECTION('center_axis',(-1.26097532010602E-16,-7.12300817482632E-15,
1.));
#132428=DIRECTION('ref_axis',(-4.47664446791214E-34,-1.,-7.12300817482632E-15));
#132429=DIRECTION('center_axis',(-0.994521895368272,-0.104528463267664,
-8.69963854894046E-16));
#132430=DIRECTION('ref_axis',(1.26097532010602E-16,7.12300817482632E-15,
-1.));
#132431=DIRECTION('center_axis',(-0.994521895368272,-0.104528463267665,
-4.06622861650637E-15));
#132432=DIRECTION('ref_axis',(0.0914259726158941,-0.869860024049313,0.484752338923875));
#132433=DIRECTION('',(-0.0553922155203146,0.527021726387062,-0.848044693619241));
#132434=DIRECTION('',(0.104528463267664,-0.994521895368272,-7.07080680950905E-15));
#132435=DIRECTION('',(-0.0553921607193175,0.527021204990389,0.848045021223121));
#132436=DIRECTION('center_axis',(-0.994521895368273,-0.104528463267656,
-1.16128759054646E-14));
#132437=DIRECTION('ref_axis',(0.0914257765946433,-0.869858159031697,-0.484755722544926));
#132438=DIRECTION('',(-0.104528463267664,0.994521895368272,6.92998990261914E-15));
#132439=DIRECTION('',(-0.0522647556052188,0.497265932938934,-0.866022509672756));
#132440=DIRECTION('center_axis',(0.994521994337724,0.104527521619073,-1.63998886545253E-6));
#132441=DIRECTION('ref_axis',(0.0905292101912599,-0.861327901107503,0.49991870226657));
#132442=DIRECTION('',(-0.104528463267664,0.994521895368272,6.92998990261914E-15));
#132443=DIRECTION('center_axis',(0.994521796385909,0.104529405004782,-1.64014405966769E-6));
#132444=DIRECTION('ref_axis',(0.0905261737131075,-0.861299008812068,-0.499969028332969));
#132445=DIRECTION('',(-0.0522647719724914,0.497266088663002,0.86602241926896));
#132446=DIRECTION('',(-0.104528463267664,0.994521895368272,6.92998990261914E-15));
#132447=DIRECTION('center_axis',(-0.994521895368272,-0.104528463267664,
-8.69963854894046E-16));
#132448=DIRECTION('ref_axis',(1.26097532010602E-16,7.12300817482632E-15,
-1.));
#132449=DIRECTION('center_axis',(0.994521895368272,0.104528463267664,5.03109757269921E-15));
#132450=DIRECTION('ref_axis',(0.0914257765928723,-0.86985815901481,-0.484755722575562));
#132451=DIRECTION('',(0.0553921607193168,-0.527021204990422,-0.8480450212231));
#132452=DIRECTION('',(-0.104528463267664,0.994521895368272,7.07080680950905E-15));
#132453=DIRECTION('',(0.0553922155203126,-0.527021726387072,0.848044693619235));
#132454=DIRECTION('center_axis',(0.994521895368273,0.104528463267659,-1.53000466606121E-14));
#132455=DIRECTION('ref_axis',(0.091425972618011,-0.869860024069418,0.484752338887397));
#132456=DIRECTION('',(0.104528463267664,-0.994521895368272,-6.92998990261914E-15));
#132457=DIRECTION('',(0.0522647719724914,-0.497266088663002,-0.86602241926896));
#132458=DIRECTION('center_axis',(-0.994521994360728,-0.104527521400198,
-1.64037039730765E-6));
#132459=DIRECTION('ref_axis',(0.0905292209241536,-0.861328003226653,-0.499918524378176));
#132460=DIRECTION('',(0.104528463267664,-0.994521895368272,-6.92998990261914E-15));
#132461=DIRECTION('center_axis',(-0.994521796408006,-0.104529404794558,
-1.63977757761829E-6));
#132462=DIRECTION('ref_axis',(0.0905261626115233,-0.861298903189835,0.499969212298937));
#132463=DIRECTION('',(0.0522647556052198,-0.497265932938937,0.866022509672754));
#132464=DIRECTION('',(0.104528463267664,-0.994521895368272,-6.92998990261914E-15));
#132465=DIRECTION('center_axis',(-1.11539425682701E-16,-7.12070239730339E-15,
1.));
#132466=DIRECTION('ref_axis',(0.,-1.,-7.12070239730339E-15));
#132467=DIRECTION('',(0.20791169081777,-0.978147600733803,-6.94190761487522E-15));
#132468=DIRECTION('center_axis',(1.11539425682701E-16,7.12070239730339E-15,
-1.));
#132469=DIRECTION('ref_axis',(2.43272069155864E-12,-1.,-7.12070239730312E-15));
#132470=DIRECTION('',(-0.20791169081777,0.978147600733803,6.94190761487522E-15));
#132471=DIRECTION('center_axis',(-1.11539425682701E-16,-7.12070239730339E-15,
1.));
#132472=DIRECTION('ref_axis',(1.66310349712474E-34,-1.,-7.12070239730339E-15));
#132473=DIRECTION('center_axis',(-0.978147600733803,-0.20791169081777,-1.58957929685225E-15));
#132474=DIRECTION('ref_axis',(1.11539425682701E-16,7.12070239730339E-15,
-1.));
#132475=DIRECTION('center_axis',(-0.978147600733804,-0.207911690817767,
1.55757231750933E-14));
#132476=DIRECTION('ref_axis',(0.18185026314356,-0.855538223401705,0.484752338925015));
#132477=DIRECTION('',(-0.110177542335814,0.518344583061392,-0.848044693619241));
#132478=DIRECTION('',(0.20791169081777,-0.978147600733803,-6.94190761487522E-15));
#132479=DIRECTION('',(-0.110177433334236,0.518344070249262,0.848045021223112));
#132480=DIRECTION('center_axis',(-0.978147600733805,-0.207911690817763,
-2.29500752315691E-14));
#132481=DIRECTION('ref_axis',(0.181849873249108,-0.855536389092526,-0.484755722542607));
#132482=DIRECTION('',(-0.20791169081777,0.978147600733803,6.80109070798531E-15));
#132483=DIRECTION('',(-0.103956887610934,0.489078703542018,-0.866022509672761));
#132484=DIRECTION('center_axis',(0.978147797590168,0.207910764672768,-1.63998886205246E-6));
#132485=DIRECTION('ref_axis',(0.180066563578227,-0.847146577522247,0.499918702264151));
#132486=DIRECTION('',(-0.20791169081777,0.978147600733803,6.80109070798531E-15));
#132487=DIRECTION('center_axis',(0.978147403855344,0.20791261704947,-1.64014402984576E-6));
#132488=DIRECTION('ref_axis',(0.180060523666867,-0.847118160899729,-0.49996902833143));
#132489=DIRECTION('',(-0.103956920166131,0.489078856702218,0.866022419268938));
#132490=DIRECTION('',(-0.20791169081777,0.978147600733803,6.80109070798531E-15));
#132491=DIRECTION('center_axis',(-0.978147600733803,-0.20791169081777,-1.58957929685225E-15));
#132492=DIRECTION('ref_axis',(1.11539425682701E-16,7.12070239730339E-15,
-1.));
#132493=DIRECTION('center_axis',(0.9781476007338,0.207911690817786,-3.72163382090113E-14));
#132494=DIRECTION('ref_axis',(0.181849873245312,-0.855536389074707,-0.484755722575481));
#132495=DIRECTION('',(0.110177433334237,-0.518344070249266,-0.848045021223109));
#132496=DIRECTION('',(-0.20791169081777,0.978147600733803,6.94190761487522E-15));
#132497=DIRECTION('',(0.11017754233582,-0.518344583061406,0.848044693619231));
#132498=DIRECTION('center_axis',(0.9781476007338,0.207911690817784,3.30811819688897E-14));
#132499=DIRECTION('ref_axis',(0.181850263147783,-0.855538223421614,0.484752338888293));
#132500=DIRECTION('',(0.20791169081777,-0.978147600733803,-6.80109070798531E-15));
#132501=DIRECTION('',(0.103956920166142,-0.489078856702191,-0.866022419268952));
#132502=DIRECTION('center_axis',(-0.978147797635921,-0.207910764457509,
-1.6403703732092E-6));
#132503=DIRECTION('ref_axis',(0.18006658492685,-0.847146677960871,-0.499918524374365));
#132504=DIRECTION('',(0.20791169081777,-0.978147600733803,-6.80109070798531E-15));
#132505=DIRECTION('center_axis',(-0.978147403899293,-0.207912616842712,
-1.63977756346E-6));
#132506=DIRECTION('ref_axis',(0.18006050158514,-0.847118057014537,0.499969212300941));
#132507=DIRECTION('',(0.103956887610927,-0.489078703542022,0.866022509672759));
#132508=DIRECTION('',(0.20791169081777,-0.978147600733803,-6.80109070798531E-15));
#132509=DIRECTION('center_axis',(-9.73020895656121E-17,-7.11688751458844E-15,
1.));
#132510=DIRECTION('ref_axis',(0.,-1.,-7.11688751458844E-15));
#132511=DIRECTION('',(0.309016994374957,-0.95105651629515,-6.73849424722497E-15));
#132512=DIRECTION('center_axis',(9.73020895656121E-17,7.11688751458844E-15,
-1.));
#132513=DIRECTION('ref_axis',(2.04991579266789E-12,-1.,-7.11688751458824E-15));
#132514=DIRECTION('',(-0.309016994374957,0.95105651629515,6.73849424722497E-15));
#132515=DIRECTION('center_axis',(-9.73020895656121E-17,-7.11688751458844E-15,
1.));
#132516=DIRECTION('ref_axis',(-2.26114224696972E-34,-1.,-7.11688751458844E-15));
#132517=DIRECTION('center_axis',(-0.95105651629515,-0.309016994374957,-2.29177897539329E-15));
#132518=DIRECTION('ref_axis',(9.73020895656121E-17,7.11688751458844E-15,
-1.));
#132519=DIRECTION('center_axis',(-0.95105651629515,-0.309016994374959,-2.06757387279998E-14));
#132520=DIRECTION('ref_axis',(0.270282164134165,-0.831842966947816,0.484752338922059));
#132521=DIRECTION('',(-0.163755740941355,0.503988348013135,-0.848044693619233));
#132522=DIRECTION('',(0.309016994374957,-0.95105651629515,-6.73849424722497E-15));
#132523=DIRECTION('',(-0.16375557893343,0.503987849404,0.848045021223112));
#132524=DIRECTION('center_axis',(-0.951056516295154,-0.309016994374946,
-1.50243735750233E-14));
#132525=DIRECTION('ref_axis',(0.270281584637449,-0.831841183440299,-0.484755722543337));
#132526=DIRECTION('',(-0.309016994374957,0.95105651629515,6.59767734033506E-15));
#132527=DIRECTION('',(-0.15451004620158,0.475533025522862,-0.866022509672733));
#132528=DIRECTION('center_axis',(0.951056808881622,0.309016093880587,-1.63998882874534E-6));
#132529=DIRECTION('ref_axis',(0.267631070011315,-0.823683738749887,0.499918702274287));
#132530=DIRECTION('',(-0.309016994374957,0.95105651629515,6.59767734033506E-15));
#132531=DIRECTION('center_axis',(0.951056223677624,0.309017894953297,-1.6401440826045E-6));
#132532=DIRECTION('ref_axis',(0.267622092843495,-0.823656109145871,-0.499969028329508));
#132533=DIRECTION('',(-0.154510094588054,0.475533174441002,0.866022419268955));
#132534=DIRECTION('',(-0.309016994374957,0.95105651629515,6.59767734033506E-15));
#132535=DIRECTION('center_axis',(-0.95105651629515,-0.309016994374957,-2.29177897539329E-15));
#132536=DIRECTION('ref_axis',(9.73020895656121E-17,7.11688751458844E-15,
-1.));
#132537=DIRECTION('center_axis',(0.951056516295148,0.309016994374965,-3.58379553123804E-15));
#132538=DIRECTION('ref_axis',(0.270281584632359,-0.831841183424602,-0.48475572257311));
#132539=DIRECTION('',(0.163755578933425,-0.503987849403991,-0.848045021223118));
#132540=DIRECTION('',(-0.309016994374957,0.95105651629515,6.73849424722497E-15));
#132541=DIRECTION('',(0.16375574094136,-0.503988348013125,0.848044693619238));
#132542=DIRECTION('center_axis',(0.951056516295157,0.309016994374937,-1.84703265992951E-14));
#132543=DIRECTION('ref_axis',(0.27028216414019,-0.831842966966363,0.484752338886874));
#132544=DIRECTION('',(0.309016994374957,-0.95105651629515,-6.59767734033506E-15));
#132545=DIRECTION('',(0.154510094588066,-0.475533174440984,-0.866022419268963));
#132546=DIRECTION('center_axis',(-0.95105680894964,-0.309016093671246,-1.64037039704993E-6));
#132547=DIRECTION('ref_axis',(0.267631101742292,-0.823683836408668,-0.49991852438103));
#132548=DIRECTION('',(0.309016994374957,-0.95105651629515,-6.59767734033506E-15));
#132549=DIRECTION('center_axis',(-0.951056223742958,-0.309017894752224,
-1.63977753144346E-6));
#132550=DIRECTION('ref_axis',(0.267622060023759,-0.823656008137881,0.499969212299128));
#132551=DIRECTION('',(0.154510046201588,-0.475533025522832,0.866022509672748));
#132552=DIRECTION('',(0.309016994374957,-0.95105651629515,-6.59767734033506E-15));
#132553=DIRECTION('center_axis',(-8.35415108931894E-17,-7.11160532333482E-15,
1.));
#132554=DIRECTION('ref_axis',(0.,-1.,-7.11160532333482E-15));
#132555=DIRECTION('',(0.40673664307581,-0.913545457642596,-6.46279534598126E-15));
#132556=DIRECTION('center_axis',(8.35415108931894E-17,7.11160532333482E-15,
-1.));
#132557=DIRECTION('ref_axis',(2.68496336275348E-12,-1.,-7.1116053233346E-15));
#132558=DIRECTION('',(-0.40673664307581,0.913545457642596,6.46279534598126E-15));
#132559=DIRECTION('center_axis',(-8.35415108931894E-17,-7.11160532333482E-15,
1.));
#132560=DIRECTION('ref_axis',(-2.16423649025571E-35,-1.,-7.11160532333482E-15));
#132561=DIRECTION('center_axis',(-0.913545457642596,-0.40673664307581,-2.96886944389434E-15));
#132562=DIRECTION('ref_axis',(8.35415108931894E-17,7.11160532333482E-15,
-1.));
#132563=DIRECTION('center_axis',(-0.913545457642605,-0.40673664307579,5.65136858565243E-14));
#132564=DIRECTION('ref_axis',(0.355752797174256,-0.799033864872624,0.484752338921031));
#132565=DIRECTION('',(-0.215539797381057,0.484110311157699,-0.848044693619227));
#132566=DIRECTION('',(0.40673664307581,-0.913545457642596,-6.46279534598126E-15));
#132567=DIRECTION('',(-0.215539584141776,0.484109832214421,0.848045021223116));
#132568=DIRECTION('center_axis',(-0.913545457642584,-0.406736643075839,
5.12758437606272E-14));
#132569=DIRECTION('ref_axis',(0.355752034424302,-0.799032151708189,-0.484755722544409));
#132570=DIRECTION('',(-0.40673664307581,0.913545457642596,6.32197843909135E-15));
#132571=DIRECTION('',(-0.203370360392764,0.456777308164346,-0.866022509672728));
#132572=DIRECTION('center_axis',(0.913545842753558,0.406735778098021,-1.63998887083193E-6));
#132573=DIRECTION('ref_axis',(0.352263354437923,-0.791196448576317,0.499918702271044));
#132574=DIRECTION('',(-0.40673664307581,0.913545457642596,6.32197843909135E-15));
#132575=DIRECTION('center_axis',(0.913545072492023,0.406737508133752,-1.6401440046282E-6));
#132576=DIRECTION('ref_axis',(0.352251538366133,-0.791169908695755,-0.4999690283338));
#132577=DIRECTION('',(-0.203370424080347,0.456777451208943,0.866022419268948));
#132578=DIRECTION('',(-0.40673664307581,0.913545457642596,6.32197843909135E-15));
#132579=DIRECTION('center_axis',(-0.913545457642596,-0.40673664307581,-2.96886944389434E-15));
#132580=DIRECTION('ref_axis',(8.35415108931894E-17,7.11160532333482E-15,
-1.));
#132581=DIRECTION('center_axis',(0.913545457642598,0.406736643075806,1.40595055456264E-14));
#132582=DIRECTION('ref_axis',(0.355752034418223,-0.799032151694536,-0.484755722571374));
#132583=DIRECTION('',(0.215539584141769,-0.484109832214432,-0.848045021223112));
#132584=DIRECTION('',(-0.40673664307581,0.913545457642596,6.46279534598126E-15));
#132585=DIRECTION('',(0.215539797381038,-0.484110311157674,0.848044693619246));
#132586=DIRECTION('center_axis',(0.913545457642592,0.40673664307582,1.10270606562972E-15));
#132587=DIRECTION('ref_axis',(0.355752797182001,-0.799033864890016,0.484752338886678));
#132588=DIRECTION('',(0.40673664307581,-0.913545457642596,-6.32197843909135E-15));
#132589=DIRECTION('',(0.203370424080339,-0.456777451208961,-0.866022419268941));
#132590=DIRECTION('center_axis',(-0.91354584284308,-0.406735777896949,-1.64037046486974E-6));
#132591=DIRECTION('ref_axis',(0.352263396203447,-0.791196542383823,-0.499918524376819));
#132592=DIRECTION('',(0.40673664307581,-0.913545457642596,-6.32197843909135E-15));
#132593=DIRECTION('center_axis',(-0.913545072577972,-0.406737507940709,
-1.63977757327142E-6));
#132594=DIRECTION('ref_axis',(0.352251495169606,-0.791169811675268,0.499969212296615));
#132595=DIRECTION('',(0.203370360392774,-0.456777308164294,0.866022509672754));
#132596=DIRECTION('',(0.40673664307581,-0.913545457642596,-6.32197843909135E-15));
#132597=DIRECTION('center_axis',(-7.04084534449538E-17,-7.10491369633528E-15,
1.));
#132598=DIRECTION('ref_axis',(0.,-1.,-7.10491369633528E-15));
#132599=DIRECTION('',(0.50000000000001,-0.866025403784433,-6.11783152599983E-15));
#132600=DIRECTION('center_axis',(7.04084534449538E-17,7.10491369633528E-15,
-1.));
#132601=DIRECTION('ref_axis',(3.95505850292466E-12,-1.,-7.104913696335E-15));
#132602=DIRECTION('',(-0.50000000000001,0.866025403784433,6.11783152599983E-15));
#132603=DIRECTION('center_axis',(-7.04084534449538E-17,-7.10491369633528E-15,
1.));
#132604=DIRECTION('ref_axis',(2.79014006612264E-35,-1.,-7.10491369633528E-15));
#132605=DIRECTION('center_axis',(-0.866025403784433,-0.50000000000001,-3.61343235749221E-15));
#132606=DIRECTION('ref_axis',(7.04084534449532E-17,7.10491369633528E-15,
-1.));
#132607=DIRECTION('center_axis',(-0.866025403784415,-0.500000000000041,
-4.57623017179726E-14));
#132608=DIRECTION('ref_axis',(0.437325728121579,-0.75747038056359,0.484752338923477));
#132609=DIRECTION('',(-0.264962354696025,0.458928260426615,-0.848044693619233));
#132610=DIRECTION('',(0.50000000000001,-0.866025403784433,-6.11783152599983E-15));
#132611=DIRECTION('',(-0.264962092561705,0.458927806396624,0.84804502122311));
#132612=DIRECTION('center_axis',(-0.866025403784414,-0.500000000000042,
4.24541932211702E-14));
#132613=DIRECTION('ref_axis',(0.437324790476598,-0.757468756514837,-0.484755722543288));
#132614=DIRECTION('',(-0.50000000000001,0.866025403784433,5.97701461910992E-15));
#132615=DIRECTION('',(-0.250002506357492,0.433017043030769,-0.866022509672735));
#132616=DIRECTION('center_axis',(0.866025877200505,0.499999180015734,-1.63998885826603E-6));
#132617=DIRECTION('ref_axis',(0.433036167836874,-0.750040644541799,0.499918702271157));
#132618=DIRECTION('',(-0.50000000000001,0.866025403784433,5.97701461910992E-15));
#132619=DIRECTION('center_axis',(0.866024930320558,0.500000820059909,-1.64014405299743E-6));
#132620=DIRECTION('ref_axis',(0.433021642322225,-0.750015485165992,-0.49996902833254));
#132621=DIRECTION('',(-0.25000258464842,0.4330171786346,0.866022419268947));
#132622=DIRECTION('',(-0.50000000000001,0.866025403784433,5.97701461910992E-15));
#132623=DIRECTION('center_axis',(-0.866025403784433,-0.50000000000001,-3.61343235749221E-15));
#132624=DIRECTION('ref_axis',(7.04084534449532E-17,7.10491369633528E-15,
-1.));
#132625=DIRECTION('center_axis',(0.866025403784456,0.499999999999971,7.05732043074528E-14));
#132626=DIRECTION('ref_axis',(0.437324790468406,-0.757468756500684,-0.484755722572795));
#132627=DIRECTION('',(0.264962092561699,-0.458927806396623,-0.848045021223113));
#132628=DIRECTION('',(-0.50000000000001,0.866025403784433,6.11783152599983E-15));
#132629=DIRECTION('',(0.264962354696034,-0.45892826042662,0.848044693619228));
#132630=DIRECTION('center_axis',(0.866025403784424,0.500000000000025,2.86703577063736E-14));
#132631=DIRECTION('ref_axis',(0.437325728131524,-0.75747038058083,0.484752338887564));
#132632=DIRECTION('',(0.50000000000001,-0.866025403784433,-5.97701461910992E-15));
#132633=DIRECTION('',(0.250002584648411,-0.433017178634585,-0.866022419268958));
#132634=DIRECTION('center_axis',(-0.866025877310554,-0.499999179825123,
-1.64037042562352E-6));
#132635=DIRECTION('ref_axis',(0.433036219179263,-0.750040733469941,-0.499918524376525));
#132636=DIRECTION('',(0.50000000000001,-0.866025403784433,-5.97701461910992E-15));
#132637=DIRECTION('center_axis',(-0.866024930426216,-0.500000819876906,
-1.63977764694425E-6));
#132638=DIRECTION('ref_axis',(0.433021589220468,-0.750015393191488,0.499969212296916));
#132639=DIRECTION('',(0.25000250635749,-0.433017043030737,0.866022509672751));
#132640=DIRECTION('',(0.50000000000001,-0.866025403784433,-5.97701461910992E-15));
#132641=DIRECTION('center_axis',(-5.80468057465775E-17,-7.09688594845552E-15,
1.));
#132642=DIRECTION('ref_axis',(0.,-1.,-7.09688594845552E-15));
#132643=DIRECTION('',(0.587785252292482,-0.809016994374941,-5.70738228308071E-15));
#132644=DIRECTION('center_axis',(5.80468057465775E-17,7.09688594845552E-15,
-1.));
#132645=DIRECTION('ref_axis',(1.29496413592278E-12,-1.,-7.09688594845544E-15));
#132646=DIRECTION('',(-0.587785252292482,0.809016994374941,5.70738228308071E-15));
#132647=DIRECTION('center_axis',(-5.80468057465775E-17,-7.09688594845552E-15,
1.));
#132648=DIRECTION('ref_axis',(-1.65143981133805E-35,-1.,-7.09688594845552E-15));
#132649=DIRECTION('center_axis',(-0.809016994374941,-0.587785252292482,
-4.21840575002206E-15));
#132650=DIRECTION('ref_axis',(5.80468057465773E-17,7.09688594845552E-15,
-1.));
#132651=DIRECTION('center_axis',(-0.809016994374934,-0.587785252292492,
-1.70919440151463E-14));
#132652=DIRECTION('ref_axis',(0.514107226875991,-0.707607892255666,0.484752338923055));
#132653=DIRECTION('',(-0.311481929006023,0.428718095637386,-0.848044693619234));
#132654=DIRECTION('',(0.587785252292482,-0.809016994374941,-5.70738228308071E-15));
#132655=DIRECTION('',(-0.311481620848639,0.42871767149511,0.848045021223116));
#132656=DIRECTION('center_axis',(-0.809016994374956,-0.587785252292461,
-4.25920315108481E-14));
#132657=DIRECTION('ref_axis',(0.514106124607205,-0.707606375112844,-0.484755722545925));
#132658=DIRECTION('',(-0.587785252292482,0.809016994374941,5.5665653761908E-15));
#132659=DIRECTION('',(-0.293895572546166,0.404512552559088,-0.866022509672753));
#132660=DIRECTION('center_axis',(0.809017550909288,0.587784486285619,-1.6399888522409E-6));
#132661=DIRECTION('ref_axis',(0.509064546362868,-0.700667238250335,0.499918702269694));
#132662=DIRECTION('',(-0.587785252292482,0.809016994374941,5.5665653761908E-15));
#132663=DIRECTION('center_axis',(0.809016437785122,0.587786018369595,-1.64014405557944E-6));
#132664=DIRECTION('ref_axis',(0.509047470547774,-0.700643735027332,-0.499969028336619));
#132665=DIRECTION('',(-0.2938956645827,0.40451267923647,0.866022419268939));
#132666=DIRECTION('',(-0.587785252292482,0.809016994374941,5.5665653761908E-15));
#132667=DIRECTION('center_axis',(-0.809016994374941,-0.587785252292482,
-4.21840575002206E-15));
#132668=DIRECTION('ref_axis',(5.80468057465773E-17,7.09688594845552E-15,
-1.));
#132669=DIRECTION('center_axis',(0.80901699437492,0.587785252292511,-6.86434682521677E-14));
#132670=DIRECTION('ref_axis',(0.514106124598168,-0.707606375100405,-0.484755722573667));
#132671=DIRECTION('',(0.311481620848642,-0.428717671495118,-0.848045021223111));
#132672=DIRECTION('',(-0.587785252292482,0.809016994374941,5.70738228308071E-15));
#132673=DIRECTION('',(0.311481929006041,-0.428718095637379,0.848044693619231));
#132674=DIRECTION('center_axis',(0.809016994374977,0.587785252292433,-9.88300311320588E-14));
#132675=DIRECTION('ref_axis',(0.514107226887611,-0.707607892271672,0.484752338887366));
#132676=DIRECTION('',(0.587785252292482,-0.809016994374941,-5.5665653761908E-15));
#132677=DIRECTION('',(0.293895664582663,-0.404512679236504,-0.866022419268936));
#132678=DIRECTION('center_axis',(-0.809017551038663,-0.587784486107547,
-1.6403705092797E-6));
#132679=DIRECTION('ref_axis',(0.509064606718493,-0.700667321323101,-0.49991852437818));
#132680=DIRECTION('',(0.587785252292482,-0.809016994374941,-5.5665653761908E-15));
#132681=DIRECTION('center_axis',(-0.809016437909362,-0.587786018198594,
-1.63977769066598E-6));
#132682=DIRECTION('ref_axis',(0.509047408122836,-0.700643649107263,0.499969212301199));
#132683=DIRECTION('',(0.293895572546205,-0.40451255255908,0.866022509672743));
#132684=DIRECTION('',(0.587785252292482,-0.809016994374941,-5.5665653761908E-15));
#132685=DIRECTION('center_axis',(-4.65920045970846E-17,-7.08761003338123E-15,
1.));
#132686=DIRECTION('ref_axis',(0.,-1.,-7.08761003338124E-15));
#132687=DIRECTION('',(0.669130606358867,-0.743144825477386,-5.23594458502135E-15));
#132688=DIRECTION('center_axis',(4.65920045970846E-17,7.08761003338124E-15,
-1.));
#132689=DIRECTION('ref_axis',(-5.08215691752411E-12,-1.,-7.08761003338147E-15));
#132690=DIRECTION('',(-0.669130606358867,0.743144825477386,5.23594458502135E-15));
#132691=DIRECTION('center_axis',(-4.65920045970846E-17,-7.08761003338124E-15,
1.));
#132692=DIRECTION('ref_axis',(-1.03129032759636E-34,-1.,-7.08761003338123E-15));
#132693=DIRECTION('center_axis',(-0.743144825477386,-0.669130606358867,
-4.77716140639652E-15));
#132694=DIRECTION('ref_axis',(4.65920045970844E-17,7.08761003338124E-15,
-1.));
#132695=DIRECTION('center_axis',(-0.743144825477404,-0.669130606358848,
1.37838258186658E-14));
#132696=DIRECTION('ref_axis',(0.585256059268725,-0.64999270380347,0.484752338923184));
#132697=DIRECTION('',(-0.354588842120043,0.393810805677302,-0.848044693619246));
#132698=DIRECTION('',(0.669130606358867,-0.743144825477386,-5.23594458502135E-15));
#132699=DIRECTION('',(-0.354588491315847,0.39381041606975,0.84804502122312));
#132700=DIRECTION('center_axis',(-0.743144825477363,-0.669130606358893,
8.68381224978359E-14));
#132701=DIRECTION('ref_axis',(0.585254804454868,-0.649991310191489,-0.484755722542855));
#132702=DIRECTION('',(-0.669130606358867,0.743144825477386,5.09512767813144E-15));
#132703=DIRECTION('',(-0.33456865734045,0.371576137911913,-0.866022509672743));
#132704=DIRECTION('center_axis',(0.743145459032533,0.669129902721913,-1.63998890336437E-6));
#132705=DIRECTION('ref_axis',(0.579515507191614,-0.643617175073762,0.499918702265194));
#132706=DIRECTION('',(-0.669130606358867,0.743144825477386,5.09512767813144E-15));
#132707=DIRECTION('center_axis',(0.743144191859767,0.669131310059845,-1.64014407107154E-6));
#132708=DIRECTION('ref_axis',(0.579496068163303,-0.643595585511986,-0.499969028333513));
#132709=DIRECTION('',(-0.334568762114147,0.371576254274927,0.866022419268937));
#132710=DIRECTION('',(-0.669130606358867,0.743144825477386,5.09512767813144E-15));
#132711=DIRECTION('center_axis',(-0.743144825477386,-0.669130606358867,
-4.77716140639652E-15));
#132712=DIRECTION('ref_axis',(4.65920045970844E-17,7.08761003338124E-15,
-1.));
#132713=DIRECTION('center_axis',(0.743144825477406,0.669130606358846,1.31773404917825E-13));
#132714=DIRECTION('ref_axis',(0.585254804442819,-0.649991310178033,-0.484755722575444));
#132715=DIRECTION('',(0.35458849131585,-0.393810416069767,-0.848045021223111));
#132716=DIRECTION('',(-0.669130606358867,0.743144825477386,5.23594458502135E-15));
#132717=DIRECTION('',(0.354588842120061,-0.393810805677319,0.848044693619231));
#132718=DIRECTION('center_axis',(0.743144825477364,0.669130606358892,1.20746314186455E-13));
#132719=DIRECTION('ref_axis',(0.585256059281856,-0.649992703818073,0.48475233888775));
#132720=DIRECTION('',(0.669130606358867,-0.743144825477386,-5.09512767813144E-15));
#132721=DIRECTION('',(0.334568762114181,-0.371576254274921,-0.866022419268926));
#132722=DIRECTION('center_axis',(-0.743145459179761,-0.669129902558398,
-1.64037041512388E-6));
#132723=DIRECTION('ref_axis',(0.579515575899139,-0.643617251381538,-0.499918524376086));
#132724=DIRECTION('',(0.669130606358867,-0.743144825477386,-5.09512767813144E-15));
#132725=DIRECTION('center_axis',(-0.743144192001212,-0.669131309902755,
-1.63977757292739E-6));
#132726=DIRECTION('ref_axis',(0.579495997099853,-0.643595506588377,0.499969212296615));
#132727=DIRECTION('',(0.334568657340469,-0.371576137911896,0.866022509672743));
#132728=DIRECTION('',(0.669130606358867,-0.743144825477386,-5.09512767813144E-15));
#132729=DIRECTION('center_axis',(-3.61695511949404E-17,-7.07718757997909E-15,
1.));
#132730=DIRECTION('ref_axis',(0.,-1.,-7.07718757997909E-15));
#132731=DIRECTION('',(0.743144825477402,-0.66913060635885,-4.70868360189637E-15));
#132732=DIRECTION('center_axis',(3.61695511949404E-17,7.07718757997909E-15,
-1.));
#132733=DIRECTION('ref_axis',(1.24700250125898E-12,-1.,-7.07718757997905E-15));
#132734=DIRECTION('',(-0.743144825477402,0.66913060635885,4.70868360189637E-15));
#132735=DIRECTION('center_axis',(-3.61695511949404E-17,-7.07718757997909E-15,
1.));
#132736=DIRECTION('ref_axis',(7.4438098531367E-35,-1.,-7.07718757997909E-15));
#132737=DIRECTION('center_axis',(-0.66913060635885,-0.743144825477402,-5.2835774827172E-15));
#132738=DIRECTION('ref_axis',(3.61695511949403E-17,7.07718757997909E-15,
-1.));
#132739=DIRECTION('center_axis',(-0.669130606358838,-0.743144825477412,
-6.12001866348751E-14));
#132740=DIRECTION('ref_axis',(0.649992703804337,-0.585256059269522,0.484752338921059));
#132741=DIRECTION('',(-0.393810805677327,0.354588842120035,-0.848044693619238));
#132742=DIRECTION('',(0.743144825477402,-0.66913060635885,-4.70868360189637E-15));
#132743=DIRECTION('',(-0.393810416069782,0.354588491315838,0.848045021223109));
#132744=DIRECTION('center_axis',(-0.669130606358808,-0.743144825477439,
6.53353493078882E-14));
#132745=DIRECTION('ref_axis',(0.649991310191254,-0.58525480445462,-0.484755722543471));
#132746=DIRECTION('',(-0.743144825477402,0.66913060635885,4.56786669500646E-15));
#132747=DIRECTION('',(-0.371576137911926,0.334568657340426,-0.866022509672746));
#132748=DIRECTION('center_axis',(0.669131309993341,0.743144191919648,-1.63998873674059E-6));
#132749=DIRECTION('ref_axis',(0.643617174849297,-0.579515507438223,0.499918702268307));
#132750=DIRECTION('',(-0.743144825477402,0.66913060635885,4.56786669500646E-15));
#132751=DIRECTION('center_axis',(0.669129902655539,0.743145459092296,-1.64014398156296E-6));
#132752=DIRECTION('ref_axis',(0.643595585587785,-0.579496068079448,-0.499969028333132));
#132753=DIRECTION('',(-0.371576254274935,0.334568762114158,0.866022419268929));
#132754=DIRECTION('',(-0.743144825477402,0.66913060635885,4.56786669500646E-15));
#132755=DIRECTION('center_axis',(-0.66913060635885,-0.743144825477402,-5.2835774827172E-15));
#132756=DIRECTION('ref_axis',(3.61695511949403E-17,7.07718757997909E-15,
-1.));
#132757=DIRECTION('center_axis',(0.669130606358883,0.743144825477372,6.25785835070068E-14));
#132758=DIRECTION('ref_axis',(0.649991310179483,-0.585254804444058,-0.484755722572005));
#132759=DIRECTION('',(0.393810416069765,-0.354588491315822,-0.848045021223123));
#132760=DIRECTION('',(-0.743144825477402,0.66913060635885,4.70868360189637E-15));
#132761=DIRECTION('',(0.393810805677295,-0.354588842120035,0.848044693619253));
#132762=DIRECTION('center_axis',(0.669130606358823,0.743144825477426,-4.13514774611113E-15));
#132763=DIRECTION('ref_axis',(0.649992703818683,-0.585256059282372,0.48475233888631));
#132764=DIRECTION('',(0.743144825477402,-0.66913060635885,-4.56786669500646E-15));
#132765=DIRECTION('',(0.371576254274878,-0.334568762114136,-0.866022419268962));
#132766=DIRECTION('center_axis',(-0.669131310156998,-0.743144191772289,
-1.64037057985418E-6));
#132767=DIRECTION('ref_axis',(0.643617251158517,-0.579515576147659,-0.499918524375124));
#132768=DIRECTION('',(0.743144825477402,-0.66913060635885,-4.56786669500646E-15));
#132769=DIRECTION('center_axis',(-0.669129902812614,-0.743145458950866,
-1.63977747515624E-6));
#132770=DIRECTION('ref_axis',(0.643595506663296,-0.579495997015805,0.499969212297591));
#132771=DIRECTION('',(0.371576137911909,-0.334568657340446,0.866022509672746));
#132772=DIRECTION('',(0.743144825477402,-0.66913060635885,-4.56786669500646E-15));
#132773=DIRECTION('center_axis',(-2.68936361206573E-17,-7.0657327788296E-15,
1.));
#132774=DIRECTION('ref_axis',(0.,-1.,-7.0657327788296E-15));
#132775=DIRECTION('',(0.809016994374955,-0.587785252292463,-4.13137611537333E-15));
#132776=DIRECTION('center_axis',(2.68936361206573E-17,7.0657327788296E-15,
-1.));
#132777=DIRECTION('ref_axis',(1.22302168392707E-12,-1.,-7.06573277882956E-15));
#132778=DIRECTION('',(-0.809016994374955,0.587785252292463,4.13137611537333E-15));
#132779=DIRECTION('center_axis',(-2.68936361206573E-17,-7.0657327788296E-15,
1.));
#132780=DIRECTION('ref_axis',(-5.51266204707114E-35,-1.,-7.0657327788296E-15));
#132781=DIRECTION('center_axis',(-0.587785252292463,-0.809016994374955,
-5.73210557847756E-15));
#132782=DIRECTION('ref_axis',(2.68936361206571E-17,7.0657327788296E-15,
-1.));
#132783=DIRECTION('center_axis',(-0.587785252292406,-0.809016994374997,
-1.16611166425919E-13));
#132784=DIRECTION('ref_axis',(0.707607892255381,-0.514107226875749,0.484752338923727));
#132785=DIRECTION('',(-0.428718095637369,0.31148192900601,-0.848044693619247));
#132786=DIRECTION('',(0.809016994374955,-0.587785252292463,-4.13137611537333E-15));
#132787=DIRECTION('',(-0.428717671495122,0.311481620848618,0.848045021223118));
#132788=DIRECTION('center_axis',(-0.587785252292469,-0.809016994374951,
-1.77811393686054E-14));
#132789=DIRECTION('ref_axis',(0.707606375113731,-0.514106124607824,-0.484755722543974));
#132790=DIRECTION('',(-0.809016994374955,0.587785252292463,3.99055920848342E-15));
#132791=DIRECTION('',(-0.404512552559104,0.293895572546187,-0.866022509672738));
#132792=DIRECTION('center_axis',(0.587786018297211,0.809016437837712,-1.63998882504441E-6));
#132793=DIRECTION('ref_axis',(0.700667238053777,-0.509064546632195,0.499918702270929));
#132794=DIRECTION('',(-0.809016994374955,0.587785252292463,3.99055920848342E-15));
#132795=DIRECTION('center_axis',(0.587784486213298,0.809017550961831,-1.64014397261229E-6));
#132796=DIRECTION('ref_axis',(0.700643735093623,-0.509047470456162,-0.499969028336995));
#132797=DIRECTION('',(-0.404512679236441,0.293895664582704,0.866022419268951));
#132798=DIRECTION('',(-0.809016994374955,0.587785252292463,3.99055920848342E-15));
#132799=DIRECTION('center_axis',(-0.587785252292463,-0.809016994374955,
-5.73210557847756E-15));
#132800=DIRECTION('ref_axis',(2.68936361206571E-17,7.0657327788296E-15,
-1.));
#132801=DIRECTION('center_axis',(0.587785252292428,0.80901699437498,-5.15515203339627E-14));
#132802=DIRECTION('ref_axis',(0.707606375100059,-0.514106124597877,-0.48475572257448));
#132803=DIRECTION('',(0.428717671495112,-0.311481620848614,-0.848045021223125));
#132804=DIRECTION('',(-0.809016994374955,0.587785252292463,4.13137611537333E-15));
#132805=DIRECTION('',(0.428718095637375,-0.311481929006031,0.848044693619236));
#132806=DIRECTION('center_axis',(0.587785252292464,0.809016994374954,7.58110420120383E-15));
#132807=DIRECTION('ref_axis',(0.707607892271749,-0.514107226887654,0.484752338887208));
#132808=DIRECTION('',(0.809016994374955,-0.587785252292463,-3.99055920848342E-15));
#132809=DIRECTION('',(0.404512679236445,-0.293895664582672,-0.86602241926896));
#132810=DIRECTION('center_axis',(-0.587786018475315,-0.809016437708311,
-1.64037046349258E-6));
#132811=DIRECTION('ref_axis',(0.700667321127176,-0.509064606988881,-0.499918524377446));
#132812=DIRECTION('',(0.809016994374955,-0.587785252292463,-3.99055920848342E-15));
#132813=DIRECTION('center_axis',(-0.587784486384234,-0.80901755083764,-1.63977767276418E-6));
#132814=DIRECTION('ref_axis',(0.700643649175429,-0.509047408033247,0.499969212296889));
#132815=DIRECTION('',(0.404512552559084,-0.293895572546137,0.866022509672764));
#132816=DIRECTION('',(0.809016994374955,-0.587785252292463,-3.99055920848342E-15));
#132817=DIRECTION('center_axis',(-1.88658882408992E-17,-7.05337113113122E-15,
1.));
#132818=DIRECTION('ref_axis',(0.,-1.,-7.05337113113122E-15));
#132819=DIRECTION('',(0.866025403784445,-0.499999999999989,-3.51034722708395E-15));
#132820=DIRECTION('center_axis',(1.88658882408992E-17,7.05337113113122E-15,
-1.));
#132821=DIRECTION('ref_axis',(1.7245796508144E-35,-1.,-7.05337113113122E-15));
#132822=DIRECTION('',(-0.866025403784445,0.499999999999989,3.51034722708395E-15));
#132823=DIRECTION('center_axis',(-1.88658882408992E-17,-7.05337113113122E-15,
1.));
#132824=DIRECTION('ref_axis',(5.32933612927079E-36,-1.,-7.05337113113122E-15));
#132825=DIRECTION('center_axis',(-0.499999999999989,-0.866025403784445,
-6.11783152599991E-15));
#132826=DIRECTION('ref_axis',(1.88658882408991E-17,7.05337113113122E-15,
-1.));
#132827=DIRECTION('center_axis',(-0.500000000000019,-0.866025403784427,
1.90216796297591E-14));
#132828=DIRECTION('ref_axis',(0.7574703805651,-0.437325728122441,0.484752338920339));
#132829=DIRECTION('',(-0.458928260426615,0.264962354696012,-0.848044693619237));
#132830=DIRECTION('',(0.866025403784445,-0.499999999999989,-3.51034722708395E-15));
#132831=DIRECTION('',(-0.458927806396625,0.264962092561681,0.848045021223117));
#132832=DIRECTION('center_axis',(-0.499999999999992,-0.866025403784443,
4.09379720346935E-14));
#132833=DIRECTION('ref_axis',(0.757468756514768,-0.437324790476546,-0.484755722543443));
#132834=DIRECTION('',(-0.866025403784445,0.499999999999989,3.36953032019404E-15));
#132835=DIRECTION('',(-0.433017043030785,0.250002506357516,-0.86602250967272));
#132836=DIRECTION('center_axis',(0.500000819982458,0.866024930365276,-1.63998880283935E-6));
#132837=DIRECTION('ref_axis',(0.750040644375926,-0.43303616812611,0.49991870226948));
#132838=DIRECTION('',(-0.866025403784445,0.499999999999989,3.36953032019404E-15));
#132839=DIRECTION('center_axis',(0.49999917993825,0.86602587724524,-1.64014411875219E-6));
#132840=DIRECTION('ref_axis',(0.750015485220901,-0.433021642223407,-0.499969028335756));
#132841=DIRECTION('',(-0.433017178634628,0.25000258464838,0.866022419268945));
#132842=DIRECTION('',(-0.866025403784445,0.499999999999989,3.36953032019404E-15));
#132843=DIRECTION('center_axis',(-0.499999999999989,-0.866025403784445,
-6.11783152599991E-15));
#132844=DIRECTION('ref_axis',(1.88658882408991E-17,7.05337113113122E-15,
-1.));
#132845=DIRECTION('center_axis',(0.499999999999992,0.866025403784443,2.56379218773161E-14));
#132846=DIRECTION('ref_axis',(0.757468756499777,-0.437324790467854,-0.48475572257471));
#132847=DIRECTION('',(0.458927806396632,-0.264962092561684,-0.848045021223112));
#132848=DIRECTION('',(-0.866025403784445,0.499999999999989,3.51034722708395E-15));
#132849=DIRECTION('',(0.458928260426591,-0.264962354696007,0.848044693619252));
#132850=DIRECTION('center_axis',(0.499999999999983,0.866025403784448,1.94351944067221E-14));
#132851=DIRECTION('ref_axis',(0.757470380580877,-0.437325728131528,0.484752338887488));
#132852=DIRECTION('',(0.866025403784445,-0.499999999999989,-3.36953032019404E-15));
#132853=DIRECTION('',(0.433017178634599,-0.250002584648384,-0.866022419268958));
#132854=DIRECTION('center_axis',(-0.500000820173042,-0.866024930255241,
-1.64037038534468E-6));
#132855=DIRECTION('ref_axis',(0.750040733305284,-0.433036219469757,-0.499918524371935));
#132856=DIRECTION('',(0.866025403784445,-0.499999999999989,-3.36953032019404E-15));
#132857=DIRECTION('center_axis',(-0.499999180121316,-0.866025877139547,
-1.639777584288E-6));
#132858=DIRECTION('ref_axis',(0.750015393247918,-0.433021589123031,0.499969212296653));
#132859=DIRECTION('',(0.433017043030737,-0.25000250635749,0.866022509672751));
#132860=DIRECTION('',(0.866025403784445,-0.499999999999989,-3.36953032019404E-15));
#132861=DIRECTION('center_axis',(-1.2174261241351E-17,-7.04023807368298E-15,
1.));
#132862=DIRECTION('ref_axis',(0.,-1.,-7.04023807368299E-15));
#132863=DIRECTION('',(0.913545457642606,-0.406736643075789,-2.85240105948698E-15));
#132864=DIRECTION('center_axis',(1.2174261241351E-17,7.04023807368298E-15,
-1.));
#132865=DIRECTION('ref_axis',(-7.04858393874019E-12,-1.,-7.04023807368307E-15));
#132866=DIRECTION('',(-0.913545457642606,0.406736643075789,2.85240105948698E-15));
#132867=DIRECTION('center_axis',(-1.2174261241351E-17,-7.04023807368298E-15,
1.));
#132868=DIRECTION('ref_axis',(2.24415770289596E-35,-1.,-7.04023807368298E-15));
#132869=DIRECTION('center_axis',(-0.406736643075789,-0.913545457642606,
-6.43652923108486E-15));
#132870=DIRECTION('ref_axis',(1.21742612413511E-17,7.04023807368299E-15,
-1.));
#132871=DIRECTION('center_axis',(-0.406736643075775,-0.913545457642612,
-5.54109797910375E-14));
#132872=DIRECTION('ref_axis',(0.799033864872087,-0.355752797174001,0.484752338922104));
#132873=DIRECTION('',(-0.484110311157674,0.215539797381038,-0.848044693619246));
#132874=DIRECTION('',(0.913545457642606,-0.406736643075789,-2.85240105948698E-15));
#132875=DIRECTION('',(-0.484109832214431,0.215539584141763,0.848045021223114));
#132876=DIRECTION('center_axis',(-0.406736643075784,-0.913545457642608,
-1.07513865949709E-14));
#132877=DIRECTION('ref_axis',(0.79903215170898,-0.355752034424618,-0.484755722542873));
#132878=DIRECTION('',(-0.913545457642606,0.406736643075789,2.71158415259707E-15));
#132879=DIRECTION('',(-0.456777308164329,0.203370360392772,-0.866022509672736));
#132880=DIRECTION('center_axis',(0.406737508052128,0.913545072528365,-1.63998884277371E-6));
#132881=DIRECTION('ref_axis',(0.791196448441515,-0.352263354742916,0.499918702269479));
#132882=DIRECTION('',(-0.913545457642606,0.406736643075789,2.71158415259707E-15));
#132883=DIRECTION('center_axis',(0.406735778016422,0.913545842789888,-1.64014388757881E-6));
#132884=DIRECTION('ref_axis',(0.791169908742249,-0.352251538263108,-0.499969028332811));
#132885=DIRECTION('',(-0.456777451208919,0.203370424080316,0.866022419268968));
#132886=DIRECTION('',(-0.913545457642606,0.406736643075789,2.71158415259707E-15));
#132887=DIRECTION('center_axis',(-0.406736643075789,-0.913545457642606,
-6.43652923108486E-15));
#132888=DIRECTION('ref_axis',(1.21742612413511E-17,7.04023807368299E-15,
-1.));
#132889=DIRECTION('center_axis',(0.406736643075769,0.913545457642615,1.24054460696708E-14));
#132890=DIRECTION('ref_axis',(0.79903215169305,-0.355752034417508,-0.484755722574348));
#132891=DIRECTION('',(0.484109832214428,-0.21553958414176,-0.848045021223116));
#132892=DIRECTION('',(-0.913545457642606,0.406736643075789,2.85240105948698E-15));
#132893=DIRECTION('',(0.484110311157676,-0.215539797381039,0.848044693619245));
#132894=DIRECTION('center_axis',(0.406736643075817,0.913545457642593,-4.39704043669829E-14));
#132895=DIRECTION('ref_axis',(0.799033864889077,-0.355752797181557,0.484752338888553));
#132896=DIRECTION('',(0.913545457642606,-0.406736643075789,-2.71158415259707E-15));
#132897=DIRECTION('',(0.456777451208934,-0.203370424080325,-0.866022419268958));
#132898=DIRECTION('center_axis',(-0.406737508253126,-0.913545072438874,
-1.64037033628669E-6));
#132899=DIRECTION('ref_axis',(0.791196542248508,-0.352263396508728,-0.499918524375862));
#132900=DIRECTION('',(0.913545457642606,-0.406736643075789,-2.71158415259707E-15));
#132901=DIRECTION('center_axis',(-0.406735778209486,-0.913545842703931,
-1.63977751199268E-6));
#132902=DIRECTION('ref_axis',(0.791169811719898,-0.352251495066249,0.499969212298812));
#132903=DIRECTION('',(0.456777308164306,-0.203370360392779,0.866022509672746));
#132904=DIRECTION('',(0.913545457642606,-0.406736643075789,-2.71158415259707E-15));
#132905=DIRECTION('center_axis',(-6.89206998773264E-18,-7.02647749501056E-15,
1.));
#132906=DIRECTION('ref_axis',(0.,-1.,-7.02647749501056E-15));
#132907=DIRECTION('',(0.951056516295158,-0.309016994374935,-2.16474620847869E-15));
#132908=DIRECTION('center_axis',(6.89206998773264E-18,7.02647749501056E-15,
-1.));
#132909=DIRECTION('ref_axis',(-6.90292267790937E-12,-1.,-7.02647749501061E-15));
#132910=DIRECTION('',(-0.951056516295158,0.309016994374935,2.16474620847869E-15));
#132911=DIRECTION('center_axis',(-6.89206998773264E-18,-7.02647749501056E-15,
1.));
#132912=DIRECTION('ref_axis',(1.91373385038743E-35,-1.,-7.02647749501056E-15));
#132913=DIRECTION('center_axis',(-0.309016994374935,-0.951056516295158,
-6.6847069749837E-15));
#132914=DIRECTION('ref_axis',(6.89206998773277E-18,7.02647749501056E-15,
-1.));
#132915=DIRECTION('center_axis',(-0.309016994374942,-0.951056516295155,
2.52244012481594E-14));
#132916=DIRECTION('ref_axis',(0.831842966947875,-0.270282164134165,0.484752338921958));
#132917=DIRECTION('',(-0.503988348013123,0.163755740941358,-0.84804469361924));
#132918=DIRECTION('',(0.951056516295158,-0.309016994374935,-2.16474620847869E-15));
#132919=DIRECTION('',(-0.503987849404009,0.163755578933409,0.848045021223111));
#132920=DIRECTION('center_axis',(-0.309016994374912,-0.951056516295165,
4.46596058560273E-14));
#132921=DIRECTION('ref_axis',(0.831841183439677,-0.270281584637229,-0.484755722544527));
#132922=DIRECTION('',(-0.951056516295158,0.309016994374935,2.02392930158878E-15));
#132923=DIRECTION('',(-0.475533025522877,0.154510046201611,-0.866022509672719));
#132924=DIRECTION('center_axis',(0.309017894868202,0.951056223705274,-1.6399888374375E-6));
#132925=DIRECTION('ref_axis',(0.823683738650715,-0.267631070329656,0.499918702267262));
#132926=DIRECTION('',(-0.951056516295158,0.309016994374935,2.02392930158878E-15));
#132927=DIRECTION('center_axis',(0.309016093795519,0.951056808909262,-1.64014404180921E-6));
#132928=DIRECTION('ref_axis',(0.823656109178864,-0.26762209273534,-0.499969028333049));
#132929=DIRECTION('',(-0.475533174441005,0.154510094588011,0.866022419268961));
#132930=DIRECTION('',(-0.951056516295158,0.309016994374935,2.02392930158878E-15));
#132931=DIRECTION('center_axis',(-0.309016994374935,-0.951056516295158,
-6.6847069749837E-15));
#132932=DIRECTION('ref_axis',(6.89206998773277E-18,7.02647749501056E-15,
-1.));
#132933=DIRECTION('center_axis',(0.309016994374906,0.951056516295167,-2.55000835876527E-14));
#132934=DIRECTION('ref_axis',(0.831841183424368,-0.27028158463224,-0.484755722573579));
#132935=DIRECTION('',(0.503987849404013,-0.163755578933417,-0.848045021223107));
#132936=DIRECTION('',(-0.951056516295158,0.309016994374935,2.16474620847869E-15));
#132937=DIRECTION('',(0.503988348013109,-0.163755740941346,0.84804469361925));
#132938=DIRECTION('center_axis',(0.30901699437495,0.951056516295153,-1.10270606562971E-14));
#132939=DIRECTION('ref_axis',(0.831842966967129,-0.270282164140436,0.484752338885422));
#132940=DIRECTION('',(0.951056516295158,-0.309016994374935,-2.02392930158878E-15));
#132941=DIRECTION('',(0.475533174441021,-0.154510094588014,-0.866022419268952));
#132942=DIRECTION('center_axis',(-0.309017895077545,-0.951056223637253,
-1.64037043268108E-6));
#132943=DIRECTION('ref_axis',(0.823683836308317,-0.267631102060807,-0.499918524375855));
#132944=DIRECTION('',(0.951056516295158,-0.309016994374935,-2.02392930158878E-15));
#132945=DIRECTION('center_axis',(-0.309016093996576,-0.951056808843936,
-1.63977750631261E-6));
#132946=DIRECTION('ref_axis',(0.823656008174437,-0.267622059917255,0.499969212295914));
#132947=DIRECTION('',(0.475533025522831,-0.154510046201605,0.866022509672745));
#132948=DIRECTION('',(0.951056516295158,-0.309016994374935,-2.02392930158878E-15));
#132949=DIRECTION('center_axis',(-3.07718727278846E-18,-7.01224015889347E-15,
1.));
#132950=DIRECTION('ref_axis',(0.,-1.,-7.01224015889347E-15));
#132951=DIRECTION('',(0.978147600733808,-0.207911690817747,-1.45491676450776E-15));
#132952=DIRECTION('center_axis',(3.07718727278846E-18,7.01224015889347E-15,
-1.));
#132953=DIRECTION('ref_axis',(2.25419682919892E-12,-1.,-7.01224015889347E-15));
#132954=DIRECTION('',(-0.978147600733808,0.207911690817747,1.45491676450776E-15));
#132955=DIRECTION('center_axis',(-3.07718727278846E-18,-7.01224015889347E-15,
1.));
#132956=DIRECTION('ref_axis',(9.94952222982948E-36,-1.,-7.01224015889347E-15));
#132957=DIRECTION('center_axis',(-0.207911690817747,-0.978147600733808,
-6.85964567039976E-15));
#132958=DIRECTION('ref_axis',(3.07718727278847E-18,7.01224015889347E-15,
-1.));
#132959=DIRECTION('center_axis',(-0.207911690817745,-0.978147600733809,
-2.7567651637332E-15));
#132960=DIRECTION('ref_axis',(0.855538223402208,-0.181850263143641,0.484752338924096));
#132961=DIRECTION('',(-0.518344583061391,0.11017754233581,-0.848044693619241));
#132962=DIRECTION('',(0.978147600733808,-0.207911690817747,-1.45491676450776E-15));
#132963=DIRECTION('',(-0.518344070249268,0.110177433334218,0.848045021223111));
#132964=DIRECTION('center_axis',(-0.207911690817745,-0.978147600733809,
-7.09867191847369E-15));
#132965=DIRECTION('ref_axis',(0.855536389092356,-0.18184987324904,-0.484755722542933));
#132966=DIRECTION('',(-0.978147600733808,0.207911690817747,1.31409985761785E-15));
#132967=DIRECTION('',(-0.489078703542046,0.103956887610932,-0.866022509672745));
#132968=DIRECTION('center_axis',(0.207912616962018,0.978147403873933,-1.63998885026162E-6));
#132969=DIRECTION('ref_axis',(0.847146577451534,-0.180066563904072,0.499918702266611));
#132970=DIRECTION('',(-0.978147600733808,0.207911690817747,1.31409985761785E-15));
#132971=DIRECTION('center_axis',(0.207910764585284,0.978147797608763,-1.6401440529113E-6));
#132972=DIRECTION('ref_axis',(0.847118160921299,-0.18006052355587,-0.499969028334858));
#132973=DIRECTION('',(-0.489078856702219,0.103956920166105,0.86602241926894));
#132974=DIRECTION('',(-0.978147600733808,0.207911690817747,1.31409985761785E-15));
#132975=DIRECTION('center_axis',(-0.207911690817747,-0.978147600733808,
-6.85964567039976E-15));
#132976=DIRECTION('ref_axis',(3.07718727278847E-18,7.01224015889347E-15,
-1.));
#132977=DIRECTION('center_axis',(0.20791169081776,0.978147600733805,3.47352489950765E-14));
#132978=DIRECTION('ref_axis',(0.855536389075249,-0.181849873245405,-0.484755722574488));
#132979=DIRECTION('',(0.518344070249258,-0.110177433334215,-0.848045021223117));
#132980=DIRECTION('',(-0.978147600733808,0.207911690817747,1.45491676450776E-15));
#132981=DIRECTION('',(0.518344583061387,-0.110177542335809,0.848044693619244));
#132982=DIRECTION('center_axis',(0.207911690817735,0.978147600733811,2.13649300215755E-14));
#132983=DIRECTION('ref_axis',(0.855538223422491,-0.181850263147953,0.484752338886681));
#132984=DIRECTION('',(0.978147600733808,-0.207911690817747,-1.31409985761785E-15));
#132985=DIRECTION('',(0.489078856702207,-0.103956920166111,-0.866022419268947));
#132986=DIRECTION('center_axis',(-0.207912617177289,-0.978147403828175,
-1.64037042596789E-6));
#132987=DIRECTION('ref_axis',(0.847146677889706,-0.180066585253107,-0.499918524377443));
#132988=DIRECTION('',(0.978147600733808,-0.207911690817747,-1.31409985761785E-15));
#132989=DIRECTION('center_axis',(-0.207910764792045,-0.978147797564815,
-1.6397775832553E-6));
#132990=DIRECTION('ref_axis',(0.847118057040066,-0.180060501475481,0.499969212297179));
#132991=DIRECTION('',(0.489078703542049,-0.103956887610926,0.866022509672744));
#132992=DIRECTION('',(0.978147600733808,-0.207911690817747,-1.31409985761785E-15));
#132993=DIRECTION('center_axis',(-7.71409749858844E-19,-6.99768205256557E-15,
1.));
#132994=DIRECTION('ref_axis',(0.,-1.,-6.99768205256557E-15));
#132995=DIRECTION('',(0.994521895368275,-0.10452846326764,-7.3068976750369E-16));
#132996=DIRECTION('center_axis',(7.71409749858844E-19,6.99768205256557E-15,
-1.));
#132997=DIRECTION('ref_axis',(2.20623519453511E-12,-1.,-6.99768205256557E-15));
#132998=DIRECTION('',(-0.994521895368275,0.10452846326764,7.3068976750369E-16));
#132999=DIRECTION('center_axis',(-7.71409749858844E-19,-6.99768205256557E-15,
1.));
#133000=DIRECTION('ref_axis',(2.59899164973018E-36,-1.,-6.99768205256557E-15));
#133001=DIRECTION('center_axis',(-0.10452846326764,-0.994521895368275,-6.95942865237777E-15));
#133002=DIRECTION('ref_axis',(7.71409749858829E-19,6.99768205256557E-15,
-1.));
#133003=DIRECTION('center_axis',(-0.10452846326763,-0.994521895368276,-2.52933203772504E-14));
#133004=DIRECTION('ref_axis',(0.869860024050779,-0.0914259726160321,0.484752338921217));
#133005=DIRECTION('',(-0.527021726387077,0.0553922155203068,-0.848044693619232));
#133006=DIRECTION('',(0.994521895368275,-0.10452846326764,-7.3068976750369E-16));
#133007=DIRECTION('',(-0.527021204990414,0.0553921607192977,0.848045021223107));
#133008=DIRECTION('center_axis',(-0.104528463267641,-0.994521895368275,
-4.78988056634914E-15));
#133009=DIRECTION('ref_axis',(0.86985815903191,-0.091425776594645,-0.484755722544544));
#133010=DIRECTION('',(-0.994521895368275,0.10452846326764,5.89872860613779E-16));
#133011=DIRECTION('',(-0.497265932938972,0.0522647556052191,-0.866022509672734));
#133012=DIRECTION('center_axis',(0.104529404915855,0.994521796395256,-1.63998886015915E-6));
#133013=DIRECTION('ref_axis',(0.861327901070753,-0.0905292105226655,0.499918702269873));
#133014=DIRECTION('',(-0.994521895368275,0.10452846326764,5.89872860613779E-16));
#133015=DIRECTION('center_axis',(0.104527521530137,0.994521994347072,-1.64014407012473E-6));
#133016=DIRECTION('ref_axis',(0.8612990088216,-0.0905261736004439,-0.499969028336947));
#133017=DIRECTION('',(-0.497266088662992,0.0522647719724638,0.866022419268968));
#133018=DIRECTION('',(-0.994521895368275,0.10452846326764,5.89872860613779E-16));
#133019=DIRECTION('center_axis',(-0.10452846326764,-0.994521895368275,-6.95942865237777E-15));
#133020=DIRECTION('ref_axis',(7.71409749858829E-19,6.99768205256557E-15,
-1.));
#133021=DIRECTION('center_axis',(0.104528463267642,0.994521895368275,1.39905864007942E-14));
#133022=DIRECTION('ref_axis',(0.869858159014795,-0.0914257765928421,-0.484755722575595));
#133023=DIRECTION('',(0.527021204990409,-0.0553921607193002,-0.84804502122311));
#133024=DIRECTION('',(-0.994521895368275,0.10452846326764,7.3068976750369E-16));
#133025=DIRECTION('',(0.527021726387067,-0.0553922155203071,0.848044693619238));
#133026=DIRECTION('center_axis',(0.104528463267631,0.994521895368276,2.0158845262292E-14));
#133027=DIRECTION('ref_axis',(0.869860024068846,-0.0914259726179291,0.48475233888844));
#133028=DIRECTION('',(0.994521895368275,-0.10452846326764,-5.89872860613779E-16));
#133029=DIRECTION('',(0.497266088663057,-0.0522647719724677,-0.86602241926893));
#133030=DIRECTION('center_axis',(-0.104529405134737,-0.99452179637225,-1.64037044313809E-6));
#133031=DIRECTION('ref_axis',(0.861328003191411,-0.0905292212562206,-0.499918524378763));
#133032=DIRECTION('',(0.994521895368275,-0.10452846326764,-5.89872860613779E-16));
#133033=DIRECTION('center_axis',(-0.104527521740345,-0.994521994324979,
-1.63977763949909E-6));
#133034=DIRECTION('ref_axis',(0.861298903203584,-0.0905261624997945,0.499969212295481));
#133035=DIRECTION('',(0.497265932938949,-0.0522647556052211,0.866022509672747));
#133036=DIRECTION('',(0.994521895368275,-0.10452846326764,-5.89872860613779E-16));
#133037=DIRECTION('center_axis',(0.994521895368273,0.104528463267654,7.29146948004067E-16));
#133038=DIRECTION('ref_axis',(0.104528463267654,-0.994521895368273,-7.42349998278334E-15));
#133039=DIRECTION('center_axis',(-0.994521895368273,-0.104528463267654,
-7.29146948004067E-16));
#133040=DIRECTION('ref_axis',(-0.104528463267654,0.994521895368273,7.42349998278332E-15));
#133041=DIRECTION('center_axis',(0.978147600733806,0.20791169081776,1.44876238996227E-15));
#133042=DIRECTION('ref_axis',(0.20791169081776,-0.978147600733805,-7.42349998278335E-15));
#133043=DIRECTION('center_axis',(-0.978147600733806,-0.20791169081776,-1.44876238996227E-15));
#133044=DIRECTION('ref_axis',(-0.20791169081776,0.978147600733805,7.42349998278332E-15));
#133045=DIRECTION('center_axis',(0.951056516295153,0.309016994374948,2.15096206850332E-15));
#133046=DIRECTION('ref_axis',(0.309016994374948,-0.951056516295153,-7.42349998278335E-15));
#133047=DIRECTION('center_axis',(-0.951056516295153,-0.309016994374948,
-2.15096206850332E-15));
#133048=DIRECTION('ref_axis',(-0.309016994374948,0.951056516295153,7.42349998278333E-15));
#133049=DIRECTION('center_axis',(0.913545457642601,0.406736643075801,2.82805253700437E-15));
#133050=DIRECTION('ref_axis',(0.406736643075801,-0.913545457642601,-7.42349998278338E-15));
#133051=DIRECTION('center_axis',(-0.913545457642601,-0.406736643075801,
-2.82805253700437E-15));
#133052=DIRECTION('ref_axis',(-0.406736643075801,0.9135454576426,7.42349998278333E-15));
#133053=DIRECTION('center_axis',(0.866025403784438,0.500000000000001,3.47261545060224E-15));
#133054=DIRECTION('ref_axis',(0.500000000000001,-0.866025403784438,-4.94899998852227E-15));
#133055=DIRECTION('center_axis',(-0.866025403784438,-0.500000000000001,
-3.47261545060224E-15));
#133056=DIRECTION('ref_axis',(-0.500000000000001,0.866025403784438,4.94899998852221E-15));
#133057=DIRECTION('center_axis',(0.809016994374947,0.587785252292474,4.0775888431321E-15));
#133058=DIRECTION('ref_axis',(0.587785252292474,-0.809016994374947,-4.9489999885223E-15));
#133059=DIRECTION('center_axis',(-0.809016994374947,-0.587785252292474,
-4.0775888431321E-15));
#133060=DIRECTION('ref_axis',(-0.587785252292474,0.809016994374947,4.94899998852222E-15));
#133061=DIRECTION('center_axis',(0.743144825477393,0.669130606358859,4.63634449950655E-15));
#133062=DIRECTION('ref_axis',(0.669130606358859,-0.743144825477393,-4.94899998852211E-15));
#133063=DIRECTION('center_axis',(-0.743144825477393,-0.669130606358859,
-4.63634449950655E-15));
#133064=DIRECTION('ref_axis',(-0.669130606358859,0.743144825477393,4.94899998852222E-15));
#133065=DIRECTION('center_axis',(0.669130606358857,0.743144825477395,5.14276057582724E-15));
#133066=DIRECTION('ref_axis',(0.743144825477396,-0.669130606358857,-4.94899998852226E-15));
#133067=DIRECTION('center_axis',(-0.669130606358857,-0.743144825477395,
-5.14276057582724E-15));
#133068=DIRECTION('ref_axis',(-0.743144825477395,0.669130606358857,4.94899998852221E-15));
#133069=DIRECTION('center_axis',(0.587785252292471,0.809016994374949,5.59128867158761E-15));
#133070=DIRECTION('ref_axis',(0.809016994374949,-0.587785252292471,-4.94899998852211E-15));
#133071=DIRECTION('center_axis',(-0.587785252292471,-0.809016994374949,
-5.59128867158761E-15));
#133072=DIRECTION('ref_axis',(-0.809016994374949,0.587785252292472,4.94899998852222E-15));
#133073=DIRECTION('center_axis',(0.499999999999998,0.86602540378444,5.97701461910997E-15));
#133074=DIRECTION('ref_axis',(0.86602540378444,-0.499999999999998,-2.47449999426116E-15));
#133075=DIRECTION('center_axis',(-0.499999999999998,-0.86602540378444,-5.97701461910997E-15));
#133076=DIRECTION('ref_axis',(-0.86602540378444,0.499999999999998,2.47449999426111E-15));
#133077=DIRECTION('center_axis',(0.406736643075798,0.913545457642602,6.29571232419492E-15));
#133078=DIRECTION('ref_axis',(0.913545457642602,-0.406736643075798,-2.474499994261E-15));
#133079=DIRECTION('center_axis',(-0.406736643075798,-0.913545457642602,
-6.29571232419492E-15));
#133080=DIRECTION('ref_axis',(-0.913545457642602,0.406736643075798,2.47449999426111E-15));
#133081=DIRECTION('center_axis',(0.309016994374945,0.951056516295155,6.54389006809377E-15));
#133082=DIRECTION('ref_axis',(0.951056516295154,-0.309016994374945,-2.47449999426112E-15));
#133083=DIRECTION('center_axis',(-0.309016994374945,-0.951056516295155,
-6.54389006809377E-15));
#133084=DIRECTION('ref_axis',(-0.951056516295154,0.309016994374945,2.47449999426111E-15));
#133085=DIRECTION('center_axis',(0.207911690817756,0.978147600733806,6.71882876350984E-15));
#133086=DIRECTION('ref_axis',(0.978147600733806,-0.207911690817756,-2.47449999426122E-15));
#133087=DIRECTION('center_axis',(-0.207911690817756,-0.978147600733806,
-6.71882876350984E-15));
#133088=DIRECTION('ref_axis',(-0.978147600733806,0.207911690817756,2.47449999426111E-15));
#133089=DIRECTION('center_axis',(0.10452846326765,0.994521895368274,6.81861174548786E-15));
#133090=DIRECTION('ref_axis',(0.994521895368274,-0.10452846326765,-7.6256220630635E-29));
#133091=DIRECTION('center_axis',(-0.10452846326765,-0.994521895368274,-6.81861174548786E-15));
#133092=DIRECTION('ref_axis',(-0.994521895368274,0.10452846326765,5.35058014197221E-32));
#133093=DIRECTION('center_axis',(-3.49148133884313E-15,1.,6.84214577079636E-15));
#133094=DIRECTION('ref_axis',(1.,3.49148133884313E-15,2.38892242763799E-29));
#133095=DIRECTION('center_axis',(3.49148133884313E-15,-1.,-6.84214577079636E-15));
#133096=DIRECTION('ref_axis',(-1.,-3.49148133884313E-15,3.67140197653102E-43));
#133097=DIRECTION('center_axis',(-0.104528463267657,0.994521895368273,6.78917299572924E-15));
#133098=DIRECTION('ref_axis',(0.994521895368273,0.104528463267657,1.21818699066432E-28));
#133099=DIRECTION('center_axis',(0.104528463267657,-0.994521895368273,-6.78917299572924E-15));
#133100=DIRECTION('ref_axis',(-0.994521895368273,-0.104528463267657,-1.19282195192603E-32));
#133101=DIRECTION('center_axis',(-0.207911690817763,0.978147600733805,6.66027380109541E-15));
#133102=DIRECTION('ref_axis',(0.978147600733805,0.207911690817763,2.47449999426098E-15));
#133103=DIRECTION('center_axis',(0.207911690817763,-0.978147600733805,-6.66027380109541E-15));
#133104=DIRECTION('ref_axis',(-0.978147600733805,-0.207911690817763,-2.47449999426111E-15));
#133105=DIRECTION('center_axis',(-0.309016994374951,0.951056516295152,6.45686043344516E-15));
#133106=DIRECTION('ref_axis',(0.951056516295152,0.309016994374951,2.47449999426116E-15));
#133107=DIRECTION('center_axis',(0.309016994374951,-0.951056516295152,-6.45686043344516E-15));
#133108=DIRECTION('ref_axis',(-0.951056516295152,-0.309016994374951,-2.47449999426111E-15));
#133109=DIRECTION('center_axis',(-0.406736643075804,0.913545457642599,6.18116153220146E-15));
#133110=DIRECTION('ref_axis',(0.913545457642599,0.406736643075804,2.47449999426104E-15));
#133111=DIRECTION('center_axis',(0.406736643075804,-0.913545457642599,-6.18116153220146E-15));
#133112=DIRECTION('ref_axis',(-0.913545457642599,-0.406736643075804,-2.47449999426111E-15));
#133113=DIRECTION('center_axis',(-0.500000000000004,0.866025403784436,5.83619771222003E-15));
#133114=DIRECTION('ref_axis',(0.866025403784436,0.500000000000004,2.47449999426119E-15));
#133115=DIRECTION('center_axis',(0.500000000000004,-0.866025403784436,-5.83619771222003E-15));
#133116=DIRECTION('ref_axis',(-0.866025403784436,-0.500000000000004,-2.47449999426111E-15));
#133117=DIRECTION('center_axis',(-0.587785252292477,0.809016994374945,5.42574846930092E-15));
#133118=DIRECTION('ref_axis',(0.809016994374945,0.587785252292477,4.94899998852215E-15));
#133119=DIRECTION('center_axis',(0.587785252292477,-0.809016994374945,-5.42574846930092E-15));
#133120=DIRECTION('ref_axis',(-0.809016994374945,-0.587785252292477,-4.94899998852222E-15));
#133121=DIRECTION('center_axis',(-0.669130606358862,0.743144825477391,4.95431077124156E-15));
#133122=DIRECTION('ref_axis',(0.743144825477391,0.669130606358862,4.9489999885223E-15));
#133123=DIRECTION('center_axis',(0.669130606358862,-0.743144825477391,-4.95431077124156E-15));
#133124=DIRECTION('ref_axis',(-0.743144825477391,-0.669130606358862,-4.94899998852222E-15));
#133125=DIRECTION('center_axis',(-0.743144825477398,0.669130606358854,4.42704978811658E-15));
#133126=DIRECTION('ref_axis',(0.669130606358854,0.743144825477398,4.94899998852214E-15));
#133127=DIRECTION('center_axis',(0.743144825477398,-0.669130606358854,-4.42704978811658E-15));
#133128=DIRECTION('ref_axis',(-0.669130606358854,-0.743144825477398,-4.94899998852222E-15));
#133129=DIRECTION('center_axis',(-0.809016994374951,0.587785252292469,3.84974230159355E-15));
#133130=DIRECTION('ref_axis',(0.587785252292469,0.80901699437495,4.94899998852232E-15));
#133131=DIRECTION('center_axis',(0.809016994374951,-0.587785252292469,-3.84974230159355E-15));
#133132=DIRECTION('ref_axis',(-0.587785252292469,-0.809016994374951,-4.94899998852222E-15));
#133133=DIRECTION('center_axis',(-0.866025403784442,0.499999999999995,3.22871341330418E-15));
#133134=DIRECTION('ref_axis',(0.499999999999995,0.866025403784442,4.94899998852218E-15));
#133135=DIRECTION('center_axis',(0.866025403784442,-0.499999999999995,-3.22871341330418E-15));
#133136=DIRECTION('ref_axis',(-0.499999999999995,-0.866025403784442,-4.94899998852222E-15));
#133137=DIRECTION('center_axis',(-0.913545457642603,0.406736643075795,2.57076724570721E-15));
#133138=DIRECTION('ref_axis',(0.406736643075795,0.913545457642603,7.42349998278324E-15));
#133139=DIRECTION('center_axis',(0.913545457642603,-0.406736643075795,-2.57076724570721E-15));
#133140=DIRECTION('ref_axis',(-0.406736643075795,-0.913545457642603,-7.42349998278332E-15));
#133141=DIRECTION('center_axis',(-0.951056516295156,0.309016994374942,1.88311239469892E-15));
#133142=DIRECTION('ref_axis',(0.309016994374942,0.951056516295155,7.42349998278336E-15));
#133143=DIRECTION('center_axis',(0.951056516295156,-0.309016994374942,-1.88311239469892E-15));
#133144=DIRECTION('ref_axis',(-0.309016994374942,-0.951056516295156,-7.42349998278332E-15));
#133145=DIRECTION('center_axis',(-0.978147600733807,0.207911690817753,1.17328295072799E-15));
#133146=DIRECTION('ref_axis',(0.207911690817753,0.978147600733807,7.42349998278336E-15));
#133147=DIRECTION('center_axis',(0.978147600733807,-0.207911690817753,-1.17328295072799E-15));
#133148=DIRECTION('ref_axis',(-0.207911690817753,-0.978147600733807,-7.42349998278332E-15));
#133149=DIRECTION('center_axis',(-0.994521895368274,0.104528463267647,4.49055953723918E-16));
#133150=DIRECTION('ref_axis',(0.104528463267647,0.994521895368274,7.42349998278331E-15));
#133151=DIRECTION('center_axis',(0.994521895368274,-0.104528463267647,-4.49055953723918E-16));
#133152=DIRECTION('ref_axis',(-0.104528463267647,-0.994521895368274,-7.42349998278332E-15));
#133153=DIRECTION('center_axis',(-1.,1.96663841039893E-30,-2.81633813779821E-16));
#133154=DIRECTION('ref_axis',(2.81633813779821E-16,6.97886326506453E-15,
-1.));
#133155=DIRECTION('center_axis',(1.,-1.96663841039893E-30,2.81633813779821E-16));
#133156=DIRECTION('ref_axis',(-2.81633813779821E-16,-6.97886326506453E-15,
1.));
#133157=DIRECTION('center_axis',(-0.994521895368273,-0.104528463267661,
-1.01078076178394E-15));
#133158=DIRECTION('ref_axis',(-0.104528463267661,0.994521895368273,7.42349998278334E-15));
#133159=DIRECTION('center_axis',(0.994521895368273,0.104528463267661,1.01078076178394E-15));
#133160=DIRECTION('ref_axis',(0.104528463267661,-0.994521895368273,-7.42349998278332E-15));
#133161=DIRECTION('center_axis',(-0.978147600733804,-0.207911690817766,
-1.73039620374214E-15));
#133162=DIRECTION('ref_axis',(-0.207911690817766,0.978147600733804,7.42349998278333E-15));
#133163=DIRECTION('center_axis',(0.978147600733804,0.207911690817766,1.73039620374214E-15));
#133164=DIRECTION('ref_axis',(0.207911690817766,-0.978147600733804,-7.42349998278332E-15));
#133165=DIRECTION('center_axis',(-0.951056516295151,-0.309016994374955,
-2.43259588228318E-15));
#133166=DIRECTION('ref_axis',(-0.309016994374955,0.951056516295151,7.42349998278333E-15));
#133167=DIRECTION('center_axis',(0.951056516295151,0.309016994374955,2.43259588228318E-15));
#133168=DIRECTION('ref_axis',(0.309016994374954,-0.951056516295151,-7.42349998278332E-15));
#133169=DIRECTION('center_axis',(-0.913545457642598,-0.406736643075807,
-3.10968635078423E-15));
#133170=DIRECTION('ref_axis',(-0.406736643075807,0.913545457642598,7.42349998278337E-15));
#133171=DIRECTION('center_axis',(0.913545457642598,0.406736643075807,3.10968635078423E-15));
#133172=DIRECTION('ref_axis',(0.406736643075807,-0.913545457642598,-7.42349998278332E-15));
#133173=DIRECTION('center_axis',(-0.866025403784435,-0.500000000000007,
-3.7542492643821E-15));
#133174=DIRECTION('ref_axis',(-0.500000000000007,0.866025403784435,4.94899998852224E-15));
#133175=DIRECTION('center_axis',(0.866025403784435,0.500000000000007,3.7542492643821E-15));
#133176=DIRECTION('ref_axis',(0.500000000000007,-0.866025403784435,-4.94899998852222E-15));
#133177=DIRECTION('center_axis',(-0.809016994374943,-0.58778525229248,-4.35922265691196E-15));
#133178=DIRECTION('ref_axis',(-0.58778525229248,0.809016994374943,4.94899998852228E-15));
#133179=DIRECTION('center_axis',(0.809016994374943,0.58778525229248,4.35922265691196E-15));
#133180=DIRECTION('ref_axis',(0.58778525229248,-0.809016994374943,-4.94899998852221E-15));
#133181=DIRECTION('center_axis',(-0.743144825477389,-0.669130606358864,
-4.91797831328641E-15));
#133182=DIRECTION('ref_axis',(-0.669130606358864,0.743144825477389,4.94899998852235E-15));
#133183=DIRECTION('center_axis',(0.743144825477389,0.669130606358864,4.91797831328641E-15));
#133184=DIRECTION('ref_axis',(0.669130606358864,-0.743144825477388,-4.94899998852221E-15));
#133185=DIRECTION('center_axis',(-0.669130606358852,-0.7431448254774,-5.42439438960709E-15));
#133186=DIRECTION('ref_axis',(-0.7431448254774,0.669130606358852,4.94899998852223E-15));
#133187=DIRECTION('center_axis',(0.669130606358852,0.7431448254774,5.42439438960709E-15));
#133188=DIRECTION('ref_axis',(0.7431448254774,-0.669130606358852,-4.94899998852222E-15));
#133189=DIRECTION('center_axis',(-0.587785252292466,-0.809016994374953,
-5.87292248536745E-15));
#133190=DIRECTION('ref_axis',(-0.809016994374953,0.587785252292466,4.94899998852237E-15));
#133191=DIRECTION('center_axis',(0.587785252292466,0.809016994374953,5.87292248536745E-15));
#133192=DIRECTION('ref_axis',(0.809016994374953,-0.587785252292466,-4.94899998852222E-15));
#133193=DIRECTION('center_axis',(-0.499999999999992,-0.866025403784443,
-6.25864843288981E-15));
#133194=DIRECTION('ref_axis',(-0.866025403784443,0.499999999999992,2.47449999426112E-15));
#133195=DIRECTION('center_axis',(0.499999999999992,0.866025403784443,6.25864843288981E-15));
#133196=DIRECTION('ref_axis',(0.866025403784443,-0.499999999999992,-2.47449999426111E-15));
#133197=DIRECTION('center_axis',(-0.406736643075792,-0.913545457642605,
-6.57734613797476E-15));
#133198=DIRECTION('ref_axis',(-0.913545457642605,0.406736643075792,2.47449999426124E-15));
#133199=DIRECTION('center_axis',(0.406736643075792,0.913545457642605,6.57734613797476E-15));
#133200=DIRECTION('ref_axis',(0.913545457642605,-0.406736643075792,-2.47449999426111E-15));
#133201=DIRECTION('center_axis',(-0.309016994374938,-0.951056516295157,
-6.82552388187361E-15));
#133202=DIRECTION('ref_axis',(-0.951056516295157,0.309016994374938,2.47449999426107E-15));
#133203=DIRECTION('center_axis',(0.309016994374938,0.951056516295157,6.82552388187361E-15));
#133204=DIRECTION('ref_axis',(0.951056516295157,-0.309016994374938,-2.47449999426111E-15));
#133205=DIRECTION('center_axis',(-0.207911690817749,-0.978147600733808,
-7.00046257728967E-15));
#133206=DIRECTION('ref_axis',(-0.978147600733808,0.207911690817749,2.47449999426117E-15));
#133207=DIRECTION('center_axis',(0.207911690817749,0.978147600733808,7.00046257728967E-15));
#133208=DIRECTION('ref_axis',(0.978147600733808,-0.207911690817749,-2.47449999426111E-15));
#133209=DIRECTION('center_axis',(-0.104528463267644,-0.994521895368275,
-7.10024555926768E-15));
#133210=DIRECTION('ref_axis',(-0.994521895368274,0.104528463267644,3.50875041575624E-29));
#133211=DIRECTION('center_axis',(0.104528463267644,0.994521895368275,7.10024555926768E-15));
#133212=DIRECTION('ref_axis',(0.994521895368274,-0.104528463267644,-7.58109811812969E-32));
#133213=DIRECTION('center_axis',(1.04744440165294E-14,-1.,-7.12377958457618E-15));
#133214=DIRECTION('ref_axis',(-1.,-1.04744440165294E-14,-7.46176304447382E-29));
#133215=DIRECTION('center_axis',(-1.04744440165294E-14,1.,7.12377958457618E-15));
#133216=DIRECTION('ref_axis',(1.,1.04744440165294E-14,-1.5694542800438E-43));
#133217=DIRECTION('center_axis',(0.104528463267664,-0.994521895368272,-7.07080680950905E-15));
#133218=DIRECTION('ref_axis',(-0.994521895368272,-0.104528463267664,1.05361876330055E-28));
#133219=DIRECTION('center_axis',(-0.104528463267664,0.994521895368272,7.07080680950905E-15));
#133220=DIRECTION('ref_axis',(0.994521895368272,0.104528463267664,-1.29041391784167E-31));
#133221=DIRECTION('center_axis',(0.20791169081777,-0.978147600733803,-6.94190761487522E-15));
#133222=DIRECTION('ref_axis',(-0.978147600733803,-0.20791169081777,-2.47449999426102E-15));
#133223=DIRECTION('center_axis',(-0.20791169081777,0.978147600733803,6.94190761487522E-15));
#133224=DIRECTION('ref_axis',(0.978147600733803,0.20791169081777,2.47449999426111E-15));
#133225=DIRECTION('center_axis',(0.309016994374957,-0.95105651629515,-6.73849424722497E-15));
#133226=DIRECTION('ref_axis',(-0.95105651629515,-0.309016994374957,-2.47449999426121E-15));
#133227=DIRECTION('center_axis',(-0.309016994374957,0.95105651629515,6.73849424722497E-15));
#133228=DIRECTION('ref_axis',(0.95105651629515,0.309016994374957,2.47449999426111E-15));
#133229=DIRECTION('center_axis',(0.40673664307581,-0.913545457642596,-6.46279534598126E-15));
#133230=DIRECTION('ref_axis',(-0.913545457642597,-0.40673664307581,-2.47449999426108E-15));
#133231=DIRECTION('center_axis',(-0.40673664307581,0.913545457642596,6.46279534598126E-15));
#133232=DIRECTION('ref_axis',(0.913545457642596,0.40673664307581,2.47449999426111E-15));
#133233=DIRECTION('center_axis',(0.50000000000001,-0.866025403784433,-6.11783152599983E-15));
#133234=DIRECTION('ref_axis',(-0.866025403784433,-0.50000000000001,-2.47449999426098E-15));
#133235=DIRECTION('center_axis',(-0.50000000000001,0.866025403784433,6.11783152599983E-15));
#133236=DIRECTION('ref_axis',(0.866025403784433,0.50000000000001,2.47449999426111E-15));
#133237=DIRECTION('center_axis',(0.587785252292482,-0.809016994374941,-5.70738228308071E-15));
#133238=DIRECTION('ref_axis',(-0.809016994374941,-0.587785252292482,-4.94899998852218E-15));
#133239=DIRECTION('center_axis',(-0.587785252292482,0.809016994374941,5.70738228308071E-15));
#133240=DIRECTION('ref_axis',(0.809016994374941,0.587785252292482,4.94899998852221E-15));
#133241=DIRECTION('center_axis',(0.669130606358867,-0.743144825477386,-5.23594458502135E-15));
#133242=DIRECTION('ref_axis',(-0.743144825477386,-0.669130606358867,-4.94899998852234E-15));
#133243=DIRECTION('center_axis',(-0.669130606358867,0.743144825477386,5.23594458502135E-15));
#133244=DIRECTION('ref_axis',(0.743144825477386,0.669130606358867,4.94899998852222E-15));
#133245=DIRECTION('center_axis',(0.743144825477402,-0.66913060635885,-4.70868360189637E-15));
#133246=DIRECTION('ref_axis',(-0.66913060635885,-0.743144825477402,-4.94899998852217E-15));
#133247=DIRECTION('center_axis',(-0.743144825477402,0.66913060635885,4.70868360189637E-15));
#133248=DIRECTION('ref_axis',(0.66913060635885,0.743144825477402,4.94899998852222E-15));
#133249=DIRECTION('center_axis',(0.809016994374955,-0.587785252292463,-4.13137611537334E-15));
#133250=DIRECTION('ref_axis',(-0.587785252292463,-0.809016994374955,-4.94899998852209E-15));
#133251=DIRECTION('center_axis',(-0.809016994374955,0.587785252292463,4.13137611537334E-15));
#133252=DIRECTION('ref_axis',(0.587785252292463,0.809016994374955,4.94899998852222E-15));
#133253=DIRECTION('center_axis',(0.866025403784445,-0.499999999999989,-3.51034722708396E-15));
#133254=DIRECTION('ref_axis',(-0.499999999999989,-0.866025403784445,-4.9489999885222E-15));
#133255=DIRECTION('center_axis',(-0.866025403784445,0.499999999999989,3.51034722708396E-15));
#133256=DIRECTION('ref_axis',(0.499999999999989,0.866025403784445,4.94899998852222E-15));
#133257=DIRECTION('center_axis',(0.913545457642606,-0.406736643075789,-2.85240105948698E-15));
#133258=DIRECTION('ref_axis',(-0.406736643075789,-0.913545457642606,-7.42349998278328E-15));
#133259=DIRECTION('center_axis',(-0.913545457642606,0.406736643075789,2.85240105948698E-15));
#133260=DIRECTION('ref_axis',(0.406736643075789,0.913545457642606,7.42349998278333E-15));
#133261=DIRECTION('center_axis',(0.951056516295158,-0.309016994374935,-2.16474620847869E-15));
#133262=DIRECTION('ref_axis',(-0.309016994374935,-0.951056516295158,-7.42349998278338E-15));
#133263=DIRECTION('center_axis',(-0.951056516295158,0.309016994374935,2.16474620847869E-15));
#133264=DIRECTION('ref_axis',(0.309016994374935,0.951056516295158,7.42349998278332E-15));
#133265=DIRECTION('center_axis',(0.978147600733808,-0.207911690817747,-1.45491676450776E-15));
#133266=DIRECTION('ref_axis',(-0.207911690817747,-0.978147600733808,-7.42349998278336E-15));
#133267=DIRECTION('center_axis',(-0.978147600733808,0.207911690817747,1.45491676450776E-15));
#133268=DIRECTION('ref_axis',(0.207911690817747,0.978147600733808,7.42349998278332E-15));
#133269=DIRECTION('center_axis',(0.994521895368275,-0.10452846326764,-7.3068976750369E-16));
#133270=DIRECTION('ref_axis',(-0.10452846326764,-0.994521895368275,-7.42349998278331E-15));
#133271=DIRECTION('center_axis',(-0.994521895368275,0.10452846326764,7.3068976750369E-16));
#133272=DIRECTION('ref_axis',(0.10452846326764,0.994521895368275,7.42349998278333E-15));
#133273=DIRECTION('center_axis',(-0.497265934576059,-0.0522647557772786,
-0.866022508722343));
#133274=DIRECTION('ref_axis',(0.104528463272604,-0.994521895367753,-2.8717186175955E-12));
#133275=DIRECTION('center_axis',(-0.861277224843021,-0.0904936763726118,
-0.500012436348611));
#133276=DIRECTION('ref_axis',(0.49716964624235,0.0532497882929787,-0.866017784402843));
#133277=DIRECTION('center_axis',(0.497265943181924,0.0522647566817827,0.866022503726309));
#133278=DIRECTION('ref_axis',(-0.867207748104374,-7.42381499369421E-15,
0.497946504785143));
#133279=DIRECTION('center_axis',(0.994521895368276,0.104528463267628,7.29918357753749E-16));
#133280=DIRECTION('ref_axis',(0.104528463267628,-0.994521895368276,-6.82961998416064E-15));
#133281=DIRECTION('center_axis',(-0.994521895368273,-0.104528463267654,
-8.69963854893977E-16));
#133282=DIRECTION('ref_axis',(-0.104528463267654,0.994521895368273,6.82961998416066E-15));
#133283=DIRECTION('center_axis',(-0.994521895368276,-0.104528463267629,
6.97861005538628E-16));
#133284=DIRECTION('ref_axis',(-0.104528463267629,0.994521895368276,6.82961998416064E-15));
#133285=DIRECTION('center_axis',(-0.994521895368273,-0.104528463267654,
-8.69963854893977E-16));
#133286=DIRECTION('ref_axis',(-0.104528463267654,0.994521895368273,6.82961998416066E-15));
#133287=DIRECTION('center_axis',(0.994521895368276,0.104528463267628,7.29918357753744E-16));
#133288=DIRECTION('ref_axis',(0.104528463267628,-0.994521895368276,-6.82961998416064E-15));
#133289=DIRECTION('center_axis',(-0.527021232978597,-0.0553921636609822,
0.848045003637587));
#133290=DIRECTION('ref_axis',(-0.849349030019387,7.20117432794764E-15,-0.527831625809903));
#133291=DIRECTION('center_axis',(0.497266077958583,0.0522647708474123,-0.866022425483287));
#133292=DIRECTION('ref_axis',(0.867207670398076,-6.88055504554487E-15,0.497946640115929));
#133293=DIRECTION('center_axis',(0.527021202611631,0.055392182212892,-0.848045021297504));
#133294=DIRECTION('ref_axis',(0.842941044395307,0.0929299148191017,0.529919264233208));
#133295=DIRECTION('center_axis',(-0.527021177161361,-0.0553921577943543,
0.84804503870864));
#133296=DIRECTION('ref_axis',(-0.84934906486751,6.64538535710706E-15,-0.527831569734783));
#133297=DIRECTION('center_axis',(0.497266090635357,0.0522647827543777,-0.866022417485752));
#133298=DIRECTION('ref_axis',(0.860793892490753,0.0950466972103146,0.500000000000028));
#133299=DIRECTION('center_axis',(0.861296695145007,0.0904912830031523,-0.499979330205491));
#133300=DIRECTION('ref_axis',(0.49734089486934,0.0513033470000485,0.866036951219264));
#133301=DIRECTION('center_axis',(-0.104769627595161,0.994496518411991,1.52498774835248E-16));
#133302=DIRECTION('ref_axis',(0.994496518411991,0.104769627595161,7.18497231411654E-31));
#133303=DIRECTION('center_axis',(-0.994521895368273,-0.104528463267654,
-8.69963854893977E-16));
#133304=DIRECTION('ref_axis',(-0.104528463267654,0.994521895368273,6.82961998416066E-15));
#133305=DIRECTION('center_axis',(0.994521895368276,0.104528463267627,7.29918357753739E-16));
#133306=DIRECTION('ref_axis',(0.104528463267627,-0.994521895368276,-6.82961998416064E-15));
#133307=DIRECTION('center_axis',(-7.71409749859041E-19,-6.96824330280696E-15,
1.));
#133308=DIRECTION('ref_axis',(0.,-1.,-6.96738351343764E-15));
#133309=DIRECTION('center_axis',(-0.104287292793436,0.994547213842468,6.94488607545882E-15));
#133310=DIRECTION('ref_axis',(0.994547213842468,0.104287292793436,3.36172022659011E-29));
#133311=DIRECTION('center_axis',(0.52702169399903,0.0553922121162167,0.848044713969296));
#133312=DIRECTION('ref_axis',(-0.849348742192381,-6.70998093352327E-15,
0.527832088960325));
#133313=DIRECTION('center_axis',(0.52702117716142,0.055392157794407,-0.8480450387086));
#133314=DIRECTION('ref_axis',(0.849349064867473,-6.23548807247744E-15,0.527831569734843));
#133315=DIRECTION('center_axis',(0.52702172906978,0.0553921904544422,0.848044693589293));
#133316=DIRECTION('ref_axis',(-0.842916495802168,-0.0931523188070211,0.529919264233212));
#133317=DIRECTION('center_axis',(0.527021758969982,0.0553922189448927,0.848044673146732));
#133318=DIRECTION('ref_axis',(-0.849348701629304,-6.73646265345537E-15,
0.527832154231452));
#133319=DIRECTION('center_axis',(-0.527021202762452,-0.0553921822924323,
0.84804502119858));
#133320=DIRECTION('ref_axis',(0.843841975851294,0.0843581245990787,0.529919264233252));
#133321=DIRECTION('center_axis',(0.527021232978612,0.0553921636609838,-0.848045003637577));
#133322=DIRECTION('ref_axis',(0.849349030019378,-7.37535688457201E-15,0.527831625809918));
#133323=DIRECTION('center_axis',(-0.10478522557409,0.994494875050338,6.94452059562678E-15));
#133324=DIRECTION('ref_axis',(0.994494875050338,0.10478522557409,-6.10576890204024E-30));
#133325=DIRECTION('center_axis',(0.994521895368276,0.104528463267629,7.29918357753754E-16));
#133326=DIRECTION('ref_axis',(0.104528463267629,-0.994521895368276,-6.82961998416064E-15));
#133327=DIRECTION('center_axis',(-7.71409749859041E-19,-6.96824330280696E-15,
1.));
#133328=DIRECTION('ref_axis',(0.,-1.,-6.96662863860695E-15));
#133329=DIRECTION('center_axis',(-0.104271693993672,0.994548849394382,1.52506799409043E-16));
#133330=DIRECTION('ref_axis',(0.994548849394382,0.104271693993672,4.10784825130666E-32));
#133331=DIRECTION('center_axis',(0.994521895368273,0.104528463267654,8.69963854893977E-16));
#133332=DIRECTION('ref_axis',(0.104528463267654,-0.994521895368273,-6.82961998416066E-15));
#133333=DIRECTION('center_axis',(0.861270944310205,0.0905534316534015,0.500012436348137));
#133334=DIRECTION('ref_axis',(0.497376550147764,0.0512812291253674,-0.866017784403127));
#133335=DIRECTION('center_axis',(-0.527021758969975,-0.0553922189448919,
-0.848044673146736));
#133336=DIRECTION('ref_axis',(0.849348701629309,6.90235289882492E-15,-0.527832154231445));
#133337=DIRECTION('center_axis',(-0.497265930898087,-0.0522647452161537,
-0.866022511471584));
#133338=DIRECTION('ref_axis',(-0.861737632556767,-0.0860712067739632,0.499999999999932));
#133339=DIRECTION('center_axis',(0.497265943181814,0.0522647566817715,0.866022503726373));
#133340=DIRECTION('ref_axis',(-0.867207748104437,-6.28489530937578E-15,
0.497946504785033));
#133341=DIRECTION('center_axis',(-0.527021728885167,-0.0553921903536622,
-0.848044693710605));
#133342=DIRECTION('ref_axis',(-0.843864204094708,-0.0841354767153469,0.529919264233228));
#133343=DIRECTION('center_axis',(-0.527021693998979,-0.0553922121161939,
-0.848044713969329));
#133344=DIRECTION('ref_axis',(0.849348742192414,5.97509586698296E-15,-0.527832088960272));
#133345=DIRECTION('center_axis',(0.994521895368276,0.104528463267629,7.29918357753754E-16));
#133346=DIRECTION('ref_axis',(0.104528463267629,-0.994521895368276,-6.82961998416064E-15));
#133347=DIRECTION('center_axis',(-0.994521895368276,-0.104528463267629,
-7.29918357753754E-16));
#133348=DIRECTION('ref_axis',(-0.104528463267629,0.994521895368276,6.82961998416064E-15));
#133349=DIRECTION('center_axis',(0.994521895368273,0.104528463267654,8.69963854893977E-16));
#133350=DIRECTION('ref_axis',(0.104528463267654,-0.994521895368273,-6.82961998416066E-15));
#133351=DIRECTION('center_axis',(0.994521895368276,0.104528463267629,1.44380803939994E-15));
#133352=DIRECTION('ref_axis',(0.104528463267629,-0.994521895368276,-6.82961998416064E-15));
#133353=DIRECTION('center_axis',(0.994521895368273,0.104528463267654,8.69963854893977E-16));
#133354=DIRECTION('ref_axis',(0.104528463267654,-0.994521895368273,-6.82961998416066E-15));
#133355=DIRECTION('center_axis',(-0.861289491529676,-0.0905598208268648,
0.499979330205117));
#133356=DIRECTION('ref_axis',(0.497139368682041,0.0532207405894839,0.866036951219478));
#133357=DIRECTION('center_axis',(0.497266077958573,0.0522647708473918,-0.866022425483294));
#133358=DIRECTION('ref_axis',(0.867207670398082,-6.72680058735007E-15,0.497946640115918));
#133359=DIRECTION('center_axis',(0.497266086881507,0.0522647717852377,-0.866022420303188));
#133360=DIRECTION('ref_axis',(-0.104528463263061,0.994521895368756,2.66191267869619E-12));
#133361=DIRECTION('center_axis',(-0.489078705153339,-0.103956887953411,
-0.86602250872167));
#133362=DIRECTION('ref_axis',(0.207911690816915,-0.978147600733985,4.76434291194686E-13));
#133363=DIRECTION('center_axis',(-0.847099893161541,-0.18002592730432,-0.500012436349263));
#133364=DIRECTION('ref_axis',(0.488879980353917,0.104926459522144,-0.866017784402435));
#133365=DIRECTION('center_axis',(0.489078713616375,0.103956889752287,0.866022503726308));
#133366=DIRECTION('ref_axis',(-0.8707403454847,2.60936961613722E-16,0.491743073916842));
#133367=DIRECTION('center_axis',(0.978147600733807,0.207911690817754,1.45183957723502E-15));
#133368=DIRECTION('ref_axis',(0.207911690817754,-0.978147600733807,-6.8296199841607E-15));
#133369=DIRECTION('center_axis',(-0.978147600733806,-0.20791169081776,-1.58957929685218E-15));
#133370=DIRECTION('ref_axis',(-0.20791169081776,0.978147600733805,6.82961998416066E-15));
#133371=DIRECTION('center_axis',(-0.978147600733806,-0.207911690817757,
-1.45183957723504E-15));
#133372=DIRECTION('ref_axis',(-0.207911690817757,0.978147600733806,6.8296199841607E-15));
#133373=DIRECTION('center_axis',(-0.978147600733806,-0.20791169081776,-1.58957929685218E-15));
#133374=DIRECTION('ref_axis',(-0.20791169081776,0.978147600733805,6.82961998416066E-15));
#133375=DIRECTION('center_axis',(0.978147600733806,0.207911690817757,1.45183957723504E-15));
#133376=DIRECTION('ref_axis',(0.207911690817757,-0.978147600733806,-6.8296199841607E-15));
#133377=DIRECTION('center_axis',(-0.518344097776643,-0.110177439185358,
0.848045003637587));
#133378=DIRECTION('ref_axis',(-0.853239582811875,1.09365286413532E-15,-0.521519140898029));
#133379=DIRECTION('center_axis',(0.489078846174041,0.103956917928299,-0.866022425483266));
#133380=DIRECTION('ref_axis',(0.870740269393754,-1.06873346547645E-15,0.491743208652741));
#133381=DIRECTION('center_axis',(0.518344065636772,0.110177454461713,-0.848045021297501));
#133382=DIRECTION('ref_axis',(0.828609503968484,0.180532167016336,0.529919264233232));
#133383=DIRECTION('center_axis',(-0.518344042878402,-0.110177427516376,
0.848045038708645));
#133384=DIRECTION('ref_axis',(-0.853239616987301,5.33563410317125E-16,-0.521519084984782));
#133385=DIRECTION('center_axis',(0.489078857536798,0.103956931094697,-0.866022417485756));
#133386=DIRECTION('ref_axis',(0.846143288283833,0.18450348422784,0.50000000000001));
#133387=DIRECTION('center_axis',(0.847119506978957,0.180025582247261,-0.499979330205024));
#133388=DIRECTION('ref_axis',(0.489253749387828,0.10300858135289,0.86603695121953));
#133389=DIRECTION('center_axis',(-0.208148881407599,0.978097154258597,6.83001592333893E-15));
#133390=DIRECTION('ref_axis',(0.978097154258597,0.2081488814076,6.48647463947594E-29));
#133391=DIRECTION('center_axis',(-0.978147600733806,-0.20791169081776,-1.58957929685218E-15));
#133392=DIRECTION('ref_axis',(-0.20791169081776,0.978147600733805,6.82961998416066E-15));
#133393=DIRECTION('center_axis',(0.978147600733806,0.207911690817757,1.45183957723504E-15));
#133394=DIRECTION('ref_axis',(0.207911690817757,-0.978147600733806,-6.8296199841607E-15));
#133395=DIRECTION('center_axis',(-3.07718727278886E-18,-6.95368519647906E-15,
1.));
#133396=DIRECTION('ref_axis',(0.,-1.,-6.95327949822825E-15));
#133397=DIRECTION('center_axis',(-0.20767448800182,0.978197989689808,6.83072005339167E-15));
#133398=DIRECTION('ref_axis',(0.978197989689808,0.20767448800182,-2.3436552753213E-29));
#133399=DIRECTION('center_axis',(0.518344551206617,0.110177535564844,0.848044713969298));
#133400=DIRECTION('ref_axis',(-0.85323930054102,1.72522091353502E-16,0.521519602711414));
#133401=DIRECTION('center_axis',(0.518344042878406,0.110177427516377,-0.848045038708642));
#133402=DIRECTION('ref_axis',(0.853239616987298,-7.31872120548215E-16,0.521519084984786));
#133403=DIRECTION('center_axis',(0.518344588350353,0.110177517683876,0.848044693589272));
#133404=DIRECTION('ref_axis',(-0.828561842307896,-0.18075078662581,0.529919264233238));
#133405=DIRECTION('center_axis',(0.518344615107834,0.110177549147485,0.848044673146742));
#133406=DIRECTION('ref_axis',(-0.853239260760976,1.17359536946331E-15,0.521519667794095));
#133407=DIRECTION('center_axis',(-0.518344065777961,-0.11017745455898,0.848045021198566));
#133408=DIRECTION('ref_axis',(0.830401496091911,0.172101506916234,0.52991926423322));
#133409=DIRECTION('center_axis',(0.518344097776693,0.110177439185368,-0.848045003637555));
#133410=DIRECTION('ref_axis',(0.853239582811844,2.59696859442649E-16,0.52151914089808));
#133411=DIRECTION('center_axis',(-0.208164222161104,0.978093889466682,6.82999312541884E-15));
#133412=DIRECTION('ref_axis',(0.978093889466682,0.208164222161104,3.86600523032468E-29));
#133413=DIRECTION('center_axis',(0.978147600733806,0.207911690817757,1.45183957723504E-15));
#133414=DIRECTION('ref_axis',(0.207911690817757,-0.978147600733806,-6.8296199841607E-15));
#133415=DIRECTION('center_axis',(-3.07718727278886E-18,-6.95368519647906E-15,
1.));
#133416=DIRECTION('ref_axis',(0.,-1.,-6.95161435274788E-15));
#133417=DIRECTION('center_axis',(-0.207659145615656,0.978201246800563,6.8307427976745E-15));
#133418=DIRECTION('ref_axis',(0.978201246800563,0.207659145615656,5.37895539563461E-29));
#133419=DIRECTION('center_axis',(0.978147600733806,0.20791169081776,1.58957929685218E-15));
#133420=DIRECTION('ref_axis',(0.20791169081776,-0.978147600733806,-6.82961998416069E-15));
#133421=DIRECTION('center_axis',(0.847087400906439,0.18008469874752,0.500012436347927));
#133422=DIRECTION('ref_axis',(0.489291521298834,0.102990311594979,-0.866017784403208));
#133423=DIRECTION('center_axis',(-0.518344615107832,-0.110177549147514,
-0.84804467314674));
#133424=DIRECTION('ref_axis',(0.853239260760976,-1.16622482208424E-15,-0.521519667794095));
#133425=DIRECTION('center_axis',(-0.489078702596298,-0.103956877075459,
-0.866022511471521));
#133426=DIRECTION('ref_axis',(-0.84802005266229,-0.175675810180602,0.500000000000036));
#133427=DIRECTION('center_axis',(0.489078713616259,0.103956889752262,0.866022503726376));
#133428=DIRECTION('ref_axis',(-0.870740345484766,-4.19511635357395E-16,
0.491743073916725));
#133429=DIRECTION('center_axis',(-0.518344588177165,-0.110177517564694,
-0.848044693710613));
#133430=DIRECTION('ref_axis',(-0.830446875605574,-0.171882402215915,0.529919264233172));
#133431=DIRECTION('center_axis',(-0.518344551206558,-0.110177535564878,
-0.84804471396933));
#133432=DIRECTION('ref_axis',(0.853239300541055,-1.32448832729202E-15,-0.521519602711356));
#133433=DIRECTION('center_axis',(0.978147600733806,0.207911690817757,1.45183957723504E-15));
#133434=DIRECTION('ref_axis',(0.207911690817757,-0.978147600733806,-6.8296199841607E-15));
#133435=DIRECTION('center_axis',(-0.978147600733806,-0.207911690817757,
-1.45183957723504E-15));
#133436=DIRECTION('ref_axis',(-0.207911690817757,0.978147600733806,6.8296199841607E-15));
#133437=DIRECTION('center_axis',(0.978147600733806,0.20791169081776,1.58957929685218E-15));
#133438=DIRECTION('ref_axis',(0.20791169081776,-0.978147600733806,-6.82961998416069E-15));
#133439=DIRECTION('center_axis',(0.978147600733806,0.207911690817757,4.29175525433417E-15));
#133440=DIRECTION('ref_axis',(0.207911690817757,-0.978147600733806,-6.8296199841607E-15));
#133441=DIRECTION('center_axis',(0.978147600733806,0.20791169081776,1.58957929685218E-15));
#133442=DIRECTION('ref_axis',(0.20791169081776,-0.978147600733806,-6.82961998416069E-15));
#133443=DIRECTION('center_axis',(-0.847105178672008,-0.18009299163103,0.499979330205211));
#133444=DIRECTION('ref_axis',(0.488852904976872,0.104894406038809,0.866036951219426));
#133445=DIRECTION('center_axis',(0.489078846174021,0.103956917928296,-0.866022425483277));
#133446=DIRECTION('ref_axis',(0.870740269393765,-5.71691885207346E-16,0.491743208652721));
#133447=DIRECTION('center_axis',(0.489078854950998,0.103956919793908,-0.866022420302606));
#133448=DIRECTION('ref_axis',(-0.207911690815927,0.978147600734195,1.10148110841986E-12));
#133449=DIRECTION('center_axis',(-0.475533027092007,-0.154510046711426,
-0.866022508720152));
#133450=DIRECTION('ref_axis',(0.30901699437304,-0.951056516295773,1.14519068158217E-12));
#133451=DIRECTION('center_axis',(-0.82364155778377,-0.267585776505831,-0.500012436348634));
#133452=DIRECTION('ref_axis',(0.475234043093109,0.15545353448369,-0.866017784402783));
#133453=DIRECTION('center_axis',(0.475533035318149,0.154510049384265,0.866022503726307));
#133454=DIRECTION('ref_axis',(-0.876548788012431,1.65548636897334E-15,0.481313018974075));
#133455=DIRECTION('center_axis',(0.951056516295146,0.309016994374972,2.15785413849121E-15));
#133456=DIRECTION('ref_axis',(0.309016994374972,-0.951056516295146,-6.82961998416073E-15));
#133457=DIRECTION('center_axis',(-0.951056516295153,-0.309016994374948,
-2.29177897539323E-15));
#133458=DIRECTION('ref_axis',(-0.309016994374948,0.951056516295153,6.82961998416066E-15));
#133459=DIRECTION('center_axis',(-0.951056516295148,-0.309016994374964,
-2.15785413849116E-15));
#133460=DIRECTION('ref_axis',(-0.309016994374964,0.951056516295148,6.82961998416075E-15));
#133461=DIRECTION('center_axis',(-0.951056516295153,-0.309016994374948,
-2.29177897539323E-15));
#133462=DIRECTION('ref_axis',(-0.309016994374948,0.951056516295153,6.82961998416066E-15));
#133463=DIRECTION('center_axis',(0.951056516295165,0.309016994374914,2.15785413849081E-15));
#133464=DIRECTION('ref_axis',(0.309016994374914,-0.951056516295164,-6.82961998416067E-15));
#133465=DIRECTION('center_axis',(-0.503987876168977,-0.163755587629907,
0.848045003637583));
#133466=DIRECTION('ref_axis',(-0.859649462041492,-3.17523175098311E-16,
-0.510884333691858));
#133467=DIRECTION('center_axis',(0.475533164204456,0.154510091262,-0.866022425483259));
#133468=DIRECTION('ref_axis',(0.87654871462881,1.46236813511121E-15,0.481313152617484));
#133469=DIRECTION('center_axis',(0.503987842607937,0.163755599464321,-0.848045021297501));
#133470=DIRECTION('ref_axis',(0.805199544420696,0.266156471007566,0.529919264233244));
#133471=DIRECTION('center_axis',(-0.503987822791217,-0.163755570286421,
0.84804503870864));
#133472=DIRECTION('ref_axis',(-0.859649495083695,-1.02670203161972E-15,
-0.510884278092749));
#133473=DIRECTION('center_axis',(0.475533174128557,0.154510105544451,-0.86602241748575));
#133474=DIRECTION('ref_axis',(0.822222161144199,0.271938812462168,0.500000000000029));
#133475=DIRECTION('center_axis',(0.823661100222806,0.26758748354006,-0.499979330205214));
#133476=DIRECTION('ref_axis',(0.475806237446429,0.153585232133988,0.866036951219416));
#133477=DIRECTION('center_axis',(-0.309247612517368,0.950981553003163,6.64066869178921E-15));
#133478=DIRECTION('ref_axis',(0.950981553003163,0.309247612517368,3.41480999208042E-15));
#133479=DIRECTION('center_axis',(-0.951056516295153,-0.309016994374948,
-2.29177897539323E-15));
#133480=DIRECTION('ref_axis',(-0.309016994374948,0.951056516295153,6.82961998416066E-15));
#133481=DIRECTION('center_axis',(0.951056516295165,0.309016994374914,2.15785413849081E-15));
#133482=DIRECTION('ref_axis',(0.309016994374914,-0.951056516295164,-6.82961998416067E-15));
#133483=DIRECTION('center_axis',(-6.89206998773325E-18,-6.93944786036197E-15,
1.));
#133484=DIRECTION('ref_axis',(0.,-1.,-6.93917548301887E-15));
#133485=DIRECTION('center_axis',(-0.308786358061007,0.95113142366101,6.64171523299944E-15));
#133486=DIRECTION('ref_axis',(0.95113142366101,0.308786358061007,3.41480999208033E-15));
#133487=DIRECTION('center_axis',(0.503988317040591,0.163755730877766,0.848044713969305));
#133488=DIRECTION('ref_axis',(-0.859649189130459,9.85221772351679E-16,0.510884792910637));
#133489=DIRECTION('center_axis',(0.503987822791257,0.163755570286483,-0.848045038708604));
#133490=DIRECTION('ref_axis',(0.859649495083668,-9.8120496246209E-16,0.510884278092794));
#133491=DIRECTION('center_axis',(0.503988355850447,0.163755716975672,0.848044693589287));
#133492=DIRECTION('ref_axis',(-0.805129291879168,-0.266368911010095,0.52991926423319));
#133493=DIRECTION('center_axis',(0.503988379172007,0.163755751065438,0.848044673146744));
#133494=DIRECTION('ref_axis',(-0.859649150669465,-1.91533628641601E-15,
0.510884857627692));
#133495=DIRECTION('center_axis',(-0.503987842737568,-0.163755599577719,
0.848045021198565));
#133496=DIRECTION('ref_axis',(0.807862963765903,0.25795930913596,0.529919264233213));
#133497=DIRECTION('center_axis',(0.503987876169007,0.163755587629917,-0.848045003637563));
#133498=DIRECTION('ref_axis',(0.859649462041474,-1.19924147547379E-15,0.510884333691888));
#133499=DIRECTION('center_axis',(-0.309262527968962,0.950976702550723,2.35377991522115E-14));
#133500=DIRECTION('ref_axis',(0.950976702550723,0.309262527968962,3.4148099920802E-15));
#133501=DIRECTION('center_axis',(0.951056516295148,0.309016994374964,5.41206908565348E-14));
#133502=DIRECTION('ref_axis',(0.309016994374964,-0.951056516295148,-6.82961998416119E-15));
#133503=DIRECTION('center_axis',(-6.89206998773325E-18,-6.93944786036197E-15,
1.));
#133504=DIRECTION('ref_axis',(0.,-1.,-6.93660006688881E-15));
#133505=DIRECTION('center_axis',(-0.308771440182806,0.951136266645025,6.64174905137606E-15));
#133506=DIRECTION('ref_axis',(0.951136266645025,0.308771440182806,3.41480999208035E-15));
#133507=DIRECTION('center_axis',(0.951056516295153,0.309016994374948,2.29177897539323E-15));
#133508=DIRECTION('ref_axis',(0.309016994374948,-0.951056516295153,-6.82961998416059E-15));
#133509=DIRECTION('center_axis',(0.823622990673535,0.267642920194618,0.500012436349017));
#133510=DIRECTION('ref_axis',(0.475845712147552,0.153571010705906,-0.866017784402581));
#133511=DIRECTION('center_axis',(-0.503988379172001,-0.163755751065509,
-0.848044673146734));
#133512=DIRECTION('ref_axis',(0.859649150669465,1.85736175073367E-15,-0.510884857627692));
#133513=DIRECTION('center_axis',(-0.475533025685126,-0.154510035619843,
-0.866022511471558));
#133514=DIRECTION('ref_axis',(-0.825011387616483,-0.263355672623859,0.49999999999996));
#133515=DIRECTION('center_axis',(0.475533035318008,0.154510049384242,0.866022503726388));
#133516=DIRECTION('ref_axis',(-0.87654878801251,1.92597280652308E-16,0.481313018973931));
#133517=DIRECTION('center_axis',(-0.50398835568966,-0.16375571684218,-0.848044693710619));
#133518=DIRECTION('ref_axis',(-0.807930997354701,-0.257746148192231,0.529919264233247));
#133519=DIRECTION('center_axis',(-0.50398831704056,-0.163755730877761,-0.848044713969325));
#133520=DIRECTION('ref_axis',(0.859649189130478,3.22133773568149E-16,-0.510884792910605));
#133521=DIRECTION('center_axis',(0.951056516295148,0.309016994374964,5.41206908565348E-14));
#133522=DIRECTION('ref_axis',(0.309016994374964,-0.951056516295148,-6.82961998416119E-15));
#133523=DIRECTION('center_axis',(-0.951056516295148,-0.309016994374964,
-2.15785413849116E-15));
#133524=DIRECTION('ref_axis',(-0.309016994374964,0.951056516295148,6.82961998416075E-15));
#133525=DIRECTION('center_axis',(0.951056516295153,0.309016994374948,2.29177897539323E-15));
#133526=DIRECTION('ref_axis',(0.309016994374948,-0.951056516295153,-6.82961998416059E-15));
#133527=DIRECTION('center_axis',(0.951056516295148,0.309016994374964,-1.47258949833367E-14));
#133528=DIRECTION('ref_axis',(0.309016994374964,-0.951056516295148,-6.82961998416061E-15));
#133529=DIRECTION('center_axis',(0.951056516295153,0.309016994374948,2.29177897539323E-15));
#133530=DIRECTION('ref_axis',(0.309016994374948,-0.951056516295153,-6.82961998416059E-15));
#133531=DIRECTION('center_axis',(-0.823639804208724,-0.267653025932271,
0.499979330205074));
#133532=DIRECTION('ref_axis',(0.475210466544364,0.15541882643076,0.866036951219504));
#133533=DIRECTION('center_axis',(0.475533164204417,0.154510091261987,-0.866022425483283));
#133534=DIRECTION('ref_axis',(0.876548714628833,-9.26574607259983E-16,0.481313152617443));
#133535=DIRECTION('center_axis',(0.475533172743519,0.154510094036525,-0.866022420299444));
#133536=DIRECTION('ref_axis',(-0.309016994369036,0.951056516297074,3.61478125659533E-12));
#133537=DIRECTION('center_axis',(-0.456777309669968,-0.203370361063118,
-0.866022508721178));
#133538=DIRECTION('ref_axis',(0.406736643078441,-0.913545457641425,-1.66970549760595E-12));
#133539=DIRECTION('center_axis',(-0.791159233141002,-0.352213899941929,
-0.500012436348776));
#133540=DIRECTION('ref_axis',(0.456381342238393,0.20427742791317,-0.866017784402758));
#133541=DIRECTION('center_axis',(0.456777317573273,0.203370364581906,0.866022503726311));
#133542=DIRECTION('ref_axis',(-0.884507036382099,-1.20094363058356E-15,
0.466526850878443));
#133543=DIRECTION('center_axis',(0.913545457642594,0.406736643075817,-5.81845465367576E-14));
#133544=DIRECTION('ref_axis',(0.406736643075817,-0.913545457642593,-6.82961998416125E-15));
#133545=DIRECTION('center_axis',(-0.913545457642601,-0.406736643075801,
-2.96886944389428E-15));
#133546=DIRECTION('ref_axis',(-0.406736643075801,0.9135454576426,6.82961998416066E-15));
#133547=DIRECTION('center_axis',(-0.913545457642598,-0.406736643075807,
-2.84022679824576E-15));
#133548=DIRECTION('ref_axis',(-0.406736643075807,0.913545457642598,6.8296199841606E-15));
#133549=DIRECTION('center_axis',(-0.913545457642601,-0.406736643075801,
-2.96886944389428E-15));
#133550=DIRECTION('ref_axis',(-0.406736643075801,0.9135454576426,6.82961998416066E-15));
#133551=DIRECTION('center_axis',(0.913545457642594,0.406736643075817,2.84022679824583E-15));
#133552=DIRECTION('ref_axis',(0.406736643075817,-0.913545457642593,-6.82961998416057E-15));
#133553=DIRECTION('center_axis',(-0.48410985792377,-0.215539595588312,0.848045003637575));
#133554=DIRECTION('ref_axis',(-0.868458021515995,2.11054687512659E-16,-0.495762710240014));
#133555=DIRECTION('center_axis',(0.456777441376059,0.203370419702488,-0.866022425483298));
#133556=DIRECTION('ref_axis',(0.884506966812066,-1.6326678946194E-15,0.466526982779045));
#133557=DIRECTION('center_axis',(0.484109823307075,0.215539603855264,-0.848045021297519));
#133558=DIRECTION('ref_axis',(0.772967650150695,0.348864709042188,0.529919264233168));
#133559=DIRECTION('center_axis',(-0.484109806651296,-0.215539572760336,
0.848045038708639));
#133560=DIRECTION('ref_axis',(-0.868458052949952,3.7813810093915E-16,-0.495762655175215));
#133561=DIRECTION('center_axis',(0.456777449752818,0.20337043494432,-0.866022417485754));
#133562=DIRECTION('ref_axis',(0.789292595944616,0.356394722164874,0.500000000000031));
#133563=DIRECTION('center_axis',(0.791178490090723,0.352217640366536,-0.499979330205153));
#133564=DIRECTION('ref_axis',(0.457145692792613,0.202479170987194,0.866036951219462));
#133565=DIRECTION('center_axis',(-0.406958162070229,0.913446798847323,6.37856490440285E-15));
#133566=DIRECTION('ref_axis',(0.913446798847323,0.406958162070229,3.41480999208031E-15));
#133567=DIRECTION('center_axis',(-0.913545457642601,-0.406736643075801,
-2.96886944389428E-15));
#133568=DIRECTION('ref_axis',(-0.406736643075801,0.9135454576426,6.82961998416066E-15));
#133569=DIRECTION('center_axis',(0.913545457642598,0.406736643075807,2.84022679824576E-15));
#133570=DIRECTION('ref_axis',(0.406736643075807,-0.913545457642598,-6.8296199841606E-15));
#133571=DIRECTION('center_axis',(-1.21742612413517E-17,-6.92568728168955E-15,
1.));
#133572=DIRECTION('ref_axis',(0.,-1.,-6.92507146780948E-15));
#133573=DIRECTION('center_axis',(-0.406515100163544,0.913644062717546,6.37994239064628E-15));
#133574=DIRECTION('ref_axis',(0.913644062717546,0.406515100163544,3.41480999208035E-15));
#133575=DIRECTION('center_axis',(0.48411028140672,0.215539784135058,0.848044713969328));
#133576=DIRECTION('ref_axis',(-0.868457761888286,-1.79355219875376E-15,
0.495763165045558));
#133577=DIRECTION('center_axis',(0.484109806651295,0.215539572760335,-0.84804503870864));
#133578=DIRECTION('ref_axis',(0.868458052949953,8.16837448075292E-17,0.495762655175213));
#133579=DIRECTION('center_axis',(0.484110321456976,0.215539774366318,0.848044693589282));
#133580=DIRECTION('ref_axis',(-0.772875576444115,-0.349068641861079,0.529919264233184));
#133581=DIRECTION('center_axis',(0.484110341087615,0.215539810706669,0.848044673146743));
#133582=DIRECTION('ref_axis',(-0.868457725299269,-6.1342256846168E-16,0.495763229140705));
#133583=DIRECTION('center_axis',(-0.484109823426906,-0.215539603975436,
0.84804502119857));
#133584=DIRECTION('ref_axis',(0.776473315750794,0.340990855187512,0.5299192642332));
#133585=DIRECTION('center_axis',(0.484109857923801,0.215539595588326,-0.848045003637554));
#133586=DIRECTION('ref_axis',(0.868458021515976,-2.74972831225249E-15,0.495762710240047));
#133587=DIRECTION('center_axis',(-0.406972488803041,0.913440415876952,6.37852033235898E-15));
#133588=DIRECTION('ref_axis',(0.913440415876952,0.406972488803041,3.41480999208023E-15));
#133589=DIRECTION('center_axis',(0.913545457642598,0.406736643075807,2.84022679824576E-15));
#133590=DIRECTION('ref_axis',(0.406736643075807,-0.913545457642598,-6.8296199841606E-15));
#133591=DIRECTION('center_axis',(-1.21742612413517E-17,-6.92568728168955E-15,
1.));
#133592=DIRECTION('ref_axis',(0.,-1.,-6.92909292395928E-15));
#133593=DIRECTION('center_axis',(-0.406500770236728,0.913650438514067,-1.85795542610555E-14));
#133594=DIRECTION('ref_axis',(0.913650438514067,0.406500770236727,3.41480999208053E-15));
#133595=DIRECTION('center_axis',(0.913545457642601,0.406736643075801,2.96886944389428E-15));
#133596=DIRECTION('ref_axis',(0.406736643075801,-0.913545457642601,-6.82961998416062E-15));
#133597=DIRECTION('center_axis',(0.791134794600465,0.352268789801546,0.500012436349572));
#133598=DIRECTION('ref_axis',(0.457186437809986,0.202469153654735,-0.866017784402232));
#133599=DIRECTION('center_axis',(-0.484110341087606,-0.2155398107067,-0.848044673146741));
#133600=DIRECTION('ref_axis',(0.868457725299272,1.42879581731315E-15,-0.495763229140699));
#133601=DIRECTION('center_axis',(-0.456777309431663,-0.20337034988632,-0.866022511471548));
#133602=DIRECTION('ref_axis',(-0.792963725159232,-0.34815015522271,0.499999999999996));
#133603=DIRECTION('center_axis',(0.456777317573163,0.203370364581857,0.866022503726381));
#133604=DIRECTION('ref_axis',(-0.88450703638216,-2.11081026387279E-15,0.466526850878326));
#133605=DIRECTION('center_axis',(-0.484110321309854,-0.215539774219457,
-0.848044693710594));
#133606=DIRECTION('ref_axis',(-0.776563258035295,-0.34078597339695,0.529919264233242));
#133607=DIRECTION('center_axis',(-0.484110281406723,-0.215539784135059,
-0.848044713969326));
#133608=DIRECTION('ref_axis',(0.868457761888284,1.78019109930865E-15,-0.495763165045561));
#133609=DIRECTION('center_axis',(0.913545457642598,0.406736643075807,2.84022679824576E-15));
#133610=DIRECTION('ref_axis',(0.406736643075807,-0.913545457642598,-6.8296199841606E-15));
#133611=DIRECTION('center_axis',(-0.913545457642598,-0.406736643075807,
-2.84022679824576E-15));
#133612=DIRECTION('ref_axis',(-0.406736643075807,0.913545457642598,6.8296199841606E-15));
#133613=DIRECTION('center_axis',(0.913545457642601,0.406736643075801,2.96886944389428E-15));
#133614=DIRECTION('ref_axis',(0.406736643075801,-0.913545457642601,-6.82961998416062E-15));
#133615=DIRECTION('center_axis',(0.913545457642598,0.406736643075807,-1.93826268484815E-14));
#133616=DIRECTION('ref_axis',(0.406736643075807,-0.913545457642598,-6.8296199841606E-15));
#133617=DIRECTION('center_axis',(0.913545457642601,0.406736643075801,2.96886944389428E-15));
#133618=DIRECTION('ref_axis',(0.406736643075801,-0.913545457642601,-6.82961998416062E-15));
#133619=DIRECTION('center_axis',(-0.791150459692754,-0.352280597671016,
0.499979330205255));
#133620=DIRECTION('ref_axis',(0.456361522795892,0.204240445637063,0.866036951219397));
#133621=DIRECTION('center_axis',(0.456777441376069,0.203370419702474,-0.866022425483296));
#133622=DIRECTION('ref_axis',(0.884506966812061,-1.94827188835773E-15,0.466526982779054));
#133623=DIRECTION('center_axis',(0.456777449574972,0.20337042335284,-0.866022420301617));
#133624=DIRECTION('ref_axis',(-0.406736643074073,0.91354545764337,1.08399728130801E-12));
#133625=DIRECTION('center_axis',(-0.43301704445909,-0.250002507182135,-0.866022508720507));
#133626=DIRECTION('ref_axis',(0.500000000001343,-0.866025403783663,-9.13529971196899E-13));
#133627=DIRECTION('center_axis',(-0.750008802378837,-0.432983094185202,
-0.500012436349409));
#133628=DIRECTION('ref_axis',(0.432528431868679,0.250863215167168,-0.866017784402383));
#133629=DIRECTION('center_axis',(0.433017051950287,0.250002511507189,0.866022503726306));
#133630=DIRECTION('ref_axis',(-0.89442479486378,1.23985474967347E-15,0.447218387740135));
#133631=DIRECTION('center_axis',(0.86602540378444,0.499999999999998,6.44677165429795E-14));
#133632=DIRECTION('ref_axis',(0.499999999999998,-0.86602540378444,-6.82961998416156E-15));
#133633=DIRECTION('center_axis',(-0.866025403784438,-0.500000000000001,
-3.61343235749215E-15));
#133634=DIRECTION('ref_axis',(-0.500000000000001,0.866025403784438,6.82961998416066E-15));
#133635=DIRECTION('center_axis',(-0.866025403784433,-0.50000000000001,-3.4914813388432E-15));
#133636=DIRECTION('ref_axis',(-0.50000000000001,0.866025403784433,6.82961998416047E-15));
#133637=DIRECTION('center_axis',(-0.866025403784438,-0.500000000000001,
-3.61343235749215E-15));
#133638=DIRECTION('ref_axis',(-0.500000000000001,0.866025403784438,6.82961998416066E-15));
#133639=DIRECTION('center_axis',(0.86602540378444,0.499999999999998,3.49148133884312E-15));
#133640=DIRECTION('ref_axis',(0.499999999999998,-0.86602540378444,-6.82961998416073E-15));
#133641=DIRECTION('center_axis',(-0.458927830768609,-0.264962106632872,
0.848045003637595));
#133642=DIRECTION('ref_axis',(-0.879478602053341,-1.06564665462097E-15,
-0.475938429348062));
#133643=DIRECTION('center_axis',(0.433017169313211,0.25000257926669,-0.866022425483299));
#133644=DIRECTION('ref_axis',(0.89442473021642,1.22965716892193E-15,0.447218517033098));
#133645=DIRECTION('center_axis',(0.458927795479855,0.26496211123202,-0.848045021297496));
#133646=DIRECTION('ref_axis',(0.73226696056946,0.427750712276335,0.529919264233198));
#133647=DIRECTION('center_axis',(-0.45892778216322,-0.264962078570537,0.848045038708634));
#133648=DIRECTION('ref_axis',(-0.879478631391241,1.07865946136944E-15,-0.475938375135048));
#133649=DIRECTION('center_axis',(0.433017176053256,0.250002595296572,-0.866022417485738));
#133650=DIRECTION('ref_axis',(0.747715375895629,0.436945896707163,0.500000000000031));
#133651=DIRECTION('center_axis',(0.750027562856292,0.432988827019189,-0.499979330205157));
#133652=DIRECTION('ref_axis',(0.433476564270849,0.249154705655846,0.866036951219455));
#133653=DIRECTION('center_axis',(-0.500209992837911,0.865904130412309,6.04657622512354E-15));
#133654=DIRECTION('ref_axis',(0.865904130412309,0.500209992837911,3.41480999208024E-15));
#133655=DIRECTION('center_axis',(-0.866025403784438,-0.500000000000001,
-3.61343235749215E-15));
#133656=DIRECTION('ref_axis',(-0.500000000000001,0.866025403784438,6.82961998416066E-15));
#133657=DIRECTION('center_axis',(0.866025403784433,0.50000000000001,3.4914813388432E-15));
#133658=DIRECTION('ref_axis',(0.50000000000001,-0.866025403784433,-6.82961998416068E-15));
#133659=DIRECTION('center_axis',(-1.88658882409001E-17,-6.91255422424131E-15,
1.));
#133660=DIRECTION('ref_axis',(0.,-1.,-6.91096745260009E-15));
#133661=DIRECTION('center_axis',(-0.499789977759974,0.86614662623062,6.04826956437229E-15));
#133662=DIRECTION('ref_axis',(0.86614662623062,0.499789977759974,3.4148099920803E-15));
#133663=DIRECTION('center_axis',(0.458928232223209,0.264962338412798,0.848044713969318));
#133664=DIRECTION('ref_axis',(-0.879478359737742,1.39963335782071E-15,0.475938877118703));
#133665=DIRECTION('center_axis',(0.458927782163206,0.264962078570538,-0.848045038708641));
#133666=DIRECTION('ref_axis',(0.879478631391249,-4.79831185544794E-17,0.475938375135034));
#133667=DIRECTION('center_axis',(0.458928273074798,0.26496233288458,0.848044693589285));
#133668=DIRECTION('ref_axis',(-0.7321540744614,-0.42794390361835,0.529919264233203));
#133669=DIRECTION('center_axis',(0.458928288799671,0.264962371077201,0.848044673146735));
#133670=DIRECTION('ref_axis',(-0.879478325588501,8.76012990705856E-16,0.475938940222426));
#133671=DIRECTION('center_axis',(-0.458927795588222,-0.264962111360946,
0.848045021198571));
#133672=DIRECTION('ref_axis',(0.736576463603418,0.420286434066109,0.529919264233219));
#133673=DIRECTION('center_axis',(0.458927830768629,0.264962106632892,-0.848045003637579));
#133674=DIRECTION('ref_axis',(0.879478602053329,-1.60404569334003E-16,0.475938429348085));
#133675=DIRECTION('center_axis',(-0.500223573885338,0.86589628485713,-1.76084488451793E-14));
#133676=DIRECTION('ref_axis',(0.86589628485713,0.500223573885338,3.41480999208019E-15));
#133677=DIRECTION('center_axis',(0.866025403784433,0.50000000000001,3.4914813388432E-15));
#133678=DIRECTION('ref_axis',(0.50000000000001,-0.866025403784433,-6.82961998416068E-15));
#133679=DIRECTION('center_axis',(-1.88658882409001E-17,-6.91255422424131E-15,
1.));
#133680=DIRECTION('ref_axis',(0.,-1.,-6.91407863810021E-15));
#133681=DIRECTION('center_axis',(-0.499776392786186,0.866154464985102,2.97103476758308E-14));
#133682=DIRECTION('ref_axis',(0.866154464985102,0.499776392786186,3.41480999208003E-15));
#133683=DIRECTION('center_axis',(0.866025403784438,0.500000000000001,3.61343235749215E-15));
#133684=DIRECTION('ref_axis',(0.500000000000001,-0.866025403784438,-6.82961998416072E-15));
#133685=DIRECTION('center_axis',(0.749978760163145,0.433035128829332,0.500012436349253));
#133686=DIRECTION('ref_axis',(-0.433518133161068,-0.249149002244091,0.866017784402443));
#133687=DIRECTION('center_axis',(-0.458928288799668,-0.264962371077187,
-0.848044673146741));
#133688=DIRECTION('ref_axis',(0.879478325588504,-1.71293817094444E-16,-0.475938940222421));
#133689=DIRECTION('center_axis',(-0.433017045390677,-0.250002496038782,
-0.86602251147156));
#133690=DIRECTION('ref_axis',(-0.752228186194176,-0.429130231858645,0.499999999999966));
#133691=DIRECTION('center_axis',(0.433017051950197,0.250002511507145,0.866022503726364));
#133692=DIRECTION('ref_axis',(-0.894424794863829,1.34326219726227E-15,0.447218387740037));
#133693=DIRECTION('center_axis',(-0.458928272943121,-0.264962332724383,
-0.848044693710595));
#133694=DIRECTION('ref_axis',(-0.73668732915487,-0.420092076165676,0.529919264233218));
#133695=DIRECTION('center_axis',(-0.458928232223181,-0.264962338412827,
-0.848044713969324));
#133696=DIRECTION('ref_axis',(0.879478359737755,-2.53168492317654E-16,-0.475938877118678));
#133697=DIRECTION('center_axis',(0.866025403784433,0.50000000000001,1.71507213071646E-14));
#133698=DIRECTION('ref_axis',(0.50000000000001,-0.866025403784433,-6.82961998416068E-15));
#133699=DIRECTION('center_axis',(-0.866025403784433,-0.50000000000001,-3.4914813388432E-15));
#133700=DIRECTION('ref_axis',(-0.50000000000001,0.866025403784433,6.82961998416068E-15));
#133701=DIRECTION('center_axis',(0.866025403784438,0.500000000000001,3.61343235749215E-15));
#133702=DIRECTION('ref_axis',(0.500000000000001,-0.866025403784438,-6.82961998416072E-15));
#133703=DIRECTION('center_axis',(0.866025403784433,0.50000000000001,3.4914813388432E-15));
#133704=DIRECTION('ref_axis',(0.50000000000001,-0.866025403784433,-6.82961998416068E-15));
#133705=DIRECTION('center_axis',(0.866025403784438,0.500000000000001,3.61343235749215E-15));
#133706=DIRECTION('ref_axis',(0.500000000000001,-0.866025403784438,-6.82961998416072E-15));
#133707=DIRECTION('center_axis',(-0.749993105181594,-0.433048509462309,
0.499979330205302));
#133708=DIRECTION('ref_axis',(-0.4325125867043,-0.250824363778751,-0.866036951219369));
#133709=DIRECTION('center_axis',(0.433017169313192,0.250002579266714,-0.866022425483302));
#133710=DIRECTION('ref_axis',(0.894424730216429,2.21005739164742E-15,0.447218517033081));
#133711=DIRECTION('center_axis',(0.433017177084447,0.250002583753453,-0.866022420302393));
#133712=DIRECTION('ref_axis',(-0.499999999997911,0.866025403785645,1.4118190397783E-12));
#133713=DIRECTION('center_axis',(-0.404512553894144,-0.293895573516168,
-0.866022508719975));
#133714=DIRECTION('ref_axis',(0.587785252291208,-0.809016994375867,9.0915901439341E-13));
#133715=DIRECTION('center_axis',(-0.700641118228567,-0.509008435041749,
-0.500012436349111));
#133716=DIRECTION('ref_axis',(0.403936649451869,0.294700492582192,-0.866017784402498));
#133717=DIRECTION('center_axis',(0.404512560891457,0.293895578600013,0.866022503726317));
#133718=DIRECTION('ref_axis',(-0.906035256115487,1.17177266627819E-15,0.423202214875754));
#133719=DIRECTION('center_axis',(0.809016994374931,0.587785252292496,4.1044824792529E-15));
#133720=DIRECTION('ref_axis',(0.587785252292496,-0.809016994374931,-6.82961998416073E-15));
#133721=DIRECTION('center_axis',(-0.809016994374947,-0.587785252292474,
-4.21840575002201E-15));
#133722=DIRECTION('ref_axis',(-0.587785252292474,0.809016994374947,6.82961998416066E-15));
#133723=DIRECTION('center_axis',(-0.809016994374931,-0.587785252292496,
2.80103167643605E-14));
#133724=DIRECTION('ref_axis',(-0.587785252292496,0.809016994374931,6.82961998416073E-15));
#133725=DIRECTION('center_axis',(-0.809016994374947,-0.587785252292474,
-4.21840575002201E-15));
#133726=DIRECTION('ref_axis',(-0.587785252292474,0.809016994374947,6.82961998416066E-15));
#133727=DIRECTION('center_axis',(0.80901699437495,0.58778525229247,4.10448247925272E-15));
#133728=DIRECTION('ref_axis',(0.58778525229247,-0.80901699437495,-6.82961998416043E-15));
#133729=DIRECTION('center_axis',(-0.428717694262756,-0.311481637390317,
0.848045003637586));
#133730=DIRECTION('ref_axis',(-0.892442058026272,-3.95378541852584E-16,
-0.45116202529228));
#133731=DIRECTION('center_axis',(0.404512670528671,0.293895658256124,-0.866022425483291));
#133732=DIRECTION('ref_axis',(0.906035197473499,1.39606431300021E-15,0.423202340422591));
#133733=DIRECTION('center_axis',(0.428717658681342,0.311481638282739,-0.848045021297507));
#133734=DIRECTION('ref_axis',(0.683543400919793,0.501950189215568,0.529919264233203));
#133735=DIRECTION('center_axis',(-0.428717648856913,-0.31148160440104,0.848045038708649));
#133736=DIRECTION('ref_axis',(-0.892442084777739,-1.07749458524948E-15,
-0.451161972375291));
#133737=DIRECTION('center_axis',(0.404512675554594,0.293895674904847,-0.866022417485765));
#133738=DIRECTION('ref_axis',(0.697946029716722,0.51270980057208,0.500000000000003));
#133739=DIRECTION('center_axis',(0.700659176689849,0.509016097474139,-0.49997933020526));
#133740=DIRECTION('ref_axis',(0.405058175792274,0.293100449242975,0.866036951219404));
#133741=DIRECTION('center_axis',(-0.587981418248406,0.808874435122407,-7.06716172179891E-14));
#133742=DIRECTION('ref_axis',(0.808874435122407,0.587981418248406,3.41480999207993E-15));
#133743=DIRECTION('center_axis',(-0.809016994374947,-0.587785252292474,
-4.21840575002201E-15));
#133744=DIRECTION('ref_axis',(-0.587785252292474,0.809016994374947,6.82961998416066E-15));
#133745=DIRECTION('center_axis',(0.809016994374969,0.587785252292444,4.10448247925254E-15));
#133746=DIRECTION('ref_axis',(0.587785252292444,-0.809016994374969,-6.8296199841606E-15));
#133747=DIRECTION('center_axis',(-2.68936361206584E-17,-6.90019257654293E-15,
1.));
#133748=DIRECTION('ref_axis',(0.,-1.,-6.8968634373907E-15));
#133749=DIRECTION('center_axis',(-0.587589051772239,0.809159506053906,5.65033063106948E-15));
#133750=DIRECTION('ref_axis',(0.809159506053906,0.587589051772239,3.41480999208021E-15));
#133751=DIRECTION('center_axis',(0.428718069290544,0.311481909863913,0.848044713969327));
#133752=DIRECTION('ref_axis',(-0.892441837073393,-4.22102850772109E-15,
0.451162462358148));
#133753=DIRECTION('center_axis',(0.428717648856975,0.311481604401142,-0.848045038708581));
#133754=DIRECTION('ref_axis',(0.892442084777698,3.18562187189916E-15,0.451161972375372));
#133755=DIRECTION('center_axis',(0.428718110493366,0.311481908639993,0.848044693589309));
#133756=DIRECTION('ref_axis',(-0.683410939232418,-0.502130522406281,0.529919264233204));
#133757=DIRECTION('center_axis',(0.428718122142701,0.311481948263281,0.848044673146731));
#133758=DIRECTION('ref_axis',(-0.892441805934775,3.97758164497583E-16,0.451162523953261));
#133759=DIRECTION('center_axis',(-0.428717658777612,-0.311481638419594,
0.848045021198573));
#133760=DIRECTION('ref_axis',(0.688609525573209,0.494977266835898,0.529919264233246));
#133761=DIRECTION('center_axis',(0.428717694262811,0.311481637390356,-0.848045003637544));
#133762=DIRECTION('ref_axis',(0.892442058026239,2.8004224903515E-15,0.451162025292345));
#133763=DIRECTION('center_axis',(-0.587994104813606,0.808865212939984,5.64827559323867E-15));
#133764=DIRECTION('ref_axis',(0.808865212939984,0.587994104813606,3.41480999208028E-15));
#133765=DIRECTION('center_axis',(0.809016994374931,0.587785252292496,8.04215107813387E-14));
#133766=DIRECTION('ref_axis',(0.587785252292496,-0.809016994374931,-6.82961998416074E-15));
#133767=DIRECTION('center_axis',(-2.68936361206584E-17,-6.90019257654293E-15,
1.));
#133768=DIRECTION('ref_axis',(0.,-1.,-6.89906435224115E-15));
#133769=DIRECTION('center_axis',(-0.587576360591353,0.80916872188328,3.77537810209823E-14));
#133770=DIRECTION('ref_axis',(0.80916872188328,0.587576360591353,3.41480999207978E-15));
#133771=DIRECTION('center_axis',(0.809016994374947,0.587785252292474,4.21840575002201E-15));
#133772=DIRECTION('ref_axis',(0.587785252292474,-0.809016994374947,-6.82961998416063E-15));
#133773=DIRECTION('center_axis',(0.700605801485416,0.509057044367926,0.500012436349707));
#133774=DIRECTION('ref_axis',(-0.405100113157865,-0.29309912217315,0.866017784402153));
#133775=DIRECTION('center_axis',(-0.428718122142726,-0.311481948263249,
-0.848044673146731));
#133776=DIRECTION('ref_axis',(0.892441805934765,-1.92098507058835E-15,-0.451162523953281));
#133777=DIRECTION('center_axis',(-0.404512555979938,-0.293895562537369,
-0.86602251147151));
#133778=DIRECTION('ref_axis',(-0.703251077800027,-0.505408667884764,0.500000000000049));
#133779=DIRECTION('center_axis',(0.404512560891371,0.293895578599951,0.866022503726378));
#133780=DIRECTION('ref_axis',(-0.906035256115534,2.25474787958917E-15,0.423202214875655));
#133781=DIRECTION('center_axis',(-0.428718110383991,-0.311481908460264,
-0.848044693710616));
#133782=DIRECTION('ref_axis',(-0.688740099734959,-0.494795562239232,0.529919264233185));
#133783=DIRECTION('center_axis',(-0.428718069290536,-0.311481909863907,
-0.848044713969333));
#133784=DIRECTION('ref_axis',(0.892441837073399,-2.5998686034382E-15,-0.451162462358136));
#133785=DIRECTION('center_axis',(0.809016994374931,0.587785252292496,4.1044824792529E-15));
#133786=DIRECTION('ref_axis',(0.587785252292496,-0.809016994374931,-6.82961998416073E-15));
#133787=DIRECTION('center_axis',(-0.80901699437495,-0.58778525229247,-4.10448247925272E-15));
#133788=DIRECTION('ref_axis',(-0.58778525229247,0.80901699437495,6.82961998416043E-15));
#133789=DIRECTION('center_axis',(0.809016994374947,0.587785252292474,4.21840575002201E-15));
#133790=DIRECTION('ref_axis',(0.587785252292474,-0.809016994374947,-6.82961998416063E-15));
#133791=DIRECTION('center_axis',(0.809016994374931,0.587785252292496,4.83067115377211E-14));
#133792=DIRECTION('ref_axis',(0.587785252292496,-0.809016994374931,-6.82961998416074E-15));
#133793=DIRECTION('center_axis',(0.809016994374947,0.587785252292474,4.21840575002201E-15));
#133794=DIRECTION('ref_axis',(0.587785252292474,-0.809016994374947,-6.82961998416063E-15));
#133795=DIRECTION('center_axis',(-0.700618669263898,-0.50907185116288,0.499979330205243));
#133796=DIRECTION('ref_axis',(-0.403924952204111,-0.294660197701536,-0.866036951219403));
#133797=DIRECTION('center_axis',(0.404512670528677,0.293895658256128,-0.866022425483287));
#133798=DIRECTION('ref_axis',(0.906035197473496,1.03251279233693E-15,0.423202340422597));
#133799=DIRECTION('center_axis',(0.404512677787197,0.293895663529747,-0.866022420303217));
#133800=DIRECTION('ref_axis',(-0.587785252301584,0.809016994368328,-6.47338699048409E-12));
#133801=DIRECTION('center_axis',(-0.371576139139117,-0.334568658445484,
-0.866022508719292));
#133802=DIRECTION('ref_axis',(0.669130606356112,-0.743144825479867,2.18984935677441E-12));
#133803=DIRECTION('center_axis',(-0.643597063368043,-0.579456972968032,
-0.500012436348095));
#133804=DIRECTION('ref_axis',(0.370919252614423,0.335308969664565,-0.866017784403095));
#133805=DIRECTION('center_axis',(0.371576145565852,0.334568664232078,0.866022503726311));
#133806=DIRECTION('ref_axis',(-0.918982183096513,9.95361655628204E-19,0.394299058014558));
#133807=DIRECTION('center_axis',(0.743144825477406,0.669130606358845,8.1834950149964E-14));
#133808=DIRECTION('ref_axis',(0.669130606358845,-0.743144825477406,-6.82961998416065E-15));
#133809=DIRECTION('center_axis',(-0.743144825477393,-0.669130606358859,
-4.77716140639646E-15));
#133810=DIRECTION('ref_axis',(-0.669130606358859,0.743144825477393,6.82961998416066E-15));
#133811=DIRECTION('center_axis',(-0.743144825477406,-0.669130606358845,
-4.6725140507014E-15));
#133812=DIRECTION('ref_axis',(-0.669130606358845,0.743144825477406,6.82961998416065E-15));
#133813=DIRECTION('center_axis',(-0.743144825477393,-0.669130606358859,
-4.77716140639646E-15));
#133814=DIRECTION('ref_axis',(-0.669130606358859,0.743144825477393,6.82961998416066E-15));
#133815=DIRECTION('center_axis',(0.743144825477382,0.669130606358872,4.67251405070159E-15));
#133816=DIRECTION('ref_axis',(0.669130606358872,-0.743144825477382,-6.82961998416048E-15));
#133817=DIRECTION('center_axis',(-0.393810436983632,-0.354588510146755,
0.848045003637582));
#133818=DIRECTION('ref_axis',(-0.906978223357768,3.01844662600193E-15,-0.421177518814558));
#133819=DIRECTION('center_axis',(0.371576246276125,0.334568754912027,-0.86602242548329));
#133820=DIRECTION('ref_axis',(0.918982131463642,-2.65789370359083E-15,0.394299178353875));
#133821=DIRECTION('center_axis',(0.393810401511434,0.354588507306632,-0.848045021297488));
#133822=DIRECTION('ref_axis',(0.627330796743794,0.570650194822807,0.529919264233231));
#133823=DIRECTION('center_axis',(-0.393810395274862,-0.35458847259201,0.84804503870863));
#133824=DIRECTION('ref_axis',(-0.906978247051284,-1.28220563798849E-15,
-0.421177467792117));
#133825=DIRECTION('center_axis',(0.371576249535771,0.334568771993211,-0.866022417485763));
#133826=DIRECTION('ref_axis',(0.640529840778939,0.582856348572902,0.499999999999971));
#133827=DIRECTION('center_axis',(0.643614221961138,0.579466481046779,-0.499979330205382));
#133828=DIRECTION('ref_axis',(0.372201885199337,0.33383492294369,0.866036951219312));
#133829=DIRECTION('center_axis',(-0.669310796197597,0.742982542253409,5.18821936272801E-15));
#133830=DIRECTION('ref_axis',(0.742982542253409,0.669310796197597,3.41480999208022E-15));
#133831=DIRECTION('center_axis',(-0.743144825477393,-0.669130606358859,
-4.77716140639646E-15));
#133832=DIRECTION('ref_axis',(-0.669130606358859,0.743144825477393,6.82961998416066E-15));
#133833=DIRECTION('center_axis',(0.743144825477382,0.669130606358872,4.67251405070159E-15));
#133834=DIRECTION('ref_axis',(0.669130606358872,-0.743144825477382,-6.82961998416048E-15));
#133835=DIRECTION('center_axis',(-3.61695511949416E-17,-6.88873777539344E-15,
1.));
#133836=DIRECTION('ref_axis',(0.,-1.,-6.88981142978601E-15));
#133837=DIRECTION('center_axis',(-0.668950377172406,0.743307065001333,5.19048549296483E-15));
#133838=DIRECTION('ref_axis',(0.743307065001333,0.668950377172406,3.41480999208041E-15));
#133839=DIRECTION('center_axis',(0.393810781475684,0.354588820328814,0.848044713969335));
#133840=DIRECTION('ref_axis',(-0.906978027661853,8.31337327814796E-16,0.421177940232647));
#133841=DIRECTION('center_axis',(0.39381039527486,0.354588472592008,-0.848045038708632));
#133842=DIRECTION('ref_axis',(0.906978247051285,2.28558738914555E-15,0.421177467792114));
#133843=DIRECTION('center_axis',(0.393810822584926,0.354588823413865,0.848044693589292));
#133844=DIRECTION('ref_axis',(-0.627180210713234,-0.570815694146828,0.529919264233126));
#133845=DIRECTION('center_axis',(0.393810830024562,0.354588864042297,0.848044673146739));
#133846=DIRECTION('ref_axis',(-0.906978000082633,2.36717991127537E-15,0.421177999622615));
#133847=DIRECTION('center_axis',(-0.393810401582745,-0.354588507464037,
0.848045021198559));
#133848=DIRECTION('ref_axis',(0.633098037497121,0.564245025066081,0.529919264233215));
#133849=DIRECTION('center_axis',(0.393810436983644,0.354588510146766,-0.848045003637571));
#133850=DIRECTION('ref_axis',(0.90697822335776,3.0270894602194E-15,0.421177518814575));
#133851=DIRECTION('center_axis',(-0.6693224492839,0.74297204448391,-3.13815977466195E-14));
#133852=DIRECTION('ref_axis',(0.74297204448391,0.6693224492839,3.41480999208017E-15));
#133853=DIRECTION('center_axis',(0.743144825477406,0.669130606358845,-3.18867480389152E-14));
#133854=DIRECTION('ref_axis',(0.669130606358845,-0.743144825477406,-6.82961998416065E-15));
#133855=DIRECTION('center_axis',(-3.61695511949416E-17,-6.88873777539344E-15,
1.));
#133856=DIRECTION('ref_axis',(0.,-1.,-6.89155720931161E-15));
#133857=DIRECTION('center_axis',(-0.668938718831589,0.743317556935091,5.19055875774668E-15));
#133858=DIRECTION('ref_axis',(0.743317556935091,0.668938718831589,3.41480999208028E-15));
#133859=DIRECTION('center_axis',(0.743144825477393,0.669130606358859,4.77716140639646E-15));
#133860=DIRECTION('ref_axis',(0.669130606358859,-0.743144825477393,-6.82961998416078E-15));
#133861=DIRECTION('center_axis',(0.643556859036851,0.579501624400588,0.500012436349041));
#133862=DIRECTION('ref_axis',(-0.372243731524368,-0.333837986812962,0.866017784402539));
#133863=DIRECTION('center_axis',(-0.393810830024468,-0.35458886404239,-0.848044673146743));
#133864=DIRECTION('ref_axis',(0.906978000082671,3.73207792763548E-15,-0.421177999622533));
#133865=DIRECTION('center_axis',(-0.371576142364556,-0.334568647739141,
-0.866022511471542));
#133866=DIRECTION('ref_axis',(-0.646569003445698,-0.576149740764733,0.499999999999968));
#133867=DIRECTION('center_axis',(0.371576145565767,0.334568664232001,0.866022503726377));
#133868=DIRECTION('ref_axis',(-0.918982183096556,1.80129298120473E-15,0.394299058014457));
#133869=DIRECTION('center_axis',(-0.393810822488479,-0.354588823230846,
-0.848044693710603));
#133870=DIRECTION('ref_axis',(-0.633246889645983,-0.564077964600818,0.529919264233229));
#133871=DIRECTION('center_axis',(-0.393810781475669,-0.354588820328858,
-0.848044713969324));
#133872=DIRECTION('ref_axis',(0.906978027661857,3.69392270454927E-16,-0.421177940232639));
#133873=DIRECTION('center_axis',(0.743144825477406,0.669130606358845,-3.18867480389132E-14));
#133874=DIRECTION('ref_axis',(0.669130606358845,-0.743144825477406,-6.82961998416065E-15));
#133875=DIRECTION('center_axis',(-0.743144825477406,-0.669130606358845,
-4.6725140507014E-15));
#133876=DIRECTION('ref_axis',(-0.669130606358845,0.743144825477406,6.82961998416065E-15));
#133877=DIRECTION('center_axis',(0.743144825477393,0.669130606358859,4.77716140639646E-15));
#133878=DIRECTION('ref_axis',(0.669130606358859,-0.743144825477393,-6.82961998416078E-15));
#133879=DIRECTION('center_axis',(0.743144825477406,0.669130606358845,-3.59306599589443E-14));
#133880=DIRECTION('ref_axis',(0.669130606358845,-0.743144825477406,-6.82961998416065E-15));
#133881=DIRECTION('center_axis',(0.743144825477393,0.669130606358859,4.77716140639646E-15));
#133882=DIRECTION('ref_axis',(0.669130606358859,-0.743144825477393,-6.82961998416078E-15));
#133883=DIRECTION('center_axis',(-0.643568108591872,-0.579517695131965,
0.499979330205175));
#133884=DIRECTION('ref_axis',(-0.370911831410088,-0.335267672826545,-0.866036951219454));
#133885=DIRECTION('center_axis',(0.371576246276117,0.33456875491202,-0.866022425483296));
#133886=DIRECTION('ref_axis',(0.918982131463646,-1.62026352763753E-15,0.394299178353866));
#133887=DIRECTION('center_axis',(0.371576252946869,0.334568760918362,-0.86602242030072));
#133888=DIRECTION('ref_axis',(-0.669130606356659,0.743144825479374,1.67407644653007E-12));
#133889=DIRECTION('center_axis',(-0.334568658443055,-0.371576139136519,
-0.866022508721346));
#133890=DIRECTION('ref_axis',(0.74314482547367,-0.669130606362995,3.24324994554054E-12));
#133891=DIRECTION('center_axis',(-0.579501624401049,-0.643556859036431,
-0.500012436349046));
#133892=DIRECTION('ref_axis',(0.333837986817552,0.372243731520247,-0.866017784402541));
#133893=DIRECTION('center_axis',(0.334568664232049,0.371576145565878,0.866022503726311));
#133894=DIRECTION('ref_axis',(1.29773672876362E-15,-0.918982183096502,0.394299058014582));
#133895=DIRECTION('center_axis',(0.669130606358845,0.743144825477406,5.1893525804244E-15));
#133896=DIRECTION('ref_axis',(0.743144825477406,-0.669130606358845,-3.41480999208033E-15));
#133897=DIRECTION('center_axis',(-0.669130606358857,-0.743144825477395,
-5.28357748271715E-15));
#133898=DIRECTION('ref_axis',(-0.743144825477395,0.669130606358857,3.41480999208033E-15));
#133899=DIRECTION('center_axis',(-0.669130606358845,-0.743144825477406,
-5.1893525804244E-15));
#133900=DIRECTION('ref_axis',(-0.743144825477406,0.669130606358845,3.41480999208033E-15));
#133901=DIRECTION('center_axis',(-0.669130606358857,-0.743144825477395,
-5.28357748271715E-15));
#133902=DIRECTION('ref_axis',(-0.743144825477395,0.669130606358857,3.41480999208033E-15));
#133903=DIRECTION('center_axis',(0.669130606358872,0.743144825477382,5.18935258042423E-15));
#133904=DIRECTION('ref_axis',(0.743144825477382,-0.669130606358872,-3.41480999208052E-15));
#133905=DIRECTION('center_axis',(-0.354588510146771,-0.393810436983662,
0.84804500363756));
#133906=DIRECTION('ref_axis',(-1.78940208541438E-15,-0.90697822335775,-0.421177518814595));
#133907=DIRECTION('center_axis',(0.334568754912014,0.371576246276123,-0.866022425483296));
#133908=DIRECTION('ref_axis',(-1.52738427012904E-15,0.918982131463644,0.394299178353872));
#133909=DIRECTION('center_axis',(0.354588475163086,0.39381043045359,-0.848045021297499));
#133910=DIRECTION('ref_axis',(0.564245025059182,0.63309803750328,0.529919264233202));
#133911=DIRECTION('center_axis',(-0.354588472592013,-0.393810395274878,
0.848045038708622));
#133912=DIRECTION('ref_axis',(-1.03488258956407E-15,-0.906978247051276,
-0.421177467792134));
#133913=DIRECTION('center_axis',(0.334568756368539,0.371576263604268,-0.866022417485772));
#133914=DIRECTION('ref_axis',(0.57609587287146,0.646617000441915,0.499999999999971));
#133915=DIRECTION('center_axis',(0.579517695131787,0.643568108591975,-0.499979330205249));
#133916=DIRECTION('ref_axis',(0.335267672846325,0.37091183139236,0.86603695121939));
#133917=DIRECTION('center_axis',(-0.743307065001336,0.668950377172403,4.67125551701904E-15));
#133918=DIRECTION('ref_axis',(0.668950377172402,0.743307065001336,6.82961998416069E-15));
#133919=DIRECTION('center_axis',(-0.669130606358857,-0.743144825477395,
-5.28357748271715E-15));
#133920=DIRECTION('ref_axis',(-0.743144825477395,0.669130606358857,3.41480999208033E-15));
#133921=DIRECTION('center_axis',(0.669130606358872,0.743144825477382,5.18935258042423E-15));
#133922=DIRECTION('ref_axis',(0.743144825477382,-0.669130606358872,-3.41480999208052E-15));
#133923=DIRECTION('center_axis',(-4.6592004597086E-17,-6.8783153219913E-15,
1.));
#133924=DIRECTION('ref_axis',(0.,-1.,-6.87570741457662E-15));
#133925=DIRECTION('center_axis',(-0.742982542253406,0.669310796197601,4.67377230962033E-15));
#133926=DIRECTION('ref_axis',(0.669310796197601,0.742982542253406,6.82961998416052E-15));
#133927=DIRECTION('center_axis',(0.354588820328813,0.393810781475708,0.848044713969324));
#133928=DIRECTION('ref_axis',(1.92894670706085E-15,-0.906978027661841,0.421177940232672));
#133929=DIRECTION('center_axis',(0.354588472591992,0.393810395274855,-0.848045038708641));
#133930=DIRECTION('ref_axis',(2.31305154500925E-15,0.906978247051289,0.421177467792106));
#133931=DIRECTION('center_axis',(0.354588860892955,0.393810788838664,0.848044693589262));
#133932=DIRECTION('ref_axis',(-0.564077964589757,-0.633246889655851,0.529919264233211));
#133933=DIRECTION('center_axis',(0.354588864042362,0.393810830024493,0.848044673146744));
#133934=DIRECTION('ref_axis',(-1.94575173309401E-15,-0.906978000082661,
0.421177999622554));
#133935=DIRECTION('center_axis',(-0.354588475221977,-0.393810430613613,
0.848045021198565));
#133936=DIRECTION('ref_axis',(0.570650194822096,0.627330796744435,0.529919264233239));
#133937=DIRECTION('center_axis',(0.35458851014676,0.39381043698365,-0.848045003637571));
#133938=DIRECTION('ref_axis',(3.38703812945195E-15,0.906978223357757,0.42117751881458));
#133939=DIRECTION('center_axis',(-0.743317556935091,0.668938718831589,4.67117410726026E-15));
#133940=DIRECTION('ref_axis',(0.668938718831589,0.743317556935091,6.82961998416059E-15));
#133941=DIRECTION('center_axis',(0.669130606358845,0.743144825477406,5.1893525804244E-15));
#133942=DIRECTION('ref_axis',(0.743144825477406,-0.669130606358845,-3.41480999208033E-15));
#133943=DIRECTION('center_axis',(-4.6592004597086E-17,-6.8783153219913E-15,
1.));
#133944=DIRECTION('ref_axis',(0.,-1.,-6.87654292345255E-15));
#133945=DIRECTION('center_axis',(-0.742972044483927,0.669322449283882,6.49863705058621E-16));
#133946=DIRECTION('ref_axis',(0.669322449283881,0.742972044483927,6.82961998416067E-15));
#133947=DIRECTION('center_axis',(0.669130606358857,0.743144825477395,5.28357748271715E-15));
#133948=DIRECTION('ref_axis',(0.743144825477395,-0.669130606358857,-3.41480999208041E-15));
#133949=DIRECTION('center_axis',(0.579456972966333,0.643597063368587,0.500012436349362));
#133950=DIRECTION('ref_axis',(-0.335308969659004,-0.370919252621144,0.86601778440237));
#133951=DIRECTION('center_axis',(-0.354588864042302,-0.393810830024557,
-0.848044673146739));
#133952=DIRECTION('ref_axis',(-1.8722112353852E-15,0.906978000082635,-0.421177999622611));
#133953=DIRECTION('center_axis',(-0.334568662772281,-0.371576128828631,
-0.866022511471553));
#133954=DIRECTION('ref_axis',(-0.582802983775234,-0.640578396531379,0.499999999999971));
#133955=DIRECTION('center_axis',(0.334568664232006,0.37157614556576,0.866022503726378));
#133956=DIRECTION('ref_axis',(1.39319519318679E-15,-0.918982183096559,0.39429905801445));
#133957=DIRECTION('center_axis',(-0.354588860821328,-0.393810788641775,
-0.848044693710641));
#133958=DIRECTION('ref_axis',(-0.570815694135724,-0.627180210723296,0.529919264233179));
#133959=DIRECTION('center_axis',(-0.354588820328737,-0.393810781475754,
-0.848044713969335));
#133960=DIRECTION('ref_axis',(2.97237289164332E-15,0.906978027661824,-0.421177940232709));
#133961=DIRECTION('center_axis',(0.669130606358845,0.743144825477406,9.23326450045792E-15));
#133962=DIRECTION('ref_axis',(0.743144825477406,-0.669130606358845,-3.41480999208032E-15));
#133963=DIRECTION('center_axis',(-0.669130606358875,-0.743144825477379,
-5.18935258042421E-15));
#133964=DIRECTION('ref_axis',(-0.743144825477379,0.669130606358875,3.41480999208015E-15));
#133965=DIRECTION('center_axis',(0.669130606358857,0.743144825477395,5.28357748271715E-15));
#133966=DIRECTION('ref_axis',(0.743144825477395,-0.669130606358857,-3.41480999208041E-15));
#133967=DIRECTION('center_axis',(0.669130606358845,0.743144825477406,5.1893525804244E-15));
#133968=DIRECTION('ref_axis',(0.743144825477406,-0.669130606358845,-3.41480999208033E-15));
#133969=DIRECTION('center_axis',(0.669130606358857,0.743144825477395,5.28357748271715E-15));
#133970=DIRECTION('ref_axis',(0.743144825477395,-0.669130606358857,-3.41480999208041E-15));
#133971=DIRECTION('center_axis',(-0.579466481046696,-0.64361422196136,0.499979330205192));
#133972=DIRECTION('ref_axis',(-0.333834922952809,-0.372201885190879,-0.866036951219431));
#133973=DIRECTION('center_axis',(0.334568754912021,0.371576246276131,-0.86602242548329));
#133974=DIRECTION('ref_axis',(-2.58413282129854E-15,0.91898213146364,0.39429917835388));
#133975=DIRECTION('center_axis',(0.334568760922057,0.371576252950874,-0.866022420297574));
#133976=DIRECTION('ref_axis',(-0.743144825476543,0.669130606359804,6.94982127933865E-13));
#133977=DIRECTION('center_axis',(-0.293895573516141,-0.404512553894111,
-0.86602250872));
#133978=DIRECTION('ref_axis',(0.809016994375186,-0.587785252292144,-2.31660710397836E-13));
#133979=DIRECTION('center_axis',(-0.509057044366969,-0.70060580148708,-0.50001243634835));
#133980=DIRECTION('ref_axis',(0.293099122185064,0.405100113147538,-0.866017784402951));
#133981=DIRECTION('center_axis',(0.293895578600017,0.404512560891464,0.866022503726313));
#133982=DIRECTION('ref_axis',(1.58451773583043E-15,-0.906035256115484,0.42320221487576));
#133983=DIRECTION('center_axis',(0.587785252292434,0.809016994374976,5.64933547733438E-15));
#133984=DIRECTION('ref_axis',(0.809016994374976,-0.587785252292434,-3.41480999208033E-15));
#133985=DIRECTION('center_axis',(-0.587785252292471,-0.809016994374949,
-5.73210557847752E-15));
#133986=DIRECTION('ref_axis',(-0.809016994374949,0.587785252292471,3.41480999208033E-15));
#133987=DIRECTION('center_axis',(-0.587785252292496,-0.809016994374931,
-5.64933547733406E-15));
#133988=DIRECTION('ref_axis',(-0.809016994374931,0.587785252292496,3.41480999208037E-15));
#133989=DIRECTION('center_axis',(-0.587785252292471,-0.809016994374949,
-5.73210557847752E-15));
#133990=DIRECTION('ref_axis',(-0.809016994374949,0.587785252292471,3.41480999208033E-15));
#133991=DIRECTION('center_axis',(0.58778525229247,0.80901699437495,5.6493354773342E-15));
#133992=DIRECTION('ref_axis',(0.80901699437495,-0.58778525229247,-3.41480999208022E-15));
#133993=DIRECTION('center_axis',(-0.311481637390324,-0.428717694262781,
0.848045003637571));
#133994=DIRECTION('ref_axis',(1.27173423926985E-15,-0.892442058026259,-0.451162025292307));
#133995=DIRECTION('center_axis',(0.293895658256083,0.404512670528694,-0.866022425483294));
#133996=DIRECTION('ref_axis',(8.91224751768462E-16,0.90603519747349,0.423202340422609));
#133997=DIRECTION('center_axis',(0.311481603280417,0.42871768411203,-0.848045021297501));
#133998=DIRECTION('ref_axis',(0.49497726682106,0.688609525583905,0.529919264233205));
#133999=DIRECTION('center_axis',(-0.31148160440103,-0.428717648856912,0.848045038708654));
#134000=DIRECTION('ref_axis',(-1.86658406301952E-15,-0.89244208477774,-0.451161972375289));
#134001=DIRECTION('center_axis',(0.293895657889663,0.404512687916895,-0.866022417485743));
#134002=DIRECTION('ref_axis',(0.50535007802797,0.703293181139326,0.500000000000052));
#134003=DIRECTION('center_axis',(0.50907185116279,0.700618669263949,-0.499979330205263));
#134004=DIRECTION('ref_axis',(0.294660197700626,0.403924952204797,0.866036951219393));
#134005=DIRECTION('center_axis',(-0.809159506053914,0.587589051772227,4.10311241834253E-15));
#134006=DIRECTION('ref_axis',(0.587589051772227,0.809159506053914,6.82961998416088E-15));
#134007=DIRECTION('center_axis',(-0.587785252292471,-0.809016994374949,
-5.73210557847752E-15));
#134008=DIRECTION('ref_axis',(-0.809016994374949,0.587785252292471,3.41480999208033E-15));
#134009=DIRECTION('center_axis',(0.58778525229246,0.809016994374957,5.64933547733425E-15));
#134010=DIRECTION('ref_axis',(0.809016994374957,-0.58778525229246,-3.41480999208051E-15));
#134011=DIRECTION('center_axis',(-5.8046805746579E-17,-6.86903940691701E-15,
1.));
#134012=DIRECTION('ref_axis',(0.,-1.,-6.86865540697193E-15));
#134013=DIRECTION('center_axis',(-0.808874435122371,0.587981418248456,4.10585229880201E-15));
#134014=DIRECTION('ref_axis',(0.587981418248456,0.808874435122371,6.82961998416081E-15));
#134015=DIRECTION('center_axis',(0.311481909863959,0.428718069290514,0.848044713969325));
#134016=DIRECTION('ref_axis',(2.35220027834147E-15,-0.892441837073406,0.451162462358122));
#134017=DIRECTION('center_axis',(0.311481604401026,0.428717648856907,-0.848045038708658));
#134018=DIRECTION('ref_axis',(2.02341423291377E-15,0.892442084777743,0.451161972375283));
#134019=DIRECTION('center_axis',(0.311481949432559,0.428718080855898,0.848044693589276));
#134020=DIRECTION('ref_axis',(-0.494795562222334,-0.688740099747117,0.529919264233162));
#134021=DIRECTION('center_axis',(0.311481948263326,0.428718122142669,0.848044673146731));
#134022=DIRECTION('ref_axis',(-1.24965575049336E-15,-0.892441805934789,
0.451162523953235));
#134023=DIRECTION('center_axis',(-0.311481603316802,-0.428717684281317,
0.848045021198556));
#134024=DIRECTION('ref_axis',(0.501950189217994,0.683543400918034,0.529919264233174));
#134025=DIRECTION('center_axis',(0.311481637390342,0.428717694262806,-0.848045003637552));
#134026=DIRECTION('ref_axis',(-3.7555222267109E-15,0.892442058026244,0.451162025292335));
#134027=DIRECTION('center_axis',(-0.809168721883308,0.587576360591314,-1.04314267264197E-13));
#134028=DIRECTION('ref_axis',(0.587576360591314,0.809168721883308,6.82961998416204E-15));
#134029=DIRECTION('center_axis',(0.587785252292496,0.809016994374931,-3.85528935811366E-14));
#134030=DIRECTION('ref_axis',(0.809016994374931,-0.587785252292496,-3.41480999208037E-15));
#134031=DIRECTION('center_axis',(-5.8046805746579E-17,-6.86903940691701E-15,
1.));
#134032=DIRECTION('ref_axis',(0.,-1.,-6.86903578052301E-15));
#134033=DIRECTION('center_axis',(-0.808865212939984,0.587994104813606,4.10594088861296E-15));
#134034=DIRECTION('ref_axis',(0.587994104813606,0.808865212939984,6.82961998416048E-15));
#134035=DIRECTION('center_axis',(0.587785252292471,0.809016994374949,5.73210557847752E-15));
#134036=DIRECTION('ref_axis',(0.809016994374949,-0.587785252292471,-3.41480999208039E-15));
#134037=DIRECTION('center_axis',(0.509008435041023,0.700641118228729,0.500012436349622));
#134038=DIRECTION('ref_axis',(-0.29470049257112,-0.403936649460554,0.866017784402214));
#134039=DIRECTION('center_axis',(-0.311481948263287,-0.428718122142695,
-0.848044673146732));
#134040=DIRECTION('ref_axis',(-4.34287574111871E-16,0.892441805934778,-0.451162523953256));
#134041=DIRECTION('center_axis',(-0.293895578893428,-0.40451254409655,-0.866022511471517));
#134042=DIRECTION('ref_axis',(-0.512651652661814,-0.697988741329765,0.500000000000001));
#134043=DIRECTION('center_axis',(0.293895578599952,0.404512560891358,0.866022503726384));
#134044=DIRECTION('ref_axis',(1.61736368199052E-15,-0.90603525611554,0.423202214875642));
#134045=DIRECTION('center_axis',(-0.311481949381041,-0.42871808065328,-0.848044693710629));
#134046=DIRECTION('ref_axis',(-0.502130522411202,-0.683410939228823,0.529919264233177));
#134047=DIRECTION('center_axis',(-0.311481909863924,-0.428718069290534,
-0.848044713969328));
#134048=DIRECTION('ref_axis',(-2.96332432358735E-15,0.892441837073399,-0.451162462358137));
#134049=DIRECTION('center_axis',(0.587785252292496,0.809016994374931,5.64933547733406E-15));
#134050=DIRECTION('ref_axis',(0.809016994374931,-0.587785252292496,-3.41480999208037E-15));
#134051=DIRECTION('center_axis',(-0.587785252292496,-0.809016994374931,
-5.64933547733406E-15));
#134052=DIRECTION('ref_axis',(-0.809016994374931,0.587785252292496,3.41480999208037E-15));
#134053=DIRECTION('center_axis',(0.587785252292471,0.809016994374949,5.73210557847752E-15));
#134054=DIRECTION('ref_axis',(0.809016994374949,-0.587785252292471,-3.41480999208039E-15));
#134055=DIRECTION('center_axis',(0.587785252292496,0.809016994374931,-5.85802630098928E-14));
#134056=DIRECTION('ref_axis',(0.809016994374931,-0.587785252292496,-3.41480999208036E-15));
#134057=DIRECTION('center_axis',(0.587785252292471,0.809016994374949,5.73210557847752E-15));
#134058=DIRECTION('ref_axis',(0.809016994374949,-0.587785252292471,-3.41480999208039E-15));
#134059=DIRECTION('center_axis',(-0.509016097474232,-0.700659176689747,
0.499979330205309));
#134060=DIRECTION('ref_axis',(-0.293100449224596,-0.405058175805674,-0.866036951219357));
#134061=DIRECTION('center_axis',(0.293895658256105,0.40451267052866,-0.866022425483303));
#134062=DIRECTION('ref_axis',(2.49577890397111E-15,0.906035197473505,0.423202340422576));
#134063=DIRECTION('center_axis',(0.293895663532304,0.40451267779073,-0.866022420300699));
#134064=DIRECTION('ref_axis',(-0.809016994372974,0.587785252295189,1.92322098297828E-12));
#134065=DIRECTION('center_axis',(-0.250002507179345,-0.433017044454286,
-0.866022508723715));
#134066=DIRECTION('ref_axis',(0.866025403784602,-0.499999999999718,-1.57354444798448E-13));
#134067=DIRECTION('center_axis',(-0.433035128830198,-0.749978760162002,
-0.500012436350217));
#134068=DIRECTION('ref_axis',(0.249149002240785,0.433518133164088,-0.866017784401882));
#134069=DIRECTION('center_axis',(0.250002511507192,0.433017051950262,0.866022503726318));
#134070=DIRECTION('ref_axis',(-4.36628801622752E-16,-0.894424794863792,
0.44721838774011));
#134071=DIRECTION('center_axis',(0.50000000000001,0.866025403784433,6.04742307255487E-15));
#134072=DIRECTION('ref_axis',(0.866025403784433,-0.50000000000001,-3.41480999208034E-15));
#134073=DIRECTION('center_axis',(-0.499999999999998,-0.86602540378444,-6.11783152599988E-15));
#134074=DIRECTION('ref_axis',(-0.86602540378444,0.499999999999998,3.41480999208033E-15));
#134075=DIRECTION('center_axis',(-0.50000000000001,-0.866025403784433,-6.04742307255487E-15));
#134076=DIRECTION('ref_axis',(-0.866025403784433,0.50000000000001,3.41480999208034E-15));
#134077=DIRECTION('center_axis',(-0.499999999999998,-0.86602540378444,-6.11783152599988E-15));
#134078=DIRECTION('ref_axis',(-0.86602540378444,0.499999999999998,3.41480999208033E-15));
#134079=DIRECTION('center_axis',(0.499999999999998,0.86602540378444,6.04742307255492E-15));
#134080=DIRECTION('ref_axis',(0.86602540378444,-0.499999999999998,-3.41480999208026E-15));
#134081=DIRECTION('center_axis',(-0.264962106632886,-0.458927830768635,
0.848045003637578));
#134082=DIRECTION('ref_axis',(1.98079904364529E-16,-0.879478602053326,-0.47593842934809));
#134083=DIRECTION('center_axis',(0.250002579266718,0.433017169313216,-0.866022425483289));
#134084=DIRECTION('ref_axis',(6.12936842783791E-16,0.894424730216417,0.447218517033106));
#134085=DIRECTION('center_axis',(0.264962073775778,0.458927817105223,-0.848045021297498));
#134086=DIRECTION('ref_axis',(0.420286434071742,0.736576463600215,0.529919264233205));
#134087=DIRECTION('center_axis',(-0.264962078570523,-0.458927782163196,
0.848045038708651));
#134088=DIRECTION('ref_axis',(-1.14611944484251E-15,-0.879478631391255,
-0.475938375135022));
#134089=DIRECTION('center_axis',(0.25000257708854,0.433017186565615,-0.866022417485764));
#134090=DIRECTION('ref_axis',(0.429067561974734,0.752263934574208,0.499999999999989));
#134091=DIRECTION('center_axis',(0.433048509462478,0.749993105181596,-0.499979330205153));
#134092=DIRECTION('ref_axis',(0.250824363776623,0.432512586705358,0.866036951219457));
#134093=DIRECTION('center_axis',(-0.866146626230631,0.499789977759954,3.49001476137941E-15));
#134094=DIRECTION('ref_axis',(0.499789977759954,0.866146626230631,6.82961998416062E-15));
#134095=DIRECTION('center_axis',(-0.499999999999998,-0.86602540378444,-6.11783152599988E-15));
#134096=DIRECTION('ref_axis',(-0.86602540378444,0.499999999999998,3.41480999208033E-15));
#134097=DIRECTION('center_axis',(0.500000000000051,0.866025403784409,6.04742307255471E-15));
#134098=DIRECTION('ref_axis',(0.866025403784409,-0.500000000000051,-3.41480999208024E-15));
#134099=DIRECTION('center_axis',(-7.04084534449556E-17,-6.86101165903726E-15,
1.));
#134100=DIRECTION('ref_axis',(0.,-1.,-6.86160339936723E-15));
#134101=DIRECTION('center_axis',(-0.865904130412286,0.500209992837952,3.49294771099313E-15));
#134102=DIRECTION('ref_axis',(0.500209992837952,0.865904130412285,6.82961998416082E-15));
#134103=DIRECTION('center_axis',(0.264962338412812,0.458928232223232,0.848044713969301));
#134104=DIRECTION('ref_axis',(-3.05791874716061E-15,-0.879478359737727,
0.47593887711873));
#134105=DIRECTION('center_axis',(0.264962078570518,0.458927782163202,-0.84804503870865));
#134106=DIRECTION('ref_axis',(1.10726528648156E-15,0.879478631391252,0.475938375135027));
#134107=DIRECTION('center_axis',(0.264962376554839,0.45892824786176,0.848044693589287));
#134108=DIRECTION('ref_axis',(-0.420092076161922,-0.736687329157012,0.529919264233218));
#134109=DIRECTION('center_axis',(0.264962371077221,0.458928288799647,0.848044673146743));
#134110=DIRECTION('ref_axis',(-4.96536252013644E-16,-0.879478325588514,
0.475938940222403));
#134111=DIRECTION('center_axis',(-0.264962073795953,-0.458927817276387,
0.848045021198568));
#134112=DIRECTION('ref_axis',(0.427750712262654,0.732266960577407,0.529919264233259));
#134113=DIRECTION('center_axis',(0.264962106632913,0.458927830768697,-0.848045003637535));
#134114=DIRECTION('ref_axis',(1.9774222481973E-15,0.879478602053289,0.475938429348159));
#134115=DIRECTION('center_axis',(-0.86615446498511,0.499776392786171,3.48991989801451E-15));
#134116=DIRECTION('ref_axis',(0.499776392786171,0.86615446498511,6.82961998416069E-15));
#134117=DIRECTION('center_axis',(0.50000000000001,0.866025403784433,-7.61181689576648E-15));
#134118=DIRECTION('ref_axis',(0.866025403784433,-0.50000000000001,-3.41480999208034E-15));
#134119=DIRECTION('center_axis',(-7.04084534449556E-17,-6.86101165903726E-15,
1.));
#134120=DIRECTION('ref_axis',(0.,-1.,-6.86152863759348E-15));
#134121=DIRECTION('center_axis',(-0.865896284857144,0.500223573885314,-1.6486202689183E-14));
#134122=DIRECTION('ref_axis',(0.500223573885314,0.865896284857144,6.8296199841604E-15));
#134123=DIRECTION('center_axis',(0.499999999999998,0.86602540378444,6.11783152599988E-15));
#134124=DIRECTION('ref_axis',(0.86602540378444,-0.499999999999998,-3.41480999208026E-15));
#134125=DIRECTION('center_axis',(0.432983094183966,0.750008802379043,0.500012436350171));
#134126=DIRECTION('ref_axis',(-0.250863215247218,-0.432528431823293,0.866017784401863));
#134127=DIRECTION('center_axis',(-0.264962371077247,-0.458928288799642,
-0.848044673146737));
#134128=DIRECTION('ref_axis',(7.54047727203941E-16,0.879478325588514,-0.475938940222403));
#134129=DIRECTION('center_axis',(-0.250002513555107,-0.433017035277681,
-0.86602251147153));
#134130=DIRECTION('ref_axis',(-0.436883602753634,-0.747751775420824,0.500000000000011));
#134131=DIRECTION('center_axis',(0.250002511507137,0.433017051950166,0.866022503726382));
#134132=DIRECTION('ref_axis',(-2.6848219789663E-16,-0.894424794863845,0.447218387740004));
#134133=DIRECTION('center_axis',(-0.264962376528037,-0.458928247653003,
-0.848044693710631));
#134134=DIRECTION('ref_axis',(-0.427943903632674,-0.732154074453082,0.529919264233127));
#134135=DIRECTION('center_axis',(-0.264962338412751,-0.458928232223233,
-0.848044713969319));
#134136=DIRECTION('ref_axis',(-3.1300340695229E-15,0.879478359737731,-0.475938877118722));
#134137=DIRECTION('center_axis',(0.50000000000001,0.866025403784433,-6.85880520999069E-14));
#134138=DIRECTION('ref_axis',(0.866025403784433,-0.50000000000001,-3.41480999208034E-15));
#134139=DIRECTION('center_axis',(-0.499999999999998,-0.86602540378444,-6.04742307255492E-15));
#134140=DIRECTION('ref_axis',(-0.86602540378444,0.499999999999998,3.41480999208026E-15));
#134141=DIRECTION('center_axis',(0.499999999999998,0.86602540378444,6.11783152599988E-15));
#134142=DIRECTION('ref_axis',(0.86602540378444,-0.499999999999998,-3.41480999208026E-15));
#134143=DIRECTION('center_axis',(0.50000000000001,0.866025403784433,-4.12695721632601E-14));
#134144=DIRECTION('ref_axis',(0.866025403784433,-0.50000000000001,-3.41480999208034E-15));
#134145=DIRECTION('center_axis',(0.499999999999998,0.86602540378444,6.11783152599988E-15));
#134146=DIRECTION('ref_axis',(0.86602540378444,-0.499999999999998,-3.41480999208026E-15));
#134147=DIRECTION('center_axis',(-0.432988827019191,-0.750027562856308,
0.499979330205132));
#134148=DIRECTION('ref_axis',(-0.249154705657247,-0.433476564270011,-0.866036951219471));
#134149=DIRECTION('center_axis',(0.250002579266723,0.433017169313225,-0.866022425483282));
#134150=DIRECTION('ref_axis',(2.19053741258821E-17,0.894424730216412,0.447218517033116));
#134151=DIRECTION('center_axis',(0.250002583755455,0.433017177087939,-0.866022420300069));
#134152=DIRECTION('ref_axis',(-0.86602540378426,0.500000000000309,2.22918795752825E-13));
#134153=DIRECTION('center_axis',(-0.203370361061543,-0.456777309666408,
-0.866022508723426));
#134154=DIRECTION('ref_axis',(0.913545457644901,-0.406736643070633,-3.26510472955345E-12));
#134155=DIRECTION('center_axis',(-0.35226878980237,-0.791134794599544,-0.500012436350449));
#134156=DIRECTION('ref_axis',(0.202469153687492,0.457186437796381,-0.866017784401756));
#134157=DIRECTION('center_axis',(0.203370364581923,0.456777317573264,0.866022503726311));
#134158=DIRECTION('ref_axis',(-1.56869163259611E-15,-0.884507036382102,
0.466526850878436));
#134159=DIRECTION('center_axis',(0.406736643075797,0.913545457642603,6.37925383508811E-15));
#134160=DIRECTION('ref_axis',(0.913545457642603,-0.406736643075797,-3.41480999208023E-15));
#134161=DIRECTION('center_axis',(-0.406736643075798,-0.913545457642602,
-6.43652923108483E-15));
#134162=DIRECTION('ref_axis',(-0.913545457642602,0.406736643075798,3.41480999208033E-15));
#134163=DIRECTION('center_axis',(-0.406736643075807,-0.913545457642598,
-6.37925383508808E-15));
#134164=DIRECTION('ref_axis',(-0.913545457642598,0.406736643075807,3.4148099920803E-15));
#134165=DIRECTION('center_axis',(-0.406736643075798,-0.913545457642602,
-6.43652923108483E-15));
#134166=DIRECTION('ref_axis',(-0.913545457642602,0.406736643075798,3.41480999208033E-15));
#134167=DIRECTION('center_axis',(0.406736643075817,0.913545457642594,6.37925383508805E-15));
#134168=DIRECTION('ref_axis',(0.913545457642593,-0.406736643075817,-3.41480999208037E-15));
#134169=DIRECTION('center_axis',(-0.215539595588311,-0.484109857923786,
0.848045003637566));
#134170=DIRECTION('ref_axis',(1.22794633366769E-15,-0.868458021515985,-0.495762710240031));
#134171=DIRECTION('center_axis',(0.203370419702463,0.456777441376078,-0.866022425483294));
#134172=DIRECTION('ref_axis',(-1.81222983169436E-15,0.884506966812057,0.466526982779062));
#134173=DIRECTION('center_axis',(0.21553956433415,0.484109840903014,-0.848045021297516));
#134174=DIRECTION('ref_axis',(0.340990855172982,0.776473315757201,0.529919264233163));
#134175=DIRECTION('center_axis',(-0.215539572760312,-0.48410980665126,0.848045038708666));
#134176=DIRECTION('ref_axis',(-2.44700238975538E-15,-0.868458052949974,
-0.495762655175175));
#134177=DIRECTION('center_axis',(0.203370415728145,0.456777458308414,-0.866022417485752));
#134178=DIRECTION('ref_axis',(0.348084091910994,0.792992726926611,0.499999999999996));
#134179=DIRECTION('center_axis',(0.352280597671115,0.791150459692777,-0.499979330205149));
#134180=DIRECTION('ref_axis',(0.204240445631702,0.456361522798167,0.866036951219463));
#134181=DIRECTION('center_axis',(-0.913644062717548,0.406515100163541,2.8386797723579E-15));
#134182=DIRECTION('ref_axis',(0.406515100163541,0.913644062717548,6.82961998416062E-15));
#134183=DIRECTION('center_axis',(-0.406736643075798,-0.913545457642602,
-6.43652923108483E-15));
#134184=DIRECTION('ref_axis',(-0.913545457642602,0.406736643075798,3.41480999208033E-15));
#134185=DIRECTION('center_axis',(0.406736643075807,0.913545457642598,6.37925383508808E-15));
#134186=DIRECTION('ref_axis',(0.913545457642598,-0.406736643075807,-3.4148099920803E-15));
#134187=DIRECTION('center_axis',(-8.35415108931911E-17,-6.85432003203771E-15,
1.));
#134188=DIRECTION('ref_axis',(0.,-1.,-6.85455139176254E-15));
#134189=DIRECTION('center_axis',(-0.913446798847332,0.406958162070208,2.84177365711606E-15));
#134190=DIRECTION('ref_axis',(0.406958162070208,0.913446798847332,6.82961998416058E-15));
#134191=DIRECTION('center_axis',(0.215539784135028,0.484110281406733,0.848044713969328));
#134192=DIRECTION('ref_axis',(-1.26159198727182E-15,-0.86845776188828,0.495763165045568));
#134193=DIRECTION('center_axis',(0.215539572760318,0.484109806651275,-0.848045038708655));
#134194=DIRECTION('ref_axis',(1.56117104191503E-15,0.868458052949965,0.495762655175191));
#134195=DIRECTION('center_axis',(0.215539820433354,0.484110300946589,0.848044693589295));
#134196=DIRECTION('ref_axis',(-0.340785973376786,-0.776563258044201,0.529919264233158));
#134197=DIRECTION('center_axis',(0.215539810706706,0.4841103410876,0.848044673146743));
#134198=DIRECTION('ref_axis',(-1.47259052727932E-15,-0.868457725299275,
0.495763229140694));
#134199=DIRECTION('center_axis',(-0.215539564338139,-0.484109841074578,
0.848045021198564));
#134200=DIRECTION('ref_axis',(0.348864709021599,0.772967650159955,0.529919264233216));
#134201=DIRECTION('center_axis',(0.215539595588311,0.484109857923786,-0.848045003637566));
#134202=DIRECTION('ref_axis',(-1.22794633366769E-15,0.868458021515985,0.495762710240031));
#134203=DIRECTION('center_axis',(-0.913650438514067,0.406500770236727,2.7798120880666E-14));
#134204=DIRECTION('ref_axis',(0.406500770236727,0.913650438514067,6.82961998416101E-15));
#134205=DIRECTION('center_axis',(0.406736643075807,0.913545457642598,6.37925383508808E-15));
#134206=DIRECTION('ref_axis',(0.913545457642598,-0.406736643075807,-3.4148099920803E-15));
#134207=DIRECTION('center_axis',(-8.35415108931911E-17,-6.85432003203771E-15,
1.));
#134208=DIRECTION('ref_axis',(0.,-1.,-6.85402149466395E-15));
#134209=DIRECTION('center_axis',(-0.913440415876952,0.406972488803039,1.23809565966439E-16));
#134210=DIRECTION('ref_axis',(0.406972488803039,0.913440415876953,6.82961998416061E-15));
#134211=DIRECTION('center_axis',(0.406736643075798,0.913545457642602,6.43652923108483E-15));
#134212=DIRECTION('ref_axis',(0.913545457642602,-0.406736643075798,-3.41480999208024E-15));
#134213=DIRECTION('center_axis',(0.352213899942024,0.791159233141463,0.500012436347979));
#134214=DIRECTION('ref_axis',(-0.204277427918833,-0.456381342234996,0.866017784403213));
#134215=DIRECTION('center_axis',(-0.215539810706709,-0.484110341087593,
-0.848044673146745));
#134216=DIRECTION('ref_axis',(1.74357575843794E-15,0.868457725299279,-0.495763229140688));
#134217=DIRECTION('center_axis',(-0.203370368360526,-0.456777301206467,
-0.866022511471521));
#134218=DIRECTION('ref_axis',(-0.356328964673919,-0.789322284579871,0.500000000000026));
#134219=DIRECTION('center_axis',(0.203370364581877,0.456777317573187,0.866022503726363));
#134220=DIRECTION('ref_axis',(-7.57999114950329E-16,-0.884507036382146,
0.466526850878353));
#134221=DIRECTION('center_axis',(-0.215539820428636,-0.484110300736156,
-0.84804469371062));
#134222=DIRECTION('ref_axis',(-0.349068641879027,-0.772875576436027,0.529919264233156));
#134223=DIRECTION('center_axis',(-0.21553978413504,-0.484110281406725,-0.84804471396933));
#134224=DIRECTION('ref_axis',(1.68002389095411E-15,0.868457761888284,-0.495763165045561));
#134225=DIRECTION('center_axis',(0.406736643075807,0.913545457642598,6.37925383508808E-15));
#134226=DIRECTION('ref_axis',(0.913545457642598,-0.406736643075807,-3.4148099920803E-15));
#134227=DIRECTION('center_axis',(-0.406736643075797,-0.913545457642603,
-6.37925383508811E-15));
#134228=DIRECTION('ref_axis',(-0.913545457642603,0.406736643075797,3.41480999208023E-15));
#134229=DIRECTION('center_axis',(0.406736643075798,0.913545457642602,6.43652923108483E-15));
#134230=DIRECTION('ref_axis',(0.913545457642602,-0.406736643075798,-3.41480999208024E-15));
#134231=DIRECTION('center_axis',(0.406736643075807,0.913545457642598,-4.35340926765517E-14));
#134232=DIRECTION('ref_axis',(0.913545457642598,-0.406736643075807,-3.4148099920803E-15));
#134233=DIRECTION('center_axis',(0.406736643075798,0.913545457642602,6.43652923108483E-15));
#134234=DIRECTION('ref_axis',(0.913545457642602,-0.406736643075798,-3.41480999208024E-15));
#134235=DIRECTION('center_axis',(-0.352217640366521,-0.791178490090796,
0.499979330205049));
#134236=DIRECTION('ref_axis',(-0.202479170981813,-0.457145692794892,-0.866036951219517));
#134237=DIRECTION('center_axis',(0.20337041970247,0.456777441376081,-0.866022425483291));
#134238=DIRECTION('ref_axis',(-2.00922857707489E-15,0.884506966812055,0.466526982779065));
#134239=DIRECTION('center_axis',(0.203370423351993,0.456777449573005,-0.866022420302853));
#134240=DIRECTION('ref_axis',(-0.91354545764246,0.406736643076116,1.61725400840202E-13));
#134241=DIRECTION('center_axis',(-0.154510046710251,-0.475533027088399,
-0.866022508722343));
#134242=DIRECTION('ref_axis',(0.951056516294649,-0.309016994376501,9.57239539185634E-13));
#134243=DIRECTION('center_axis',(-0.267642920194609,-0.823622990673633,
-0.50001243634886));
#134244=DIRECTION('ref_axis',(0.153571010704088,0.475845712147976,-0.866017784402671));
#134245=DIRECTION('center_axis',(0.154510049384272,0.475533035318147,0.866022503726306));
#134246=DIRECTION('ref_axis',(1.85643597775053E-15,-0.876548788012432,0.481313018974073));
#134247=DIRECTION('center_axis',(0.309016994374956,0.951056516295151,5.86040288757031E-14));
#134248=DIRECTION('ref_axis',(0.951056516295151,-0.309016994374956,-3.41480999207978E-15));
#134249=DIRECTION('center_axis',(-0.309016994374945,-0.951056516295154,
-6.68470697498368E-15));
#134250=DIRECTION('ref_axis',(-0.951056516295154,0.309016994374945,3.41480999208033E-15));
#134251=DIRECTION('center_axis',(-0.309016994374964,-0.951056516295148,
-5.01621543147891E-14));
#134252=DIRECTION('ref_axis',(-0.951056516295148,0.309016994374964,3.41480999207994E-15));
#134253=DIRECTION('center_axis',(-0.309016994374945,-0.951056516295154,
-6.68470697498368E-15));
#134254=DIRECTION('ref_axis',(-0.951056516295154,0.309016994374945,3.41480999208033E-15));
#134255=DIRECTION('center_axis',(0.309016994374972,0.951056516295146,6.64119215765932E-15));
#134256=DIRECTION('ref_axis',(0.951056516295146,-0.309016994374972,-3.41480999208037E-15));
#134257=DIRECTION('center_axis',(-0.163755587629913,-0.50398787616902,0.848045003637556));
#134258=DIRECTION('ref_axis',(1.74588362472744E-15,-0.859649462041466,-0.510884333691901));
#134259=DIRECTION('center_axis',(0.154510091261934,0.475533164204418,-0.866022425483291));
#134260=DIRECTION('ref_axis',(-8.93385339497672E-16,0.876548714628834,0.48131315261744));
#134261=DIRECTION('center_axis',(0.163755558326672,0.503987855974368,-0.848045021297501));
#134262=DIRECTION('ref_axis',(0.257959309137026,0.807862963765574,0.529919264233195));
#134263=DIRECTION('center_axis',(-0.16375557028641,-0.503987822791206,0.848045038708648));
#134264=DIRECTION('ref_axis',(-1.88791329792594E-15,-0.859649495083702,
-0.510884278092736));
#134265=DIRECTION('center_axis',(0.154510085545305,0.47553318062662,-0.866022417485779));
#134266=DIRECTION('ref_axis',(0.263286939716706,0.825033325008545,0.499999999999957));
#134267=DIRECTION('center_axis',(0.26765302593241,0.82363980420871,-0.499979330205022));
#134268=DIRECTION('ref_axis',(0.155418826426913,0.475210466545561,0.866036951219537));
#134269=DIRECTION('center_axis',(-0.951131423661017,0.308786358060986,2.15624361371854E-15));
#134270=DIRECTION('ref_axis',(0.308786358060986,0.951131423661017,6.82961998416067E-15));
#134271=DIRECTION('center_axis',(-0.309016994374945,-0.951056516295154,
-6.68470697498368E-15));
#134272=DIRECTION('ref_axis',(-0.951056516295154,0.309016994374945,3.41480999208033E-15));
#134273=DIRECTION('center_axis',(0.309016994374922,0.951056516295162,6.64119215765944E-15));
#134274=DIRECTION('ref_axis',(0.951056516295162,-0.309016994374922,-3.41480999208039E-15));
#134275=DIRECTION('center_axis',(-9.73020895656139E-17,-6.84903784078409E-15,
1.));
#134276=DIRECTION('ref_axis',(0.,-1.,-6.84749938415785E-15));
#134277=DIRECTION('center_axis',(-0.95098155300316,0.309247612517378,2.15946453637244E-15));
#134278=DIRECTION('ref_axis',(0.309247612517378,0.95098155300316,6.82961998416082E-15));
#134279=DIRECTION('center_axis',(0.163755730877736,0.503988317040564,0.848044713969328));
#134280=DIRECTION('ref_axis',(1.3688970201719E-17,-0.859649189130477,0.510884792910607));
#134281=DIRECTION('center_axis',(0.163755570286409,0.503987822791204,-0.84804503870865));
#134282=DIRECTION('ref_axis',(1.78266007267482E-15,0.859649495083703,0.510884278092735));
#134283=DIRECTION('center_axis',(0.16375576493453,0.503988340267678,0.848044693589281));
#134284=DIRECTION('ref_axis',(-0.257746148173953,-0.807930997360561,0.529919264233203));
#134285=DIRECTION('center_axis',(0.163755751065515,0.503988379171995,0.848044673146736));
#134286=DIRECTION('ref_axis',(-2.42242054595195E-15,-0.859649150669468,
0.510884857627686));
#134287=DIRECTION('center_axis',(-0.163755558317466,-0.50398785614383,0.848045021198569));
#134288=DIRECTION('ref_axis',(0.26615647101259,0.805199544419036,0.529919264233243));
#134289=DIRECTION('center_axis',(0.1637555876299,0.50398787616898,-0.848045003637583));
#134290=DIRECTION('ref_axis',(4.71498135796894E-16,0.859649462041491,0.510884333691859));
#134291=DIRECTION('center_axis',(-0.951136266645027,0.308771440182801,-6.95712478733955E-15));
#134292=DIRECTION('ref_axis',(0.308771440182801,0.951136266645027,6.82961998416065E-15));
#134293=DIRECTION('center_axis',(0.309016994374964,0.951056516295148,-4.53216445603843E-14));
#134294=DIRECTION('ref_axis',(0.951056516295148,-0.309016994374964,-3.41480999208075E-15));
#134295=DIRECTION('center_axis',(-9.73020895656139E-17,-6.84903784078409E-15,
1.));
#134296=DIRECTION('ref_axis',(0.,-1.,-6.84651435173441E-15));
#134297=DIRECTION('center_axis',(-0.950976702550722,0.309262527968967,-6.92250494748091E-15));
#134298=DIRECTION('ref_axis',(0.309262527968967,0.950976702550722,6.8296199841605E-15));
#134299=DIRECTION('center_axis',(0.309016994374945,0.951056516295154,6.68470697498368E-15));
#134300=DIRECTION('ref_axis',(0.951056516295154,-0.309016994374945,-3.41480999208036E-15));
#134301=DIRECTION('center_axis',(0.267585776505841,0.823641557783774,0.500012436348622));
#134302=DIRECTION('ref_axis',(-0.155453534525656,-0.475234043079439,0.866017784402751));
#134303=DIRECTION('center_axis',(-0.163755751065466,-0.503988379171994,
-0.848044673146746));
#134304=DIRECTION('ref_axis',(-1.95984699059842E-15,0.859649150669472,-0.51088485762768));
#134305=DIRECTION('center_axis',(-0.154510054857039,-0.475533019434617,
-0.866022511471539));
#134306=DIRECTION('ref_axis',(-0.27187031189046,-0.822244813612451,0.50000000000001));
#134307=DIRECTION('center_axis',(0.154510049384245,0.475533035317994,0.866022503726395));
#134308=DIRECTION('ref_axis',(-3.62116518657123E-16,-0.876548788012518,
0.481313018973917));
#134309=DIRECTION('center_axis',(-0.163755764949564,-0.503988340058636,
-0.848044693710611));
#134310=DIRECTION('ref_axis',(-0.266368911015363,-0.805129291877427,0.529919264233188));
#134311=DIRECTION('center_axis',(-0.16375573087769,-0.503988317040571,-0.848044713969332));
#134312=DIRECTION('ref_axis',(3.12513560129423E-16,0.859649189130475,-0.51088479291061));
#134313=DIRECTION('center_axis',(0.309016994374964,0.951056516295148,1.50830667185733E-14));
#134314=DIRECTION('ref_axis',(0.951056516295148,-0.309016994374964,-3.41480999208024E-15));
#134315=DIRECTION('center_axis',(-0.309016994374964,-0.951056516295148,
-6.64119215765934E-15));
#134316=DIRECTION('ref_axis',(-0.951056516295148,0.309016994374964,3.41480999208031E-15));
#134317=DIRECTION('center_axis',(0.309016994374945,0.951056516295154,6.68470697498368E-15));
#134318=DIRECTION('ref_axis',(0.951056516295154,-0.309016994374945,-3.41480999208036E-15));
#134319=DIRECTION('center_axis',(0.309016994374964,0.951056516295148,-6.22053936822121E-14));
#134320=DIRECTION('ref_axis',(0.951056516295148,-0.309016994374964,-3.41480999208089E-15));
#134321=DIRECTION('center_axis',(0.309016994374945,0.951056516295154,6.68470697498368E-15));
#134322=DIRECTION('ref_axis',(0.951056516295154,-0.309016994374945,-3.41480999208036E-15));
#134323=DIRECTION('center_axis',(-0.267587483540256,-0.82366110022265,0.499979330205367));
#134324=DIRECTION('ref_axis',(-0.15358523212817,-0.475806237448477,-0.866036951219323));
#134325=DIRECTION('center_axis',(0.154510091261981,0.475533164204423,-0.86602242548328));
#134326=DIRECTION('ref_axis',(-1.07558166235271E-15,0.876548714628829,0.481313152617449));
#134327=DIRECTION('center_axis',(0.154510094033318,0.475533172733701,-0.866022420305407));
#134328=DIRECTION('ref_axis',(-0.951056516296803,0.309016994369873,-3.0946373998982E-12));
#134329=DIRECTION('center_axis',(-0.10395688795453,-0.489078705158565,-0.866022508718584));
#134330=DIRECTION('ref_axis',(0.978147600733646,-0.207911690818511,4.5895046399331E-13));
#134331=DIRECTION('center_axis',(-0.180084698746432,-0.847087400906293,
-0.500012436348566));
#134332=DIRECTION('ref_axis',(0.102990311619474,0.489291521294292,-0.866017784402861));
#134333=DIRECTION('center_axis',(0.103956889752271,0.489078713616363,0.866022503726317));
#134334=DIRECTION('ref_axis',(-3.34623636700672E-16,-0.870740345484707,
0.49174307391683));
#134335=DIRECTION('center_axis',(0.20791169081776,0.978147600733806,-4.66126430222498E-14));
#134336=DIRECTION('ref_axis',(0.978147600733806,-0.20791169081776,1.32038128099746E-28));
#134337=DIRECTION('center_axis',(-0.207911690817756,-0.978147600733806,
-6.85964567039975E-15));
#134338=DIRECTION('ref_axis',(-0.978147600733806,0.207911690817756,4.65131225051149E-31));
#134339=DIRECTION('center_axis',(-0.207911690817757,-0.978147600733806,
-6.83036818919254E-15));
#134340=DIRECTION('ref_axis',(-0.978147600733806,0.207911690817757,-2.9624920046404E-32));
#134341=DIRECTION('center_axis',(-0.207911690817756,-0.978147600733806,
-6.85964567039975E-15));
#134342=DIRECTION('ref_axis',(-0.978147600733806,0.207911690817756,-4.9939677714214E-31));
#134343=DIRECTION('center_axis',(0.207911690817754,0.978147600733807,6.83036818919254E-15));
#134344=DIRECTION('ref_axis',(0.978147600733807,-0.207911690817754,1.95800148050649E-29));
#134345=DIRECTION('center_axis',(-0.110177439185354,-0.518344097776659,
0.848045003637578));
#134346=DIRECTION('ref_axis',(-1.54555453578699E-15,-0.853239582811865,
-0.521519140898045));
#134347=DIRECTION('center_axis',(0.103956917928293,0.489078846174045,-0.866022425483264));
#134348=DIRECTION('ref_axis',(-1.23054211610355E-15,0.870740269393752,0.491743208652745));
#134349=DIRECTION('center_axis',(0.110177412156739,0.518344074628991,-0.848045021297489));
#134350=DIRECTION('ref_axis',(0.172101506937256,0.830401496087534,0.529919264233252));
#134351=DIRECTION('center_axis',(-0.110177427516371,-0.518344042878412,
0.848045038708639));
#134352=DIRECTION('ref_axis',(8.08042342219762E-16,-0.853239616987295,-0.521519084984792));
#134353=DIRECTION('center_axis',(0.103956910525269,0.48907886190895,-0.866022417485764));
#134354=DIRECTION('ref_axis',(0.175605160703735,0.848034685336757,0.500000000000003));
#134355=DIRECTION('center_axis',(0.180092991630818,0.847105178672015,-0.499979330205275));
#134356=DIRECTION('ref_axis',(0.104894406050269,0.488852904974495,0.86603695121938));
#134357=DIRECTION('center_axis',(-0.978197989689806,0.20767448800183,1.45018319882439E-15));
#134358=DIRECTION('ref_axis',(0.20767448800183,0.978197989689806,6.82961998416083E-15));
#134359=DIRECTION('center_axis',(-0.207911690817756,-0.978147600733806,
-6.85964567039975E-15));
#134360=DIRECTION('ref_axis',(-0.978147600733806,0.207911690817756,4.65131225051149E-31));
#134361=DIRECTION('center_axis',(0.207911690817757,0.978147600733806,6.83036818919254E-15));
#134362=DIRECTION('ref_axis',(0.978147600733806,-0.207911690817757,2.9624920046404E-32));
#134363=DIRECTION('center_axis',(-1.11539425682703E-16,-6.84522295806915E-15,
1.));
#134364=DIRECTION('ref_axis',(0.,-1.,-6.84749938415785E-15));
#134365=DIRECTION('center_axis',(-0.978097154258596,0.208148881407602,1.45349587027143E-15));
#134366=DIRECTION('ref_axis',(0.208148881407602,0.978097154258596,6.82961998416047E-15));
#134367=DIRECTION('center_axis',(0.110177535564839,0.518344551206562,0.848044713969333));
#134368=DIRECTION('ref_axis',(1.17513314922421E-15,-0.853239300541054,0.521519602711358));
#134369=DIRECTION('center_axis',(0.110177427516339,0.518344042878482,-0.848045038708601));
#134370=DIRECTION('ref_axis',(-1.26528534754762E-16,0.853239616987253,0.521519084984861));
#134371=DIRECTION('center_axis',(0.110177567011267,0.518344577865476,0.848044693589282));
#134372=DIRECTION('ref_axis',(-0.171882402210563,-0.830446875606688,0.529919264233162));
#134373=DIRECTION('center_axis',(0.110177549147492,0.518344615107833,0.848044673146742));
#134374=DIRECTION('ref_axis',(1.16486514661486E-15,-0.853239260760976,0.521519667794095));
#134375=DIRECTION('center_axis',(-0.110177412123957,-0.518344074797815,
0.84804502119856));
#134376=DIRECTION('ref_axis',(0.1805321670207,0.828609503967533,0.529919264233231));
#134377=DIRECTION('center_axis',(0.110177439185352,0.51834409777665,-0.848045003637584));
#134378=DIRECTION('ref_axis',(-1.32803749140163E-15,0.853239582811871,0.521519140898035));
#134379=DIRECTION('center_axis',(-0.978201246800567,0.207659145615639,-5.65545097523496E-16));
#134380=DIRECTION('ref_axis',(0.207659145615639,0.978201246800567,6.82961998416065E-15));
#134381=DIRECTION('center_axis',(0.207911690817757,0.978147600733806,6.83036818919254E-15));
#134382=DIRECTION('ref_axis',(0.978147600733806,-0.207911690817757,2.9624920046404E-32));
#134383=DIRECTION('center_axis',(-1.11539425682703E-16,-6.84522295806915E-15,
1.));
#134384=DIRECTION('ref_axis',(0.,-1.,-6.84651435173441E-15));
#134385=DIRECTION('center_axis',(-0.978093889466682,0.208164222161104,1.45360299418058E-15));
#134386=DIRECTION('ref_axis',(0.208164222161104,0.978093889466682,6.82961998416055E-15));
#134387=DIRECTION('center_axis',(0.207911690817756,0.978147600733806,6.85964567039975E-15));
#134388=DIRECTION('ref_axis',(0.978147600733806,-0.207911690817756,-5.48498646232285E-30));
#134389=DIRECTION('center_axis',(0.180025927304963,0.847099893161503,0.500012436349096));
#134390=DIRECTION('ref_axis',(-0.104926459548316,-0.488879980348169,0.866017784402509));
#134391=DIRECTION('center_axis',(-0.110177549147462,-0.518344615107834,
-0.848044673146745));
#134392=DIRECTION('ref_axis',(-1.35828912679475E-15,0.853239260760977,-0.521519667794094));
#134393=DIRECTION('center_axis',(-0.103956896854893,-0.489078698392047,
-0.866022511471522));
#134394=DIRECTION('ref_axis',(-0.184432991087763,-0.846158656398667,0.500000000000023));
#134395=DIRECTION('center_axis',(0.103956889752284,0.489078713616327,0.866022503726335));
#134396=DIRECTION('ref_axis',(-1.08655637743655E-15,-0.870740345484727,
0.491743073916795));
#134397=DIRECTION('center_axis',(-0.110177567046589,-0.518344577659445,
-0.848044693710624));
#134398=DIRECTION('ref_axis',(-0.180750786634256,-0.828561842306085,0.529919264233189));
#134399=DIRECTION('center_axis',(-0.110177535564859,-0.518344551206569,
-0.848044713969325));
#134400=DIRECTION('ref_axis',(1.46521819382421E-15,0.853239300541049,-0.521519602711367));
#134401=DIRECTION('center_axis',(0.207911690817757,0.978147600733806,6.83036818919254E-15));
#134402=DIRECTION('ref_axis',(0.978147600733806,-0.207911690817757,2.9624920046404E-32));
#134403=DIRECTION('center_axis',(-0.207911690817754,-0.978147600733807,
-6.83036818919254E-15));
#134404=DIRECTION('ref_axis',(-0.978147600733807,0.207911690817754,-1.95800148050649E-29));
#134405=DIRECTION('center_axis',(0.207911690817756,0.978147600733806,6.85964567039975E-15));
#134406=DIRECTION('ref_axis',(0.978147600733806,-0.207911690817756,-5.48498646232285E-30));
#134407=DIRECTION('center_axis',(0.207911690817757,0.978147600733806,-1.68937884210484E-15));
#134408=DIRECTION('ref_axis',(0.978147600733806,-0.207911690817757,4.04710180979884E-32));
#134409=DIRECTION('center_axis',(0.207911690817756,0.978147600733806,6.85964567039975E-15));
#134410=DIRECTION('ref_axis',(0.978147600733806,-0.207911690817756,-5.48498646232285E-30));
#134411=DIRECTION('center_axis',(-0.180025582247582,-0.847119506978666,
0.499979330205401));
#134412=DIRECTION('ref_axis',(-0.103008581356496,-0.489253749387449,-0.866036951219315));
#134413=DIRECTION('center_axis',(0.103956917928286,0.489078846174007,-0.866022425483286));
#134414=DIRECTION('ref_axis',(-1.08851636843951E-16,0.870740269393773,0.491743208652707));
#134415=DIRECTION('center_axis',(0.103956919794677,0.489078854954631,-0.866022420300462));
#134416=DIRECTION('ref_axis',(-0.978147600734682,0.207911690813636,-2.45647771009641E-12));
#134417=DIRECTION('center_axis',(-0.0522647557773232,-0.497265934576513,
-0.866022508722079));
#134418=DIRECTION('ref_axis',(0.994521895368419,-0.104528463266268,-7.73659353600025E-13));
#134419=DIRECTION('center_axis',(-0.0905534316550513,-0.861270944309439,
-0.500012436349159));
#134420=DIRECTION('ref_axis',(0.051281229102223,0.497376550151214,-0.866017784402516));
#134421=DIRECTION('center_axis',(0.0522647566818157,0.497265943181911,0.866022503726315));
#134422=DIRECTION('ref_axis',(5.43068232277855E-16,-0.867207748104381,0.497946504785131));
#134423=DIRECTION('center_axis',(0.104528463267629,0.994521895368276,6.94470927749848E-15));
#134424=DIRECTION('ref_axis',(0.994521895368276,-0.104528463267629,-4.99922698313062E-30));
#134425=DIRECTION('center_axis',(-0.10452846326765,-0.994521895368274,-6.95942865237777E-15));
#134426=DIRECTION('ref_axis',(-0.994521895368274,0.10452846326765,-1.06118964965575E-32));
#134427=DIRECTION('center_axis',(-0.104528463267629,-0.994521895368276,
-6.23081959585229E-15));
#134428=DIRECTION('ref_axis',(-0.994521895368276,0.104528463267629,4.55502821820944E-30));
#134429=DIRECTION('center_axis',(-0.10452846326765,-0.994521895368274,-6.95942865237777E-15));
#134430=DIRECTION('ref_axis',(-0.994521895368274,0.10452846326765,-1.06118964965575E-32));
#134431=DIRECTION('center_axis',(0.104528463267629,0.994521895368276,6.94470927749848E-15));
#134432=DIRECTION('ref_axis',(0.994521895368276,-0.104528463267629,-4.99922698313062E-30));
#134433=DIRECTION('center_axis',(-0.0553921636609753,-0.527021232978594,
0.848045003637589));
#134434=DIRECTION('ref_axis',(3.12484149181909E-16,-0.84934903001939,-0.5278316258099));
#134435=DIRECTION('center_axis',(0.0522647708473854,0.497266077958579,-0.866022425483291));
#134436=DIRECTION('ref_axis',(-1.07267863460433E-16,0.867207670398078,0.497946640115924));
#134437=DIRECTION('center_axis',(0.0553921391963296,0.527021207132855,-0.848045021297503));
#134438=DIRECTION('ref_axis',(0.0843581245585095,0.843841975855393,0.529919264233182));
#134439=DIRECTION('center_axis',(-0.0553921577943468,-0.527021177161352,
0.848045038708646));
#134440=DIRECTION('ref_axis',(-2.92497129473667E-16,-0.849349064867516,
-0.527831569734774));
#134441=DIRECTION('center_axis',(0.0522647618413962,0.497266092833347,-0.866022417485783));
#134442=DIRECTION('ref_axis',(0.0859994148076584,0.861744800189005,0.499999999999952));
#134443=DIRECTION('center_axis',(0.0905598208271191,0.861289491529708,-0.499979330205016));
#134444=DIRECTION('ref_axis',(0.0532207405910698,0.497139368681772,0.866036951219535));
#134445=DIRECTION('center_axis',(-0.994547213842469,0.104287292793432,-6.06414525351624E-15));
#134446=DIRECTION('ref_axis',(0.104287292793432,0.994547213842469,6.82961998416055E-15));
#134447=DIRECTION('center_axis',(-0.10452846326765,-0.994521895368274,-6.95942865237777E-15));
#134448=DIRECTION('ref_axis',(-0.994521895368274,0.10452846326765,-1.06118964965575E-32));
#134449=DIRECTION('center_axis',(0.104528463267628,0.994521895368276,6.94470927749848E-15));
#134450=DIRECTION('ref_axis',(0.994521895368276,-0.104528463267628,1.09814391166396E-31));
#134451=DIRECTION('center_axis',(-1.26097532010604E-16,-6.84291718054622E-15,
1.));
#134452=DIRECTION('ref_axis',(0.,-1.,-6.84044737655315E-15));
#134453=DIRECTION('center_axis',(-0.994496518411991,0.10476962759516,7.3160239925209E-16));
#134454=DIRECTION('ref_axis',(0.10476962759516,0.994496518411991,6.82961998416045E-15));
#134455=DIRECTION('center_axis',(0.0553922121161709,0.527021693998976,0.848044713969333));
#134456=DIRECTION('ref_axis',(7.77180288600867E-16,-0.849348742192416,0.527832088960269));
#134457=DIRECTION('center_axis',(0.0553921577943474,0.527021177161358,-0.848045038708643));
#134458=DIRECTION('ref_axis',(8.49466062352983E-17,0.849349064867513,0.52783156973478));
#134459=DIRECTION('center_axis',(0.0553922406021807,0.527021723799047,0.848044693589289));
#134460=DIRECTION('ref_axis',(-0.0841354766906324,-0.843864204097235,0.529919264233128));
#134461=DIRECTION('center_axis',(0.0553922189448978,0.527021758969969,0.84804467314674));
#134462=DIRECTION('ref_axis',(-1.4399498926774E-16,-0.849348701629312,0.527832154231438));
#134463=DIRECTION('center_axis',(-0.0553921391403666,-0.527021207297975,
0.848045021198544));
#134464=DIRECTION('ref_axis',(0.0929299148375028,0.842941044393284,0.529919264233197));
#134465=DIRECTION('center_axis',(0.0553921636609804,0.527021232978642,-0.848045003637559));
#134466=DIRECTION('ref_axis',(3.75742388398108E-16,0.849349030019359,0.527831625809948));
#134467=DIRECTION('center_axis',(-0.994548849394383,0.104271693993668,7.28125347496908E-16));
#134468=DIRECTION('ref_axis',(0.104271693993668,0.994548849394383,6.8296199841608E-15));
#134469=DIRECTION('center_axis',(0.104528463267629,0.994521895368276,6.23081959585229E-15));
#134470=DIRECTION('ref_axis',(0.994521895368276,-0.104528463267629,-4.55502821820944E-30));
#134471=DIRECTION('center_axis',(-1.26097532010604E-16,-6.84291718054622E-15,
1.));
#134472=DIRECTION('ref_axis',(0.,-1.,-6.84651435173441E-15));
#134473=DIRECTION('center_axis',(-0.994494875050338,0.104785225574086,6.45685748436114E-15));
#134474=DIRECTION('ref_axis',(0.104785225574086,0.994494875050338,6.82961998416065E-15));
#134475=DIRECTION('center_axis',(0.10452846326765,0.994521895368274,6.95942865237777E-15));
#134476=DIRECTION('ref_axis',(0.994521895368274,-0.10452846326765,-8.52179472506115E-30));
#134477=DIRECTION('center_axis',(0.0904936763725661,0.86127722484297,0.500012436348706));
#134478=DIRECTION('ref_axis',(-0.0532497883514946,-0.497169646236267,0.866017784402737));
#134479=DIRECTION('center_axis',(-0.0553922189448982,-0.527021758969977,
-0.848044673146735));
#134480=DIRECTION('ref_axis',(1.29981789962805E-16,0.849348701629308,-0.527832154231446));
#134481=DIRECTION('center_axis',(-0.0522647653362515,-0.497265928783454,
-0.866022511471541));
#134482=DIRECTION('ref_axis',(-0.0949749838229919,-0.860801807879048,0.499999999999985));
#134483=DIRECTION('center_axis',(0.0522647566817756,0.49726594318179,0.866022503726387));
#134484=DIRECTION('ref_axis',(1.39619082696246E-16,-0.867207748104452,0.497946504785008));
#134485=DIRECTION('center_axis',(-0.055392240656774,-0.527021723598077,
-0.848044693710617));
#134486=DIRECTION('ref_axis',(-0.093152318817715,-0.842916495801014,0.529919264233168));
#134487=DIRECTION('center_axis',(-0.0553922121161263,-0.527021693998996,
-0.848044713969323));
#134488=DIRECTION('ref_axis',(5.85779016094295E-16,0.849348742192404,-0.527832088960287));
#134489=DIRECTION('center_axis',(0.104528463267629,0.994521895368276,6.23081959585229E-15));
#134490=DIRECTION('ref_axis',(0.994521895368276,-0.104528463267629,-4.55502821820944E-30));
#134491=DIRECTION('center_axis',(-0.104528463267628,-0.994521895368276,
-6.94470927749848E-15));
#134492=DIRECTION('ref_axis',(-0.994521895368276,0.104528463267628,-1.09814391166396E-31));
#134493=DIRECTION('center_axis',(0.10452846326765,0.994521895368274,6.95942865237777E-15));
#134494=DIRECTION('ref_axis',(0.994521895368274,-0.10452846326765,-8.52179472506115E-30));
#134495=DIRECTION('center_axis',(0.104528463267629,0.994521895368276,6.23081959585229E-15));
#134496=DIRECTION('ref_axis',(0.994521895368276,-0.104528463267629,-4.55502821820944E-30));
#134497=DIRECTION('center_axis',(0.10452846326765,0.994521895368274,6.95942865237777E-15));
#134498=DIRECTION('ref_axis',(0.994521895368274,-0.10452846326765,-8.52179472506115E-30));
#134499=DIRECTION('center_axis',(-0.0904912830029572,-0.861296695145089,
0.499979330205386));
#134500=DIRECTION('ref_axis',(-0.0513033469950975,-0.497340894869751,-0.866036951219321));
#134501=DIRECTION('center_axis',(0.0522647708473846,0.497266077958568,-0.866022425483298));
#134502=DIRECTION('ref_axis',(9.84167878630125E-17,0.867207670398085,0.497946640115913));
#134503=DIRECTION('center_axis',(0.0522647717855327,0.497266086884299,-0.866022420301566));
#134504=DIRECTION('ref_axis',(-0.994521895368333,0.104528463267083,-3.23450801682927E-13));
#134505=DIRECTION('center_axis',(1.82822378937428E-15,-0.500005014363672,
-0.866022508720867));
#134506=DIRECTION('ref_axis',(1.,-5.03534223352382E-12,2.91979914235583E-12));
#134507=DIRECTION('center_axis',(-3.0042215982928E-5,-0.866018223014645,
-0.500012436349359));
#134508=DIRECTION('ref_axis',(-0.00098970133587607,0.500012217440829,-0.866017784402359));
#134509=DIRECTION('center_axis',(-1.99980824065794E-14,0.500005023014366,
0.86602250372632));
#134510=DIRECTION('ref_axis',(9.19523158479882E-29,-0.86602250372632,0.500005023014366));
#134511=DIRECTION('center_axis',(0.,1.,6.98296267768627E-15));
#134512=DIRECTION('ref_axis',(0.,-6.98296267768627E-15,1.));
#134513=DIRECTION('center_axis',(3.49148133884313E-15,-1.,-6.98296267768627E-15));
#134514=DIRECTION('ref_axis',(-1.,-3.49148133884313E-15,-4.51218105512591E-43));
#134515=DIRECTION('center_axis',(0.,-1.,-6.98296267768627E-15));
#134516=DIRECTION('ref_axis',(0.,6.98296267768627E-15,-1.));
#134517=DIRECTION('center_axis',(3.49148133884313E-15,-1.,-6.98296267768627E-15));
#134518=DIRECTION('ref_axis',(-1.,-3.49148133884313E-15,-4.51218105512591E-43));
#134519=DIRECTION('center_axis',(0.,1.,6.98296267768627E-15));
#134520=DIRECTION('ref_axis',(0.,-6.98296267768627E-15,1.));
#134521=DIRECTION('center_axis',(0.,-0.529924213265795,0.848045003637559));
#134522=DIRECTION('ref_axis',(0.,-0.848045003637559,-0.529924213265795));
#134523=DIRECTION('center_axis',(0.,0.500005158533428,-0.866022425483291));
#134524=DIRECTION('ref_axis',(0.,0.866022425483291,0.500005158533428));
#134525=DIRECTION('center_axis',(-2.16295993207103E-8,0.529924185004342,
-0.848045021297503));
#134526=DIRECTION('ref_axis',(-0.00430950304133444,0.848037146343309,0.529919264233179));
#134527=DIRECTION('center_axis',(0.,-0.529924157141057,0.848045038708641));
#134528=DIRECTION('ref_axis',(0.,-0.848045038708641,-0.529924157141057));
#134529=DIRECTION('center_axis',(-1.05163242810076E-8,0.500005172385359,
-0.866022417485764));
#134530=DIRECTION('ref_axis',(-0.00454855868657297,0.866013458679407,0.500000000000005));
#134531=DIRECTION('center_axis',(3.44576745319419E-5,0.866037336481644,
-0.499979330205208));
#134532=DIRECTION('ref_axis',(0.000963977564194347,0.499979069431728,0.866036951219426));
#134533=DIRECTION('center_axis',(-0.999999970597889,-0.000242495818334613,
-1.35084350642584E-16));
#134534=DIRECTION('ref_axis',(-0.000242495818334613,0.999999970597889,6.82961998416057E-15));
#134535=DIRECTION('center_axis',(3.49148133884313E-15,-1.,-6.98296267768627E-15));
#134536=DIRECTION('ref_axis',(-1.,-3.49148133884313E-15,-4.51218105512591E-43));
#134537=DIRECTION('center_axis',(0.,1.,6.98296267768627E-15));
#134538=DIRECTION('ref_axis',(0.,-6.98296267768627E-15,1.));
#134539=DIRECTION('center_axis',(-1.40816906889911E-16,-6.84214577079636E-15,
1.));
#134540=DIRECTION('ref_axis',(-1.,1.20258066624967E-30,-1.41040152093879E-16));
#134541=DIRECTION('center_axis',(-0.999999970597889,0.000242495818327663,
-1.45036773284147E-16));
#134542=DIRECTION('ref_axis',(0.000242495818327663,0.999999970597889,6.82961998416057E-15));
#134543=DIRECTION('center_axis',(2.89534733035821E-14,0.52992467682556,
0.848044713969332));
#134544=DIRECTION('ref_axis',(-8.01740051201329E-29,-0.848044713969332,
0.52992467682556));
#134545=DIRECTION('center_axis',(-4.63346027506605E-14,0.529924157141126,
-0.848045038708598));
#134546=DIRECTION('ref_axis',(-4.22399707661028E-28,0.848045038708598,0.529924157141126));
#134547=DIRECTION('center_axis',(2.52111351274489E-8,0.529924709439963,
0.8480446935893));
#134548=DIRECTION('ref_axis',(0.00453325469978111,-0.848035979777039,0.529919264233169));
#134549=DIRECTION('center_axis',(4.63345827774717E-14,0.529924742154426,
0.848044673146742));
#134550=DIRECTION('ref_axis',(-4.19038424263683E-28,-0.848044673146742,
0.529924742154426));
#134551=DIRECTION('center_axis',(2.16910432124849E-8,-0.529924185162658,
0.848045021198575));
#134552=DIRECTION('ref_axis',(0.0043095030298541,0.848037146343357,0.529919264233196));
#134553=DIRECTION('center_axis',(0.,0.529924213265795,-0.848045003637559));
#134554=DIRECTION('ref_axis',(0.,0.848045003637559,0.529924213265795));
#134555=DIRECTION('center_axis',(-0.99999996667151,-0.000258180127967688,
-1.61872075241625E-16));
#134556=DIRECTION('ref_axis',(-0.000258180127967688,0.99999996667151,6.82961998416055E-15));
#134557=DIRECTION('center_axis',(0.,1.,6.98296267768627E-15));
#134558=DIRECTION('ref_axis',(0.,-6.98296267768627E-15,1.));
#134559=DIRECTION('center_axis',(-1.40816906889911E-16,-6.84214577079636E-15,
1.));
#134560=DIRECTION('ref_axis',(-1.,8.53463339982835E-31,-1.42635715661134E-16));
#134561=DIRECTION('center_axis',(-0.99999996667151,0.000258180127960702,
-1.44160173554759E-16));
#134562=DIRECTION('ref_axis',(0.000258180127960701,0.99999996667151,6.82961998416055E-15));
#134563=DIRECTION('center_axis',(-3.49148133884313E-15,1.,6.98296267768627E-15));
#134564=DIRECTION('ref_axis',(1.,3.49148133884313E-15,1.12103877145985E-43));
#134565=DIRECTION('center_axis',(-3.00422149895149E-5,0.866018223015033,
0.500012436348687));
#134566=DIRECTION('ref_axis',(-0.000989701305755301,-0.50001221744017,0.866017784402774));
#134567=DIRECTION('center_axis',(0.,-0.529924742154426,-0.848044673146742));
#134568=DIRECTION('ref_axis',(0.,0.848044673146742,-0.529924742154426));
#134569=DIRECTION('center_axis',(-1.01157682251589E-8,-0.500005009599441,
-0.866022511471534));
#134570=DIRECTION('ref_axis',(-0.00447641077753576,-0.86601383461614,0.5));
#134571=DIRECTION('center_axis',(0.,0.500005023014325,0.866022503726343));
#134572=DIRECTION('ref_axis',(0.,-0.866022503726343,0.500005023014325));
#134573=DIRECTION('center_axis',(-2.52907361300284E-8,-0.52992470924582,
-0.848044693710616));
#134574=DIRECTION('ref_axis',(-0.0045332546860101,-0.848035979777084,0.529919264233216));
#134575=DIRECTION('center_axis',(0.,-0.52992467682556,-0.848044713969332));
#134576=DIRECTION('ref_axis',(0.,0.848044713969332,-0.52992467682556));
#134577=DIRECTION('center_axis',(0.,1.,6.98296267768627E-15));
#134578=DIRECTION('ref_axis',(0.,-6.98296267768627E-15,1.));
#134579=DIRECTION('center_axis',(0.,-1.,-6.98296267768627E-15));
#134580=DIRECTION('ref_axis',(0.,6.98296267768627E-15,-1.));
#134581=DIRECTION('center_axis',(-3.49148133884313E-15,1.,6.98296267768627E-15));
#134582=DIRECTION('ref_axis',(1.,3.49148133884313E-15,-5.88545355016423E-44));
#134583=DIRECTION('center_axis',(0.,1.,6.98296267768627E-15));
#134584=DIRECTION('ref_axis',(0.,-6.98296267768627E-15,1.));
#134585=DIRECTION('center_axis',(-3.49148133884313E-15,1.,6.98296267768627E-15));
#134586=DIRECTION('ref_axis',(1.,3.49148133884313E-15,-5.88545355016423E-44));
#134587=DIRECTION('center_axis',(3.44576747051342E-5,-0.866037336481666,
0.499979330205169));
#134588=DIRECTION('ref_axis',(0.000963977560427604,-0.49997906943169,-0.866036951219452));
#134589=DIRECTION('center_axis',(0.,0.500005158533428,-0.866022425483291));
#134590=DIRECTION('ref_axis',(0.,0.866022425483291,0.500005158533428));
#134591=DIRECTION('center_axis',(-1.4393932896948E-15,0.500005167509625,
-0.866022420300809));
#134592=DIRECTION('ref_axis',(-1.,0.,-1.7483827117929E-14));
#134593=DIRECTION('center_axis',(0.0522647557776122,-0.497265934579085,
-0.866022508720585));
#134594=DIRECTION('ref_axis',(0.99452189536815,0.104528463268829,-6.68756390392693E-13));
#134595=DIRECTION('center_axis',(0.0904936763724324,-0.861277224842764,
-0.500012436349085));
#134596=DIRECTION('ref_axis',(-0.053249788326405,0.497169646239297,-0.866017784402541));
#134597=DIRECTION('center_axis',(-0.0522647566818161,0.497265943181915,
0.866022503726313));
#134598=DIRECTION('ref_axis',(-6.22122455512283E-16,-0.867207748104379,
0.497946504785135));
#134599=DIRECTION('center_axis',(-0.104528463267684,0.99452189536827,6.94470927749844E-15));
#134600=DIRECTION('ref_axis',(0.99452189536827,0.104528463267684,4.95746224200719E-30));
#134601=DIRECTION('center_axis',(0.104528463267657,-0.994521895368273,-6.92998990261915E-15));
#134602=DIRECTION('ref_axis',(-0.994521895368273,-0.104528463267657,3.48082151219685E-32));
#134603=DIRECTION('center_axis',(0.104528463267683,-0.99452189536827,-6.94470927749844E-15));
#134604=DIRECTION('ref_axis',(-0.99452189536827,-0.104528463267683,5.29715191372443E-32));
#134605=DIRECTION('center_axis',(0.104528463267657,-0.994521895368273,-6.92998990261915E-15));
#134606=DIRECTION('ref_axis',(-0.994521895368273,-0.104528463267657,3.48082151219685E-32));
#134607=DIRECTION('center_axis',(-0.104528463267683,0.99452189536827,6.94470927749844E-15));
#134608=DIRECTION('ref_axis',(0.99452189536827,0.104528463267683,-5.29715191372443E-32));
#134609=DIRECTION('center_axis',(0.0553921636610116,-0.527021232978663,
0.848045003637544));
#134610=DIRECTION('ref_axis',(5.49983303975455E-17,-0.849349030019346,-0.527831625809971));
#134611=DIRECTION('center_axis',(-0.0522647708473925,0.497266077958566,
-0.866022425483298));
#134612=DIRECTION('ref_axis',(-1.7055667978759E-16,0.867207670398085,0.497946640115912));
#134613=DIRECTION('center_axis',(-0.0553921822241136,0.527021202610446,
-0.848045021297507));
#134614=DIRECTION('ref_axis',(-0.0929299148436241,0.842941044392624,0.529919264233175));
#134615=DIRECTION('center_axis',(0.0553921577943745,-0.52702117716134,0.848045038708652));
#134616=DIRECTION('ref_axis',(3.95891136703E-16,-0.849349064867523,-0.527831569734763));
#134617=DIRECTION('center_axis',(-0.0522647827552366,0.497266090635247,
-0.866022417485764));
#134618=DIRECTION('ref_axis',(-0.0950466972106211,0.860793892490734,0.500000000000003));
#134619=DIRECTION('center_axis',(-0.090491283003073,0.861296695145105,-0.499979330205338));
#134620=DIRECTION('ref_axis',(-0.0513033469963453,0.497340894869573,0.866036951219349));
#134621=DIRECTION('center_axis',(-0.994496518411991,-0.10476962759516,-7.3160239925209E-16));
#134622=DIRECTION('ref_axis',(-0.10476962759516,0.994496518411991,6.82961998416045E-15));
#134623=DIRECTION('center_axis',(0.104528463267657,-0.994521895368273,-6.92998990261915E-15));
#134624=DIRECTION('ref_axis',(-0.994521895368273,-0.104528463267657,3.48082151219685E-32));
#134625=DIRECTION('center_axis',(-0.104528463267683,0.99452189536827,6.94470927749844E-15));
#134626=DIRECTION('ref_axis',(0.99452189536827,0.104528463267683,-5.29715191372443E-32));
#134627=DIRECTION('center_axis',(-1.55536281769218E-16,-6.84291718054622E-15,
1.));
#134628=DIRECTION('ref_axis',(-1.,1.20258066624967E-30,-1.55144167303267E-16));
#134629=DIRECTION('center_axis',(-0.994547213842468,-0.104287292793436,
-7.28234273333503E-16));
#134630=DIRECTION('ref_axis',(-0.104287292793436,0.994547213842468,6.82961998416053E-15));
#134631=DIRECTION('center_axis',(-0.0553922121162014,0.527021693998987,
0.848044713969324));
#134632=DIRECTION('ref_axis',(6.84979756801523E-16,-0.849348742192409,0.527832088960281));
#134633=DIRECTION('center_axis',(-0.0553921577943754,0.527021177161349,
-0.848045038708646));
#134634=DIRECTION('ref_axis',(-2.883936554783E-16,0.849349064867518,0.527831569734772));
#134635=DIRECTION('center_axis',(-0.0553921904533803,0.527021729069898,
0.848044693589289));
#134636=DIRECTION('ref_axis',(0.0931523188159149,-0.84291649580119,0.529919264233203));
#134637=DIRECTION('center_axis',(-0.0553922189449272,0.527021758969973,
0.848044673146735));
#134638=DIRECTION('ref_axis',(1.27494230359798E-16,-0.849348701629309,0.527832154231444));
#134639=DIRECTION('center_axis',(0.0553921822969478,-0.527021202762016,
0.848045021198556));
#134640=DIRECTION('ref_axis',(-0.0843581245706196,0.843841975854163,0.529919264233213));
#134641=DIRECTION('center_axis',(-0.0553921636610064,0.527021232978614,
-0.848045003637574));
#134642=DIRECTION('ref_axis',(5.9573696388713E-16,0.849349030019376,0.527831625809922));
#134643=DIRECTION('center_axis',(-0.994494875050338,-0.10478522557409,-7.31711319356807E-16));
#134644=DIRECTION('ref_axis',(-0.10478522557409,0.994494875050338,6.82961998416065E-15));
#134645=DIRECTION('center_axis',(-0.104528463267683,0.99452189536827,6.94470927749844E-15));
#134646=DIRECTION('ref_axis',(0.99452189536827,0.104528463267683,2.7081584375864E-32));
#134647=DIRECTION('center_axis',(-1.55536281769218E-16,-6.84291718054622E-15,
1.));
#134648=DIRECTION('ref_axis',(-1.,1.28019500997425E-30,-1.576500015202E-16));
#134649=DIRECTION('center_axis',(-0.994548849394382,-0.104271693993676,
-7.28125347496963E-16));
#134650=DIRECTION('ref_axis',(-0.104271693993676,0.994548849394382,6.8296199841608E-15));
#134651=DIRECTION('center_axis',(-0.104528463267657,0.994521895368273,6.92998990261915E-15));
#134652=DIRECTION('ref_axis',(0.994521895368273,0.104528463267657,8.40007115892777E-30));
#134653=DIRECTION('center_axis',(-0.0905534316544792,0.861270944309615,
0.500012436348959));
#134654=DIRECTION('ref_axis',(0.0512812290718702,-0.497376550154188,0.866017784402605));
#134655=DIRECTION('center_axis',(0.0553922189449268,-0.527021758969966,
-0.84804467314674));
#134656=DIRECTION('ref_axis',(-2.83402997067715E-16,0.849348701629314,-0.527832154231436));
#134657=DIRECTION('center_axis',(0.0522647452180362,-0.497265930897975,
-0.866022511471535));
#134658=DIRECTION('ref_axis',(0.0860712067675025,-0.861737632557378,0.499999999999992));
#134659=DIRECTION('center_axis',(-0.0522647566818046,0.497265943181806,
0.866022503726376));
#134660=DIRECTION('ref_axis',(-3.85785311454816E-16,-0.867207748104442,
0.497946504785025));
#134661=DIRECTION('center_axis',(0.0553921903485681,-0.527021728885636,
-0.848044693710646));
#134662=DIRECTION('ref_axis',(0.0841354767001877,-0.843864204096268,0.529919264233152));
#134663=DIRECTION('center_axis',(0.0553922121161999,-0.527021693998973,
-0.848044713969333));
#134664=DIRECTION('ref_axis',(6.18235216948487E-16,0.849348742192417,-0.527832088960266));
#134665=DIRECTION('center_axis',(-0.104528463267683,0.99452189536827,6.94470927749844E-15));
#134666=DIRECTION('ref_axis',(0.99452189536827,0.104528463267683,2.7081584375864E-32));
#134667=DIRECTION('center_axis',(0.104528463267682,-0.99452189536827,-6.94470927749844E-15));
#134668=DIRECTION('ref_axis',(-0.99452189536827,-0.104528463267682,4.98335217676857E-30));
#134669=DIRECTION('center_axis',(-0.104528463267657,0.994521895368273,6.92998990261915E-15));
#134670=DIRECTION('ref_axis',(0.994521895368273,0.104528463267657,8.40007115892777E-30));
#134671=DIRECTION('center_axis',(-0.104528463267683,0.99452189536827,6.19962518494839E-14));
#134672=DIRECTION('ref_axis',(0.99452189536827,0.104528463267683,3.69415865639377E-31));
#134673=DIRECTION('center_axis',(-0.104528463267657,0.994521895368273,6.92998990261915E-15));
#134674=DIRECTION('ref_axis',(0.994521895368273,0.104528463267657,8.40007115892777E-30));
#134675=DIRECTION('center_axis',(0.0905598208266182,-0.861289491529548,
0.499979330205383));
#134676=DIRECTION('ref_axis',(0.0532207405915228,-0.497139368682093,-0.866036951219323));
#134677=DIRECTION('center_axis',(-0.0522647708474152,0.4972660779586,-0.866022425483278));
#134678=DIRECTION('ref_axis',(3.08393337172386E-16,0.867207670398066,0.497946640115946));
#134679=DIRECTION('center_axis',(-0.0522647717851799,0.497266086880897,
-0.866022420303541));
#134680=DIRECTION('ref_axis',(-0.994521895368013,-0.104528463270131,-1.43804478045958E-12));
#134681=DIRECTION('center_axis',(0.103956887953212,-0.4890787051524,-0.866022508722225));
#134682=DIRECTION('ref_axis',(0.978147600733671,0.207911690818393,-3.89015155196725E-13));
#134683=DIRECTION('center_axis',(0.180025927304702,-0.847099893161453,-0.500012436349274));
#134684=DIRECTION('ref_axis',(-0.104926459543619,0.488879980349352,-0.86601778440241));
#134685=DIRECTION('center_axis',(-0.103956889752312,0.489078713616365,0.866022503726311));
#134686=DIRECTION('ref_axis',(1.64971394491684E-16,-0.870740345484705,0.491743073916834));
#134687=DIRECTION('center_axis',(-0.207911690817751,0.978147600733807,6.83036818919254E-15));
#134688=DIRECTION('ref_axis',(0.978147600733807,0.207911690817751,-3.90426835043966E-29));
#134689=DIRECTION('center_axis',(0.207911690817763,-0.978147600733805,-6.80109070798532E-15));
#134690=DIRECTION('ref_axis',(-0.978147600733805,-0.207911690817763,2.97563208683757E-32));
#134691=DIRECTION('center_axis',(0.207911690817757,-0.978147600733806,-3.99045251209326E-15));
#134692=DIRECTION('ref_axis',(-0.978147600733806,-0.207911690817757,7.01829476299402E-32));
#134693=DIRECTION('center_axis',(0.207911690817763,-0.978147600733805,-6.80109070798532E-15));
#134694=DIRECTION('ref_axis',(-0.978147600733805,-0.207911690817763,2.97563208683757E-32));
#134695=DIRECTION('center_axis',(-0.207911690817757,0.978147600733806,6.83036818919254E-15));
#134696=DIRECTION('ref_axis',(0.978147600733806,0.207911690817757,-2.9624920046404E-32));
#134697=DIRECTION('center_axis',(0.110177439185365,-0.518344097776712,0.848045003637544));
#134698=DIRECTION('ref_axis',(-2.27092564730572E-16,-0.853239582811832,
-0.521519140898099));
#134699=DIRECTION('center_axis',(-0.103956917928266,0.489078846174011,-0.866022425483286));
#134700=DIRECTION('ref_axis',(3.62085698470434E-16,0.870740269393772,0.491743208652709));
#134701=DIRECTION('center_axis',(-0.110177454465313,0.518344065636003,-0.848045021297503));
#134702=DIRECTION('ref_axis',(-0.180532167021475,0.82860950396738,0.529919264233207));
#134703=DIRECTION('center_axis',(0.110177427516371,-0.518344042878409,0.848045038708641));
#134704=DIRECTION('ref_axis',(-7.51351770475333E-16,-0.853239616987296,
-0.521519084984789));
#134705=DIRECTION('center_axis',(-0.103956931087326,0.489078857538383,-0.866022417485746));
#134706=DIRECTION('ref_axis',(-0.184503484218911,0.846143288285776,0.500000000000017));
#134707=DIRECTION('center_axis',(-0.180025582247482,0.847119506978703,-0.499979330205374));
#134708=DIRECTION('ref_axis',(-0.103008581351147,0.489253749388556,0.866036951219325));
#134709=DIRECTION('center_axis',(-0.978097154258593,-0.208148881407615,
-1.45349587027152E-15));
#134710=DIRECTION('ref_axis',(-0.208148881407615,0.978097154258593,6.82961998416083E-15));
#134711=DIRECTION('center_axis',(0.207911690817763,-0.978147600733805,-6.80109070798532E-15));
#134712=DIRECTION('ref_axis',(-0.978147600733805,-0.207911690817763,2.97563208683757E-32));
#134713=DIRECTION('center_axis',(-0.207911690817757,0.978147600733806,6.83036818919254E-15));
#134714=DIRECTION('ref_axis',(0.978147600733806,0.207911690817757,-2.9624920046404E-32));
#134715=DIRECTION('center_axis',(-1.70094388097119E-16,-6.84522295806915E-15,
1.));
#134716=DIRECTION('ref_axis',(-1.,1.20258066624967E-30,-1.69248182512655E-16));
#134717=DIRECTION('center_axis',(-0.978197989689808,-0.20767448800182,-1.45018319882431E-15));
#134718=DIRECTION('ref_axis',(-0.20767448800182,0.978197989689808,6.82961998416085E-15));
#134719=DIRECTION('center_axis',(-0.110177535564866,0.518344551206608,0.848044713969301));
#134720=DIRECTION('ref_axis',(2.46979766523084E-16,-0.853239300541025,0.521519602711406));
#134721=DIRECTION('center_axis',(-0.110177427516374,0.518344042878427,-0.84804503870863));
#134722=DIRECTION('ref_axis',(1.47794069500662E-15,0.853239616987286,0.521519084984807));
#134723=DIRECTION('center_axis',(-0.110177517688164,0.518344588349403,0.848044693589296));
#134724=DIRECTION('ref_axis',(0.180750786632584,-0.828561842306435,0.529919264233211));
#134725=DIRECTION('center_axis',(-0.110177549147463,0.518344615107834,0.848044673146745));
#134726=DIRECTION('ref_axis',(-1.32855656284121E-15,-0.853239260760977,
0.521519667794093));
#134727=DIRECTION('center_axis',(0.110177454563686,-0.518344065776971,0.84804502119856));
#134728=DIRECTION('ref_axis',(-0.172101506913406,0.830401496092503,0.529919264233211));
#134729=DIRECTION('center_axis',(-0.110177439185362,0.518344097776696,-0.848045003637554));
#134730=DIRECTION('ref_axis',(-1.92246784709572E-16,0.853239582811842,0.521519140898083));
#134731=DIRECTION('center_axis',(-0.978093889466682,-0.208164222161104,
-1.45360299418058E-15));
#134732=DIRECTION('ref_axis',(-0.208164222161104,0.978093889466682,6.82961998416055E-15));
#134733=DIRECTION('center_axis',(-0.207911690817757,0.978147600733806,6.83036818919254E-15));
#134734=DIRECTION('ref_axis',(0.978147600733806,0.207911690817757,-2.70700739195018E-31));
#134735=DIRECTION('center_axis',(-1.70094388097119E-16,-6.84522295806915E-15,
1.));
#134736=DIRECTION('ref_axis',(-1.,1.28019500997425E-30,-1.72664287379267E-16));
#134737=DIRECTION('center_axis',(-0.978201246800563,-0.207659145615656,
-1.45007606351434E-15));
#134738=DIRECTION('ref_axis',(-0.207659145615656,0.978201246800563,6.82961998416061E-15));
#134739=DIRECTION('center_axis',(-0.207911690817763,0.978147600733805,6.80109070798532E-15));
#134740=DIRECTION('ref_axis',(0.978147600733805,0.207911690817763,-4.42525447058535E-29));
#134741=DIRECTION('center_axis',(-0.18008469874793,0.847087400905451,0.500012436349452));
#134742=DIRECTION('ref_axis',(0.10299031155993,-0.489291521307827,0.866017784402296));
#134743=DIRECTION('center_axis',(0.110177549147566,-0.518344615107816,-0.848044673146743));
#134744=DIRECTION('ref_axis',(8.16820715362172E-16,0.853239260760984,-0.521519667794082));
#134745=DIRECTION('center_axis',(0.103956877076738,-0.489078702596054,-0.866022511471505));
#134746=DIRECTION('ref_axis',(0.175675810171962,-0.848020052664076,0.500000000000043));
#134747=DIRECTION('center_axis',(-0.103956889752265,0.489078713616238,0.866022503726388));
#134748=DIRECTION('ref_axis',(1.0747599324937E-15,-0.870740345484778,0.491743073916704));
#134749=DIRECTION('center_axis',(0.1101775175661,-0.518344588176855,-0.848044693710619));
#134750=DIRECTION('ref_axis',(0.1718824022104,-0.83044687560673,0.52991926423315));
#134751=DIRECTION('center_axis',(0.110177535564884,-0.518344551206552,-0.848044713969332));
#134752=DIRECTION('ref_axis',(9.13576263120513E-16,0.853239300541059,-0.521519602711351));
#134753=DIRECTION('center_axis',(-0.207911690817757,0.978147600733806,9.67028386629181E-15));
#134754=DIRECTION('ref_axis',(0.978147600733806,0.207911690817757,-3.68301291740874E-31));
#134755=DIRECTION('center_axis',(0.207911690817754,-0.978147600733807,-6.83036818919254E-15));
#134756=DIRECTION('ref_axis',(-0.978147600733807,-0.207911690817754,1.95800148050649E-29));
#134757=DIRECTION('center_axis',(-0.207911690817763,0.978147600733805,6.80109070798532E-15));
#134758=DIRECTION('ref_axis',(0.978147600733805,0.207911690817763,-4.42525447058535E-29));
#134759=DIRECTION('center_axis',(-0.207911690817757,0.978147600733806,2.67097779288864E-14));
#134760=DIRECTION('ref_axis',(0.978147600733806,0.207911690817757,2.13282960949029E-31));
#134761=DIRECTION('center_axis',(-0.207911690817763,0.978147600733805,6.80109070798532E-15));
#134762=DIRECTION('ref_axis',(0.978147600733805,0.207911690817763,-4.42525447058535E-29));
#134763=DIRECTION('center_axis',(0.180092991631071,-0.847105178672037,0.499979330205147));
#134764=DIRECTION('ref_axis',(0.104894406048821,-0.488852904974673,-0.866036951219455));
#134765=DIRECTION('center_axis',(-0.10395691792829,0.489078846174027,-0.866022425483274));
#134766=DIRECTION('ref_axis',(6.38663846784148E-16,0.870740269393762,0.491743208652727));
#134767=DIRECTION('center_axis',(-0.103956919793601,0.489078854949547,-0.866022420303462));
#134768=DIRECTION('ref_axis',(-0.978147600732871,-0.207911690822154,-2.56575162955948E-12));
#134769=DIRECTION('center_axis',(0.154510046709071,-0.475533027084736,-0.866022508724565));
#134770=DIRECTION('ref_axis',(0.951056516293718,0.309016994379366,-2.70999321601511E-12));
#134771=DIRECTION('center_axis',(0.267585776505254,-0.823641557784567,-0.50001243634763));
#134772=DIRECTION('ref_axis',(-0.155453534437441,0.475234043107105,-0.866017784403404));
#134773=DIRECTION('center_axis',(-0.154510049384291,0.475533035318136,0.866022503726309));
#134774=DIRECTION('ref_axis',(-1.56718497740608E-15,-0.876548788012437,
0.481313018974064));
#134775=DIRECTION('center_axis',(-0.309016994374972,0.951056516295146,6.64119215765932E-15));
#134776=DIRECTION('ref_axis',(0.951056516295146,0.309016994374972,3.41480999208037E-15));
#134777=DIRECTION('center_axis',(0.309016994374951,-0.951056516295152,-6.59767734033507E-15));
#134778=DIRECTION('ref_axis',(-0.951056516295152,-0.309016994374951,-3.41480999208033E-15));
#134779=DIRECTION('center_axis',(0.309016994374964,-0.951056516295148,-6.64119215765934E-15));
#134780=DIRECTION('ref_axis',(-0.951056516295148,-0.309016994374964,-3.41480999208031E-15));
#134781=DIRECTION('center_axis',(0.309016994374951,-0.951056516295152,-6.59767734033507E-15));
#134782=DIRECTION('ref_axis',(-0.951056516295152,-0.309016994374951,-3.41480999208033E-15));
#134783=DIRECTION('center_axis',(-0.309016994374922,0.951056516295162,6.64119215765944E-15));
#134784=DIRECTION('ref_axis',(0.951056516295162,0.309016994374922,3.41480999208039E-15));
#134785=DIRECTION('center_axis',(0.163755587629901,-0.503987876168983,0.84804500363758));
#134786=DIRECTION('ref_axis',(2.36007916206428E-16,-0.859649462041489,-0.510884333691863));
#134787=DIRECTION('center_axis',(-0.154510091261978,0.475533164204401,-0.866022425483293));
#134788=DIRECTION('ref_axis',(2.20635803329686E-16,0.876548714628842,0.481313152617426));
#134789=DIRECTION('center_axis',(-0.163755599470739,0.503987842605832,-0.848045021297512));
#134790=DIRECTION('ref_axis',(-0.266156471022805,0.805199544415683,0.529919264233206));
#134791=DIRECTION('center_axis',(0.163755570286413,-0.503987822791216,0.848045038708642));
#134792=DIRECTION('ref_axis',(1.41142713906073E-15,-0.859649495083696,-0.510884278092747));
#134793=DIRECTION('center_axis',(-0.154510105538923,0.475533174130323,-0.866022417485766));
#134794=DIRECTION('ref_axis',(-0.271938812460818,0.822222161144676,0.499999999999979));
#134795=DIRECTION('center_axis',(-0.267587483539841,0.823661100222957,-0.499979330205082));
#134796=DIRECTION('ref_axis',(-0.153585232147035,0.475806237442058,0.866036951219504));
#134797=DIRECTION('center_axis',(-0.950981553003154,-0.309247612517397,
-2.15946453637257E-15));
#134798=DIRECTION('ref_axis',(-0.309247612517397,0.950981553003154,6.82961998416078E-15));
#134799=DIRECTION('center_axis',(0.309016994374951,-0.951056516295152,-6.59767734033507E-15));
#134800=DIRECTION('ref_axis',(-0.951056516295152,-0.309016994374951,-3.41480999208033E-15));
#134801=DIRECTION('center_axis',(-0.309016994374972,0.951056516295146,6.64119215765932E-15));
#134802=DIRECTION('ref_axis',(0.951056516295146,0.309016994374972,3.41480999208037E-15));
#134803=DIRECTION('center_axis',(-1.84331724214208E-16,-6.84903784078409E-15,
1.));
#134804=DIRECTION('ref_axis',(-1.,1.20258066624967E-30,-1.83352197722043E-16));
#134805=DIRECTION('center_axis',(-0.951131423661017,-0.308786358060986,
-2.15624361371854E-15));
#134806=DIRECTION('ref_axis',(-0.308786358060986,0.951131423661017,6.82961998416067E-15));
#134807=DIRECTION('center_axis',(-0.163755730877694,0.50398831704057,0.848044713969332));
#134808=DIRECTION('ref_axis',(4.71763757776837E-17,-0.859649189130476,0.510884792910609));
#134809=DIRECTION('center_axis',(-0.163755570286353,0.503987822791179,-0.848045038708675));
#134810=DIRECTION('ref_axis',(1.32327065984906E-15,0.859649495083721,0.510884278092704));
#134811=DIRECTION('center_axis',(-0.163755716975923,0.503988355850381,0.848044693589277));
#134812=DIRECTION('ref_axis',(0.266368911021071,-0.805129291875531,0.5299192642332));
#134813=DIRECTION('center_axis',(-0.163755751065448,0.503988379172,0.848044673146746));
#134814=DIRECTION('ref_axis',(-2.31894814760129E-15,-0.859649150669469,
0.510884857627685));
#134815=DIRECTION('center_axis',(0.163755599576039,-0.503987842738117,0.848045021198563));
#134816=DIRECTION('ref_axis',(-0.25795930914358,0.80786296376346,0.529919264233228));
#134817=DIRECTION('center_axis',(-0.163755587629911,0.503987876169013,-0.848045003637561));
#134818=DIRECTION('ref_axis',(1.28133843970483E-15,0.859649462041471,0.510884333691894));
#134819=DIRECTION('center_axis',(-0.950976702550718,-0.309262527968978,
-1.12416423283092E-14));
#134820=DIRECTION('ref_axis',(-0.309262527968978,0.950976702550718,6.82961998416086E-15));
#134821=DIRECTION('center_axis',(-0.309016994374964,0.951056516295148,6.64119215765934E-15));
#134822=DIRECTION('ref_axis',(0.951056516295148,0.309016994374964,3.41480999208031E-15));
#134823=DIRECTION('center_axis',(-1.84331724214208E-16,-6.84903784078409E-15,
1.));
#134824=DIRECTION('ref_axis',(-1.,1.28019500997425E-30,-1.87678573238334E-16));
#134825=DIRECTION('center_axis',(-0.951136266645025,-0.308771440182806,
-2.15613944273197E-15));
#134826=DIRECTION('ref_axis',(-0.308771440182806,0.951136266645025,6.82961998416067E-15));
#134827=DIRECTION('center_axis',(-0.309016994374951,0.951056516295152,6.59767734033507E-15));
#134828=DIRECTION('ref_axis',(0.951056516295152,0.309016994374951,3.41480999208041E-15));
#134829=DIRECTION('center_axis',(-0.267642920196027,0.823622990672906,0.500012436349299));
#134830=DIRECTION('ref_axis',(0.153571010712917,-0.475845712145576,0.866017784402424));
#134831=DIRECTION('center_axis',(0.163755751065493,-0.503988379172002,-0.848044673146736));
#134832=DIRECTION('ref_axis',(-1.92007597614245E-15,0.859649150669465,-0.510884857627692));
#134833=DIRECTION('center_axis',(0.154510035625077,-0.475533025683493,-0.866022511471521));
#134834=DIRECTION('ref_axis',(0.26335567262561,-0.825011387615885,0.500000000000024));
#134835=DIRECTION('center_axis',(-0.154510049384261,0.475533035318041,0.866022503726367));
#134836=DIRECTION('ref_axis',(-1.66937126522959E-15,-0.876548788012491,
0.481313018973965));
#134837=DIRECTION('center_axis',(0.163755716841192,-0.503988355689969,-0.848044693710625));
#134838=DIRECTION('ref_axis',(0.257746148176438,-0.807930997359779,0.529919264233187));
#134839=DIRECTION('center_axis',(0.163755730877767,-0.503988317040554,-0.848044713969328));
#134840=DIRECTION('ref_axis',(-4.27283864732672E-16,0.859649189130481,-0.510884792910599));
#134841=DIRECTION('center_axis',(-0.309016994374964,0.951056516295148,6.64119215765934E-15));
#134842=DIRECTION('ref_axis',(0.951056516295148,0.309016994374964,3.41480999208031E-15));
#134843=DIRECTION('center_axis',(0.309016994374964,-0.951056516295148,-6.64119215765934E-15));
#134844=DIRECTION('ref_axis',(-0.951056516295148,-0.309016994374964,-3.41480999208031E-15));
#134845=DIRECTION('center_axis',(-0.309016994374951,0.951056516295152,6.59767734033507E-15));
#134846=DIRECTION('ref_axis',(0.951056516295152,0.309016994374951,3.41480999208041E-15));
#134847=DIRECTION('center_axis',(-0.309016994374964,0.951056516295148,7.54877779975346E-14));
#134848=DIRECTION('ref_axis',(0.951056516295148,0.309016994374964,3.41480999207973E-15));
#134849=DIRECTION('center_axis',(-0.309016994374951,0.951056516295152,6.59767734033507E-15));
#134850=DIRECTION('ref_axis',(0.951056516295152,0.309016994374951,3.41480999208041E-15));
#134851=DIRECTION('center_axis',(0.267653025932096,-0.823639804208751,0.499979330205123));
#134852=DIRECTION('ref_axis',(0.15541882643867,-0.475210466541842,-0.866036951219468));
#134853=DIRECTION('center_axis',(-0.154510091261975,0.475533164204405,-0.866022425483291));
#134854=DIRECTION('ref_axis',(4.76968987462892E-16,0.87654871462884,0.48131315261743));
#134855=DIRECTION('center_axis',(-0.154510094034918,0.47553317273861,-0.866022420302426));
#134856=DIRECTION('ref_axis',(-0.951056516295898,-0.309016994372655,1.39870616942708E-12));
#134857=DIRECTION('center_axis',(0.203370361064571,-0.456777309673213,-0.866022508719126));
#134858=DIRECTION('ref_axis',(0.913545457644057,0.406736643072529,2.07183352317727E-12));
#134859=DIRECTION('center_axis',(0.352213899943352,-0.791159233140772,-0.500012436348137));
#134860=DIRECTION('ref_axis',(-0.204277427961519,0.456381342216139,-0.866017784403081));
#134861=DIRECTION('center_axis',(-0.203370364581912,0.456777317573267,0.866022503726313));
#134862=DIRECTION('ref_axis',(1.2472944269153E-15,-0.884507036382102,0.466526850878437));
#134863=DIRECTION('center_axis',(-0.406736643075807,0.913545457642598,6.37925383508808E-15));
#134864=DIRECTION('ref_axis',(0.913545457642598,0.406736643075807,3.4148099920803E-15));
#134865=DIRECTION('center_axis',(0.406736643075804,-0.913545457642599,-6.32197843909137E-15));
#134866=DIRECTION('ref_axis',(-0.913545457642599,-0.406736643075804,-3.41480999208033E-15));
#134867=DIRECTION('center_axis',(0.406736643075807,-0.913545457642598,-6.37925383508808E-15));
#134868=DIRECTION('ref_axis',(-0.913545457642598,-0.406736643075807,-3.4148099920803E-15));
#134869=DIRECTION('center_axis',(0.406736643075804,-0.913545457642599,-6.32197843909137E-15));
#134870=DIRECTION('ref_axis',(-0.913545457642599,-0.406736643075804,-3.41480999208033E-15));
#134871=DIRECTION('center_axis',(-0.406736643075817,0.913545457642594,6.37925383508805E-15));
#134872=DIRECTION('ref_axis',(0.913545457642593,0.406736643075817,3.41480999208037E-15));
#134873=DIRECTION('center_axis',(0.215539595588306,-0.484109857923776,0.848045003637573));
#134874=DIRECTION('ref_axis',(-8.96693424359429E-16,-0.868458021515992,
-0.495762710240019));
#134875=DIRECTION('center_axis',(-0.203370419702479,0.45677744137614,-0.866022425483258));
#134876=DIRECTION('ref_axis',(5.21321035819439E-17,0.884506966812022,0.466526982779128));
#134877=DIRECTION('center_axis',(-0.215539603846564,0.484109823311004,-0.848045021297487));
#134878=DIRECTION('ref_axis',(-0.348864709038018,0.77296765015256,0.529919264233192));
#134879=DIRECTION('center_axis',(0.215539572760321,-0.484109806651282,0.848045038708651));
#134880=DIRECTION('ref_axis',(1.04124665764134E-15,-0.868458052949961,-0.495762655175199));
#134881=DIRECTION('center_axis',(-0.203370434945702,0.456777449752215,-0.866022417485748));
#134882=DIRECTION('ref_axis',(-0.356394722164787,0.789292595944645,0.500000000000047));
#134883=DIRECTION('center_axis',(-0.35221764036688,0.791178490090346,-0.499979330205507));
#134884=DIRECTION('ref_axis',(-0.202479170976877,0.457145692797587,0.866036951219248));
#134885=DIRECTION('center_axis',(-0.913446798847324,-0.406958162070226,
-2.84177365711619E-15));
#134886=DIRECTION('ref_axis',(-0.406958162070226,0.913446798847324,6.82961998416052E-15));
#134887=DIRECTION('center_axis',(0.406736643075804,-0.913545457642599,-6.32197843909137E-15));
#134888=DIRECTION('ref_axis',(-0.913545457642599,-0.406736643075804,-3.41480999208033E-15));
#134889=DIRECTION('center_axis',(-0.406736643075817,0.913545457642594,6.37925383508805E-15));
#134890=DIRECTION('ref_axis',(0.913545457642593,0.406736643075817,3.41480999208037E-15));
#134891=DIRECTION('center_axis',(-1.98092302886631E-16,-6.85432003203771E-15,
1.));
#134892=DIRECTION('ref_axis',(-1.,1.60344088833289E-30,-1.97456212931431E-16));
#134893=DIRECTION('center_axis',(-0.913644062717546,-0.406515100163544,
-2.83867977235792E-15));
#134894=DIRECTION('ref_axis',(-0.406515100163544,0.913644062717546,6.82961998416061E-15));
#134895=DIRECTION('center_axis',(-0.21553978413504,0.484110281406725,0.84804471396933));
#134896=DIRECTION('ref_axis',(1.68002389095411E-15,-0.868457761888284,0.495763165045561));
#134897=DIRECTION('center_axis',(-0.215539572760312,0.48410980665126,-0.848045038708666));
#134898=DIRECTION('ref_axis',(-2.44700238975538E-15,0.868458052949974,0.495762655175175));
#134899=DIRECTION('center_axis',(-0.215539774366204,0.484110321457017,0.848044693589288));
#134900=DIRECTION('ref_axis',(0.349068641889459,-0.772875576431343,0.529919264233116));
#134901=DIRECTION('center_axis',(-0.215539810706662,0.484110341087615,0.848044673146745));
#134902=DIRECTION('ref_axis',(8.10725224855173E-16,-0.86845772529927,0.495763229140704));
#134903=DIRECTION('center_axis',(0.215539603979383,-0.484109823425178,0.848045021198553));
#134904=DIRECTION('ref_axis',(-0.340990855174767,0.776473315756408,0.529919264233177));
#134905=DIRECTION('center_axis',(-0.215539595588304,0.484109857923771,-0.848045003637576));
#134906=DIRECTION('ref_axis',(3.1646774827737E-16,0.868458021515995,0.495762710240014));
#134907=DIRECTION('center_axis',(-0.913440415876946,-0.406972488803054,
-2.50776132404211E-14));
#134908=DIRECTION('ref_axis',(-0.406972488803054,0.913440415876946,6.82961998416034E-15));
#134909=DIRECTION('center_axis',(-0.406736643075807,0.913545457642598,1.74906806584517E-14));
#134910=DIRECTION('ref_axis',(0.913545457642598,0.406736643075807,3.4148099920803E-15));
#134911=DIRECTION('center_axis',(-1.98092302886631E-16,-6.85432003203771E-15,
1.));
#134912=DIRECTION('ref_axis',(-1.,1.28019500997425E-30,-1.95185716167867E-16));
#134913=DIRECTION('center_axis',(-0.913650438514062,-0.40650077023674,-2.83857970701388E-15));
#134914=DIRECTION('ref_axis',(-0.40650077023674,0.913650438514061,6.8296199841608E-15));
#134915=DIRECTION('center_axis',(-0.406736643075804,0.913545457642599,6.32197843909137E-15));
#134916=DIRECTION('ref_axis',(0.913545457642599,0.406736643075804,3.41480999208028E-15));
#134917=DIRECTION('center_axis',(-0.352268789800574,0.791134794601461,0.500012436348681));
#134918=DIRECTION('ref_axis',(0.202469153692002,-0.457186437792438,0.866017784402783));
#134919=DIRECTION('center_axis',(0.215539810706706,-0.4841103410876,-0.848044673146743));
#134920=DIRECTION('ref_axis',(-1.47259052727932E-15,0.868457725299275,-0.495763229140694));
#134921=DIRECTION('center_axis',(0.203370349883188,-0.456777309433043,-0.866022511471555));
#134922=DIRECTION('ref_axis',(0.348150155221207,-0.792963725159901,0.499999999999983));
#134923=DIRECTION('center_axis',(-0.203370364581871,0.456777317573174,0.866022503726371));
#134924=DIRECTION('ref_axis',(1.52619955059002E-15,-0.884507036382154,0.466526850878339));
#134925=DIRECTION('center_axis',(0.215539774217316,-0.484110321310761,-0.848044693710621));
#134926=DIRECTION('ref_axis',(0.340785973383427,-0.776563258041277,0.529919264233172));
#134927=DIRECTION('center_axis',(0.215539784135144,-0.484110281406682,-0.848044713969328));
#134928=DIRECTION('ref_axis',(1.69535706659914E-15,0.868457761888303,-0.495763165045528));
#134929=DIRECTION('center_axis',(-0.406736643075807,0.913545457642598,6.37925383508808E-15));
#134930=DIRECTION('ref_axis',(0.913545457642598,0.406736643075807,3.4148099920803E-15));
#134931=DIRECTION('center_axis',(0.406736643075807,-0.913545457642598,-6.37925383508808E-15));
#134932=DIRECTION('ref_axis',(-0.913545457642598,-0.406736643075807,-3.4148099920803E-15));
#134933=DIRECTION('center_axis',(-0.406736643075804,0.913545457642599,6.32197843909137E-15));
#134934=DIRECTION('ref_axis',(0.913545457642599,0.406736643075804,3.41480999208028E-15));
#134935=DIRECTION('center_axis',(-0.406736643075807,0.913545457642598,-1.58435998116392E-14));
#134936=DIRECTION('ref_axis',(0.913545457642598,0.406736643075807,3.4148099920803E-15));
#134937=DIRECTION('center_axis',(-0.406736643075804,0.913545457642599,6.32197843909137E-15));
#134938=DIRECTION('ref_axis',(0.913545457642599,0.406736643075804,3.41480999208028E-15));
#134939=DIRECTION('center_axis',(0.352280597671406,-0.791150459692788,0.499979330204927));
#134940=DIRECTION('ref_axis',(0.204240445639035,-0.456361522794654,-0.866036951219584));
#134941=DIRECTION('center_axis',(-0.203370419702479,0.4567774413761,-0.866022425483279));
#134942=DIRECTION('ref_axis',(-2.08635189661219E-15,0.884506966812044,0.466526982779087));
#134943=DIRECTION('center_axis',(-0.203370423353607,0.456777449576576,-0.866022420300591));
#134944=DIRECTION('ref_axis',(-0.913545457644566,-0.406736643071388,2.81926712275846E-12));
#134945=DIRECTION('center_axis',(0.250002507180728,-0.433017044456612,-0.866022508722152));
#134946=DIRECTION('ref_axis',(0.866025403787112,0.49999999999537,3.0815245439773E-12));
#134947=DIRECTION('center_axis',(0.432983094187539,-0.750008802379581,-0.500012436346269));
#134948=DIRECTION('ref_axis',(-0.250863215247079,0.432528431818864,-0.866017784404115));
#134949=DIRECTION('center_axis',(-0.250002511507198,0.433017051950273,0.866022503726311));
#134950=DIRECTION('ref_axis',(-4.23904869311635E-16,-0.894424794863787,
0.447218387740121));
#134951=DIRECTION('center_axis',(-0.499999999999998,0.86602540378444,6.70236582766913E-14));
#134952=DIRECTION('ref_axis',(0.86602540378444,0.499999999999998,3.41480999207943E-15));
#134953=DIRECTION('center_axis',(0.500000000000004,-0.866025403784436,-5.97701461910994E-15));
#134954=DIRECTION('ref_axis',(-0.866025403784436,-0.500000000000004,-3.41480999208033E-15));
#134955=DIRECTION('center_axis',(0.50000000000001,-0.866025403784433,-6.04742307255487E-15));
#134956=DIRECTION('ref_axis',(-0.866025403784433,-0.50000000000001,-3.41480999208034E-15));
#134957=DIRECTION('center_axis',(0.500000000000004,-0.866025403784436,-5.97701461910994E-15));
#134958=DIRECTION('ref_axis',(-0.866025403784436,-0.500000000000004,-3.41480999208033E-15));
#134959=DIRECTION('center_axis',(-0.50000000000001,0.866025403784433,6.04742307255487E-15));
#134960=DIRECTION('ref_axis',(0.866025403784433,0.50000000000001,3.41480999208034E-15));
#134961=DIRECTION('center_axis',(0.264962106632886,-0.458927830768649,0.84804500363757));
#134962=DIRECTION('ref_axis',(-1.55726465520226E-15,-0.879478602053318,
-0.475938429348105));
#134963=DIRECTION('center_axis',(-0.250002579266717,0.433017169313229,-0.866022425483282));
#134964=DIRECTION('ref_axis',(-1.52069700702419E-17,0.89442473021641,0.447218517033119));
#134965=DIRECTION('center_axis',(-0.264962111229841,0.458927795481119,-0.848045021297493));
#134966=DIRECTION('ref_axis',(-0.427750712273125,0.732266960571309,0.529919264233234));
#134967=DIRECTION('center_axis',(0.264962078570521,-0.458927782163207,0.848045038708646));
#134968=DIRECTION('ref_axis',(2.63879185457581E-16,-0.879478631391249,-0.475938375135033));
#134969=DIRECTION('center_axis',(-0.250002595299953,0.433017176051205,-0.866022417485787));
#134970=DIRECTION('ref_axis',(-0.436945896712322,0.747715375892674,0.499999999999942));
#134971=DIRECTION('center_axis',(-0.432988827019173,0.750027562856349,-0.499979330205085));
#134972=DIRECTION('ref_axis',(-0.249154705660435,0.433476564268119,0.866036951219501));
#134973=DIRECTION('center_axis',(-0.865904130412325,-0.500209992837883,
-3.49294771099265E-15));
#134974=DIRECTION('ref_axis',(-0.500209992837883,0.865904130412325,6.82961998416073E-15));
#134975=DIRECTION('center_axis',(0.500000000000004,-0.866025403784436,-5.97701461910994E-15));
#134976=DIRECTION('ref_axis',(-0.866025403784436,-0.500000000000004,-3.41480999208033E-15));
#134977=DIRECTION('center_axis',(-0.500000000000022,0.866025403784426,6.04742307255483E-15));
#134978=DIRECTION('ref_axis',(0.866025403784426,0.500000000000022,3.41480999208042E-15));
#134979=DIRECTION('center_axis',(-2.11225360334866E-16,-6.86101165903726E-15,
1.));
#134980=DIRECTION('ref_axis',(-1.,1.60344088833289E-30,-2.11560228140819E-16));
#134981=DIRECTION('center_axis',(-0.866146626230631,-0.499789977759954,
-3.49001476137941E-15));
#134982=DIRECTION('ref_axis',(-0.499789977759954,0.866146626230631,6.82961998416062E-15));
#134983=DIRECTION('center_axis',(-0.264962338412801,0.458928232223198,0.848044713969323));
#134984=DIRECTION('ref_axis',(-1.17907827621235E-15,-0.879478359737748,
0.475938877118691));
#134985=DIRECTION('center_axis',(-0.264962078570535,0.458927782163217,-0.848045038708636));
#134986=DIRECTION('ref_axis',(2.54209381385958E-16,0.879478631391243,0.475938375135045));
#134987=DIRECTION('center_axis',(-0.264962332887377,0.458928273073164,0.848044693589296));
#134988=DIRECTION('ref_axis',(0.427943903629752,-0.73215407445476,0.529919264233169));
#134989=DIRECTION('center_axis',(-0.264962371077225,0.458928288799655,0.848044673146737));
#134990=DIRECTION('ref_axis',(8.29844606197542E-17,-0.879478325588509,0.475938940222412));
#134991=DIRECTION('center_axis',(0.264962111362087,-0.458927795587544,0.848045021198581));
#134992=DIRECTION('ref_axis',(-0.420286434088522,0.736576463590586,0.52991926423328));
#134993=DIRECTION('center_axis',(-0.264962106632899,0.458927830768658,-0.848045003637561));
#134994=DIRECTION('ref_axis',(2.40514549107199E-15,0.879478602053312,0.475938429348116));
#134995=DIRECTION('center_axis',(-0.865896284857136,-0.500223573885327,
-7.16876759590109E-15));
#134996=DIRECTION('ref_axis',(-0.500223573885327,0.865896284857136,6.82961998416072E-15));
#134997=DIRECTION('center_axis',(-0.50000000000001,0.866025403784433,-7.61181689576648E-15));
#134998=DIRECTION('ref_axis',(0.866025403784433,0.50000000000001,3.41480999208034E-15));
#134999=DIRECTION('center_axis',(-2.11225360334866E-16,-6.86101165903726E-15,
1.));
#135000=DIRECTION('ref_axis',(-1.,1.70692667996567E-30,-2.10200002026934E-16));
#135001=DIRECTION('center_axis',(-0.866154464985103,-0.499776392786184,
2.38163428202604E-14));
#135002=DIRECTION('ref_axis',(-0.499776392786184,0.866154464985103,6.82961998416098E-15));
#135003=DIRECTION('center_axis',(-0.500000000000004,0.866025403784436,5.97701461910994E-15));
#135004=DIRECTION('ref_axis',(0.866025403784436,0.500000000000004,3.4148099920803E-15));
#135005=DIRECTION('center_axis',(-0.43303512883018,0.74997876016208,0.500012436350116));
#135006=DIRECTION('ref_axis',(0.249149002218687,-0.433518133176716,0.866017784401919));
#135007=DIRECTION('center_axis',(0.264962371077208,-0.458928288799654,-0.848044673146743));
#135008=DIRECTION('ref_axis',(-3.50114051472713E-16,0.879478325588511,-0.475938940222409));
#135009=DIRECTION('center_axis',(0.250002496045881,-0.433017045386664,-0.866022511471516));
#135010=DIRECTION('ref_axis',(0.42913023185866,-0.752228186194135,0.500000000000015));
#135011=DIRECTION('center_axis',(-0.250002511507148,0.433017051950186,0.866022503726369));
#135012=DIRECTION('ref_axis',(-1.26959939242869E-15,-0.894424794863834,
0.447218387740026));
#135013=DIRECTION('center_axis',(0.26496233271549,-0.458928272948179,-0.848044693710637));
#135014=DIRECTION('ref_axis',(0.420092076158679,-0.736687329158891,0.529919264233176));
#135015=DIRECTION('center_axis',(0.264962338412815,-0.458928232223186,-0.848044713969325));
#135016=DIRECTION('ref_axis',(3.76176649168549E-16,0.879478359737753,-0.475938877118681));
#135017=DIRECTION('center_axis',(-0.50000000000001,0.866025403784433,5.33644183083698E-14));
#135018=DIRECTION('ref_axis',(0.866025403784433,0.50000000000001,3.41480999208034E-15));
#135019=DIRECTION('center_axis',(0.50000000000001,-0.866025403784433,-6.04742307255487E-15));
#135020=DIRECTION('ref_axis',(-0.866025403784433,-0.50000000000001,-3.41480999208034E-15));
#135021=DIRECTION('center_axis',(-0.500000000000004,0.866025403784436,5.97701461910994E-15));
#135022=DIRECTION('ref_axis',(0.866025403784436,0.500000000000004,3.4148099920803E-15));
#135023=DIRECTION('center_axis',(-0.50000000000001,0.866025403784433,1.41659133449149E-13));
#135024=DIRECTION('ref_axis',(0.866025403784433,0.50000000000001,3.41480999208033E-15));
#135025=DIRECTION('center_axis',(-0.500000000000004,0.866025403784436,5.97701461910994E-15));
#135026=DIRECTION('ref_axis',(0.866025403784436,0.500000000000004,3.4148099920803E-15));
#135027=DIRECTION('center_axis',(0.433048509461644,-0.749993105181733,0.49997933020567));
#135028=DIRECTION('ref_axis',(0.250824363776384,-0.432512586706094,-0.866036951219159));
#135029=DIRECTION('center_axis',(-0.250002579266721,0.433017169313221,-0.866022425483285));
#135030=DIRECTION('ref_axis',(-5.6317795126628E-16,0.894424730216414,0.447218517033111));
#135031=DIRECTION('center_axis',(-0.25000258375266,0.433017177083137,-0.866022420303277));
#135032=DIRECTION('ref_axis',(-0.86602540378567,-0.499999999997868,1.38122234231956E-12));
#135033=DIRECTION('center_axis',(0.293895573516245,-0.40451255389424,-0.866022508719904));
#135034=DIRECTION('ref_axis',(0.809016994374529,0.587785252293049,-3.93386111998895E-13));
#135035=DIRECTION('center_axis',(0.509008435041564,-0.700641118228579,-0.500012436349281));
#135036=DIRECTION('ref_axis',(-0.294700492544349,0.403936649479602,-0.86601778440244));
#135037=DIRECTION('center_axis',(-0.293895578600006,0.404512560891461,0.866022503726318));
#135038=DIRECTION('ref_axis',(-1.11508461107079E-15,-0.906035256115486,
0.423202214875756));
#135039=DIRECTION('center_axis',(-0.58778525229247,0.80901699437495,5.6493354773342E-15));
#135040=DIRECTION('ref_axis',(0.80901699437495,0.58778525229247,3.41480999208022E-15));
#135041=DIRECTION('center_axis',(0.587785252292477,-0.809016994374945,-5.56656537619083E-15));
#135042=DIRECTION('ref_axis',(-0.809016994374945,-0.587785252292477,-3.41480999208033E-15));
#135043=DIRECTION('center_axis',(0.587785252292496,-0.809016994374931,-5.64933547733406E-15));
#135044=DIRECTION('ref_axis',(-0.809016994374931,-0.587785252292496,-3.41480999208037E-15));
#135045=DIRECTION('center_axis',(0.587785252292477,-0.809016994374945,-5.56656537619083E-15));
#135046=DIRECTION('ref_axis',(-0.809016994374945,-0.587785252292477,-3.41480999208033E-15));
#135047=DIRECTION('center_axis',(-0.58778525229247,0.80901699437495,5.6493354773342E-15));
#135048=DIRECTION('ref_axis',(0.80901699437495,0.58778525229247,3.41480999208022E-15));
#135049=DIRECTION('center_axis',(0.311481637390311,-0.428717694262762,0.848045003637585));
#135050=DIRECTION('ref_axis',(-4.68396541467905E-16,-0.89244205802627,-0.451162025292285));
#135051=DIRECTION('center_axis',(-0.293895658256084,0.404512670528685,-0.866022425483298));
#135052=DIRECTION('ref_axis',(-1.37831840766723E-15,0.906035197473495,0.423202340422599));
#135053=DIRECTION('center_axis',(-0.311481638273913,0.428717658687788,-0.84804502129749));
#135054=DIRECTION('ref_axis',(-0.501950189201556,0.683543400930059,0.529919264233232));
#135055=DIRECTION('center_axis',(0.311481604401037,-0.428717648856923,0.848045038708646));
#135056=DIRECTION('ref_axis',(4.76842727666993E-16,-0.892442084777734,-0.451161972375301));
#135057=DIRECTION('center_axis',(-0.293895674905427,0.404512675554181,-0.866022417485761));
#135058=DIRECTION('ref_axis',(-0.512709800571862,0.697946029716874,0.500000000000014));
#135059=DIRECTION('center_axis',(-0.509016097474244,0.70065917668986,-0.499979330205139));
#135060=DIRECTION('ref_axis',(-0.293100449232004,0.405058175800086,0.866036951219464));
#135061=DIRECTION('center_axis',(-0.808874435122379,-0.587981418248444,
-4.10585229880193E-15));
#135062=DIRECTION('ref_axis',(-0.587981418248444,0.808874435122379,6.82961998416087E-15));
#135063=DIRECTION('center_axis',(0.587785252292477,-0.809016994374945,-5.56656537619083E-15));
#135064=DIRECTION('ref_axis',(-0.809016994374945,-0.587785252292477,-3.41480999208033E-15));
#135065=DIRECTION('center_axis',(-0.58778525229247,0.80901699437495,5.6493354773342E-15));
#135066=DIRECTION('ref_axis',(0.80901699437495,0.58778525229247,3.41480999208022E-15));
#135067=DIRECTION('center_axis',(-2.23587008033243E-16,-6.86903940691702E-15,
1.));
#135068=DIRECTION('ref_axis',(-1.,1.60344088833289E-30,-2.25664243350207E-16));
#135069=DIRECTION('center_axis',(-0.809159506053914,-0.587589051772227,
-4.10311241834253E-15));
#135070=DIRECTION('ref_axis',(-0.587589051772227,0.809159506053914,6.82961998416088E-15));
#135071=DIRECTION('center_axis',(-0.311481909863919,0.428718069290538,0.848044713969328));
#135072=DIRECTION('ref_axis',(-3.03126833680443E-15,-0.892441837073397,
0.45116246235814));
#135073=DIRECTION('center_axis',(-0.311481604401053,0.428717648856944,-0.848045038708629));
#135074=DIRECTION('ref_axis',(5.0971935593662E-16,0.892442084777722,0.451161972375325));
#135075=DIRECTION('center_axis',(-0.311481908636353,0.428718110496056,0.848044693589286));
#135076=DIRECTION('ref_axis',(0.502130522416782,-0.683410939224696,0.529919264233211));
#135077=DIRECTION('center_axis',(-0.31148194826326,0.428718122142697,0.848044673146741));
#135078=DIRECTION('ref_axis',(3.18320034982604E-16,-0.892441805934779,0.451162523953254));
#135079=DIRECTION('center_axis',(0.311481638422179,-0.428717658775754,0.848045021198563));
#135080=DIRECTION('ref_axis',(-0.494977266831898,0.688609525576092,0.529919264233236));
#135081=DIRECTION('center_axis',(-0.311481637390301,0.428717694262749,-0.848045003637595));
#135082=DIRECTION('ref_axis',(-1.11423082982692E-15,0.892442058026277,0.45116202529227));
#135083=DIRECTION('center_axis',(-0.808865212939984,-0.587994104813606,
-4.10594088861296E-15));
#135084=DIRECTION('ref_axis',(-0.587994104813606,0.808865212939984,6.82961998416048E-15));
#135085=DIRECTION('center_axis',(-0.587785252292496,0.809016994374931,5.64933547733406E-15));
#135086=DIRECTION('ref_axis',(0.809016994374931,0.587785252292496,3.41480999208037E-15));
#135087=DIRECTION('center_axis',(-2.23587008033243E-16,-6.86903940691702E-15,
1.));
#135088=DIRECTION('ref_axis',(-1.,1.70692667996567E-30,-2.25214287886E-16));
#135089=DIRECTION('center_axis',(-0.80916872188328,-0.587576360591353,2.80003622398218E-14));
#135090=DIRECTION('ref_axis',(-0.587576360591353,0.809168721883279,6.82961998416027E-15));
#135091=DIRECTION('center_axis',(-0.587785252292477,0.809016994374945,5.56656537619083E-15));
#135092=DIRECTION('ref_axis',(0.809016994374945,0.587785252292477,3.41480999208025E-15));
#135093=DIRECTION('center_axis',(-0.509057044367654,0.700605801485977,0.500012436349198));
#135094=DIRECTION('ref_axis',(0.293099122184579,-0.40510011314894,0.86601778440246));
#135095=DIRECTION('center_axis',(0.311481948263274,-0.428718122142706,-0.848044673146732));
#135096=DIRECTION('ref_axis',(8.47741889849977E-16,0.892441805934773,-0.451162523953265));
#135097=DIRECTION('center_axis',(0.29389556253521,-0.404512555981462,-0.866022511471531));
#135098=DIRECTION('ref_axis',(0.505408667886012,-0.703251077799154,0.500000000000015));
#135099=DIRECTION('center_axis',(-0.293895578599989,0.40451256089141,0.866022503726348));
#135100=DIRECTION('ref_axis',(1.46405018279522E-15,-0.906035256115512,0.423202214875701));
#135101=DIRECTION('center_axis',(0.311481908456066,-0.428718110387007,-0.848044693710633));
#135102=DIRECTION('ref_axis',(0.494795562239831,-0.688740099734527,0.529919264233188));
#135103=DIRECTION('center_axis',(0.311481909863932,-0.428718069290516,-0.848044713969334));
#135104=DIRECTION('ref_axis',(1.60825548672769E-15,0.892441837073407,-0.45116246235812));
#135105=DIRECTION('center_axis',(-0.587785252292496,0.809016994374931,8.19663637794157E-14));
#135106=DIRECTION('ref_axis',(0.809016994374931,0.587785252292496,3.41480999208037E-15));
#135107=DIRECTION('center_axis',(0.587785252292496,-0.809016994374931,-5.64933547733406E-15));
#135108=DIRECTION('ref_axis',(-0.809016994374931,-0.587785252292496,-3.41480999208037E-15));
#135109=DIRECTION('center_axis',(-0.587785252292477,0.809016994374945,5.56656537619083E-15));
#135110=DIRECTION('ref_axis',(0.809016994374945,0.587785252292477,3.41480999208025E-15));
#135111=DIRECTION('center_axis',(-0.587785252292496,0.809016994374931,5.64933547733406E-15));
#135112=DIRECTION('ref_axis',(0.809016994374931,0.587785252292496,3.41480999208037E-15));
#135113=DIRECTION('center_axis',(-0.587785252292477,0.809016994374945,5.56656537619083E-15));
#135114=DIRECTION('ref_axis',(0.809016994374945,0.587785252292477,3.41480999208025E-15));
#135115=DIRECTION('center_axis',(0.509071851162528,-0.700618669263996,0.499979330205464));
#135116=DIRECTION('ref_axis',(0.294660197709419,-0.40392495219865,-0.866036951219268));
#135117=DIRECTION('center_axis',(-0.293895658256125,0.404512670528687,-0.866022425483283));
#135118=DIRECTION('ref_axis',(-1.31874420873521E-15,0.906035197473491,0.423202340422608));
#135119=DIRECTION('center_axis',(-0.293895663531681,0.404512677789842,-0.866022420301325));
#135120=DIRECTION('ref_axis',(-0.809016994375559,-0.587785252291632,6.29417776249093E-13));
#135121=DIRECTION('center_axis',(0.334568658444718,-0.371576139138295,-0.866022508719941));
#135122=DIRECTION('ref_axis',(0.743144825481234,0.669130606354594,3.34378195195858E-12));
#135123=DIRECTION('center_axis',(0.579456972966719,-0.643597063368448,-0.500012436349093));
#135124=DIRECTION('ref_axis',(-0.33530896966219,0.37091925261791,-0.866017784402521));
#135125=DIRECTION('center_axis',(-0.334568664232084,0.371576145565846,0.866022503726311));
#135126=DIRECTION('ref_axis',(-6.66659759826789E-17,-0.918982183096515,
0.394299058014553));
#135127=DIRECTION('center_axis',(-0.669130606358875,0.743144825477379,5.18935258042421E-15));
#135128=DIRECTION('ref_axis',(0.743144825477379,0.669130606358875,3.41480999208015E-15));
#135129=DIRECTION('center_axis',(0.669130606358862,-0.743144825477391,-5.09512767813147E-15));
#135130=DIRECTION('ref_axis',(-0.743144825477391,-0.669130606358862,-3.41480999208033E-15));
#135131=DIRECTION('center_axis',(0.669130606358845,-0.743144825477406,-3.77047027500057E-14));
#135132=DIRECTION('ref_axis',(-0.743144825477406,-0.669130606358845,-3.41480999208033E-15));
#135133=DIRECTION('center_axis',(0.669130606358862,-0.743144825477391,-5.09512767813147E-15));
#135134=DIRECTION('ref_axis',(-0.743144825477391,-0.669130606358862,-3.41480999208033E-15));
#135135=DIRECTION('center_axis',(-0.669130606358872,0.743144825477382,5.18935258042423E-15));
#135136=DIRECTION('ref_axis',(0.743144825477382,0.669130606358872,3.41480999208052E-15));
#135137=DIRECTION('center_axis',(0.354588510146763,-0.393810436983653,0.848045003637568));
#135138=DIRECTION('ref_axis',(2.80320064824192E-15,-0.906978223357755,-0.421177518814584));
#135139=DIRECTION('center_axis',(-0.334568754912021,0.371576246276131,-0.86602242548329));
#135140=DIRECTION('ref_axis',(2.58413282129854E-15,0.91898213146364,0.39429917835388));
#135141=DIRECTION('center_axis',(-0.354588507309677,0.393810401508679,-0.848045021297495));
#135142=DIRECTION('ref_axis',(-0.570650194820549,0.627330796745847,0.529919264233231));
#135143=DIRECTION('center_axis',(0.354588472592004,-0.393810395274868,0.84804503870863));
#135144=DIRECTION('ref_axis',(1.40544149701058E-15,-0.906978247051282,-0.421177467792122));
#135145=DIRECTION('center_axis',(-0.334568771995868,0.37157624953337,-0.866022417485767));
#135146=DIRECTION('ref_axis',(-0.582856348576968,0.640529840775232,0.49999999999998));
#135147=DIRECTION('center_axis',(-0.57946648104675,0.643614221961317,-0.499979330205185));
#135148=DIRECTION('ref_axis',(-0.333834922946612,0.372201885196443,0.866036951219429));
#135149=DIRECTION('center_axis',(-0.742982542253438,-0.669310796197565,
-4.67377230962008E-15));
#135150=DIRECTION('ref_axis',(-0.669310796197565,0.742982542253438,6.82961998416081E-15));
#135151=DIRECTION('center_axis',(0.669130606358862,-0.743144825477391,-5.09512767813147E-15));
#135152=DIRECTION('ref_axis',(-0.743144825477391,-0.669130606358862,-3.41480999208033E-15));
#135153=DIRECTION('center_axis',(-0.669130606358869,0.743144825477384,5.18935258042425E-15));
#135154=DIRECTION('ref_axis',(0.743144825477384,0.669130606358869,3.41480999208049E-15));
#135155=DIRECTION('center_axis',(-2.35041809182736E-16,-6.8783153219913E-15,
1.));
#135156=DIRECTION('ref_axis',(-1.,1.60344088833289E-30,-2.32716250954901E-16));
#135157=DIRECTION('center_axis',(-0.743307065001301,-0.668950377172442,
-4.67125551701931E-15));
#135158=DIRECTION('ref_axis',(-0.668950377172442,0.743307065001301,6.82961998416084E-15));
#135159=DIRECTION('center_axis',(-0.35458882032882,0.393810781475678,0.848044713969335));
#135160=DIRECTION('ref_axis',(8.82527612096891E-17,-0.906978027661855,0.421177940232642));
#135161=DIRECTION('center_axis',(-0.354588472592003,0.393810395274867,-0.848045038708631));
#135162=DIRECTION('ref_axis',(-1.80259659354061E-15,0.906978247051282,0.421177467792121));
#135163=DIRECTION('center_axis',(-0.354588823415871,0.393810822583094,0.848044693589303));
#135164=DIRECTION('ref_axis',(0.570815694129367,-0.627180210729071,0.529919264233191));
#135165=DIRECTION('center_axis',(-0.354588864042336,0.393810830024526,0.848044673146739));
#135166=DIRECTION('ref_axis',(-7.39505541680538E-17,-0.906978000082647,
0.421177999622584));
#135167=DIRECTION('center_axis',(0.354588507468212,-0.393810401579006,0.848045021198549));
#135168=DIRECTION('ref_axis',(-0.564245025055622,0.633098037506472,0.52991926423318));
#135169=DIRECTION('center_axis',(-0.354588510146757,0.393810436983647,-0.848045003637574));
#135170=DIRECTION('ref_axis',(-3.65482701585664E-15,0.906978223357759,0.421177518814577));
#135171=DIRECTION('center_axis',(-0.742972044483925,-0.669322449283883,
-4.67385368268692E-15));
#135172=DIRECTION('ref_axis',(-0.669322449283883,0.742972044483925,6.82961998416059E-15));
#135173=DIRECTION('center_axis',(-0.669130606358845,0.743144825477406,5.1893525804244E-15));
#135174=DIRECTION('ref_axis',(0.743144825477406,0.669130606358845,3.41480999208033E-15));
#135175=DIRECTION('center_axis',(-2.35041809182736E-16,-6.8783153219913E-15,
1.));
#135176=DIRECTION('ref_axis',(-1.,1.70692667996567E-30,-2.32721430815534E-16));
#135177=DIRECTION('center_axis',(-0.743317556935059,-0.668938718831625,
-4.6711741072605E-15));
#135178=DIRECTION('ref_axis',(-0.668938718831625,0.743317556935059,6.82961998416081E-15));
#135179=DIRECTION('center_axis',(-0.669130606358862,0.743144825477391,5.09512767813147E-15));
#135180=DIRECTION('ref_axis',(0.743144825477391,0.669130606358862,3.41480999208025E-15));
#135181=DIRECTION('center_axis',(-0.579501624401052,0.643556859035853,0.500012436349787));
#135182=DIRECTION('ref_axis',(0.333837986823119,-0.372243731516236,0.866017784402119));
#135183=DIRECTION('center_axis',(0.354588864042412,-0.393810830024448,-0.848044673146744));
#135184=DIRECTION('ref_axis',(3.48152255375756E-15,0.90697800008268,-0.421177999622512));
#135185=DIRECTION('center_axis',(0.334568647739284,-0.371576142364415,-0.866022511471548));
#135186=DIRECTION('ref_axis',(0.576149740768964,-0.646569003441916,0.499999999999983));
#135187=DIRECTION('center_axis',(-0.334568664232057,0.371576145565816,0.866022503726334));
#135188=DIRECTION('ref_axis',(2.06791103391257E-15,-0.91898218309653,0.394299058014518));
#135189=DIRECTION('center_axis',(0.354588823232584,-0.393810822486946,-0.848044693710589));
#135190=DIRECTION('ref_axis',(0.564077964606995,-0.633246889640457,0.529919264233257));
#135191=DIRECTION('center_axis',(0.354588820328813,-0.393810781475708,-0.848044713969324));
#135192=DIRECTION('ref_axis',(1.92894670706085E-15,0.906978027661841,-0.421177940232672));
#135193=DIRECTION('center_axis',(-0.669130606358845,0.743144825477406,-3.13699095091902E-14));
#135194=DIRECTION('ref_axis',(0.743144825477406,0.669130606358845,3.41480999208033E-15));
#135195=DIRECTION('center_axis',(0.669130606358875,-0.743144825477379,-5.18935258042421E-15));
#135196=DIRECTION('ref_axis',(-0.743144825477379,-0.669130606358875,-3.41480999208015E-15));
#135197=DIRECTION('center_axis',(-0.669130606358862,0.743144825477391,5.09512767813147E-15));
#135198=DIRECTION('ref_axis',(0.743144825477391,0.669130606358862,3.41480999208025E-15));
#135199=DIRECTION('center_axis',(-0.669130606358845,0.743144825477406,1.1454406603911E-15));
#135200=DIRECTION('ref_axis',(0.743144825477406,0.669130606358845,3.41480999208033E-15));
#135201=DIRECTION('center_axis',(-0.669130606358862,0.743144825477391,5.09512767813147E-15));
#135202=DIRECTION('ref_axis',(0.743144825477391,0.669130606358862,3.41480999208025E-15));
#135203=DIRECTION('center_axis',(0.579517695132059,-0.643568108591841,0.499979330205107));
#135204=DIRECTION('ref_axis',(0.335267672834652,-0.370911831402689,-0.866036951219485));
#135205=DIRECTION('center_axis',(-0.334568754912014,0.371576246276123,-0.866022425483296));
#135206=DIRECTION('ref_axis',(1.52738427012904E-15,0.918982131463644,0.394299178353872));
#135207=DIRECTION('center_axis',(-0.334568760917208,0.37157625294558,-0.866022420301719));
#135208=DIRECTION('ref_axis',(-0.743144825476697,-0.669130606359632,-6.3378873303023E-13));
#135209=DIRECTION('center_axis',(0.371576139132289,-0.334568658439294,-0.866022508724614));
#135210=DIRECTION('ref_axis',(0.66913060635532,0.74314482548058,-2.74058991357447E-12));
#135211=DIRECTION('center_axis',(0.643556859036948,-0.579501624401494,-0.500012436347864));
#135212=DIRECTION('ref_axis',(-0.372243731486086,0.33383798685376,-0.866017784403267));
#135213=DIRECTION('center_axis',(-0.371576145565853,0.334568664232079,0.86602250372631));
#135214=DIRECTION('ref_axis',(-0.918982183096512,-4.36450986441448E-16,
-0.39429905801456));
#135215=DIRECTION('center_axis',(-0.743144825477406,0.669130606358845,4.1231776140316E-14));
#135216=DIRECTION('ref_axis',(0.669130606358845,0.743144825477406,6.82961998416065E-15));
#135217=DIRECTION('center_axis',(0.743144825477398,-0.669130606358854,-4.56786669500649E-15));
#135218=DIRECTION('ref_axis',(-0.669130606358854,-0.743144825477398,-6.82961998416066E-15));
#135219=DIRECTION('center_axis',(0.743144825477406,-0.669130606358845,-4.6725140507014E-15));
#135220=DIRECTION('ref_axis',(-0.669130606358845,-0.743144825477406,-6.82961998416065E-15));
#135221=DIRECTION('center_axis',(0.743144825477398,-0.669130606358854,-4.56786669500649E-15));
#135222=DIRECTION('ref_axis',(-0.669130606358854,-0.743144825477398,-6.82961998416066E-15));
#135223=DIRECTION('center_axis',(-0.743144825477382,0.669130606358872,4.67251405070159E-15));
#135224=DIRECTION('ref_axis',(0.669130606358872,0.743144825477382,6.82961998416048E-15));
#135225=DIRECTION('center_axis',(0.393810436983641,-0.354588510146763,0.848045003637574));
#135226=DIRECTION('ref_axis',(-0.906978223357763,-4.0628693106624E-15,0.421177518814569));
#135227=DIRECTION('center_axis',(-0.371576246276136,0.334568754912025,-0.866022425483286));
#135228=DIRECTION('ref_axis',(0.918982131463637,2.78402616629794E-15,-0.394299178353887));
#135229=DIRECTION('center_axis',(-0.393810430455843,0.354588475160546,-0.848045021297515));
#135230=DIRECTION('ref_axis',(-0.63309803750285,0.564245025059696,0.529919264233169));
#135231=DIRECTION('center_axis',(0.393810395274834,-0.354588472591985,0.848045038708654));
#135232=DIRECTION('ref_axis',(-0.906978247051301,-4.04367791047371E-15,
0.42117746779208));
#135233=DIRECTION('center_axis',(-0.371576263602274,0.334568756370825,-0.866022417485744));
#135234=DIRECTION('ref_axis',(-0.646617000432134,0.576095872882387,0.500000000000031));
#135235=DIRECTION('center_axis',(-0.643568108591837,0.57951769513197,-0.499979330205214));
#135236=DIRECTION('ref_axis',(-0.370911831402169,0.335267672835389,0.866036951219422));
#135237=DIRECTION('center_axis',(-0.668950377172403,-0.743307065001336,
-5.19048549296485E-15));
#135238=DIRECTION('ref_axis',(-0.743307065001336,0.668950377172402,3.41480999208038E-15));
#135239=DIRECTION('center_axis',(0.743144825477398,-0.669130606358854,-4.56786669500649E-15));
#135240=DIRECTION('ref_axis',(-0.669130606358854,-0.743144825477398,-6.82961998416066E-15));
#135241=DIRECTION('center_axis',(-0.743144825477382,0.669130606358872,4.67251405070159E-15));
#135242=DIRECTION('ref_axis',(0.669130606358872,0.743144825477382,6.82961998416048E-15));
#135243=DIRECTION('center_axis',(-2.4546426258488E-16,-6.88873777539344E-15,
1.));
#135244=DIRECTION('ref_axis',(-1.,1.60344088833289E-30,-2.46820266164289E-16));
#135245=DIRECTION('center_axis',(-0.669310796197597,-0.742982542253409,
-5.18821936272801E-15));
#135246=DIRECTION('ref_axis',(-0.742982542253409,0.669310796197597,3.41480999208022E-15));
#135247=DIRECTION('center_axis',(-0.393810781475716,0.354588820328864,0.848044713969299));
#135248=DIRECTION('ref_axis',(-0.906978027661834,-3.05546561312248E-15,
-0.421177940232689));
#135249=DIRECTION('center_axis',(-0.393810395274935,0.354588472592013,-0.848045038708595));
#135250=DIRECTION('ref_axis',(0.906978247051249,3.61387669870221E-15,-0.421177467792193));
#135251=DIRECTION('center_axis',(-0.393810788844785,0.354588860886062,0.848044693589302));
#135252=DIRECTION('ref_axis',(0.633246889663017,-0.56407796458175,0.52991926423317));
#135253=DIRECTION('center_axis',(-0.393810830024481,0.354588864042376,0.848044673146743));
#135254=DIRECTION('ref_axis',(-0.906978000082666,2.6591822289014E-15,-0.421177999622544));
#135255=DIRECTION('center_axis',(0.393810430615192,-0.354588475220231,0.848045021198562));
#135256=DIRECTION('ref_axis',(-0.627330796754254,0.570650194811281,0.529919264233261));
#135257=DIRECTION('center_axis',(-0.393810436983659,0.35458851014678,-0.848045003637558));
#135258=DIRECTION('ref_axis',(0.906978223357751,-2.42657603144517E-15,-0.421177518814594));
#135259=DIRECTION('center_axis',(-0.668938718831589,-0.743317556935091,
-5.19055875774668E-15));
#135260=DIRECTION('ref_axis',(-0.743317556935091,0.668938718831589,3.41480999208028E-15));
#135261=DIRECTION('center_axis',(-0.743144825477406,0.669130606358845,4.6725140507014E-15));
#135262=DIRECTION('ref_axis',(0.669130606358845,0.743144825477406,6.82961998416065E-15));
#135263=DIRECTION('center_axis',(-2.4546426258488E-16,-6.88873777539344E-15,
1.));
#135264=DIRECTION('ref_axis',(-1.,1.70692667996567E-30,-2.477357166746E-16));
#135265=DIRECTION('center_axis',(-0.669322449283883,-0.742972044483925,
-5.18814605719551E-15));
#135266=DIRECTION('ref_axis',(-0.742972044483925,0.669322449283883,3.41480999208044E-15));
#135267=DIRECTION('center_axis',(-0.743144825477398,0.669130606358854,4.56786669500649E-15));
#135268=DIRECTION('ref_axis',(0.669130606358854,0.743144825477398,6.82961998416059E-15));
#135269=DIRECTION('center_axis',(-0.643597063368553,0.579456972966944,0.500012436348699));
#135270=DIRECTION('ref_axis',(0.370919252626752,-0.335308969651789,0.866017784402761));
#135271=DIRECTION('center_axis',(0.393810830024549,-0.354588864042312,-0.848044673146739));
#135272=DIRECTION('ref_axis',(0.906978000082638,1.23065481155338E-15,0.421177999622604));
#135273=DIRECTION('center_axis',(0.371576128830121,-0.334568662770661,-0.86602251147154));
#135274=DIRECTION('ref_axis',(0.64057839653263,-0.582802983773845,0.499999999999988));
#135275=DIRECTION('center_axis',(-0.371576145565821,0.33456866423205,0.866022503726335));
#135276=DIRECTION('ref_axis',(-0.918982183096528,1.60618320049483E-15,-0.394299058014522));
#135277=DIRECTION('center_axis',(0.393810788644162,-0.354588860818729,-0.84804469371062));
#135278=DIRECTION('ref_axis',(0.627180210740024,-0.570815694117288,0.529919264233239));
#135279=DIRECTION('center_axis',(0.39381078147571,-0.354588820328811,-0.848044713969325));
#135280=DIRECTION('ref_axis',(0.906978027661841,2.25474419065798E-15,0.421177940232673));
#135281=DIRECTION('center_axis',(-0.743144825477406,0.669130606358845,4.6725140507014E-15));
#135282=DIRECTION('ref_axis',(0.669130606358845,0.743144825477406,6.82961998416065E-15));
#135283=DIRECTION('center_axis',(0.743144825477406,-0.669130606358845,-4.6725140507014E-15));
#135284=DIRECTION('ref_axis',(-0.669130606358845,-0.743144825477406,-6.82961998416065E-15));
#135285=DIRECTION('center_axis',(-0.743144825477398,0.669130606358854,4.56786669500649E-15));
#135286=DIRECTION('ref_axis',(0.669130606358854,0.743144825477398,6.82961998416059E-15));
#135287=DIRECTION('center_axis',(-0.743144825477406,0.669130606358845,4.6725140507014E-15));
#135288=DIRECTION('ref_axis',(0.669130606358845,0.743144825477406,6.82961998416065E-15));
#135289=DIRECTION('center_axis',(-0.743144825477398,0.669130606358854,4.56786669500649E-15));
#135290=DIRECTION('ref_axis',(0.669130606358854,0.743144825477398,6.82961998416059E-15));
#135291=DIRECTION('center_axis',(0.643614221961007,-0.579466481046877,0.499979330205437));
#135292=DIRECTION('ref_axis',(0.372201885211874,-0.333834922929833,-0.866036951219265));
#135293=DIRECTION('center_axis',(-0.371576246276125,0.334568754912027,-0.86602242548329));
#135294=DIRECTION('ref_axis',(0.918982131463642,2.65789370359083E-15,-0.394299178353875));
#135295=DIRECTION('center_axis',(-0.371576252946193,0.334568760917773,-0.866022420301237));
#135296=DIRECTION('ref_axis',(-0.669130606358731,-0.743144825477509,-8.30481788101122E-14));
#135297=DIRECTION('center_axis',(0.404512553891932,-0.293895573514563,-0.866022508721553));
#135298=DIRECTION('ref_axis',(0.587785252287783,0.809016994378355,-3.36126577915125E-12));
#135299=DIRECTION('center_axis',(0.700605801485285,-0.509057044368013,-0.500012436349802));
#135300=DIRECTION('ref_axis',(-0.405100113137893,0.293099122200829,-0.866017784402128));
#135301=DIRECTION('center_axis',(-0.404512560891477,0.2938955786,0.866022503726312));
#135302=DIRECTION('ref_axis',(-0.906035256115478,-1.80341242297892E-15,
-0.423202214875772));
#135303=DIRECTION('center_axis',(-0.80901699437495,0.58778525229247,4.10448247925272E-15));
#135304=DIRECTION('ref_axis',(0.58778525229247,0.80901699437495,6.82961998416043E-15));
#135305=DIRECTION('center_axis',(0.809016994374951,-0.587785252292469,-3.99055920848346E-15));
#135306=DIRECTION('ref_axis',(-0.587785252292469,-0.80901699437495,-6.82961998416066E-15));
#135307=DIRECTION('center_axis',(0.80901699437495,-0.58778525229247,-4.10448247925272E-15));
#135308=DIRECTION('ref_axis',(-0.58778525229247,-0.80901699437495,-6.82961998416043E-15));
#135309=DIRECTION('center_axis',(0.809016994374951,-0.587785252292469,-3.99055920848346E-15));
#135310=DIRECTION('ref_axis',(-0.587785252292469,-0.80901699437495,-6.82961998416066E-15));
#135311=DIRECTION('center_axis',(-0.809016994374976,0.587785252292434,4.10448247925247E-15));
#135312=DIRECTION('ref_axis',(0.587785252292434,0.809016994374976,6.82961998416065E-15));
#135313=DIRECTION('center_axis',(0.428717694262762,-0.3114816373903,0.84804500363759));
#135314=DIRECTION('ref_axis',(-0.892442058026271,-6.18994737741828E-16,
0.451162025292283));
#135315=DIRECTION('center_axis',(-0.404512670528675,0.293895658256107,-0.866022425483295));
#135316=DIRECTION('ref_axis',(0.906035197473498,-1.65240743153779E-15,-0.423202340422593));
#135317=DIRECTION('center_axis',(-0.428717684113514,0.311481603278345,-0.848045021297511));
#135318=DIRECTION('ref_axis',(-0.68860952557912,0.494977266827708,0.529919264233214));
#135319=DIRECTION('center_axis',(0.428717648856936,-0.311481604401036,0.848045038708639));
#135320=DIRECTION('ref_axis',(-0.892442084777727,-6.11447499249856E-16,
0.451161972375315));
#135321=DIRECTION('center_axis',(-0.404512687918747,0.293895657887068,-0.866022417485759));
#135322=DIRECTION('ref_axis',(-0.70329318114634,0.505350078018259,0.500000000000001));
#135323=DIRECTION('center_axis',(-0.700618669263931,0.50907185116259,-0.499979330205492));
#135324=DIRECTION('ref_axis',(-0.403924952200305,0.294660197707191,0.866036951219254));
#135325=DIRECTION('center_axis',(-0.587589051772227,-0.809159506053914,
-5.65033063106954E-15));
#135326=DIRECTION('ref_axis',(-0.809159506053914,0.587589051772227,3.41480999208049E-15));
#135327=DIRECTION('center_axis',(0.809016994374951,-0.587785252292469,-3.99055920848346E-15));
#135328=DIRECTION('ref_axis',(-0.587785252292469,-0.80901699437495,-6.82961998416066E-15));
#135329=DIRECTION('center_axis',(-0.80901699437495,0.58778525229247,4.10448247925272E-15));
#135330=DIRECTION('ref_axis',(0.58778525229247,0.80901699437495,6.82961998416043E-15));
#135331=DIRECTION('center_axis',(-2.54740177659163E-16,-6.90019257654294E-15,
1.));
#135332=DIRECTION('ref_axis',(-1.,2.00430111041611E-30,-2.53872273768983E-16));
#135333=DIRECTION('center_axis',(-0.587981418248456,-0.808874435122371,
-5.64833999139408E-15));
#135334=DIRECTION('ref_axis',(-0.808874435122371,0.587981418248456,3.41480999208034E-15));
#135335=DIRECTION('center_axis',(-0.428718069290576,0.311481909863944,0.8480447139693));
#135336=DIRECTION('ref_axis',(-0.892441837073374,1.48661188715482E-15,-0.451162462358185));
#135337=DIRECTION('center_axis',(-0.428717648856939,0.311481604401038,-0.848045038708637));
#135338=DIRECTION('ref_axis',(0.892442084777726,5.36066018208771E-16,-0.451161972375317));
#135339=DIRECTION('center_axis',(-0.428718080856456,0.311481949431746,0.848044693589292));
#135340=DIRECTION('ref_axis',(0.688740099742912,-0.494795562228176,0.529919264233172));
#135341=DIRECTION('center_axis',(-0.428718122142682,0.311481948263276,0.848044673146743));
#135342=DIRECTION('ref_axis',(-0.892441805934786,1.06689281669451E-15,-0.451162523953241));
#135343=DIRECTION('center_axis',(0.428717684276344,-0.311481603323609,0.84804502119857));
#135344=DIRECTION('ref_axis',(-0.683543400924064,0.501950189209757,0.529919264233197));
#135345=DIRECTION('center_axis',(-0.428717694262774,0.311481637390308,-0.84804500363758));
#135346=DIRECTION('ref_axis',(0.892442058026264,1.61640809885533E-15,-0.451162025292297));
#135347=DIRECTION('center_axis',(-0.587576360591347,-0.809168721883284,
-4.98609139731183E-14));
#135348=DIRECTION('ref_axis',(-0.809168721883284,0.587576360591347,3.41480999207922E-15));
#135349=DIRECTION('center_axis',(-0.80901699437495,0.58778525229247,-4.0097746579219E-14));
#135350=DIRECTION('ref_axis',(0.58778525229247,0.80901699437495,6.82961998416043E-15));
#135351=DIRECTION('center_axis',(-2.54740177659163E-16,-6.90019257654294E-15,
1.));
#135352=DIRECTION('ref_axis',(-1.,1.70692667996567E-30,-2.55242859604134E-16));
#135353=DIRECTION('center_axis',(-0.587994104813612,-0.80886521293998,6.41945027862958E-15));
#135354=DIRECTION('ref_axis',(-0.80886521293998,0.587994104813612,3.41480999208017E-15));
#135355=DIRECTION('center_axis',(-0.809016994374951,0.587785252292469,3.99055920848346E-15));
#135356=DIRECTION('ref_axis',(0.587785252292469,0.809016994374951,6.82961998416065E-15));
#135357=DIRECTION('center_axis',(-0.700641118228681,0.509008435041422,0.500012436349283));
#135358=DIRECTION('ref_axis',(0.403936649448406,-0.294700492587247,0.866017784402393));
#135359=DIRECTION('center_axis',(0.428718122142701,-0.311481948263281,-0.848044673146731));
#135360=DIRECTION('ref_axis',(0.892441805934775,3.97758164497583E-16,0.451162523953261));
#135361=DIRECTION('center_axis',(0.404512544092706,-0.293895578898575,-0.866022511471566));
#135362=DIRECTION('ref_axis',(0.697988741328929,-0.512651652663007,0.499999999999945));
#135363=DIRECTION('center_axis',(-0.404512560891434,0.293895578599976,0.86602250372634));
#135364=DIRECTION('ref_axis',(-0.906035256115501,1.10927932520561E-15,-0.423202214875725));
#135365=DIRECTION('center_axis',(0.428718080653436,-0.311481949380818,-0.848044693710632));
#135366=DIRECTION('ref_axis',(0.683410939228537,-0.502130522411571,0.529919264233195));
#135367=DIRECTION('center_axis',(0.42871806929053,-0.311481909863932,-0.848044713969327));
#135368=DIRECTION('ref_axis',(0.8924418370734,2.85180820314112E-15,0.451162462358134));
#135369=DIRECTION('center_axis',(-0.80901699437495,0.58778525229247,4.10448247925272E-15));
#135370=DIRECTION('ref_axis',(0.58778525229247,0.80901699437495,6.82961998416043E-15));
#135371=DIRECTION('center_axis',(0.809016994374976,-0.587785252292434,-4.10448247925247E-15));
#135372=DIRECTION('ref_axis',(-0.587785252292434,-0.809016994374976,-6.82961998416065E-15));
#135373=DIRECTION('center_axis',(-0.809016994374951,0.587785252292469,3.99055920848346E-15));
#135374=DIRECTION('ref_axis',(0.587785252292469,0.809016994374951,6.82961998416065E-15));
#135375=DIRECTION('center_axis',(-0.80901699437495,0.58778525229247,3.62192817228647E-14));
#135376=DIRECTION('ref_axis',(0.58778525229247,0.80901699437495,6.82961998416044E-15));
#135377=DIRECTION('center_axis',(-0.809016994374951,0.587785252292469,3.99055920848346E-15));
#135378=DIRECTION('ref_axis',(0.587785252292469,0.809016994374951,6.82961998416065E-15));
#135379=DIRECTION('center_axis',(0.700659176689191,-0.509016097474679,0.499979330205633));
#135380=DIRECTION('ref_axis',(0.405058175807095,-0.29310044922319,-0.866036951219169));
#135381=DIRECTION('center_axis',(-0.404512670528692,0.293895658256119,-0.866022425483283));
#135382=DIRECTION('ref_axis',(0.906035197473489,-1.02813875008142E-16,-0.423202340422611));
#135383=DIRECTION('center_axis',(-0.404512677788109,0.293895663530384,-0.866022420302574));
#135384=DIRECTION('ref_axis',(-0.587785252290296,-0.809016994376529,-1.56043157028568E-12));
#135385=DIRECTION('center_axis',(0.433017044463491,-0.250002507184682,-0.866022508717571));
#135386=DIRECTION('ref_axis',(0.500000000006304,0.866025403780799,4.21797331194789E-12));
#135387=DIRECTION('center_axis',(0.749978760165048,-0.433035128827861,-0.500012436347673));
#135388=DIRECTION('ref_axis',(-0.433518133167728,0.249149002229375,-0.866017784403343));
#135389=DIRECTION('center_axis',(-0.433017051950273,0.250002511507189,0.866022503726313));
#135390=DIRECTION('ref_axis',(-0.894424794863787,-3.51926008997178E-16,
-0.447218387740121));
#135391=DIRECTION('center_axis',(-0.86602540378444,0.499999999999998,6.44677165429795E-14));
#135392=DIRECTION('ref_axis',(0.499999999999998,0.86602540378444,6.82961998416156E-15));
#135393=DIRECTION('center_axis',(0.866025403784442,-0.499999999999995,-3.36953032019409E-15));
#135394=DIRECTION('ref_axis',(-0.499999999999995,-0.866025403784441,-6.82961998416066E-15));
#135395=DIRECTION('center_axis',(0.866025403784433,-0.50000000000001,-1.71507213071646E-14));
#135396=DIRECTION('ref_axis',(-0.50000000000001,-0.866025403784433,-6.82961998416068E-15));
#135397=DIRECTION('center_axis',(0.866025403784442,-0.499999999999995,-3.36953032019409E-15));
#135398=DIRECTION('ref_axis',(-0.499999999999995,-0.866025403784441,-6.82961998416066E-15));
#135399=DIRECTION('center_axis',(-0.86602540378444,0.499999999999998,3.49148133884312E-15));
#135400=DIRECTION('ref_axis',(0.499999999999998,0.86602540378444,6.82961998416073E-15));
#135401=DIRECTION('center_axis',(0.45892783076861,-0.264962106632881,0.848045003637592));
#135402=DIRECTION('ref_axis',(-0.87947860205334,1.19060858178351E-15,0.475938429348065));
#135403=DIRECTION('center_axis',(-0.43301716931323,0.250002579266689,-0.86602242548329));
#135404=DIRECTION('ref_axis',(0.894424730216411,1.60782206696907E-16,-0.447218517033116));
#135405=DIRECTION('center_axis',(-0.458927817107794,0.264962073771327,-0.848045021297498));
#135406=DIRECTION('ref_axis',(-0.736576463606657,0.420286434060449,0.529919264233207));
#135407=DIRECTION('center_axis',(0.45892778216319,-0.264962078570529,0.848045038708653));
#135408=DIRECTION('ref_axis',(-0.879478631391258,1.16952532199408E-15,0.475938375135017));
#135409=DIRECTION('center_axis',(-0.433017186567245,0.250002577085764,-0.866022417485751));
#135410=DIRECTION('ref_axis',(-0.752263934580233,0.42906756196414,0.500000000000016));
#135411=DIRECTION('center_axis',(-0.749993105181609,0.433048509462133,-0.499979330205433));
#135412=DIRECTION('ref_axis',(-0.432512586699257,0.250824363787739,0.866036951219285));
#135413=DIRECTION('center_axis',(-0.499789977759954,-0.866146626230631,
-6.04826956437238E-15));
#135414=DIRECTION('ref_axis',(-0.866146626230631,0.499789977759954,3.41480999208016E-15));
#135415=DIRECTION('center_axis',(0.866025403784442,-0.499999999999995,-3.36953032019409E-15));
#135416=DIRECTION('ref_axis',(-0.499999999999995,-0.866025403784441,-6.82961998416066E-15));
#135417=DIRECTION('center_axis',(-0.866025403784457,0.499999999999969,3.49148133884292E-15));
#135418=DIRECTION('ref_axis',(0.499999999999969,0.866025403784457,6.82961998416065E-15));
#135419=DIRECTION('center_axis',(-2.62767925538921E-16,-6.91255422424131E-15,
1.));
#135420=DIRECTION('ref_axis',(-1.,2.00430111041611E-30,-2.60924281373677E-16));
#135421=DIRECTION('center_axis',(-0.500209992837911,-0.865904130412309,
-6.04657622512354E-15));
#135422=DIRECTION('ref_axis',(-0.865904130412309,0.500209992837911,3.41480999208024E-15));
#135423=DIRECTION('center_axis',(-0.458928232223204,0.264962338412787,0.848044713969324));
#135424=DIRECTION('ref_axis',(-0.879478359737745,-9.91663607721953E-16,
-0.475938877118696));
#135425=DIRECTION('center_axis',(-0.45892778216322,0.264962078570537,-0.848045038708634));
#135426=DIRECTION('ref_axis',(0.879478631391241,1.07865946136944E-15,-0.475938375135048));
#135427=DIRECTION('center_axis',(-0.458928247863733,0.264962376551373,0.848044693589302));
#135428=DIRECTION('ref_axis',(0.736687329152564,-0.420092076169725,0.529919264233214));
#135429=DIRECTION('center_axis',(-0.458928288799617,0.264962371077277,0.848044673146741));
#135430=DIRECTION('ref_axis',(-0.879478325588526,2.57091442443615E-15,-0.475938940222381));
#135431=DIRECTION('center_axis',(0.458927817277461,-0.264962073794094,0.848045021198568));
#135432=DIRECTION('ref_axis',(-0.732266960570914,0.427750712273813,0.529919264233224));
#135433=DIRECTION('center_axis',(-0.458927830768617,0.264962106632877,-0.84804500363759));
#135434=DIRECTION('ref_axis',(0.879478602053337,-8.27701491930472E-16,-0.475938429348071));
#135435=DIRECTION('center_axis',(-0.499776392786171,-0.866154464985111,
-6.04832430210234E-15));
#135436=DIRECTION('ref_axis',(-0.86615446498511,0.499776392786171,3.41480999208032E-15));
#135437=DIRECTION('center_axis',(-0.866025403784433,0.50000000000001,1.71507213071653E-14));
#135438=DIRECTION('ref_axis',(0.50000000000001,0.866025403784433,6.82961998416068E-15));
#135439=DIRECTION('center_axis',(-2.62767925538921E-16,-6.91255422424131E-15,
1.));
#135440=DIRECTION('ref_axis',(-1.,1.70692667996567E-30,-2.62750002533667E-16));
#135441=DIRECTION('center_axis',(-0.500223573885299,-0.865896284857153,
-9.72224648886353E-15));
#135442=DIRECTION('ref_axis',(-0.865896284857153,0.500223573885299,3.41480999208028E-15));
#135443=DIRECTION('center_axis',(-0.866025403784442,0.499999999999995,3.36953032019409E-15));
#135444=DIRECTION('ref_axis',(0.499999999999995,0.866025403784442,6.82961998416074E-15));
#135445=DIRECTION('center_axis',(-0.750008802378862,0.432983094186076,0.500012436348614));
#135446=DIRECTION('ref_axis',(0.432528431874663,-0.250863215155224,0.866017784402854));
#135447=DIRECTION('center_axis',(0.458928288799688,-0.264962371077173,-0.848044673146735));
#135448=DIRECTION('ref_axis',(0.879478325588494,1.64057136930641E-15,0.475938940222439));
#135449=DIRECTION('center_axis',(0.433017035275494,-0.250002513558742,-0.866022511471574));
#135450=DIRECTION('ref_axis',(0.74775177542025,-0.436883602754709,0.499999999999929));
#135451=DIRECTION('center_axis',(-0.43301705195022,0.250002511507158,0.866022503726349));
#135452=DIRECTION('ref_axis',(-0.894424794863815,2.91747672552896E-15,-0.447218387740063));
#135453=DIRECTION('center_axis',(0.458928247653565,-0.264962376527061,-0.848044693710632));
#135454=DIRECTION('ref_axis',(0.732154074456122,-0.427943903627455,0.529919264233141));
#135455=DIRECTION('center_axis',(0.458928232223194,-0.264962338412781,-0.848044713969331));
#135456=DIRECTION('ref_axis',(0.879478359737751,1.00929923944428E-16,0.475938877118685));
#135457=DIRECTION('center_axis',(-0.866025403784433,0.50000000000001,3.4914813388432E-15));
#135458=DIRECTION('ref_axis',(0.50000000000001,0.866025403784433,6.82961998416068E-15));
#135459=DIRECTION('center_axis',(0.866025403784433,-0.50000000000001,-3.4914813388432E-15));
#135460=DIRECTION('ref_axis',(-0.50000000000001,-0.866025403784433,-6.82961998416068E-15));
#135461=DIRECTION('center_axis',(-0.866025403784442,0.499999999999995,3.36953032019409E-15));
#135462=DIRECTION('ref_axis',(0.499999999999995,0.866025403784442,6.82961998416074E-15));
#135463=DIRECTION('center_axis',(-0.866025403784433,0.50000000000001,3.4914813388432E-15));
#135464=DIRECTION('ref_axis',(0.50000000000001,0.866025403784433,6.82961998416068E-15));
#135465=DIRECTION('center_axis',(-0.866025403784442,0.499999999999995,3.36953032019409E-15));
#135466=DIRECTION('ref_axis',(0.499999999999995,0.866025403784442,6.82961998416074E-15));
#135467=DIRECTION('center_axis',(0.75002756285576,-0.432988827019632,0.499979330205573));
#135468=DIRECTION('ref_axis',(0.433476564276502,-0.249154705646875,-0.866036951219207));
#135469=DIRECTION('center_axis',(-0.433017169313196,0.250002579266716,-0.866022425483299));
#135470=DIRECTION('ref_axis',(0.894424730216427,-1.69509643524011E-15,-0.447218517033086));
#135471=DIRECTION('center_axis',(-0.433017177085375,0.250002583753999,-0.866022420301771));
#135472=DIRECTION('ref_axis',(-0.500000000003883,-0.866025403782197,2.5744935431098E-12));
#135473=DIRECTION('center_axis',(0.456777309669419,-0.203370361062852,-0.86602250872153));
#135474=DIRECTION('ref_axis',(0.406736643074989,0.913545457642962,-4.89547161595317E-13));
#135475=DIRECTION('center_axis',(0.791134794600545,-0.352268789801452,-0.500012436349511));
#135476=DIRECTION('ref_axis',(0.457186437800744,-0.202469153675368,0.866017784402287));
#135477=DIRECTION('center_axis',(-0.456777317573304,0.203370364581841,0.86602250372631));
#135478=DIRECTION('ref_axis',(-0.884507036382085,2.80052133003465E-16,-0.466526850878468));
#135479=DIRECTION('center_axis',(-0.913545457642594,0.406736643075817,2.84022679824583E-15));
#135480=DIRECTION('ref_axis',(0.406736643075817,0.913545457642593,6.82961998416057E-15));
#135481=DIRECTION('center_axis',(0.913545457642603,-0.406736643075795,-2.71158415259712E-15));
#135482=DIRECTION('ref_axis',(-0.406736643075795,-0.913545457642603,-6.82961998416066E-15));
#135483=DIRECTION('center_axis',(0.913545457642598,-0.406736643075807,-2.84022679824576E-15));
#135484=DIRECTION('ref_axis',(-0.406736643075807,-0.913545457642598,-6.8296199841606E-15));
#135485=DIRECTION('center_axis',(0.913545457642603,-0.406736643075795,-2.71158415259712E-15));
#135486=DIRECTION('ref_axis',(-0.406736643075795,-0.913545457642603,-6.82961998416066E-15));
#135487=DIRECTION('center_axis',(-0.913545457642603,0.406736643075797,2.84022679824569E-15));
#135488=DIRECTION('ref_axis',(0.406736643075797,0.913545457642603,6.82961998416064E-15));
#135489=DIRECTION('center_axis',(0.484109857923767,-0.215539595588311,0.848045003637577));
#135490=DIRECTION('ref_axis',(-0.868458021515997,-9.89659158812798E-17,
0.495762710240011));
#135491=DIRECTION('center_axis',(-0.456777441376074,0.203370419702476,-0.866022425483293));
#135492=DIRECTION('ref_axis',(0.884506966812058,1.8236239182919E-15,-0.466526982779059));
#135493=DIRECTION('center_axis',(-0.484109840902953,0.215539564334311,-0.84804502129751));
#135494=DIRECTION('ref_axis',(-0.776473315754038,0.340990855180143,0.529919264233189));
#135495=DIRECTION('center_axis',(0.484109806651284,-0.215539572760331,0.848045038708647));
#135496=DIRECTION('ref_axis',(-0.868458052949959,4.03183191579828E-16,0.495762655175201));
#135497=DIRECTION('center_axis',(-0.456777458307734,0.203370415729553,-0.86602241748578));
#135498=DIRECTION('ref_axis',(-0.792992726925484,0.34808409191359,0.499999999999977));
#135499=DIRECTION('center_axis',(-0.791150459692779,0.352280597670813,-0.499979330205359));
#135500=DIRECTION('ref_axis',(0.456361522796281,-0.204240445636448,-0.866036951219337));
#135501=DIRECTION('center_axis',(-0.406515100163568,-0.913644062717536,
-6.3799423906462E-15));
#135502=DIRECTION('ref_axis',(-0.913644062717536,0.406515100163568,3.41480999208032E-15));
#135503=DIRECTION('center_axis',(0.913545457642603,-0.406736643075795,-2.71158415259712E-15));
#135504=DIRECTION('ref_axis',(-0.406736643075795,-0.913545457642603,-6.82961998416066E-15));
#135505=DIRECTION('center_axis',(-0.913545457642603,0.406736643075797,2.84022679824569E-15));
#135506=DIRECTION('ref_axis',(0.406736643075797,0.913545457642603,6.82961998416064E-15));
#135507=DIRECTION('center_axis',(-2.6945955253847E-16,-6.92568728168955E-15,
1.));
#135508=DIRECTION('ref_axis',(-1.,2.00430111041611E-30,-2.67976288978371E-16));
#135509=DIRECTION('center_axis',(-0.406958162070199,-0.913446798847336,
-6.37856490440294E-15));
#135510=DIRECTION('ref_axis',(-0.913446798847336,0.406958162070199,3.4148099920803E-15));
#135511=DIRECTION('center_axis',(-0.484110281406756,0.21553978413508,0.848044713969301));
#135512=DIRECTION('ref_axis',(-0.868457761888264,-2.62723474582901E-16,
-0.495763165045597));
#135513=DIRECTION('center_axis',(-0.484109806651301,0.215539572760338,-0.848045038708636));
#135514=DIRECTION('ref_axis',(0.868458052949949,2.96622001727381E-16,-0.495762655175219));
#135515=DIRECTION('center_axis',(-0.48411030094316,0.2155398204412,0.848044693589258));
#135516=DIRECTION('ref_axis',(0.776563258046704,-0.340785973371052,0.529919264233178));
#135517=DIRECTION('center_axis',(-0.484110341087582,0.215539810706753,0.848044673146741));
#135518=DIRECTION('ref_axis',(-0.868457725299283,2.05000090583624E-15,-0.495763229140681));
#135519=DIRECTION('center_axis',(0.484109841073579,-0.215539564340363,0.848045021198569));
#135520=DIRECTION('ref_axis',(-0.772967650155533,0.348864709031412,0.529919264233206));
#135521=DIRECTION('center_axis',(-0.484109857923745,0.215539595588301,-0.848045003637592));
#135522=DIRECTION('ref_axis',(0.86845802151601,-1.31527569561181E-15,-0.495762710239987));
#135523=DIRECTION('center_axis',(-0.406500770236713,-0.913650438514074,
-6.37998691259547E-15));
#135524=DIRECTION('ref_axis',(-0.913650438514073,0.406500770236713,3.41480999208024E-15));
#135525=DIRECTION('center_axis',(-0.913545457642598,0.406736643075807,2.84022679824576E-15));
#135526=DIRECTION('ref_axis',(0.406736643075807,0.913545457642598,6.82961998416061E-15));
#135527=DIRECTION('center_axis',(-2.6945955253847E-16,-6.92568728168955E-15,
1.));
#135528=DIRECTION('ref_axis',(-1.,2.13365834995709E-30,-2.70257145463201E-16));
#135529=DIRECTION('center_axis',(-0.406972488803014,-0.913440415876964,
-6.37852033235906E-15));
#135530=DIRECTION('ref_axis',(-0.913440415876964,0.406972488803014,3.41480999208024E-15));
#135531=DIRECTION('center_axis',(-0.913545457642603,0.406736643075795,2.71158415259712E-15));
#135532=DIRECTION('ref_axis',(0.406736643075795,0.913545457642603,6.82961998416064E-15));
#135533=DIRECTION('center_axis',(-0.791159233140825,0.352213899939985,0.500012436350425));
#135534=DIRECTION('ref_axis',(0.456381342217505,-0.204277427964079,0.866017784401757));
#135535=DIRECTION('center_axis',(0.484110341087604,-0.215539810706705,-0.84804467314674));
#135536=DIRECTION('ref_axis',(0.868457725299273,-1.11516049819258E-15,0.495763229140698));
#135537=DIRECTION('center_axis',(0.456777301206547,-0.203370368360254,-0.866022511471542));
#135538=DIRECTION('ref_axis',(0.7893222845842,-0.356328964664343,0.500000000000017));
#135539=DIRECTION('center_axis',(-0.456777317573169,0.20337036458186,0.866022503726376));
#135540=DIRECTION('ref_axis',(-0.884507036382157,1.69032347061982E-15,-0.466526850878333));
#135541=DIRECTION('center_axis',(0.484110300737792,-0.215539820425012,-0.848044693710607));
#135542=DIRECTION('ref_axis',(0.772875576442627,-0.349068641864353,0.529919264233197));
#135543=DIRECTION('center_axis',(0.484110281406739,-0.215539784135015,-0.848044713969328));
#135544=DIRECTION('ref_axis',(0.868457761888278,-1.33747047041045E-15,0.495763165045573));
#135545=DIRECTION('center_axis',(-0.913545457642598,0.406736643075807,2.84022679824576E-15));
#135546=DIRECTION('ref_axis',(0.406736643075807,0.913545457642598,6.82961998416061E-15));
#135547=DIRECTION('center_axis',(0.913545457642598,-0.406736643075807,-2.84022679824576E-15));
#135548=DIRECTION('ref_axis',(-0.406736643075807,-0.913545457642598,-6.8296199841606E-15));
#135549=DIRECTION('center_axis',(-0.913545457642603,0.406736643075795,2.71158415259712E-15));
#135550=DIRECTION('ref_axis',(0.406736643075795,0.913545457642603,6.82961998416064E-15));
#135551=DIRECTION('center_axis',(-0.913545457642598,0.406736643075807,-8.27120002511786E-15));
#135552=DIRECTION('ref_axis',(0.406736643075807,0.913545457642598,6.8296199841606E-15));
#135553=DIRECTION('center_axis',(-0.913545457642603,0.406736643075795,2.71158415259712E-15));
#135554=DIRECTION('ref_axis',(0.406736643075795,0.913545457642603,6.82961998416064E-15));
#135555=DIRECTION('center_axis',(0.791178490090583,-0.352217640366738,0.499979330205232));
#135556=DIRECTION('ref_axis',(0.457145692799107,-0.202479170972784,-0.866036951219403));
#135557=DIRECTION('center_axis',(-0.456777441376052,0.203370419702467,-0.866022425483307));
#135558=DIRECTION('ref_axis',(0.88450696681207,8.66756486764032E-16,-0.466526982779037));
#135559=DIRECTION('center_axis',(-0.456777449573532,0.203370423352227,-0.866022420302521));
#135560=DIRECTION('ref_axis',(-0.406736643075106,-0.91354545764291,-4.45837591507382E-13));
#135561=DIRECTION('center_axis',(0.475533027095179,-0.15451004671247,-0.866022508718224));
#135562=DIRECTION('ref_axis',(0.309016994378645,0.951056516293952,2.26852657916475E-12));
#135563=DIRECTION('center_axis',(0.82362299067401,-0.267642920194133,-0.500012436348495));
#135564=DIRECTION('ref_axis',(0.475845712146801,-0.153571010706525,0.866017784402884));
#135565=DIRECTION('center_axis',(-0.475533035318161,0.154510049384242,0.866022503726304));
#135566=DIRECTION('ref_axis',(-0.876548788012425,1.94488523957394E-15,-0.481313018974086));
#135567=DIRECTION('center_axis',(-0.951056516295146,0.309016994374972,2.15785413849121E-15));
#135568=DIRECTION('ref_axis',(0.309016994374972,0.951056516295146,6.82961998416073E-15));
#135569=DIRECTION('center_axis',(0.951056516295156,-0.309016994374942,-2.02392930158883E-15));
#135570=DIRECTION('ref_axis',(-0.309016994374942,-0.951056516295155,-6.82961998416066E-15));
#135571=DIRECTION('center_axis',(0.951056516295148,-0.309016994374964,1.47258949833367E-14));
#135572=DIRECTION('ref_axis',(-0.309016994374964,-0.951056516295148,-6.82961998416061E-15));
#135573=DIRECTION('center_axis',(0.951056516295156,-0.309016994374942,-2.02392930158883E-15));
#135574=DIRECTION('ref_axis',(-0.309016994374942,-0.951056516295155,-6.82961998416066E-15));
#135575=DIRECTION('center_axis',(-0.951056516295146,0.309016994374972,2.15785413849121E-15));
#135576=DIRECTION('ref_axis',(0.309016994374972,0.951056516295146,6.82961998416073E-15));
#135577=DIRECTION('center_axis',(0.503987876168977,-0.163755587629907,0.848045003637583));
#135578=DIRECTION('ref_axis',(-0.859649462041492,4.39826809004255E-16,0.510884333691857));
#135579=DIRECTION('center_axis',(-0.475533164204401,0.154510091261986,-0.866022425483291));
#135580=DIRECTION('ref_axis',(0.876548714628841,4.29963435206314E-16,-0.481313152617427));
#135581=DIRECTION('center_axis',(-0.503987855972783,0.163755558331625,-0.848045021297487));
#135582=DIRECTION('ref_axis',(-0.807862963765476,0.257959309137282,0.529919264233221));
#135583=DIRECTION('center_axis',(0.503987822791196,-0.163755570286415,0.848045038708653));
#135584=DIRECTION('ref_axis',(-0.859649495083707,2.20200626090829E-15,0.510884278092727));
#135585=DIRECTION('center_axis',(-0.475533180627341,0.154510085543092,-0.866022417485778));
#135586=DIRECTION('ref_axis',(-0.825033325010143,0.263286939711698,0.499999999999955));
#135587=DIRECTION('center_axis',(-0.823639804208689,0.267653025932082,-0.499979330205232));
#135588=DIRECTION('ref_axis',(0.475210466541726,-0.155418826439376,-0.866036951219405));
#135589=DIRECTION('center_axis',(-0.308786358060986,-0.951131423661017,
-6.64171523299948E-15));
#135590=DIRECTION('ref_axis',(-0.951131423661017,0.308786358060986,3.41480999208039E-15));
#135591=DIRECTION('center_axis',(0.951056516295156,-0.309016994374942,-2.02392930158883E-15));
#135592=DIRECTION('ref_axis',(-0.309016994374942,-0.951056516295155,-6.82961998416066E-15));
#135593=DIRECTION('center_axis',(-0.951056516295162,0.309016994374922,2.15785413849087E-15));
#135594=DIRECTION('ref_axis',(0.309016994374922,0.951056516295162,6.82961998416065E-15));
#135595=DIRECTION('center_axis',(-2.74741743792088E-16,-6.93944786036197E-15,
1.));
#135596=DIRECTION('ref_axis',(-1.,2.00430111041611E-30,-2.75028296583065E-16));
#135597=DIRECTION('center_axis',(-0.309247612517378,-0.95098155300316,-6.64066869178919E-15));
#135598=DIRECTION('ref_axis',(-0.95098155300316,0.309247612517378,3.41480999208029E-15));
#135599=DIRECTION('center_axis',(-0.503988317040574,0.163755730877717,0.848044713969325));
#135600=DIRECTION('ref_axis',(-0.859649189130472,-2.17897991428701E-16,
-0.510884792910615));
#135601=DIRECTION('center_axis',(-0.503987822791213,0.16375557028642,-0.848045038708642));
#135602=DIRECTION('ref_axis',(0.859649495083697,-1.26799831889259E-15,-0.510884278092745));
#135603=DIRECTION('center_axis',(-0.503988340268016,0.163755764933399,0.848044693589299));
#135604=DIRECTION('ref_axis',(0.807930997358871,-0.257746148179274,0.529919264233193));
#135605=DIRECTION('center_axis',(-0.503988379172003,0.163755751065505,0.848044673146734));
#135606=DIRECTION('ref_axis',(-0.859649150669465,2.12951299205037E-15,-0.510884857627693));
#135607=DIRECTION('center_axis',(0.503987856146397,-0.163755558309613,0.84804502119856));
#135608=DIRECTION('ref_axis',(-0.80519954441769,0.26615647101673,0.529919264233209));
#135609=DIRECTION('center_axis',(-0.503987876169011,0.163755587629918,-0.84804500363756));
#135610=DIRECTION('ref_axis',(0.859649462041471,1.57485748646909E-15,-0.510884333691893));
#135611=DIRECTION('center_axis',(-0.308771440182777,-0.951136266645034,
-6.64174905137613E-15));
#135612=DIRECTION('ref_axis',(-0.951136266645034,0.308771440182777,3.41480999208035E-15));
#135613=DIRECTION('center_axis',(-0.951056516295148,0.309016994374964,-4.98049825795553E-14));
#135614=DIRECTION('ref_axis',(0.309016994374964,0.951056516295148,6.82961998416031E-15));
#135615=DIRECTION('center_axis',(-2.74741743792088E-16,-6.93944786036197E-15,
1.));
#135616=DIRECTION('ref_axis',(-1.,2.13365834995709E-30,-2.77764288392734E-16));
#135617=DIRECTION('center_axis',(-0.309262527968948,-0.950976702550728,
2.44143881663588E-15));
#135618=DIRECTION('ref_axis',(-0.950976702550728,0.309262527968948,3.41480999208024E-15));
#135619=DIRECTION('center_axis',(-0.951056516295156,0.309016994374942,2.02392930158883E-15));
#135620=DIRECTION('ref_axis',(0.309016994374942,0.951056516295156,6.8296199841606E-15));
#135621=DIRECTION('center_axis',(-0.823641557783644,0.267585776504662,0.500012436349466));
#135622=DIRECTION('ref_axis',(0.475234043100657,-0.155453534463189,0.866017784402321));
#135623=DIRECTION('center_axis',(0.503988379172001,-0.163755751065456,-0.848044673146744));
#135624=DIRECTION('ref_axis',(0.859649150669468,-2.26336925852521E-15,0.510884857627687));
#135625=DIRECTION('center_axis',(0.475533019434099,-0.154510054858537,-0.866022511471556));
#135626=DIRECTION('ref_axis',(0.822244813610406,-0.271870311896699,0.499999999999979));
#135627=DIRECTION('center_axis',(-0.475533035318099,0.154510049384272,0.866022503726332));
#135628=DIRECTION('ref_axis',(-0.876548788012458,8.76596332424742E-17,-0.481313018974026));
#135629=DIRECTION('center_axis',(0.503988340058683,-0.163755764949449,-0.848044693710605));
#135630=DIRECTION('ref_axis',(0.805129291878303,-0.266368911012672,0.529919264233209));
#135631=DIRECTION('center_axis',(0.503988317040564,-0.163755730877724,-0.84804471396933));
#135632=DIRECTION('ref_axis',(0.859649189130478,-1.64241712406884E-16,0.510884792910606));
#135633=DIRECTION('center_axis',(-0.951056516295148,0.309016994374964,-4.98049825795553E-14));
#135634=DIRECTION('ref_axis',(0.309016994374964,0.951056516295148,6.82961998416031E-15));
#135635=DIRECTION('center_axis',(0.951056516295165,-0.309016994374914,-2.15785413849081E-15));
#135636=DIRECTION('ref_axis',(-0.309016994374914,-0.951056516295164,-6.82961998416067E-15));
#135637=DIRECTION('center_axis',(-0.951056516295156,0.309016994374942,2.02392930158883E-15));
#135638=DIRECTION('ref_axis',(0.309016994374942,0.951056516295156,6.8296199841606E-15));
#135639=DIRECTION('center_axis',(-0.951056516295148,0.309016994374964,-4.98049825795525E-14));
#135640=DIRECTION('ref_axis',(0.309016994374964,0.951056516295148,6.82961998416031E-15));
#135641=DIRECTION('center_axis',(-0.951056516295156,0.309016994374942,2.02392930158883E-15));
#135642=DIRECTION('ref_axis',(0.309016994374942,0.951056516295156,6.8296199841606E-15));
#135643=DIRECTION('center_axis',(0.823661100222817,-0.267587483540044,0.499979330205204));
#135644=DIRECTION('ref_axis',(0.475806237451048,-0.153585232119715,-0.86603695121941));
#135645=DIRECTION('center_axis',(-0.475533164204424,0.154510091261989,-0.866022425483278));
#135646=DIRECTION('ref_axis',(0.876548714628828,1.33063653772379E-15,-0.48131315261745));
#135647=DIRECTION('center_axis',(-0.475533172741877,0.154510094035947,-0.866022420300449));
#135648=DIRECTION('ref_axis',(-0.309016994382379,-0.951056516292739,4.51956930993777E-12));
#135649=DIRECTION('center_axis',(0.489078705150955,-0.103956887952906,-0.866022508723077));
#135650=DIRECTION('ref_axis',(0.207911690818348,0.978147600733681,3.58418457596544E-13));
#135651=DIRECTION('center_axis',(0.847087400906921,-0.180084698747046,-0.50001243634728));
#135652=DIRECTION('ref_axis',(0.489291521297257,-0.102990311599294,0.866017784403586));
#135653=DIRECTION('center_axis',(-0.48907871361637,0.103956889752263,0.866022503726313));
#135654=DIRECTION('ref_axis',(-0.870740345484703,9.01293367321942E-17,-0.491743073916837));
#135655=DIRECTION('center_axis',(-0.978147600733807,0.207911690817751,1.45183957723501E-15));
#135656=DIRECTION('ref_axis',(0.207911690817752,0.978147600733807,6.82961998416061E-15));
#135657=DIRECTION('center_axis',(0.978147600733807,-0.207911690817753,-1.3140998576179E-15));
#135658=DIRECTION('ref_axis',(-0.207911690817753,-0.978147600733807,-6.82961998416066E-15));
#135659=DIRECTION('center_axis',(0.978147600733806,-0.207911690817757,-4.29175525433417E-15));
#135660=DIRECTION('ref_axis',(-0.207911690817757,-0.978147600733806,-6.8296199841607E-15));
#135661=DIRECTION('center_axis',(0.978147600733807,-0.207911690817753,-1.3140998576179E-15));
#135662=DIRECTION('ref_axis',(-0.207911690817753,-0.978147600733807,-6.82961998416066E-15));
#135663=DIRECTION('center_axis',(-0.978147600733807,0.207911690817751,1.45183957723501E-15));
#135664=DIRECTION('ref_axis',(0.207911690817752,0.978147600733807,6.82961998416061E-15));
#135665=DIRECTION('center_axis',(0.518344097776653,-0.11017743918536,0.848045003637581));
#135666=DIRECTION('ref_axis',(-0.853239582811868,-1.49305978118172E-15,
0.521519140898039));
#135667=DIRECTION('center_axis',(-0.489078846173993,0.103956917928318,-0.86602242548329));
#135668=DIRECTION('ref_axis',(0.87074026939378,-1.88754034186863E-16,-0.491743208652694));
#135669=DIRECTION('center_axis',(-0.518344074628652,0.110177412158262,-0.848045021297499));
#135670=DIRECTION('ref_axis',(-0.830401496087922,0.172101506935423,0.52991926423324));
#135671=DIRECTION('center_axis',(0.518344042878396,-0.110177427516375,0.848045038708649));
#135672=DIRECTION('ref_axis',(-0.853239616987304,-4.00876318608133E-16,
0.521519084984776));
#135673=DIRECTION('center_axis',(-0.489078861910606,0.103956910517348,-0.86602241748578));
#135674=DIRECTION('ref_axis',(-0.848034685338871,0.175605160693646,0.499999999999961));
#135675=DIRECTION('center_axis',(-0.847105178671992,0.180092991630944,-0.499979330205268));
#135676=DIRECTION('ref_axis',(0.488852904975874,-0.104894406043765,-0.866036951219389));
#135677=DIRECTION('center_axis',(-0.207674488001825,-0.978197989689807,
6.5307210243107E-15));
#135678=DIRECTION('ref_axis',(-0.978197989689807,0.207674488001825,7.66186706172843E-29));
#135679=DIRECTION('center_axis',(0.978147600733807,-0.207911690817753,-1.3140998576179E-15));
#135680=DIRECTION('ref_axis',(-0.207911690817753,-0.978147600733807,-6.82961998416066E-15));
#135681=DIRECTION('center_axis',(-0.978147600733807,0.207911690817751,1.45183957723501E-15));
#135682=DIRECTION('ref_axis',(0.207911690817751,0.978147600733807,6.82961998416071E-15));
#135683=DIRECTION('center_axis',(-2.78556626507032E-16,-6.95368519647906E-15,
1.));
#135684=DIRECTION('ref_axis',(-1.,2.00430111041611E-30,-2.75028296583065E-16));
#135685=DIRECTION('center_axis',(-0.208148881407613,-0.978097154258594,
-6.83001592333891E-15));
#135686=DIRECTION('ref_axis',(-0.978097154258594,0.208148881407613,-1.2419109941013E-29));
#135687=DIRECTION('center_axis',(-0.518344551206596,0.110177535564887,0.848044713969305));
#135688=DIRECTION('ref_axis',(-0.853239300541031,5.99666814548819E-16,-0.521519602711396));
#135689=DIRECTION('center_axis',(-0.518344042878388,0.110177427516373,-0.848045038708654));
#135690=DIRECTION('ref_axis',(0.853239616987309,3.25739190337144E-16,-0.521519084984768));
#135691=DIRECTION('center_axis',(-0.518344577867247,0.1101775670028,0.8480446935893));
#135692=DIRECTION('ref_axis',(0.830446875603153,-0.171882402227476,0.529919264233216));
#135693=DIRECTION('center_axis',(-0.51834461510783,0.11017754914753,0.848044673146739));
#135694=DIRECTION('ref_axis',(-0.853239260760977,-1.33244400003472E-15,
-0.521519667794093));
#135695=DIRECTION('center_axis',(0.518344074797558,-0.110177412125059,0.848045021198573));
#135696=DIRECTION('ref_axis',(-0.828609503967322,0.18053216702172,0.529919264233213));
#135697=DIRECTION('center_axis',(-0.518344097776682,0.110177439185366,-0.848045003637562));
#135698=DIRECTION('ref_axis',(0.85323958281185,-6.83615864401498E-16,-0.521519140898069));
#135699=DIRECTION('center_axis',(-0.207659145615642,-0.978201246800566,
-4.81512163663705E-15));
#135700=DIRECTION('ref_axis',(-0.978201246800566,0.207659145615642,3.22797051853182E-29));
#135701=DIRECTION('center_axis',(-0.978147600733806,0.207911690817757,4.29175525433432E-15));
#135702=DIRECTION('ref_axis',(0.207911690817757,0.978147600733806,6.8296199841607E-15));
#135703=DIRECTION('center_axis',(-2.78556626507032E-16,-6.95368519647906E-15,
1.));
#135704=DIRECTION('ref_axis',(-1.,2.13365834995709E-30,-2.77764288392734E-16));
#135705=DIRECTION('center_axis',(-0.208164222161104,-0.978093889466682,
-6.82999312541884E-15));
#135706=DIRECTION('ref_axis',(-0.978093889466682,0.208164222161104,3.8857267529552E-29));
#135707=DIRECTION('center_axis',(-0.978147600733807,0.207911690817753,1.3140998576179E-15));
#135708=DIRECTION('ref_axis',(0.207911690817753,0.978147600733807,6.8296199841607E-15));
#135709=DIRECTION('center_axis',(-0.84709989316117,0.18002592730352,0.50001243635018));
#135710=DIRECTION('ref_axis',(0.488879980354404,-0.10492645952426,0.866017784401904));
#135711=DIRECTION('center_axis',(0.518344615107833,-0.110177549147486,-0.848044673146743));
#135712=DIRECTION('ref_axis',(0.853239260760977,1.13050245003069E-15,0.521519667794094));
#135713=DIRECTION('center_axis',(0.48907869839261,-0.103956896852029,-0.866022511471548));
#135714=DIRECTION('ref_axis',(0.846158656401662,-0.184432991074133,0.499999999999983));
#135715=DIRECTION('center_axis',(-0.489078713616272,0.103956889752265,0.866022503726369));
#135716=DIRECTION('ref_axis',(-0.870740345484759,1.36101104600592E-16,-0.491743073916738));
#135717=DIRECTION('center_axis',(0.518344577661257,-0.110177567038289,-0.848044693710595));
#135718=DIRECTION('ref_axis',(0.828561842309987,-0.180750786616231,0.529919264233236));
#135719=DIRECTION('center_axis',(0.518344551206575,-0.110177535564853,-0.848044713969322));
#135720=DIRECTION('ref_axis',(0.853239300541046,-1.38182160689371E-15,0.521519602711372));
#135721=DIRECTION('center_axis',(-0.978147600733806,0.207911690817757,1.45183957723504E-15));
#135722=DIRECTION('ref_axis',(0.207911690817757,0.978147600733806,6.8296199841607E-15));
#135723=DIRECTION('center_axis',(0.978147600733806,-0.20791169081776,-1.45183957723506E-15));
#135724=DIRECTION('ref_axis',(-0.20791169081776,-0.978147600733805,-6.82961998416069E-15));
#135725=DIRECTION('center_axis',(-0.978147600733807,0.207911690817753,1.3140998576179E-15));
#135726=DIRECTION('ref_axis',(0.207911690817753,0.978147600733807,6.8296199841607E-15));
#135727=DIRECTION('center_axis',(-0.978147600733806,0.207911690817757,1.45183957723504E-15));
#135728=DIRECTION('ref_axis',(0.207911690817757,0.978147600733806,6.8296199841607E-15));
#135729=DIRECTION('center_axis',(-0.978147600733807,0.207911690817753,1.3140998576179E-15));
#135730=DIRECTION('ref_axis',(0.207911690817753,0.978147600733807,6.8296199841607E-15));
#135731=DIRECTION('center_axis',(0.847119506978456,-0.180025582247714,0.499979330205709));
#135732=DIRECTION('ref_axis',(0.489253749392351,-0.103008581334865,-0.866036951219118));
#135733=DIRECTION('center_axis',(-0.489078846173999,0.103956917928292,-0.86602242548329));
#135734=DIRECTION('ref_axis',(0.870740269393778,5.30090735249655E-17,-0.491743208652699));
#135735=DIRECTION('center_axis',(-0.489078854953935,0.103956919794531,-0.866022420300872));
#135736=DIRECTION('ref_axis',(-0.207911690814671,-0.978147600734462,-1.82268897705632E-12));
#135737=DIRECTION('center_axis',(0.497265934580328,-0.0522647557777281,
-0.866022508719865));
#135738=DIRECTION('ref_axis',(0.104528463270788,0.994521895367944,1.84891472637859E-12));
#135739=DIRECTION('center_axis',(0.861270944309348,-0.0905534316548714,
-0.500012436349348));
#135740=DIRECTION('ref_axis',(0.497376550152134,-0.0512812290952578,0.8660177844024));
#135741=DIRECTION('center_axis',(-0.497265943181917,0.0522647566818097,
0.866022503726312));
#135742=DIRECTION('ref_axis',(-0.867207748104377,6.21980953328682E-15,-0.497946504785137));
#135743=DIRECTION('center_axis',(-0.994521895368276,0.104528463267628,7.29918357753749E-16));
#135744=DIRECTION('ref_axis',(0.104528463267628,0.994521895368276,6.82961998416064E-15));
#135745=DIRECTION('center_axis',(0.994521895368274,-0.104528463267647,-5.89872860613828E-16));
#135746=DIRECTION('ref_axis',(-0.104528463267647,-0.994521895368274,-6.82961998416066E-15));
#135747=DIRECTION('center_axis',(0.994521895368276,-0.104528463267629,-2.15769772104621E-15));
#135748=DIRECTION('ref_axis',(-0.104528463267629,-0.994521895368276,-6.82961998416064E-15));
#135749=DIRECTION('center_axis',(0.994521895368274,-0.104528463267647,-5.89872860613828E-16));
#135750=DIRECTION('ref_axis',(-0.104528463267647,-0.994521895368274,-6.82961998416066E-15));
#135751=DIRECTION('center_axis',(-0.994521895368276,0.104528463267627,7.29918357753739E-16));
#135752=DIRECTION('ref_axis',(0.104528463267627,0.994521895368276,6.82961998416064E-15));
#135753=DIRECTION('center_axis',(0.527021232978627,-0.0553921636609854,
0.848045003637568));
#135754=DIRECTION('ref_axis',(-0.849349030019368,-6.14256318298022E-15,
0.527831625809934));
#135755=DIRECTION('center_axis',(-0.497266077958573,0.0522647708473914,
-0.866022425483294));
#135756=DIRECTION('ref_axis',(0.867207670398082,6.7132432122382E-15,-0.497946640115918));
#135757=DIRECTION('center_axis',(-0.527021207132412,0.0553921392005488,
-0.848045021297503));
#135758=DIRECTION('ref_axis',(-0.843841975853136,0.0843581245808926,0.529919264233213));
#135759=DIRECTION('center_axis',(0.527021177161346,-0.0553921577943527,
0.848045038708649));
#135760=DIRECTION('ref_axis',(-0.84934906486752,-6.45825246295237E-15,0.527831569734768));
#135761=DIRECTION('center_axis',(-0.497266092833451,0.0522647618405224,
-0.866022417485776));
#135762=DIRECTION('ref_axis',(-0.861744800189367,0.0859994148039461,0.499999999999967));
#135763=DIRECTION('center_axis',(-0.86128949152969,0.0905598208269947,-0.49997933020507));
#135764=DIRECTION('ref_axis',(0.497139368681892,-0.0532207405904418,-0.866036951219505));
#135765=DIRECTION('center_axis',(-0.104287292793437,-0.994547213842468,
-1.52506548609107E-16));
#135766=DIRECTION('ref_axis',(-0.994547213842468,0.104287292793437,-1.21159629448723E-31));
#135767=DIRECTION('center_axis',(0.994521895368274,-0.104528463267647,-5.89872860613828E-16));
#135768=DIRECTION('ref_axis',(-0.104528463267647,-0.994521895368274,-6.82961998416066E-15));
#135769=DIRECTION('center_axis',(-0.994521895368276,0.104528463267628,7.29918357753744E-16));
#135770=DIRECTION('ref_axis',(0.104528463267628,0.994521895368276,6.82961998416064E-15));
#135771=DIRECTION('center_axis',(-2.80862404029962E-16,-6.96824330280696E-15,
1.));
#135772=DIRECTION('ref_axis',(-1.,2.00430111041611E-30,-2.82080304187759E-16));
#135773=DIRECTION('center_axis',(-0.104769627595152,-0.994496518411992,
-6.94453207115987E-15));
#135774=DIRECTION('ref_axis',(-0.994496518411992,0.104769627595152,1.55544708777506E-29));
#135775=DIRECTION('center_axis',(-0.527021693998977,0.0553922121162114,
0.848044713969329));
#135776=DIRECTION('ref_axis',(-0.849348742192414,6.03707679245365E-15,-0.527832088960271));
#135777=DIRECTION('center_axis',(-0.527021177161337,0.0553921577943518,
-0.848045038708655));
#135778=DIRECTION('ref_axis',(0.849349064867526,6.34435230052652E-15,-0.527831569734759));
#135779=DIRECTION('center_axis',(-0.527021723799262,0.0553922406001627,
0.848044693589287));
#135780=DIRECTION('ref_axis',(0.843864204097289,-0.0841354766899499,0.52991926423315));
#135781=DIRECTION('center_axis',(-0.527021758969971,0.055392218944938,0.848044673146736));
#135782=DIRECTION('ref_axis',(-0.849348701629311,6.94167645812496E-15,-0.527832154231442));
#135783=DIRECTION('center_axis',(0.527021207296535,-0.0553921391535296,
0.848045021198579));
#135784=DIRECTION('ref_axis',(-0.842941044395143,0.092929914820619,0.529919264233202));
#135785=DIRECTION('center_axis',(-0.527021232978637,0.0553921636609864,
-0.848045003637562));
#135786=DIRECTION('ref_axis',(0.849349030019363,6.26358979594039E-15,-0.527831625809943));
#135787=DIRECTION('center_axis',(-0.104271693993661,-0.994548849394384,
-5.84959516006002E-15));
#135788=DIRECTION('ref_axis',(-0.994548849394384,0.104271693993661,-2.64454906907446E-29));
#135789=DIRECTION('center_axis',(-0.994521895368276,0.104528463267629,7.29918357753754E-16));
#135790=DIRECTION('ref_axis',(0.104528463267629,0.994521895368276,6.82961998416064E-15));
#135791=DIRECTION('center_axis',(-2.80862404029962E-16,-6.96824330280696E-15,
1.));
#135792=DIRECTION('ref_axis',(-1.,2.13365834995709E-30,-2.77764288392734E-16));
#135793=DIRECTION('center_axis',(-0.104785225574079,-0.994494875050339,
-1.26696667606311E-14));
#135794=DIRECTION('ref_axis',(-0.994494875050339,0.104785225574079,1.43090320927726E-29));
#135795=DIRECTION('center_axis',(-0.994521895368274,0.104528463267647,5.89872860613828E-16));
#135796=DIRECTION('ref_axis',(0.104528463267647,0.994521895368274,6.82961998416068E-15));
#135797=DIRECTION('center_axis',(-0.861277224843024,0.090493676372023,0.500012436348713));
#135798=DIRECTION('ref_axis',(0.497169646239502,-0.053249788320922,0.86601778440276));
#135799=DIRECTION('center_axis',(0.527021758969985,-0.0553922189448753,
-0.848044673146731));
#135800=DIRECTION('ref_axis',(0.849348701629303,-6.77688496309739E-15,0.527832154231454));
#135801=DIRECTION('center_axis',(0.497265928783437,-0.0522647653361823,
-0.866022511471555));
#135802=DIRECTION('ref_axis',(0.860801807879653,-0.0949749838175252,0.499999999999983));
#135803=DIRECTION('center_axis',(-0.497265943181819,0.052264756681772,0.86602250372637));
#135804=DIRECTION('ref_axis',(-0.867207748104435,6.1483298530269E-15,-0.497946504785037));
#135805=DIRECTION('center_axis',(0.527021723597929,-0.0553922406581351,
-0.84804469371062));
#135806=DIRECTION('ref_axis',(0.84291649580075,-0.0931523188200768,0.529919264233173));
#135807=DIRECTION('center_axis',(0.527021693998996,-0.0553922121161665,
-0.84804471396932));
#135808=DIRECTION('ref_axis',(0.849348742192403,-7.26099966146184E-15,0.52783208896029));
#135809=DIRECTION('center_axis',(-0.994521895368276,0.104528463267629,7.29918357753754E-16));
#135810=DIRECTION('ref_axis',(0.104528463267629,0.994521895368276,6.82961998416064E-15));
#135811=DIRECTION('center_axis',(0.994521895368276,-0.104528463267628,-7.29918357753749E-16));
#135812=DIRECTION('ref_axis',(-0.104528463267628,-0.994521895368276,-6.82961998416064E-15));
#135813=DIRECTION('center_axis',(-0.994521895368274,0.104528463267647,5.89872860613828E-16));
#135814=DIRECTION('ref_axis',(0.104528463267647,0.994521895368274,6.82961998416068E-15));
#135815=DIRECTION('center_axis',(-0.994521895368276,0.104528463267629,5.5067571248093E-14));
#135816=DIRECTION('ref_axis',(0.104528463267629,0.994521895368276,6.8296199841606E-15));
#135817=DIRECTION('center_axis',(-0.994521895368274,0.104528463267647,5.89872860613828E-16));
#135818=DIRECTION('ref_axis',(0.104528463267647,0.994521895368274,6.82961998416068E-15));
#135819=DIRECTION('center_axis',(0.861296695145372,-0.0904912830026448,
0.499979330204954));
#135820=DIRECTION('ref_axis',(0.497340894868293,-0.0513033470048911,-0.866036951219578));
#135821=DIRECTION('center_axis',(-0.497266077958585,0.0522647708473931,
-0.866022425483287));
#135822=DIRECTION('ref_axis',(0.867207670398075,6.99786079247477E-15,-0.497946640115931));
#135823=DIRECTION('center_axis',(-0.497266086881794,0.052264771785269,-0.866022420303021));
#135824=DIRECTION('ref_axis',(-0.104528463266305,-0.994521895368415,-7.78030306748679E-13));
#135825=DIRECTION('center_axis',(0.500005014363881,6.27963960171735E-15,
-0.866022508720747));
#135826=DIRECTION('ref_axis',(3.35689482235833E-12,1.,1.94507577597585E-12));
#135827=DIRECTION('center_axis',(0.866018223014528,-3.00422161454986E-5,
-0.500012436349562));
#135828=DIRECTION('ref_axis',(0.50001221744103,0.000989701338965518,0.86601778440224));
#135829=DIRECTION('center_axis',(-0.500005023014372,-2.60454852281367E-14,
0.866022503726316));
#135830=DIRECTION('ref_axis',(-0.866022503726316,3.41480999208025E-15,-0.500005023014372));
#135831=DIRECTION('center_axis',(-1.,0.,0.));
#135832=DIRECTION('ref_axis',(0.,6.82961998416066E-15,-1.));
#135833=DIRECTION('center_axis',(1.,-9.83319205199467E-31,1.4081690688991E-16));
#135834=DIRECTION('ref_axis',(-1.4081690688991E-16,-6.82961998416066E-15,
1.));
#135835=DIRECTION('center_axis',(1.,0.,0.));
#135836=DIRECTION('ref_axis',(0.,-6.82961998416066E-15,1.));
#135837=DIRECTION('center_axis',(1.,-9.83319205199467E-31,1.4081690688991E-16));
#135838=DIRECTION('ref_axis',(-1.4081690688991E-16,-6.82961998416066E-15,
1.));
#135839=DIRECTION('center_axis',(-1.,0.,0.));
#135840=DIRECTION('ref_axis',(0.,6.82961998416066E-15,-1.));
#135841=DIRECTION('center_axis',(0.52992421326579,-5.92186660939942E-15,
0.848045003637563));
#135842=DIRECTION('ref_axis',(-0.848045003637563,-3.84166124109038E-15,
0.52992421326579));
#135843=DIRECTION('center_axis',(-0.500005158533422,6.04740227518918E-15,
-0.866022425483294));
#135844=DIRECTION('ref_axis',(0.866022425483294,3.41480999208032E-15,-0.500005158533422));
#135845=DIRECTION('center_axis',(-0.529924185004358,-2.16245522276554E-8,
-0.848045021297494));
#135846=DIRECTION('ref_axis',(-0.848037146343364,-0.00430950302354429,0.529919264233236));
#135847=DIRECTION('center_axis',(0.529924157141051,-5.92186685429947E-15,
0.848045038708645));
#135848=DIRECTION('ref_axis',(-0.848045038708645,-3.84166124109037E-15,
0.529924157141051));
#135849=DIRECTION('center_axis',(-0.500005172385361,-1.05192126270256E-8,
-0.866022417485763));
#135850=DIRECTION('ref_axis',(-0.866013458679397,-0.0045485586909233,0.499999999999984));
#135851=DIRECTION('center_axis',(-0.866037336481536,3.44576744440026E-5,
-0.499979330205396));
#135852=DIRECTION('ref_axis',(0.499979069431911,-0.000963977572674011,-0.866036951219311));
#135853=DIRECTION('center_axis',(1.,-9.83319205199467E-31,1.4081690688991E-16));
#135854=DIRECTION('ref_axis',(-1.4081690688991E-16,-6.82961998416066E-15,
1.));
#135855=DIRECTION('center_axis',(-1.,0.,0.));
#135856=DIRECTION('ref_axis',(0.,6.82961998416066E-15,-1.));
#135857=DIRECTION('center_axis',(-0.529924676825566,-5.22564495945508E-14,
0.848044713969328));
#135858=DIRECTION('ref_axis',(-0.848044713969328,3.84166124109042E-15,-0.529924676825566));
#135859=DIRECTION('center_axis',(-0.529924157141051,5.92186685429947E-15,
-0.848045038708645));
#135860=DIRECTION('ref_axis',(0.848045038708645,3.84166124109037E-15,-0.529924157141051));
#135861=DIRECTION('center_axis',(-0.529924709439995,2.52122320211198E-8,
0.84804469358928));
#135862=DIRECTION('ref_axis',(0.848035979777046,0.00453325469327678,0.529919264233214));
#135863=DIRECTION('center_axis',(-0.529924742154432,6.93661953488301E-14,
0.848044673146739));
#135864=DIRECTION('ref_axis',(-0.848044673146739,3.84166124109097E-15,-0.529924742154432));
#135865=DIRECTION('center_axis',(0.529924185162667,2.16905868611698E-8,
0.84804502119857));
#135866=DIRECTION('ref_axis',(-0.848037146343358,0.0043095030224303,0.529919264233254));
#135867=DIRECTION('center_axis',(-0.52992421326579,5.92186660939942E-15,
-0.848045003637563));
#135868=DIRECTION('ref_axis',(0.848045003637563,3.84166124109038E-15,-0.52992421326579));
#135869=DIRECTION('center_axis',(-1.,0.,0.));
#135870=DIRECTION('ref_axis',(0.,6.82961998416066E-15,-1.));
#135871=DIRECTION('center_axis',(-1.,9.83319205199467E-31,-1.4081690688991E-16));
#135872=DIRECTION('ref_axis',(1.4081690688991E-16,6.82961998416066E-15,
-1.));
#135873=DIRECTION('center_axis',(-0.866018223014801,-3.00422156492971E-5,
0.500012436349089));
#135874=DIRECTION('ref_axis',(0.500012217440556,-0.000989701341688796,0.86601778440251));
#135875=DIRECTION('center_axis',(0.529924742154432,5.92186430159433E-15,
-0.848044673146739));
#135876=DIRECTION('ref_axis',(0.848044673146739,-3.84166124109037E-15,0.529924742154432));
#135877=DIRECTION('center_axis',(0.50000500959944,-1.01138193904953E-8,
-0.866022511471534));
#135878=DIRECTION('ref_axis',(0.866013834616146,-0.00447641077665303,0.499999999999997));
#135879=DIRECTION('center_axis',(-0.50000502301429,-6.04740282155761E-15,
0.866022503726363));
#135880=DIRECTION('ref_axis',(-0.866022503726363,3.41480999208032E-15,-0.50000502301429));
#135881=DIRECTION('center_axis',(0.529924709245831,-2.52894451112192E-8,
-0.848044693710609));
#135882=DIRECTION('ref_axis',(0.848035979777058,-0.0045332546927221,0.5299192642332));
#135883=DIRECTION('center_axis',(0.529924676825566,3.4875337890239E-14,
-0.848044713969328));
#135884=DIRECTION('ref_axis',(0.848044713969328,-3.84166124109041E-15,0.529924676825566));
#135885=DIRECTION('center_axis',(-1.,0.,0.));
#135886=DIRECTION('ref_axis',(0.,6.82961998416066E-15,-1.));
#135887=DIRECTION('center_axis',(1.,0.,0.));
#135888=DIRECTION('ref_axis',(0.,-6.82961998416066E-15,1.));
#135889=DIRECTION('center_axis',(-1.,9.83319205199467E-31,-1.4081690688991E-16));
#135890=DIRECTION('ref_axis',(1.4081690688991E-16,6.82961998416066E-15,
-1.));
#135891=DIRECTION('center_axis',(-1.,-3.81527851617387E-28,5.46369598732844E-14));
#135892=DIRECTION('ref_axis',(-5.46369598732844E-14,6.82961998416066E-15,
-1.));
#135893=DIRECTION('center_axis',(-1.,9.83319205199467E-31,-1.4081690688991E-16));
#135894=DIRECTION('ref_axis',(1.4081690688991E-16,6.82961998416066E-15,
-1.));
#135895=DIRECTION('center_axis',(0.866037336481549,3.44576743629553E-5,
0.499979330205372));
#135896=DIRECTION('ref_axis',(0.499979069431883,0.000963977580906077,-0.866036951219318));
#135897=DIRECTION('center_axis',(-0.500005158533445,6.04740227518909E-15,
-0.866022425483281));
#135898=DIRECTION('ref_axis',(0.86602242548328,3.41480999208034E-15,-0.500005158533445));
#135899=DIRECTION('center_axis',(-0.500005167502186,6.23740986055901E-15,
-0.866022420305105));
#135900=DIRECTION('ref_axis',(5.80463060319271E-12,-1.,-3.35252384988615E-12));
#135901=DIRECTION('center_axis',(0.497265934575139,0.0522647557772062,-0.866022508722875));
#135902=DIRECTION('ref_axis',(-0.104528463271195,0.994521895367901,-2.02375299837496E-12));
#135903=DIRECTION('center_axis',(0.861277224842077,0.0904936763703871,-0.500012436350639));
#135904=DIRECTION('ref_axis',(0.497169646238188,0.0532497883517295,0.86601778440162));
#135905=DIRECTION('center_axis',(-0.497265943181921,-0.0522647566818225,
0.866022503726309));
#135906=DIRECTION('ref_axis',(-0.867207748104376,6.05825588881007E-15,-0.49794650478514));
#135907=DIRECTION('center_axis',(-0.99452189536827,-0.104528463267684,-7.29918357754136E-16));
#135908=DIRECTION('ref_axis',(-0.104528463267684,0.99452189536827,6.82961998416065E-15));
#135909=DIRECTION('center_axis',(0.994521895368273,0.104528463267661,8.69963854894025E-16));
#135910=DIRECTION('ref_axis',(0.104528463267661,-0.994521895368273,-6.82961998416065E-15));
#135911=DIRECTION('center_axis',(0.99452189536827,0.104528463267683,1.60286761075321E-17));
#135912=DIRECTION('ref_axis',(0.104528463267683,-0.99452189536827,-6.82961998416065E-15));
#135913=DIRECTION('center_axis',(0.994521895368273,0.104528463267661,8.69963854894025E-16));
#135914=DIRECTION('ref_axis',(0.104528463267661,-0.994521895368273,-6.82961998416065E-15));
#135915=DIRECTION('center_axis',(-0.99452189536827,-0.104528463267684,-7.29918357754136E-16));
#135916=DIRECTION('ref_axis',(-0.104528463267684,0.99452189536827,6.82961998416065E-15));
#135917=DIRECTION('center_axis',(0.527021232978633,0.0553921636610031,0.848045003637563));
#135918=DIRECTION('ref_axis',(-0.849349030019364,-7.40393733324392E-15,
0.52783162580994));
#135919=DIRECTION('center_axis',(-0.497266077958558,-0.0522647708474047,
-0.866022425483302));
#135920=DIRECTION('ref_axis',(0.86720767039809,7.13435718091396E-15,-0.497946640115905));
#135921=DIRECTION('center_axis',(-0.527021202610616,-0.0553921822221918,
-0.848045021297528));
#135922=DIRECTION('ref_axis',(-0.842941044392581,-0.0929299148441298,0.529919264233154));
#135923=DIRECTION('center_axis',(0.527021177161334,0.0553921577943685,0.848045038708656));
#135924=DIRECTION('ref_axis',(-0.849349064867527,-7.44584183003648E-15,
0.527831569734757));
#135925=DIRECTION('center_axis',(-0.49726609063569,-0.0522647827511846,
-0.866022417485754));
#135926=DIRECTION('ref_axis',(-0.860793892491192,-0.095046697206364,0.500000000000024));
#135927=DIRECTION('center_axis',(-0.861296695145142,-0.0904912830030917,
-0.499979330205271));
#135928=DIRECTION('ref_axis',(0.497340894869072,0.051303347000484,-0.866036951219391));
#135929=DIRECTION('center_axis',(0.104769627595185,-0.994496518411988,-1.37365653674844E-14));
#135930=DIRECTION('ref_axis',(-0.994496518411988,-0.104769627595185,-2.12885829743461E-29));
#135931=DIRECTION('center_axis',(0.994521895368273,0.104528463267661,8.69963854894025E-16));
#135932=DIRECTION('ref_axis',(0.104528463267661,-0.994521895368273,-6.82961998416065E-15));
#135933=DIRECTION('center_axis',(-0.99452189536827,-0.104528463267682,-7.29918357754126E-16));
#135934=DIRECTION('ref_axis',(-0.104528463267682,0.99452189536827,6.82961998416065E-15));
#135935=DIRECTION('center_axis',(-2.80862404029962E-16,-6.99768205256557E-15,
1.));
#135936=DIRECTION('ref_axis',(-1.,2.00430111041611E-30,-2.82080304187759E-16));
#135937=DIRECTION('center_axis',(0.104287292793436,-0.994547213842468,-6.94488607545882E-15));
#135938=DIRECTION('ref_axis',(-0.994547213842468,-0.104287292793436,-3.36172022659011E-29));
#135939=DIRECTION('center_axis',(-0.527021693998993,-0.0553922121162073,
0.84804471396932));
#135940=DIRECTION('ref_axis',(-0.849348742192405,6.20133477398574E-15,-0.527832088960287));
#135941=DIRECTION('center_axis',(-0.527021177161343,-0.0553921577943695,
-0.84804503870865));
#135942=DIRECTION('ref_axis',(0.849349064867521,7.1754696837161E-15,-0.527831569734766));
#135943=DIRECTION('center_axis',(-0.527021729070144,-0.055392190451128,
0.848044693589284));
#135944=DIRECTION('ref_axis',(0.842916495800427,0.0931523188229197,0.529919264233187));
#135945=DIRECTION('center_axis',(-0.527021758969984,-0.0553922189448874,
0.848044673146731));
#135946=DIRECTION('ref_axis',(-0.849348701629304,6.81770145149935E-15,-0.527832154231453));
#135947=DIRECTION('center_axis',(0.527021202762368,0.0553921822932962,0.848045021198576));
#135948=DIRECTION('ref_axis',(-0.843841975853092,-0.0843581245812077,0.529919264233233));
#135949=DIRECTION('center_axis',(-0.527021232978546,-0.0553921636609939,
-0.848045003637618));
#135950=DIRECTION('ref_axis',(0.849349030019419,7.36199811433283E-15,-0.527831625809853));
#135951=DIRECTION('center_axis',(0.104785225574091,-0.994494875050338,-8.01139650341116E-15));
#135952=DIRECTION('ref_axis',(-0.994494875050338,-0.104785225574091,1.5603430202424E-30));
#135953=DIRECTION('center_axis',(-0.99452189536827,-0.104528463267683,-7.29918357754131E-16));
#135954=DIRECTION('ref_axis',(-0.104528463267683,0.99452189536827,6.82961998416065E-15));
#135955=DIRECTION('center_axis',(-2.80862404029962E-16,-6.99768205256557E-15,
1.));
#135956=DIRECTION('ref_axis',(-1.,2.13365834995709E-30,-2.77764288392734E-16));
#135957=DIRECTION('center_axis',(0.104271693993677,-0.994548849394382,-8.04019983285269E-15));
#135958=DIRECTION('ref_axis',(-0.994548849394382,-0.104271693993677,1.6725368118524E-29));
#135959=DIRECTION('center_axis',(-0.994521895368273,-0.104528463267661,
-8.69963854894025E-16));
#135960=DIRECTION('ref_axis',(-0.104528463267661,0.994521895368273,6.82961998416067E-15));
#135961=DIRECTION('center_axis',(-0.861270944309899,-0.0905534316539422,
0.500012436348568));
#135962=DIRECTION('ref_axis',(0.497376550152552,0.0512812290837431,0.866017784402841));
#135963=DIRECTION('center_axis',(0.527021758969972,0.0553922189449323,-0.848044673146736));
#135964=DIRECTION('ref_axis',(0.84934870162931,-6.74368895948955E-15,0.527832154231442));
#135965=DIRECTION('center_axis',(0.497265930897847,0.0522647452191274,-0.866022511471542));
#135966=DIRECTION('ref_axis',(0.861737632557095,0.0860712067703171,0.499999999999995));
#135967=DIRECTION('center_axis',(-0.497265943181812,-0.0522647566818107,
0.866022503726372));
#135968=DIRECTION('ref_axis',(-0.867207748104439,7.38830921412877E-15,-0.497946504785031));
#135969=DIRECTION('center_axis',(0.527021728884924,0.0553921903559162,-0.848044693710608));
#135970=DIRECTION('ref_axis',(0.843864204093765,0.0841354767247419,0.529919264233238));
#135971=DIRECTION('center_axis',(0.527021693998975,0.0553922121162348,-0.848044713969329));
#135972=DIRECTION('ref_axis',(0.849348742192415,-7.50888177194347E-15,0.52783208896027));
#135973=DIRECTION('center_axis',(-0.99452189536827,-0.104528463267683,-1.60286761075321E-17));
#135974=DIRECTION('ref_axis',(-0.104528463267683,0.99452189536827,6.82961998416065E-15));
#135975=DIRECTION('center_axis',(0.99452189536827,0.104528463267683,7.29918357754131E-16));
#135976=DIRECTION('ref_axis',(0.104528463267683,-0.99452189536827,-6.82961998416065E-15));
#135977=DIRECTION('center_axis',(-0.994521895368273,-0.104528463267661,
-8.69963854894025E-16));
#135978=DIRECTION('ref_axis',(-0.104528463267661,0.994521895368273,6.82961998416067E-15));
#135979=DIRECTION('center_axis',(-0.99452189536827,-0.104528463267683,-7.29918357754131E-16));
#135980=DIRECTION('ref_axis',(-0.104528463267683,0.99452189536827,6.82961998416065E-15));
#135981=DIRECTION('center_axis',(-0.994521895368273,-0.104528463267661,
-8.69963854894025E-16));
#135982=DIRECTION('ref_axis',(-0.104528463267661,0.994521895368273,6.82961998416067E-15));
#135983=DIRECTION('center_axis',(0.861289491529725,0.0905598208272782,0.499979330204959));
#135984=DIRECTION('ref_axis',(0.497139368680338,0.0532207406041062,-0.866036951219557));
#135985=DIRECTION('center_axis',(-0.497266077958593,-0.0522647708474091,
-0.866022425483282));
#135986=DIRECTION('ref_axis',(0.86720767039807,6.57816839557369E-15,-0.49794664011594));
#135987=DIRECTION('center_axis',(-0.497266086885392,-0.0522647717856406,
-0.866022420300932));
#135988=DIRECTION('ref_axis',(0.104528463264192,-0.994521895368637,2.01938203211187E-12));
#135989=DIRECTION('center_axis',(0.489078705150196,0.103956887952764,-0.866022508723523));
#135990=DIRECTION('ref_axis',(-0.207911690817648,0.978147600733829,7.86772223991619E-14));
#135991=DIRECTION('center_axis',(0.847099893162016,0.180025927305019,-0.500012436348206));
#135992=DIRECTION('ref_axis',(0.488879980349761,0.104926459536577,0.866017784403032));
#135993=DIRECTION('center_axis',(-0.489078713616374,-0.103956889752297,
0.866022503726307));
#135994=DIRECTION('ref_axis',(-0.8707403454847,2.32007185439358E-16,-0.491743073916842));
#135995=DIRECTION('center_axis',(-0.978147600733806,-0.207911690817757,
-1.45183957723504E-15));
#135996=DIRECTION('ref_axis',(-0.207911690817757,0.978147600733806,6.8296199841607E-15));
#135997=DIRECTION('center_axis',(0.978147600733804,0.207911690817766,1.58957929685223E-15));
#135998=DIRECTION('ref_axis',(0.207911690817766,-0.978147600733804,-6.82961998416066E-15));
#135999=DIRECTION('center_axis',(0.978147600733806,0.207911690817757,-1.38807609986408E-15));
#136000=DIRECTION('ref_axis',(0.207911690817757,-0.978147600733806,-6.8296199841607E-15));
#136001=DIRECTION('center_axis',(0.978147600733804,0.207911690817766,1.58957929685223E-15));
#136002=DIRECTION('ref_axis',(0.207911690817766,-0.978147600733804,-6.82961998416066E-15));
#136003=DIRECTION('center_axis',(-0.978147600733806,-0.207911690817757,
-1.45183957723504E-15));
#136004=DIRECTION('ref_axis',(-0.207911690817757,0.978147600733806,6.8296199841607E-15));
#136005=DIRECTION('center_axis',(0.518344097776651,0.110177439185348,0.848045003637583));
#136006=DIRECTION('ref_axis',(-0.85323958281187,1.15837605560063E-15,0.521519140898037));
#136007=DIRECTION('center_axis',(-0.489078846174,-0.103956917928278,-0.866022425483291));
#136008=DIRECTION('ref_axis',(0.870740269393777,1.51570610952153E-16,-0.4917432086527));
#136009=DIRECTION('center_axis',(-0.518344065636424,-0.11017745446327,-0.848045021297511));
#136010=DIRECTION('ref_axis',(-0.828609503963262,-0.180532167040568,0.52991926423314));
#136011=DIRECTION('center_axis',(0.518344042878403,0.110177427516365,0.848045038708646));
#136012=DIRECTION('ref_axis',(-0.8532396169873,5.9869712929813E-16,0.521519084984783));
#136013=DIRECTION('center_axis',(-0.489078857536072,-0.103956931097839,
-0.866022417485789));
#136014=DIRECTION('ref_axis',(-0.846143288283865,-0.184503484227827,0.499999999999961));
#136015=DIRECTION('center_axis',(-0.847119506978912,-0.180025582247147,
-0.499979330205139));
#136016=DIRECTION('ref_axis',(0.489253749388305,0.1030085813512,-0.866036951219461));
#136017=DIRECTION('center_axis',(0.208148881407623,-0.978097154258592,6.53004781901118E-15));
#136018=DIRECTION('ref_axis',(-0.978097154258592,-0.208148881407623,-2.96788381662184E-29));
#136019=DIRECTION('center_axis',(0.978147600733804,0.207911690817766,1.58957929685223E-15));
#136020=DIRECTION('ref_axis',(0.207911690817766,-0.978147600733804,-6.82961998416066E-15));
#136021=DIRECTION('center_axis',(-0.978147600733806,-0.20791169081776,-1.45183957723506E-15));
#136022=DIRECTION('ref_axis',(-0.20791169081776,0.978147600733805,6.82961998416069E-15));
#136023=DIRECTION('center_axis',(-2.78556626507032E-16,-7.01224015889348E-15,
1.));
#136024=DIRECTION('ref_axis',(-1.,2.00430111041611E-30,-2.75028296583065E-16));
#136025=DIRECTION('center_axis',(0.20767448800183,-0.978197989689806,-6.83072005339165E-15));
#136026=DIRECTION('ref_axis',(-0.978197989689806,-0.20767448800183,3.9702683762468E-29));
#136027=DIRECTION('center_axis',(-0.518344551206579,-0.110177535564846,
0.848044713969321));
#136028=DIRECTION('ref_axis',(-0.853239300541043,-1.24733491466344E-15,
-0.521519602711376));
#136029=DIRECTION('center_axis',(-0.518344042878406,-0.110177427516365,
-0.848045038708644));
#136030=DIRECTION('ref_axis',(0.853239616987299,-6.36492759772716E-16,-0.521519084984785));
#136031=DIRECTION('center_axis',(-0.518344588350029,-0.110177517685333,
0.848044693589281));
#136032=DIRECTION('ref_axis',(0.828561842307981,0.180750786625398,0.529919264233245));
#136033=DIRECTION('center_axis',(-0.518344615107843,-0.110177549147448,
0.848044673146742));
#136034=DIRECTION('ref_axis',(-0.853239260760972,1.43910732930017E-15,-0.521519667794102));
#136035=DIRECTION('center_axis',(0.518344065778186,0.110177454557846,0.848045021198576));
#136036=DIRECTION('ref_axis',(-0.830401496090018,-0.172101506925331,0.529919264233233));
#136037=DIRECTION('center_axis',(-0.518344097776628,-0.110177439185343,
-0.848045003637598));
#136038=DIRECTION('ref_axis',(0.853239582811884,-4.04112561920183E-16,-0.521519140898014));
#136039=DIRECTION('center_axis',(0.208164222161113,-0.978093889466681,4.54346712785195E-15));
#136040=DIRECTION('ref_axis',(-0.978093889466681,-0.208164222161113,4.44186922891595E-30));
#136041=DIRECTION('center_axis',(-0.978147600733806,-0.207911690817757,
4.22799177696351E-15));
#136042=DIRECTION('ref_axis',(-0.207911690817757,0.978147600733806,6.8296199841607E-15));
#136043=DIRECTION('center_axis',(-2.78556626507032E-16,-7.01224015889348E-15,
1.));
#136044=DIRECTION('ref_axis',(-1.,2.13365834995709E-30,-2.77764288392734E-16));
#136045=DIRECTION('center_axis',(0.207659145615657,-0.978201246800563,-8.8463639587112E-15));
#136046=DIRECTION('ref_axis',(-0.978201246800563,-0.207659145615657,3.74304734203989E-29));
#136047=DIRECTION('center_axis',(-0.978147600733804,-0.207911690817766,
-1.58957929685223E-15));
#136048=DIRECTION('ref_axis',(-0.207911690817766,0.978147600733804,6.82961998416068E-15));
#136049=DIRECTION('center_axis',(-0.847087400905467,-0.180084698747548,
0.500012436349562));
#136050=DIRECTION('ref_axis',(0.489291521297893,0.102990311607302,0.866017784402274));
#136051=DIRECTION('center_axis',(0.518344615107832,0.110177549147525,-0.848044673146738));
#136052=DIRECTION('ref_axis',(0.853239260760976,-1.2546710781479E-15,0.521519667794095));
#136053=DIRECTION('center_axis',(0.489078702597484,0.103956877069823,-0.866022511471527));
#136054=DIRECTION('ref_axis',(0.848020052664497,0.175675810170021,0.50000000000001));
#136055=DIRECTION('center_axis',(-0.489078713616299,-0.103956889752283,
0.866022503726351));
#136056=DIRECTION('ref_axis',(-0.870740345484743,8.1185976130115E-16,-0.491743073916766));
#136057=DIRECTION('center_axis',(0.51834458817718,0.110177517564643,-0.84804469371061));
#136058=DIRECTION('ref_axis',(0.830446875605853,0.171882402214531,0.529919264233184));
#136059=DIRECTION('center_axis',(0.518344551206566,0.110177535564845,-0.848044713969329));
#136060=DIRECTION('ref_axis',(0.853239300541051,-1.48217857625388E-15,0.521519602711362));
#136061=DIRECTION('center_axis',(-0.978147600733806,-0.207911690817757,
1.38807609986424E-15));
#136062=DIRECTION('ref_axis',(-0.207911690817757,0.978147600733806,6.8296199841607E-15));
#136063=DIRECTION('center_axis',(0.978147600733807,0.207911690817751,1.45183957723501E-15));
#136064=DIRECTION('ref_axis',(0.207911690817751,-0.978147600733807,-6.82961998416071E-15));
#136065=DIRECTION('center_axis',(-0.978147600733804,-0.207911690817766,
-1.58957929685223E-15));
#136066=DIRECTION('ref_axis',(-0.207911690817766,0.978147600733804,6.82961998416068E-15));
#136067=DIRECTION('center_axis',(-0.978147600733806,-0.207911690817757,
5.76710029884055E-14));
#136068=DIRECTION('ref_axis',(-0.207911690817757,0.978147600733806,6.8296199841607E-15));
#136069=DIRECTION('center_axis',(-0.978147600733804,-0.207911690817766,
-1.58957929685223E-15));
#136070=DIRECTION('ref_axis',(-0.207911690817766,0.978147600733804,6.82961998416068E-15));
#136071=DIRECTION('center_axis',(0.847105178672063,0.180092991630817,0.499979330205193));
#136072=DIRECTION('ref_axis',(0.488852904975831,0.104894406043608,-0.866036951219433));
#136073=DIRECTION('center_axis',(-0.489078846174022,-0.103956917928285,
-0.866022425483278));
#136074=DIRECTION('ref_axis',(0.870740269393764,-6.42192866208513E-16,-0.491743208652722));
#136075=DIRECTION('center_axis',(-0.489078854951574,-0.103956919794024,
-0.866022420302267));
#136076=DIRECTION('ref_axis',(0.207911690820505,-0.978147600733222,-1.63036687875202E-12));
#136077=DIRECTION('center_axis',(0.475533027088661,0.15451004671042,-0.866022508722169));
#136078=DIRECTION('ref_axis',(-0.309016994375666,0.95105651629492,-3.62789414398747E-13));
#136079=DIRECTION('center_axis',(0.823641557784728,0.26758577650676,-0.500012436346558));
#136080=DIRECTION('ref_axis',(0.475234043104007,0.155453534443493,0.866017784404018));
#136081=DIRECTION('center_axis',(-0.47553303531813,-0.154510049384321,0.866022503726307));
#136082=DIRECTION('ref_axis',(-0.876548788012439,1.44209482510565E-15,-0.481313018974061));
#136083=DIRECTION('center_axis',(-0.951056516295146,-0.309016994374972,
-2.15785413849121E-15));
#136084=DIRECTION('ref_axis',(-0.309016994374972,0.951056516295146,6.82961998416073E-15));
#136085=DIRECTION('center_axis',(0.951056516295151,0.309016994374955,2.29177897539327E-15));
#136086=DIRECTION('ref_axis',(0.309016994374955,-0.951056516295151,-6.82961998416066E-15));
#136087=DIRECTION('center_axis',(0.951056516295148,0.309016994374964,2.15785413849116E-15));
#136088=DIRECTION('ref_axis',(0.309016994374964,-0.951056516295148,-6.82961998416075E-15));
#136089=DIRECTION('center_axis',(0.951056516295151,0.309016994374955,2.29177897539327E-15));
#136090=DIRECTION('ref_axis',(0.309016994374955,-0.951056516295151,-6.82961998416066E-15));
#136091=DIRECTION('center_axis',(-0.951056516295151,-0.309016994374956,
-2.1578541384911E-15));
#136092=DIRECTION('ref_axis',(-0.309016994374956,0.951056516295151,6.82961998416057E-15));
#136093=DIRECTION('center_axis',(0.503987876168974,0.163755587629894,0.848045003637587));
#136094=DIRECTION('ref_axis',(-0.859649462041495,-7.24230631194929E-16,
0.510884333691853));
#136095=DIRECTION('center_axis',(-0.475533164204393,-0.154510091261976,
-0.866022425483297));
#136096=DIRECTION('ref_axis',(0.876548714628846,1.87535286613278E-16,-0.481313152617418));
#136097=DIRECTION('center_axis',(-0.503987842609475,-0.163755599459623,
-0.848045021297494));
#136098=DIRECTION('ref_axis',(-0.805199544417973,-0.266156471015856,0.529919264233218));
#136099=DIRECTION('center_axis',(0.503987822791202,0.163755570286405,0.848045038708652));
#136100=DIRECTION('ref_axis',(-0.859649495083705,-1.79266124745912E-15,
0.510884278092732));
#136101=DIRECTION('center_axis',(-0.475533174129345,-0.154510105541947,
-0.866022417485764));
#136102=DIRECTION('ref_axis',(-0.822222161144011,-0.271938812462805,0.499999999999991));
#136103=DIRECTION('center_axis',(-0.8236611002229,-0.267587483539854,-0.49997933020517));
#136104=DIRECTION('ref_axis',(0.475806237445598,0.153585232136407,-0.866036951219444));
#136105=DIRECTION('center_axis',(0.309247612517411,-0.950981553003149,-3.26200391676225E-14));
#136106=DIRECTION('ref_axis',(-0.950981553003149,-0.309247612517411,-3.41480999208011E-15));
#136107=DIRECTION('center_axis',(0.951056516295151,0.309016994374955,2.29177897539327E-15));
#136108=DIRECTION('ref_axis',(0.309016994374955,-0.951056516295151,-6.82961998416066E-15));
#136109=DIRECTION('center_axis',(-0.951056516295151,-0.309016994374956,
-2.1578541384911E-15));
#136110=DIRECTION('ref_axis',(-0.309016994374956,0.951056516295151,6.82961998416057E-15));
#136111=DIRECTION('center_axis',(-2.74741743792087E-16,-7.02647749501057E-15,
1.));
#136112=DIRECTION('ref_axis',(-1.,2.00430111041611E-30,-2.75028296583065E-16));
#136113=DIRECTION('center_axis',(0.308786358060997,-0.951131423661013,-6.64171523299946E-15));
#136114=DIRECTION('ref_axis',(-0.951131423661013,-0.308786358060997,-3.41480999208026E-15));
#136115=DIRECTION('center_axis',(-0.503988317040562,-0.16375573087774,0.848044713969328));
#136116=DIRECTION('ref_axis',(-0.859649189130478,-2.03018390514586E-16,
-0.510884792910606));
#136117=DIRECTION('center_axis',(-0.503987822791237,-0.163755570286416,
-0.848045038708628));
#136118=DIRECTION('ref_axis',(0.859649495083683,4.98171905108308E-17,-0.510884278092769));
#136119=DIRECTION('center_axis',(-0.503988355851731,-0.163755716971875,
0.848044693589256));
#136120=DIRECTION('ref_axis',(0.805129291876083,0.266368911019414,0.529919264233193));
#136121=DIRECTION('center_axis',(-0.503988379172014,-0.163755751065428,
0.848044673146742));
#136122=DIRECTION('ref_axis',(-0.859649150669462,-1.65774526852702E-15,
-0.510884857627698));
#136123=DIRECTION('center_axis',(0.503987842737129,0.163755599579094,0.84804502119856));
#136124=DIRECTION('ref_axis',(-0.807862963764753,-0.25795930913955,0.529919264233219));
#136125=DIRECTION('center_axis',(-0.50398787616897,-0.163755587629893,-0.84804500363759));
#136126=DIRECTION('ref_axis',(0.859649462041497,1.07198038077594E-15,-0.510884333691849));
#136127=DIRECTION('center_axis',(0.309262527968972,-0.95097670255072,-6.64063482126083E-15));
#136128=DIRECTION('ref_axis',(-0.95097670255072,-0.309262527968972,-3.41480999208037E-15));
#136129=DIRECTION('center_axis',(-0.951056516295148,-0.309016994374964,
-2.15785413849116E-15));
#136130=DIRECTION('ref_axis',(-0.309016994374964,0.951056516295148,6.82961998416075E-15));
#136131=DIRECTION('center_axis',(-2.74741743792087E-16,-7.02647749501057E-15,
1.));
#136132=DIRECTION('ref_axis',(-1.,2.13365834995709E-30,-2.77764288392734E-16));
#136133=DIRECTION('center_axis',(0.308771440182806,-0.951136266645025,-6.64174905137606E-15));
#136134=DIRECTION('ref_axis',(-0.951136266645025,-0.308771440182806,-3.41480999208035E-15));
#136135=DIRECTION('center_axis',(-0.951056516295151,-0.309016994374955,
-2.29177897539327E-15));
#136136=DIRECTION('ref_axis',(-0.309016994374955,0.951056516295151,6.82961998416058E-15));
#136137=DIRECTION('center_axis',(-0.823622990672772,-0.267642920195548,
0.500012436349775));
#136138=DIRECTION('ref_axis',(0.475845712151136,0.153571010697317,0.866017784402135));
#136139=DIRECTION('center_axis',(0.503988379171984,0.163755751065574,-0.848044673146731));
#136140=DIRECTION('ref_axis',(0.859649150669472,-1.91145464518171E-15,0.51088485762768));
#136141=DIRECTION('center_axis',(0.475533025685305,0.154510035619257,-0.866022511471564));
#136142=DIRECTION('ref_axis',(0.825011387615606,0.263355672626591,0.499999999999969));
#136143=DIRECTION('center_axis',(-0.475533035318107,-0.154510049384286,
0.866022503726325));
#136144=DIRECTION('ref_axis',(-0.876548788012453,5.44148765414771E-16,-0.481313018974035));
#136145=DIRECTION('center_axis',(0.503988355690328,0.163755716840074,-0.848044693710628));
#136146=DIRECTION('ref_axis',(0.807930997361746,0.257746148170262,0.529919264233192));
#136147=DIRECTION('center_axis',(0.503988317040544,0.163755730877811,-0.848044713969325));
#136148=DIRECTION('ref_axis',(0.859649189130485,7.79100967592155E-16,0.510884792910593));
#136149=DIRECTION('center_axis',(-0.951056516295148,-0.309016994374964,
-2.15785413849116E-15));
#136150=DIRECTION('ref_axis',(-0.309016994374964,0.951056516295148,6.82961998416075E-15));
#136151=DIRECTION('center_axis',(0.951056516295148,0.309016994374964,2.15785413849116E-15));
#136152=DIRECTION('ref_axis',(0.309016994374964,-0.951056516295148,-6.82961998416075E-15));
#136153=DIRECTION('center_axis',(-0.951056516295151,-0.309016994374955,
-2.29177897539327E-15));
#136154=DIRECTION('ref_axis',(-0.309016994374955,0.951056516295151,6.82961998416058E-15));
#136155=DIRECTION('center_axis',(-0.951056516295148,-0.309016994374964,
6.28402042242275E-15));
#136156=DIRECTION('ref_axis',(-0.309016994374964,0.951056516295148,6.82961998416068E-15));
#136157=DIRECTION('center_axis',(-0.951056516295151,-0.309016994374955,
-2.29177897539327E-15));
#136158=DIRECTION('ref_axis',(-0.309016994374955,0.951056516295151,6.82961998416058E-15));
#136159=DIRECTION('center_axis',(0.823639804208761,0.267653025931831,0.499979330205248));
#136160=DIRECTION('ref_axis',(0.475210466541244,0.155418826440911,-0.866036951219394));
#136161=DIRECTION('center_axis',(-0.47553316420442,-0.154510091261976,-0.866022425483283));
#136162=DIRECTION('ref_axis',(0.876548714628831,-9.05295501398111E-16,-0.481313152617445));
#136163=DIRECTION('center_axis',(-0.475533172737204,-0.154510094034435,
-0.866022420303284));
#136164=DIRECTION('ref_axis',(0.309016994382667,-0.951056516292645,-4.69440758122482E-12));
#136165=DIRECTION('center_axis',(0.456777309668931,0.203370361062697,-0.866022508721824));
#136166=DIRECTION('ref_axis',(-0.406736643079858,0.913545457640795,-2.53078398719129E-12));
#136167=DIRECTION('center_axis',(0.791159233140771,0.352213899940676,-0.500012436350025));
#136168=DIRECTION('ref_axis',(0.456381342224756,0.204277427946829,0.866017784402005));
#136169=DIRECTION('center_axis',(-0.456777317573273,-0.203370364581918,
0.866022503726308));
#136170=DIRECTION('ref_axis',(-0.884507036382098,-9.28493662905854E-16,
-0.466526850878444));
#136171=DIRECTION('center_axis',(-0.913545457642594,-0.406736643075817,
-2.84022679824583E-15));
#136172=DIRECTION('ref_axis',(-0.406736643075817,0.913545457642593,6.82961998416057E-15));
#136173=DIRECTION('center_axis',(0.913545457642598,0.406736643075807,2.96886944389432E-15));
#136174=DIRECTION('ref_axis',(0.406736643075807,-0.913545457642598,-6.82961998416066E-15));
#136175=DIRECTION('center_axis',(0.913545457642598,0.406736643075807,2.84022679824576E-15));
#136176=DIRECTION('ref_axis',(0.406736643075807,-0.913545457642598,-6.8296199841606E-15));
#136177=DIRECTION('center_axis',(0.913545457642598,0.406736643075807,2.96886944389432E-15));
#136178=DIRECTION('ref_axis',(0.406736643075807,-0.913545457642598,-6.82961998416066E-15));
#136179=DIRECTION('center_axis',(-0.913545457642594,-0.406736643075817,
-2.84022679824583E-15));
#136180=DIRECTION('ref_axis',(-0.406736643075817,0.913545457642593,6.82961998416057E-15));
#136181=DIRECTION('center_axis',(0.484109857923749,0.215539595588291,0.848045003637592));
#136182=DIRECTION('ref_axis',(-0.868458021516008,-1.07236589050538E-15,
0.495762710239991));
#136183=DIRECTION('center_axis',(-0.456777441376078,-0.203370419702497,
-0.866022425483286));
#136184=DIRECTION('ref_axis',(0.884506966812055,-2.08482502526669E-15,-0.466526982779066));
#136185=DIRECTION('center_axis',(-0.484109823308942,-0.215539603851087,
-0.848045021297514));
#136186=DIRECTION('ref_axis',(-0.77296765015055,-0.348864709042549,0.529919264233142));
#136187=DIRECTION('center_axis',(0.484109806651292,0.215539572760322,0.848045038708645));
#136188=DIRECTION('ref_axis',(-0.868458052949955,-5.26259601010897E-16,
0.495762655175208));
#136189=DIRECTION('center_axis',(-0.456777449753612,-0.203370434942479,
-0.866022417485768));
#136190=DIRECTION('ref_axis',(-0.789292595944142,-0.356394722166,0.499999999999978));
#136191=DIRECTION('center_axis',(-0.791178490090692,-0.352217640366598,
-0.499979330205158));
#136192=DIRECTION('ref_axis',(0.457145692798374,0.20247917097425,-0.866036951219447));
#136193=DIRECTION('center_axis',(0.406958162070226,-0.913446798847324,-6.37856490440286E-15));
#136194=DIRECTION('ref_axis',(-0.913446798847324,-0.406958162070226,-3.41480999208029E-15));
#136195=DIRECTION('center_axis',(0.913545457642598,0.406736643075807,2.96886944389432E-15));
#136196=DIRECTION('ref_axis',(0.406736643075807,-0.913545457642598,-6.82961998416066E-15));
#136197=DIRECTION('center_axis',(-0.913545457642603,-0.406736643075797,
-2.84022679824569E-15));
#136198=DIRECTION('ref_axis',(-0.406736643075797,0.913545457642603,6.82961998416064E-15));
#136199=DIRECTION('center_axis',(-2.69459552538469E-16,-7.04023807368299E-15,
1.));
#136200=DIRECTION('ref_axis',(-1.,2.00430111041611E-30,-2.67976288978371E-16));
#136201=DIRECTION('center_axis',(0.406515100163544,-0.913644062717546,-6.37994239064628E-15));
#136202=DIRECTION('ref_axis',(-0.913644062717546,-0.406515100163544,-3.41480999208035E-15));
#136203=DIRECTION('center_axis',(-0.484110281406756,-0.215539784135086,
0.8480447139693));
#136204=DIRECTION('ref_axis',(-0.868457761888263,3.97238567950502E-16,-0.495763165045598));
#136205=DIRECTION('center_axis',(-0.48410980665131,-0.215539572760331,-0.848045038708632));
#136206=DIRECTION('ref_axis',(0.868458052949944,-6.20882257334192E-16,-0.495762655175228));
#136207=DIRECTION('center_axis',(-0.484110321456857,-0.215539774366594,
0.84804469358928));
#136208=DIRECTION('ref_axis',(0.772875576437733,0.349068641875244,0.529919264233161));
#136209=DIRECTION('center_axis',(-0.484110341087621,-0.215539810706668,
0.84804467314674));
#136210=DIRECTION('ref_axis',(-0.868457725299266,-4.18857327554064E-16,
-0.495763229140711));
#136211=DIRECTION('center_axis',(0.484109823426014,0.215539603977446,0.848045021198568));
#136212=DIRECTION('ref_axis',(-0.776473315749786,-0.340990855189784,0.529919264233215));
#136213=DIRECTION('center_axis',(-0.484109857923765,-0.215539595588298,
-0.848045003637581));
#136214=DIRECTION('ref_axis',(0.868458021515998,4.63801329176873E-17,-0.495762710240007));
#136215=DIRECTION('center_axis',(0.406972488803041,-0.913440415876952,-6.37852033235898E-15));
#136216=DIRECTION('ref_axis',(-0.913440415876952,-0.406972488803041,-3.41480999208023E-15));
#136217=DIRECTION('center_axis',(-0.913545457642598,-0.406736643075807,
-2.84022679824576E-15));
#136218=DIRECTION('ref_axis',(-0.406736643075807,0.913545457642598,6.82961998416061E-15));
#136219=DIRECTION('center_axis',(-2.69459552538469E-16,-7.04023807368299E-15,
1.));
#136220=DIRECTION('ref_axis',(-1.,2.13365834995709E-30,-2.70257145463201E-16));
#136221=DIRECTION('center_axis',(0.40650077023674,-0.913650438514062,-6.37998691259538E-15));
#136222=DIRECTION('ref_axis',(-0.913650438514062,-0.40650077023674,-3.41480999208026E-15));
#136223=DIRECTION('center_axis',(-0.913545457642598,-0.406736643075807,
-2.96886944389432E-15));
#136224=DIRECTION('ref_axis',(-0.406736643075807,0.913545457642598,6.8296199841606E-15));
#136225=DIRECTION('center_axis',(-0.791134794600364,-0.352268789801749,
0.500012436349588));
#136226=DIRECTION('ref_axis',(0.457186437802727,0.202469153671098,0.866017784402238));
#136227=DIRECTION('center_axis',(0.484110341087585,0.21553981070676,-0.848044673146738));
#136228=DIRECTION('ref_axis',(0.868457725299281,1.87917867469974E-15,0.495763229140685));
#136229=DIRECTION('center_axis',(0.456777309429339,0.203370349891571,-0.86602251147154));
#136230=DIRECTION('ref_axis',(0.792963725156868,0.34815015522809,0.499999999999999));
#136231=DIRECTION('center_axis',(-0.456777317573209,-0.203370364581889,
0.866022503726348));
#136232=DIRECTION('ref_axis',(-0.884507036382134,8.46452346853348E-16,-0.466526850878376));
#136233=DIRECTION('center_axis',(0.484110321308894,0.215539774221645,-0.848044693710586));
#136234=DIRECTION('ref_axis',(0.776563258034758,0.340785973398144,0.529919264233261));
#136235=DIRECTION('center_axis',(0.4841102814067,0.215539784135111,-0.848044713969326));
#136236=DIRECTION('ref_axis',(0.868457761888295,-2.69120973473327E-15,0.495763165045542));
#136237=DIRECTION('center_axis',(-0.913545457642598,-0.406736643075807,
-2.84022679824576E-15));
#136238=DIRECTION('ref_axis',(-0.406736643075807,0.913545457642598,6.82961998416061E-15));
#136239=DIRECTION('center_axis',(0.913545457642598,0.406736643075807,2.84022679824576E-15));
#136240=DIRECTION('ref_axis',(0.406736643075807,-0.913545457642598,-6.8296199841606E-15));
#136241=DIRECTION('center_axis',(-0.913545457642598,-0.406736643075807,
-2.96886944389432E-15));
#136242=DIRECTION('ref_axis',(-0.406736643075807,0.913545457642598,6.8296199841606E-15));
#136243=DIRECTION('center_axis',(-0.913545457642598,-0.406736643075807,
4.70731197133941E-14));
#136244=DIRECTION('ref_axis',(-0.406736643075807,0.913545457642598,6.82961998416061E-15));
#136245=DIRECTION('center_axis',(-0.913545457642598,-0.406736643075807,
-2.96886944389432E-15));
#136246=DIRECTION('ref_axis',(-0.406736643075807,0.913545457642598,6.8296199841606E-15));
#136247=DIRECTION('center_axis',(0.791150459692853,0.352280597671104,0.499979330205037));
#136248=DIRECTION('ref_axis',(0.456361522798632,0.204240445630384,-0.866036951219528));
#136249=DIRECTION('center_axis',(-0.456777441376069,-0.203370419702462,
-0.866022425483299));
#136250=DIRECTION('ref_axis',(0.884506966812061,-1.67212674088141E-15,-0.466526982779053));
#136251=DIRECTION('center_axis',(-0.456777449577965,-0.203370423354209,
-0.866022420299717));
#136252=DIRECTION('ref_axis',(0.406736643067868,-0.913545457646133,5.02660029630347E-12));
#136253=DIRECTION('center_axis',(0.43301704445322,0.250002507178805,-0.866022508724404));
#136254=DIRECTION('ref_axis',(-0.499999999998154,0.866025403785504,1.25883555838488E-12));
#136255=DIRECTION('center_axis',(0.750008802379566,0.432983094185441,-0.500012436348108));
#136256=DIRECTION('ref_axis',(0.432528431860175,0.250863215179282,0.866017784403121));
#136257=DIRECTION('center_axis',(-0.433017051950279,-0.250002511507204,
0.866022503726306));
#136258=DIRECTION('ref_axis',(-0.894424794863783,8.12848018235645E-16,-0.447218387740128));
#136259=DIRECTION('center_axis',(-0.86602540378444,-0.499999999999998,-3.49148133884312E-15));
#136260=DIRECTION('ref_axis',(-0.499999999999998,0.86602540378444,6.82961998416073E-15));
#136261=DIRECTION('center_axis',(0.866025403784435,0.500000000000007,3.61343235749219E-15));
#136262=DIRECTION('ref_axis',(0.500000000000007,-0.866025403784434,-6.82961998416066E-15));
#136263=DIRECTION('center_axis',(0.866025403784433,0.50000000000001,1.71507213071646E-14));
#136264=DIRECTION('ref_axis',(0.50000000000001,-0.866025403784433,-6.82961998416028E-15));
#136265=DIRECTION('center_axis',(0.866025403784435,0.500000000000007,3.61343235749219E-15));
#136266=DIRECTION('ref_axis',(0.500000000000007,-0.866025403784434,-6.82961998416066E-15));
#136267=DIRECTION('center_axis',(-0.866025403784433,-0.50000000000001,-3.4914813388432E-15));
#136268=DIRECTION('ref_axis',(-0.50000000000001,0.866025403784433,6.82961998416068E-15));
#136269=DIRECTION('center_axis',(0.458927830768604,0.264962106632857,0.848045003637603));
#136270=DIRECTION('ref_axis',(-0.879478602053345,-2.33963297980692E-15,
0.475938429348056));
#136271=DIRECTION('center_axis',(-0.433017169313214,-0.250002579266714,
-0.866022425483291));
#136272=DIRECTION('ref_axis',(0.894424730216418,1.24757342180764E-15,-0.447218517033103));
#136273=DIRECTION('center_axis',(-0.458927795481002,-0.264962111230046,
-0.848045021297492));
#136274=DIRECTION('ref_axis',(-0.73226696057136,-0.42775071227305,0.529919264233224));
#136275=DIRECTION('center_axis',(0.45892778216323,0.264962078570532,0.84804503870863));
#136276=DIRECTION('ref_axis',(-0.879478631391236,9.86399431822428E-16,0.475938375135058));
#136277=DIRECTION('center_axis',(-0.433017176052355,-0.250002595298109,
-0.866022417485745));
#136278=DIRECTION('ref_axis',(-0.74771537589394,-0.436945896710048,0.500000000000037));
#136279=DIRECTION('center_axis',(-0.750027562856189,-0.432988827019237,
-0.499979330205271));
#136280=DIRECTION('ref_axis',(0.433476564277263,0.249154705644953,-0.866036951219379));
#136281=DIRECTION('center_axis',(0.500209992837911,-0.865904130412309,-6.04657622512354E-15));
#136282=DIRECTION('ref_axis',(-0.865904130412309,-0.500209992837911,-3.41480999208024E-15));
#136283=DIRECTION('center_axis',(0.866025403784435,0.500000000000007,3.61343235749219E-15));
#136284=DIRECTION('ref_axis',(0.500000000000007,-0.866025403784434,-6.82961998416066E-15));
#136285=DIRECTION('center_axis',(-0.86602540378444,-0.499999999999998,-3.49148133884312E-15));
#136286=DIRECTION('ref_axis',(-0.499999999999998,0.86602540378444,6.82961998416073E-15));
#136287=DIRECTION('center_axis',(-2.6276792553892E-16,-7.05337113113122E-15,
1.));
#136288=DIRECTION('ref_axis',(-1.,2.00430111041611E-30,-2.60924281373677E-16));
#136289=DIRECTION('center_axis',(0.499789977759954,-0.866146626230631,-6.04826956437238E-15));
#136290=DIRECTION('ref_axis',(-0.866146626230631,-0.499789977759954,-3.41480999208016E-15));
#136291=DIRECTION('center_axis',(-0.458928232223265,-0.26496233841278,0.848044713969294));
#136292=DIRECTION('ref_axis',(-0.879478359737711,-6.74342126943788E-16,
-0.475938877118759));
#136293=DIRECTION('center_axis',(-0.458927782163224,-0.264962078570537,
-0.848045038708632));
#136294=DIRECTION('ref_axis',(0.879478631391239,-9.21361465146423E-16,-0.475938375135052));
#136295=DIRECTION('center_axis',(-0.45892827307447,-0.264962332885157,0.848044693589283));
#136296=DIRECTION('ref_axis',(0.732154074464099,0.427943903613708,0.529919264233223));
#136297=DIRECTION('center_axis',(-0.458928288799681,-0.264962371077198,
0.848044673146731));
#136298=DIRECTION('ref_axis',(-0.879478325588497,1.93561850010889E-15,-0.475938940222435));
#136299=DIRECTION('center_axis',(0.458927795581622,0.264962111372437,0.848045021198552));
#136300=DIRECTION('ref_axis',(-0.736576463604389,-0.420286434064426,0.529919264233204));
#136301=DIRECTION('center_axis',(-0.458927830768623,-0.264962106632877,
-0.848045003637587));
#136302=DIRECTION('ref_axis',(0.879478602053333,4.74704422624339E-16,-0.475938429348078));
#136303=DIRECTION('center_axis',(0.500223573885336,-0.865896284857131,-2.60257666760256E-14));
#136304=DIRECTION('ref_axis',(-0.865896284857131,-0.500223573885336,-3.41480999208053E-15));
#136305=DIRECTION('center_axis',(-0.866025403784433,-0.50000000000001,-3.4914813388432E-15));
#136306=DIRECTION('ref_axis',(-0.50000000000001,0.866025403784433,6.82961998416068E-15));
#136307=DIRECTION('center_axis',(-2.6276792553892E-16,-7.05337113113122E-15,
1.));
#136308=DIRECTION('ref_axis',(-1.,1.70692667996567E-30,-2.62750002533667E-16));
#136309=DIRECTION('center_axis',(0.499776392786197,-0.866154464985095,-2.40408495755615E-15));
#136310=DIRECTION('ref_axis',(-0.866154464985095,-0.499776392786197,-3.4148099920803E-15));
#136311=DIRECTION('center_axis',(-0.866025403784435,-0.500000000000007,
-3.61343235749219E-15));
#136312=DIRECTION('ref_axis',(-0.500000000000007,0.866025403784435,6.82961998416069E-15));
#136313=DIRECTION('center_axis',(-0.749978760162892,-0.43303512882955,0.500012436349444));
#136314=DIRECTION('ref_axis',(-0.433518133162554,-0.249149002241894,-0.866017784402331));
#136315=DIRECTION('center_axis',(0.458928288799652,0.264962371077227,-0.848044673146738));
#136316=DIRECTION('ref_axis',(0.87947832558851,-9.67081701894375E-18,0.47593894022241));
#136317=DIRECTION('center_axis',(0.433017045388799,0.250002496042169,-0.866022511471521));
#136318=DIRECTION('ref_axis',(0.752228186192834,0.42913023186094,0.500000000000015));
#136319=DIRECTION('center_axis',(-0.433017051950174,-0.250002511507144,
0.866022503726376));
#136320=DIRECTION('ref_axis',(-0.89442479486384,8.04235003406217E-16,-0.447218387740013));
#136321=DIRECTION('center_axis',(0.458928272945295,0.264962332720549,-0.848044693710617));
#136322=DIRECTION('ref_axis',(0.736687329162614,0.420092076152143,0.529919264233182));
#136323=DIRECTION('center_axis',(0.458928232223185,0.264962338412833,-0.84804471396932));
#136324=DIRECTION('ref_axis',(0.879478359737753,-7.9487078306857E-16,0.475938877118682));
#136325=DIRECTION('center_axis',(-0.866025403784433,-0.50000000000001,-3.4914813388432E-15));
#136326=DIRECTION('ref_axis',(-0.50000000000001,0.866025403784433,6.82961998416068E-15));
#136327=DIRECTION('center_axis',(0.866025403784433,0.50000000000001,3.4914813388432E-15));
#136328=DIRECTION('ref_axis',(0.50000000000001,-0.866025403784433,-6.82961998416068E-15));
#136329=DIRECTION('center_axis',(-0.866025403784435,-0.500000000000007,
-3.61343235749219E-15));
#136330=DIRECTION('ref_axis',(-0.500000000000007,0.866025403784435,6.82961998416069E-15));
#136331=DIRECTION('center_axis',(-0.866025403784433,-0.50000000000001,3.74862385661209E-14));
#136332=DIRECTION('ref_axis',(-0.50000000000001,0.866025403784433,6.82961998416068E-15));
#136333=DIRECTION('center_axis',(-0.866025403784435,-0.500000000000007,
-3.61343235749219E-15));
#136334=DIRECTION('ref_axis',(-0.500000000000007,0.866025403784435,6.82961998416069E-15));
#136335=DIRECTION('center_axis',(0.74999310518165,0.433048509462076,0.49997933020542));
#136336=DIRECTION('ref_axis',(-0.432512586705212,-0.25082436377741,0.866036951219302));
#136337=DIRECTION('center_axis',(-0.433017169313192,-0.250002579266702,
-0.866022425483305));
#136338=DIRECTION('ref_axis',(0.89442473021643,2.60762584234072E-15,-0.44721851703308));
#136339=DIRECTION('center_axis',(-0.433017177087641,-0.250002583755266,
-0.866022420300272));
#136340=DIRECTION('ref_axis',(0.500000000001662,-0.866025403783479,-1.11022302198922E-12));
#136341=DIRECTION('center_axis',(0.404512553890246,0.293895573513346,-0.866022508722754));
#136342=DIRECTION('ref_axis',(-0.587785252293392,0.80901699437428,-6.3815969278833E-13));
#136343=DIRECTION('center_axis',(0.7006411182289,0.509008435040742,-0.500012436349669));
#136344=DIRECTION('ref_axis',(0.403936649482838,0.294700492540559,0.866017784402221));
#136345=DIRECTION('center_axis',(-0.404512560891457,-0.293895578600025,
0.866022503726313));
#136346=DIRECTION('ref_axis',(-0.906035256115487,1.67656260149152E-15,-0.423202214875755));
#136347=DIRECTION('center_axis',(-0.80901699437495,-0.58778525229247,2.80103167643593E-14));
#136348=DIRECTION('ref_axis',(-0.58778525229247,0.80901699437495,6.82961998416043E-15));
#136349=DIRECTION('center_axis',(0.809016994374943,0.58778525229248,4.21840575002204E-15));
#136350=DIRECTION('ref_axis',(0.58778525229248,-0.809016994374943,-6.82961998416066E-15));
#136351=DIRECTION('center_axis',(0.809016994374931,0.587785252292496,4.83067115377211E-14));
#136352=DIRECTION('ref_axis',(0.587785252292496,-0.809016994374931,-6.82961998416074E-15));
#136353=DIRECTION('center_axis',(0.809016994374943,0.58778525229248,4.21840575002204E-15));
#136354=DIRECTION('ref_axis',(0.58778525229248,-0.809016994374943,-6.82961998416066E-15));
#136355=DIRECTION('center_axis',(-0.80901699437495,-0.58778525229247,-4.10448247925272E-15));
#136356=DIRECTION('ref_axis',(-0.58778525229247,0.80901699437495,6.82961998416043E-15));
#136357=DIRECTION('center_axis',(0.428717694262752,0.311481637390302,0.848045003637594));
#136358=DIRECTION('ref_axis',(-0.892442058026275,-9.10482188530049E-16,
0.451162025292274));
#136359=DIRECTION('center_axis',(-0.404512670528681,-0.293895658256099,
-0.866022425483295));
#136360=DIRECTION('ref_axis',(0.906035197473496,2.00150227313137E-15,-0.423202340422597));
#136361=DIRECTION('center_axis',(-0.428717658683062,-0.311481638280321,
-0.848045021297526));
#136362=DIRECTION('ref_axis',(-0.683543400924993,-0.501950189208491,0.529919264233199));
#136363=DIRECTION('center_axis',(0.428717648856917,0.311481604401031,0.848045038708651));
#136364=DIRECTION('ref_axis',(-0.892442084777737,-1.93926946889151E-15,
0.451161972375294));
#136365=DIRECTION('center_axis',(-0.404512675554545,-0.293895674904908,
-0.866022417485767));
#136366=DIRECTION('ref_axis',(-0.697946029716633,-0.512709800572198,0.500000000000006));
#136367=DIRECTION('center_axis',(-0.700659176690448,-0.509016097473817,
-0.499979330204749));
#136368=DIRECTION('ref_axis',(0.405058175797697,0.293100449234632,-0.866036951219692));
#136369=DIRECTION('center_axis',(0.587981418248444,-0.808874435122379,-5.64833999139414E-15));
#136370=DIRECTION('ref_axis',(-0.808874435122379,-0.587981418248444,-3.41480999208026E-15));
#136371=DIRECTION('center_axis',(0.809016994374943,0.58778525229248,4.21840575002204E-15));
#136372=DIRECTION('ref_axis',(0.58778525229248,-0.809016994374943,-6.82961998416066E-15));
#136373=DIRECTION('center_axis',(-0.809016994374912,-0.587785252292522,
-4.10448247925309E-15));
#136374=DIRECTION('ref_axis',(-0.587785252292522,0.809016994374912,6.82961998416056E-15));
#136375=DIRECTION('center_axis',(-2.54740177659162E-16,-7.0657327788296E-15,
1.));
#136376=DIRECTION('ref_axis',(-1.,2.00430111041611E-30,-2.53872273768983E-16));
#136377=DIRECTION('center_axis',(0.587589051772227,-0.809159506053914,-5.65033063106954E-15));
#136378=DIRECTION('ref_axis',(-0.809159506053914,-0.587589051772227,-3.41480999208049E-15));
#136379=DIRECTION('center_axis',(-0.428718069290599,-0.311481909863915,
0.848044713969298));
#136380=DIRECTION('ref_axis',(-0.892441837073364,8.23210690846008E-16,-0.451162462358205));
#136381=DIRECTION('center_axis',(-0.428717648856922,-0.311481604401035,
-0.848045038708647));
#136382=DIRECTION('ref_axis',(0.892442084777735,8.95023997870107E-16,-0.4511619723753));
#136383=DIRECTION('center_axis',(-0.428718110495355,-0.31148190863732,0.848044693589286));
#136384=DIRECTION('ref_axis',(0.683410939224747,0.502130522416714,0.529919264233211));
#136385=DIRECTION('center_axis',(-0.428718122142699,-0.311481948263271,
0.848044673146736));
#136386=DIRECTION('ref_axis',(-0.892441805934777,1.08348165947679E-15,-0.451162523953258));
#136387=DIRECTION('center_axis',(0.428717658780688,0.311481638415343,0.848045021198579));
#136388=DIRECTION('ref_axis',(-0.688609525569338,-0.494977266841255,0.529919264233272));
#136389=DIRECTION('center_axis',(-0.428717694262775,-0.311481637390318,
-0.848045003637576));
#136390=DIRECTION('ref_axis',(0.892442058026262,-8.62993040855731E-16,-0.4511620252923));
#136391=DIRECTION('center_axis',(0.587994104813606,-0.808865212939984,-5.64827559323867E-15));
#136392=DIRECTION('ref_axis',(-0.808865212939984,-0.587994104813606,-3.41480999208028E-15));
#136393=DIRECTION('center_axis',(-0.809016994374931,-0.587785252292496,
-4.1044824792529E-15));
#136394=DIRECTION('ref_axis',(-0.587785252292496,0.809016994374931,6.82961998416073E-15));
#136395=DIRECTION('center_axis',(-2.54740177659162E-16,-7.0657327788296E-15,
1.));
#136396=DIRECTION('ref_axis',(-1.,1.70692667996567E-30,-2.55242859604134E-16));
#136397=DIRECTION('center_axis',(0.587576360591375,-0.809168721883263,-1.77575279369932E-14));
#136398=DIRECTION('ref_axis',(-0.809168721883263,-0.587576360591375,-3.41480999208057E-15));
#136399=DIRECTION('center_axis',(-0.809016994374943,-0.58778525229248,-4.21840575002204E-15));
#136400=DIRECTION('ref_axis',(-0.58778525229248,0.809016994374943,6.8296199841606E-15));
#136401=DIRECTION('center_axis',(-0.70060580148539,-0.50905704436808,0.500012436349587));
#136402=DIRECTION('ref_axis',(-0.40510011312848,-0.29309912221343,-0.866017784402266));
#136403=DIRECTION('center_axis',(0.428718122142675,0.311481948263332,-0.848044673146726));
#136404=DIRECTION('ref_axis',(0.892441805934785,6.84549135789276E-16,0.451162523953242));
#136405=DIRECTION('center_axis',(0.404512555980279,0.293895562536812,-0.866022511471539));
#136406=DIRECTION('ref_axis',(0.703251077798178,0.505408667887383,0.500000000000001));
#136407=DIRECTION('center_axis',(-0.404512560891349,-0.293895578599947,
0.86602250372639));
#136408=DIRECTION('ref_axis',(-0.906035256115544,1.03179550260572E-15,-0.423202214875631));
#136409=DIRECTION('center_axis',(0.428718110387558,0.311481908455336,-0.848044693710623));
#136410=DIRECTION('ref_axis',(0.688740099740287,0.494795562231826,0.529919264233176));
#136411=DIRECTION('center_axis',(0.428718069290549,0.3114819098639,-0.848044713969329));
#136412=DIRECTION('ref_axis',(0.892441837073392,2.99591639139466E-15,0.451162462358151));
#136413=DIRECTION('center_axis',(-0.809016994374931,-0.587785252292496,
-4.1044824792529E-15));
#136414=DIRECTION('ref_axis',(-0.587785252292496,0.809016994374931,6.82961998416073E-15));
#136415=DIRECTION('center_axis',(0.809016994374931,0.587785252292496,4.1044824792529E-15));
#136416=DIRECTION('ref_axis',(0.587785252292496,-0.809016994374931,-6.82961998416073E-15));
#136417=DIRECTION('center_axis',(-0.809016994374943,-0.58778525229248,-4.21840575002204E-15));
#136418=DIRECTION('ref_axis',(-0.58778525229248,0.809016994374943,6.8296199841606E-15));
#136419=DIRECTION('center_axis',(-0.809016994374931,-0.587785252292496,
1.04327345066442E-13));
#136420=DIRECTION('ref_axis',(-0.587785252292496,0.809016994374931,6.82961998416073E-15));
#136421=DIRECTION('center_axis',(-0.809016994374943,-0.58778525229248,-4.21840575002204E-15));
#136422=DIRECTION('ref_axis',(-0.58778525229248,0.809016994374943,6.8296199841606E-15));
#136423=DIRECTION('center_axis',(0.700618669264079,0.509071851162291,0.499979330205589));
#136424=DIRECTION('ref_axis',(-0.403924952195115,-0.294660197714492,0.866036951219191));
#136425=DIRECTION('center_axis',(-0.404512670528659,-0.293895658256103,
-0.866022425483304));
#136426=DIRECTION('ref_axis',(0.906035197473506,2.60041954384793E-15,-0.423202340422576));
#136427=DIRECTION('center_axis',(-0.404512677788203,-0.293895663530555,
-0.866022420302472));
#136428=DIRECTION('ref_axis',(0.587785252293442,-0.809016994374244,-6.11933949130544E-13));
#136429=DIRECTION('center_axis',(0.371576139138171,0.334568658444613,-0.866022508720035));
#136430=DIRECTION('ref_axis',(-0.669130606363659,0.743144825473072,-3.70220040960197E-12));
#136431=DIRECTION('center_axis',(0.643597063368372,0.579456972966985,-0.500012436348884));
#136432=DIRECTION('ref_axis',(0.370919252678232,0.335308969594947,0.866017784402721));
#136433=DIRECTION('center_axis',(-0.37157614556582,-0.334568664232125,0.866022503726307));
#136434=DIRECTION('ref_axis',(-0.918982183096524,-2.90533283465756E-16,
-0.394299058014532));
#136435=DIRECTION('center_axis',(-0.743144825477379,-0.669130606358875,
-4.67251405070161E-15));
#136436=DIRECTION('ref_axis',(-0.669130606358875,0.743144825477379,6.82961998416085E-15));
#136437=DIRECTION('center_axis',(0.743144825477389,0.669130606358864,4.7771614063965E-15));
#136438=DIRECTION('ref_axis',(0.669130606358864,-0.743144825477389,-6.82961998416066E-15));
#136439=DIRECTION('center_axis',(0.743144825477406,0.669130606358845,-3.59306599589465E-14));
#136440=DIRECTION('ref_axis',(0.669130606358845,-0.743144825477406,-6.82961998416065E-15));
#136441=DIRECTION('center_axis',(0.743144825477389,0.669130606358864,4.7771614063965E-15));
#136442=DIRECTION('ref_axis',(0.669130606358864,-0.743144825477389,-6.82961998416066E-15));
#136443=DIRECTION('center_axis',(-0.743144825477382,-0.669130606358872,
-4.67251405070159E-15));
#136444=DIRECTION('ref_axis',(-0.669130606358872,0.743144825477382,6.82961998416048E-15));
#136445=DIRECTION('center_axis',(0.393810436983645,0.354588510146755,0.848045003637575));
#136446=DIRECTION('ref_axis',(-0.90697822335776,-4.43466984905637E-15,0.421177518814575));
#136447=DIRECTION('center_axis',(-0.371576246276111,-0.33456875491203,-0.866022425483295));
#136448=DIRECTION('ref_axis',(0.918982131463648,-8.42496017976876E-16,-0.394299178353862));
#136449=DIRECTION('center_axis',(-0.393810401512578,-0.354588507305327,
-0.848045021297503));
#136450=DIRECTION('ref_axis',(-0.627330796743312,-0.570650194823359,0.529919264233208));
#136451=DIRECTION('center_axis',(0.393810395274833,0.354588472591972,0.84804503870866));
#136452=DIRECTION('ref_axis',(-0.906978247051303,2.81492198842025E-15,0.421177467792077));
#136453=DIRECTION('center_axis',(-0.371576249533521,-0.334568771995624,
-0.866022417485796));
#136454=DIRECTION('ref_axis',(-0.640529840772685,-0.582856348579827,0.499999999999909));
#136455=DIRECTION('center_axis',(-0.643614221961003,-0.579466481046856,
-0.499979330205465));
#136456=DIRECTION('ref_axis',(0.372201885192739,0.33383492295115,-0.866036951219271));
#136457=DIRECTION('center_axis',(0.669310796197597,-0.742982542253409,-5.18821936272801E-15));
#136458=DIRECTION('ref_axis',(-0.742982542253409,-0.669310796197597,-3.41480999208022E-15));
#136459=DIRECTION('center_axis',(0.743144825477389,0.669130606358864,4.7771614063965E-15));
#136460=DIRECTION('ref_axis',(0.669130606358864,-0.743144825477389,-6.82961998416066E-15));
#136461=DIRECTION('center_axis',(-0.743144825477379,-0.669130606358875,
-4.67251405070161E-15));
#136462=DIRECTION('ref_axis',(-0.669130606358875,0.743144825477379,6.82961998416085E-15));
#136463=DIRECTION('center_axis',(-2.45464262584879E-16,-7.07718757997909E-15,
1.));
#136464=DIRECTION('ref_axis',(-1.,1.60344088833289E-30,-2.46820266164289E-16));
#136465=DIRECTION('center_axis',(0.668950377172438,-0.743307065001304,-5.19048549296463E-15));
#136466=DIRECTION('ref_axis',(-0.743307065001304,-0.668950377172438,-3.41480999208024E-15));
#136467=DIRECTION('center_axis',(-0.39381078147567,-0.354588820328842,0.84804471396933));
#136468=DIRECTION('ref_axis',(-0.906978027661858,9.58633533089459E-18,-0.421177940232637));
#136469=DIRECTION('center_axis',(-0.393810395274846,-0.354588472591984,
-0.848045038708649));
#136470=DIRECTION('ref_axis',(0.906978247051294,3.98971491588805E-15,-0.421177467792096));
#136471=DIRECTION('center_axis',(-0.393810822585816,-0.354588823412929,
0.848044693589269));
#136472=DIRECTION('ref_axis',(0.627180210728517,0.570815694129948,0.529919264233221));
#136473=DIRECTION('center_axis',(-0.393810830024562,-0.354588864042309,
0.848044673146734));
#136474=DIRECTION('ref_axis',(-0.906978000082632,3.09313791198912E-15,-0.421177999622617));
#136475=DIRECTION('center_axis',(0.393810401584693,0.354588507461832,0.848045021198576));
#136476=DIRECTION('ref_axis',(-0.633098037503341,-0.564245025059131,0.529919264233184));
#136477=DIRECTION('center_axis',(-0.393810436983627,-0.354588510146739,
-0.84804500363759));
#136478=DIRECTION('ref_axis',(0.906978223357771,-2.42620968147434E-15,-0.421177518814551));
#136479=DIRECTION('center_axis',(0.669322449283885,-0.742972044483923,-9.21213603482361E-15));
#136480=DIRECTION('ref_axis',(-0.742972044483923,-0.669322449283885,-3.41480999208054E-15));
#136481=DIRECTION('center_axis',(-0.743144825477406,-0.669130606358845,
-4.6725140507014E-15));
#136482=DIRECTION('ref_axis',(-0.669130606358845,0.743144825477406,6.82961998416065E-15));
#136483=DIRECTION('center_axis',(-2.45464262584879E-16,-7.07718757997909E-15,
1.));
#136484=DIRECTION('ref_axis',(-1.,1.70692667996567E-30,-2.477357166746E-16));
#136485=DIRECTION('center_axis',(0.668938718831625,-0.743317556935059,-5.19055875774645E-15));
#136486=DIRECTION('ref_axis',(-0.743317556935059,-0.668938718831625,-3.41480999208048E-15));
#136487=DIRECTION('center_axis',(-0.743144825477389,-0.669130606358864,
-4.7771614063965E-15));
#136488=DIRECTION('ref_axis',(-0.669130606358865,0.743144825477389,6.82961998416053E-15));
#136489=DIRECTION('center_axis',(-0.643556859036855,-0.579501624400643,
0.500012436348971));
#136490=DIRECTION('ref_axis',(-0.372243731528579,-0.333837986808177,-0.866017784402574));
#136491=DIRECTION('center_axis',(0.393810830024499,0.354588864042367,-0.848044673146739));
#136492=DIRECTION('ref_axis',(0.906978000082658,2.87858588363672E-16,0.421177999622561));
#136493=DIRECTION('center_axis',(0.371576142364791,0.334568647738853,-0.866022511471553));
#136494=DIRECTION('ref_axis',(0.646569003435637,0.576149740776005,0.499999999999988));
#136495=DIRECTION('center_axis',(-0.371576145565792,-0.334568664232036,
0.866022503726353));
#136496=DIRECTION('ref_axis',(-0.918982183096542,-3.10377123333878E-15,
-0.39429905801449));
#136497=DIRECTION('center_axis',(0.393810822485845,0.354588823233822,-0.848044693710583));
#136498=DIRECTION('ref_axis',(0.633246889646911,0.564077964599757,0.529919264233249));
#136499=DIRECTION('center_axis',(0.393810781475714,0.354588820328819,-0.848044713969319));
#136500=DIRECTION('ref_axis',(0.906978027661838,-3.63667371350487E-15,0.421177940232679));
#136501=DIRECTION('center_axis',(-0.743144825477406,-0.669130606358845,
-4.52756880603493E-14));
#136502=DIRECTION('ref_axis',(-0.669130606358845,0.743144825477406,6.82961998416065E-15));
#136503=DIRECTION('center_axis',(0.743144825477379,0.669130606358875,4.67251405070161E-15));
#136504=DIRECTION('ref_axis',(0.669130606358875,-0.743144825477379,-6.82961998416085E-15));
#136505=DIRECTION('center_axis',(-0.743144825477389,-0.669130606358864,
-4.7771614063965E-15));
#136506=DIRECTION('ref_axis',(-0.669130606358865,0.743144825477389,6.82961998416075E-15));
#136507=DIRECTION('center_axis',(-0.743144825477406,-0.669130606358845,
-4.52756880603471E-14));
#136508=DIRECTION('ref_axis',(-0.669130606358845,0.743144825477406,6.82961998416065E-15));
#136509=DIRECTION('center_axis',(-0.743144825477389,-0.669130606358864,
-4.7771614063965E-15));
#136510=DIRECTION('ref_axis',(-0.669130606358865,0.743144825477389,6.82961998416075E-15));
#136511=DIRECTION('center_axis',(0.643568108592016,0.579517695131662,0.499979330205341));
#136512=DIRECTION('ref_axis',(-0.37091183139934,-0.335267672838718,0.866036951219345));
#136513=DIRECTION('center_axis',(-0.37157624627613,-0.33456875491202,-0.866022425483291));
#136514=DIRECTION('ref_axis',(0.91898213146364,-2.37633339499038E-15,-0.39429917835388));
#136515=DIRECTION('center_axis',(-0.371576252942618,-0.334568760914637,
-0.866022420303983));
#136516=DIRECTION('ref_axis',(0.669130606365272,-0.743144825471619,-4.92606829050724E-12));
#136517=DIRECTION('center_axis',(0.334568658444856,0.371576139138533,-0.866022508719786));
#136518=DIRECTION('ref_axis',(-0.743144825477019,0.669130606359275,3.84644198394791E-13));
#136519=DIRECTION('center_axis',(0.579501624400154,0.643556859037784,-0.500012436348342));
#136520=DIRECTION('ref_axis',(0.333837986840269,0.372243731498863,0.866017784402976));
#136521=DIRECTION('center_axis',(-0.3345686642321,-0.371576145565845,0.866022503726305));
#136522=DIRECTION('ref_axis',(-2.10155353069294E-16,-0.918982183096514,
-0.394299058014555));
#136523=DIRECTION('center_axis',(-0.669130606358875,-0.743144825477379,
-5.18935258042421E-15));
#136524=DIRECTION('ref_axis',(-0.743144825477379,0.669130606358875,3.41480999208015E-15));
#136525=DIRECTION('center_axis',(0.669130606358852,0.7431448254774,5.28357748271718E-15));
#136526=DIRECTION('ref_axis',(0.7431448254774,-0.669130606358852,-3.41480999208033E-15));
#136527=DIRECTION('center_axis',(0.669130606358845,0.743144825477406,4.1748614670039E-14));
#136528=DIRECTION('ref_axis',(0.743144825477406,-0.669130606358845,-3.41480999208033E-15));
#136529=DIRECTION('center_axis',(0.669130606358852,0.7431448254774,5.28357748271718E-15));
#136530=DIRECTION('ref_axis',(0.7431448254774,-0.669130606358852,-3.41480999208033E-15));
#136531=DIRECTION('center_axis',(-0.669130606358845,-0.743144825477406,
-5.1893525804244E-15));
#136532=DIRECTION('ref_axis',(-0.743144825477406,0.669130606358845,3.41480999208033E-15));
#136533=DIRECTION('center_axis',(0.354588510146745,0.393810436983621,0.848045003637591));
#136534=DIRECTION('ref_axis',(2.48577593066859E-15,-0.906978223357774,0.421177518814545));
#136535=DIRECTION('center_axis',(-0.334568754912041,-0.371576246276141,
-0.866022425483277));
#136536=DIRECTION('ref_axis',(-3.67049197560442E-15,0.918982131463634,-0.394299178353895));
#136537=DIRECTION('center_axis',(-0.354588475162944,-0.393810430453691,
-0.848045021297511));
#136538=DIRECTION('ref_axis',(-0.564245025068804,-0.633098037494702,0.529919264233205));
#136539=DIRECTION('center_axis',(0.354588472592002,0.393810395274854,0.848045038708637));
#136540=DIRECTION('ref_axis',(-2.96450180524908E-15,-0.906978247051289,
0.421177467792107));
#136541=DIRECTION('center_axis',(-0.334568756368592,-0.371576263604271,
-0.86602241748575));
#136542=DIRECTION('ref_axis',(-0.57609587287649,-0.646617000437385,0.500000000000034));
#136543=DIRECTION('center_axis',(-0.579517695132434,-0.643568108591643,
-0.499979330204926));
#136544=DIRECTION('ref_axis',(0.335267672834376,0.370911831402694,-0.86603695121959));
#136545=DIRECTION('center_axis',(0.743307065001336,-0.668950377172403,-4.67125551701904E-15));
#136546=DIRECTION('ref_axis',(-0.668950377172402,-0.743307065001336,-6.82961998416069E-15));
#136547=DIRECTION('center_axis',(0.669130606358852,0.7431448254774,5.28357748271718E-15));
#136548=DIRECTION('ref_axis',(0.7431448254774,-0.669130606358852,-3.41480999208033E-15));
#136549=DIRECTION('center_axis',(-0.669130606358872,-0.743144825477382,
-5.18935258042423E-15));
#136550=DIRECTION('ref_axis',(-0.743144825477382,0.669130606358872,3.41480999208052E-15));
#136551=DIRECTION('center_axis',(-2.35041809182734E-16,-7.08761003338124E-15,
1.));
#136552=DIRECTION('ref_axis',(-1.,1.60344088833289E-30,-2.32716250954901E-16));
#136553=DIRECTION('center_axis',(0.742982542253406,-0.669310796197601,-4.67377230962033E-15));
#136554=DIRECTION('ref_axis',(-0.669310796197601,-0.742982542253406,-6.82961998416052E-15));
#136555=DIRECTION('center_axis',(-0.35458882032884,-0.393810781475749,0.848044713969294));
#136556=DIRECTION('ref_axis',(-2.33925611613224E-15,-0.906978027661818,
-0.421177940232722));
#136557=DIRECTION('center_axis',(-0.354588472592004,-0.393810395274856,
-0.848045038708635));
#136558=DIRECTION('ref_axis',(1.94126359720515E-15,0.906978247051288,-0.421177467792109));
#136559=DIRECTION('center_axis',(-0.354588860888781,-0.393810788842403,
0.848044693589271));
#136560=DIRECTION('ref_axis',(0.564077964581017,0.63324688966366,0.529919264233183));
#136561=DIRECTION('center_axis',(-0.354588864042363,-0.393810830024504,
0.848044673146738));
#136562=DIRECTION('ref_axis',(-8.09796269128675E-16,-0.906978000082656,
-0.421177999622565));
#136563=DIRECTION('center_axis',(0.354588475230927,0.393810430605494,0.848045021198593));
#136564=DIRECTION('ref_axis',(-0.570650194812903,-0.627330796752771,0.529919264233269));
#136565=DIRECTION('center_axis',(-0.354588510146774,-0.393810436983654,
-0.848045003637564));
#136566=DIRECTION('ref_axis',(3.03817507168769E-15,0.906978223357754,-0.421177518814587));
#136567=DIRECTION('center_axis',(0.743317556935089,-0.668938718831591,-6.07340514377938E-16));
#136568=DIRECTION('ref_axis',(-0.668938718831591,-0.743317556935089,-6.82961998416058E-15));
#136569=DIRECTION('center_axis',(-0.669130606358845,-0.743144825477406,
-5.1893525804244E-15));
#136570=DIRECTION('ref_axis',(-0.743144825477406,0.669130606358845,3.41480999208033E-15));
#136571=DIRECTION('center_axis',(-2.35041809182734E-16,-7.08761003338124E-15,
1.));
#136572=DIRECTION('ref_axis',(-1.,1.70692667996567E-30,-2.32721430815534E-16));
#136573=DIRECTION('center_axis',(0.742972044483923,-0.669322449283885,-6.49863705058595E-16));
#136574=DIRECTION('ref_axis',(-0.669322449283885,-0.742972044483923,-6.82961998416067E-15));
#136575=DIRECTION('center_axis',(-0.669130606358852,-0.7431448254774,-5.28357748271718E-15));
#136576=DIRECTION('ref_axis',(-0.7431448254774,0.669130606358852,3.41480999208037E-15));
#136577=DIRECTION('center_axis',(-0.5794569729669,-0.64359706336836,0.500012436348998));
#136578=DIRECTION('ref_axis',(-0.335308969632734,-0.370919252644328,-0.866017784402611));
#136579=DIRECTION('center_axis',(0.354588864042318,0.393810830024554,-0.848044673146734));
#136580=DIRECTION('ref_axis',(-1.8846300391506E-15,0.906978000082635,0.421177999622611));
#136581=DIRECTION('center_axis',(0.334568662774178,0.371576128826869,-0.866022511471576));
#136582=DIRECTION('ref_axis',(0.582802983776954,0.640578396529848,0.499999999999928));
#136583=DIRECTION('center_axis',(-0.334568664232029,-0.371576145565797,
0.866022503726353));
#136584=DIRECTION('ref_axis',(-2.68749946785539E-15,-0.91898218309654,-0.394299058014494));
#136585=DIRECTION('center_axis',(0.354588860816318,0.393810788646376,-0.8480446937106));
#136586=DIRECTION('ref_axis',(0.5708156941274,0.627180210730821,0.52991926423324));
#136587=DIRECTION('center_axis',(0.354588820328778,0.39381078147575,-0.848044713969319));
#136588=DIRECTION('ref_axis',(2.773318553842E-15,0.906978027661822,0.421177940232713));
#136589=DIRECTION('center_axis',(-0.669130606358845,-0.743144825477406,
3.54138214292235E-14));
#136590=DIRECTION('ref_axis',(-0.743144825477406,0.669130606358845,3.41480999208033E-15));
#136591=DIRECTION('center_axis',(0.669130606358872,0.743144825477382,5.18935258042423E-15));
#136592=DIRECTION('ref_axis',(0.743144825477382,-0.669130606358872,-3.41480999208052E-15));
#136593=DIRECTION('center_axis',(-0.669130606358852,-0.7431448254774,-5.28357748271718E-15));
#136594=DIRECTION('ref_axis',(-0.7431448254774,0.669130606358852,3.41480999208037E-15));
#136595=DIRECTION('center_axis',(-0.669130606358845,-0.743144825477406,
3.13699095091902E-14));
#136596=DIRECTION('ref_axis',(-0.743144825477406,0.669130606358845,3.41480999208033E-15));
#136597=DIRECTION('center_axis',(-0.669130606358852,-0.7431448254774,-5.28357748271718E-15));
#136598=DIRECTION('ref_axis',(-0.7431448254774,0.669130606358852,3.41480999208037E-15));
#136599=DIRECTION('center_axis',(0.579466481046767,0.643614221961237,0.499979330205268));
#136600=DIRECTION('ref_axis',(-0.333834922934168,-0.372201885207748,0.866036951219367));
#136601=DIRECTION('center_axis',(-0.334568754912033,-0.371576246276132,
-0.866022425483285));
#136602=DIRECTION('ref_axis',(-2.55402912997765E-15,0.918982131463639,-0.394299178353883));
#136603=DIRECTION('center_axis',(-0.334568760920321,-0.371576252949017,
-0.866022420299042));
#136604=DIRECTION('ref_axis',(0.743144825474438,-0.669130606362141,2.55700971598187E-12));
#136605=DIRECTION('center_axis',(0.29389557351548,0.404512553893185,-0.866022508720657));
#136606=DIRECTION('ref_axis',(-0.809016994376333,0.587785252290566,-1.38996426237733E-12));
#136607=DIRECTION('center_axis',(0.509057044367788,0.700605801485607,-0.500012436349579));
#136608=DIRECTION('ref_axis',(0.293099122190702,0.405100113144966,0.866017784402246));
#136609=DIRECTION('center_axis',(-0.293895578600024,-0.40451256089147,0.866022503726307));
#136610=DIRECTION('ref_axis',(2.32982689944053E-15,-0.90603525611548,-0.423202214875768));
#136611=DIRECTION('center_axis',(-0.58778525229247,-0.80901699437495,-5.6493354773342E-15));
#136612=DIRECTION('ref_axis',(-0.80901699437495,0.58778525229247,3.41480999208022E-15));
#136613=DIRECTION('center_axis',(0.587785252292466,0.809016994374953,5.73210557847754E-15));
#136614=DIRECTION('ref_axis',(0.809016994374953,-0.587785252292466,-3.41480999208033E-15));
#136615=DIRECTION('center_axis',(0.58778525229247,0.80901699437495,5.6493354773342E-15));
#136616=DIRECTION('ref_axis',(0.80901699437495,-0.58778525229247,-3.41480999208022E-15));
#136617=DIRECTION('center_axis',(0.587785252292466,0.809016994374953,5.73210557847754E-15));
#136618=DIRECTION('ref_axis',(0.809016994374953,-0.587785252292466,-3.41480999208033E-15));
#136619=DIRECTION('center_axis',(-0.58778525229247,-0.80901699437495,-5.6493354773342E-15));
#136620=DIRECTION('ref_axis',(-0.80901699437495,0.58778525229247,3.41480999208022E-15));
#136621=DIRECTION('center_axis',(0.311481637390299,0.428717694262763,0.848045003637589));
#136622=DIRECTION('ref_axis',(1.51664064046204E-16,-0.89244205802627,0.451162025292284));
#136623=DIRECTION('center_axis',(-0.293895658256123,-0.404512670528727,
-0.866022425483265));
#136624=DIRECTION('ref_axis',(-1.09162433120364E-15,0.906035197473472,-0.423202340422648));
#136625=DIRECTION('center_axis',(-0.311481603281241,-0.4287176841114,-0.848045021297516));
#136626=DIRECTION('ref_axis',(-0.494977266824932,-0.68860952558114,0.529919264233183));
#136627=DIRECTION('center_axis',(0.311481604401019,0.428717648856915,0.848045038708656));
#136628=DIRECTION('ref_axis',(-1.55513761614889E-15,-0.89244208477774,0.45116197237529));
#136629=DIRECTION('center_axis',(-0.293895657890896,-0.404512687915994,
-0.866022417485746));
#136630=DIRECTION('ref_axis',(-0.505350078025385,-0.703293181141193,0.500000000000038));
#136631=DIRECTION('center_axis',(-0.509071851163456,-0.700618669263731,
-0.49997933020489));
#136632=DIRECTION('ref_axis',(0.294660197697665,0.403924952206488,-0.866036951219611));
#136633=DIRECTION('center_axis',(0.809159506053914,-0.587589051772227,-4.10311241834253E-15));
#136634=DIRECTION('ref_axis',(-0.587589051772227,-0.809159506053914,-6.82961998416088E-15));
#136635=DIRECTION('center_axis',(0.587785252292466,0.809016994374953,5.73210557847754E-15));
#136636=DIRECTION('ref_axis',(0.809016994374953,-0.587785252292466,-3.41480999208033E-15));
#136637=DIRECTION('center_axis',(-0.58778525229247,-0.80901699437495,-5.6493354773342E-15));
#136638=DIRECTION('ref_axis',(-0.80901699437495,0.58778525229247,3.41480999208022E-15));
#136639=DIRECTION('center_axis',(-2.23587008033241E-16,-7.09688594845552E-15,
1.));
#136640=DIRECTION('ref_axis',(-1.,1.60344088833289E-30,-2.25664243350207E-16));
#136641=DIRECTION('center_axis',(0.808874435122379,-0.587981418248444,-4.10585229880193E-15));
#136642=DIRECTION('ref_axis',(-0.587981418248444,-0.808874435122379,-6.82961998416087E-15));
#136643=DIRECTION('center_axis',(-0.311481909863932,-0.428718069290528,
0.848044713969328));
#136644=DIRECTION('ref_axis',(3.08013998868981E-15,-0.892441837073401,-0.451162462358132));
#136645=DIRECTION('center_axis',(-0.311481604401018,-0.428717648856992,
-0.848045038708618));
#136646=DIRECTION('ref_axis',(3.62313198634112E-15,0.892442084777698,-0.451161972375371));
#136647=DIRECTION('center_axis',(-0.311481949432504,-0.428718080855936,
0.848044693589277));
#136648=DIRECTION('ref_axis',(0.494795562236623,0.688740099736818,0.529919264233205));
#136649=DIRECTION('center_axis',(-0.311481948263276,-0.428718122142692,
0.848044673146738));
#136650=DIRECTION('ref_axis',(-3.57201939485921E-16,-0.892441805934781,
-0.451162523953251));
#136651=DIRECTION('center_axis',(0.311481603328271,0.428717684272931,0.848045021198583));
#136652=DIRECTION('ref_axis',(-0.501950189201534,-0.683543400930078,0.52991926423323));
#136653=DIRECTION('center_axis',(-0.311481637390294,-0.428717694262756,
-0.848045003637594));
#136654=DIRECTION('ref_axis',(7.82282120695661E-16,0.892442058026274,-0.451162025292277));
#136655=DIRECTION('center_axis',(0.809168721883286,-0.587576360591345,8.00410915583402E-15));
#136656=DIRECTION('ref_axis',(-0.587576360591345,-0.809168721883286,-6.82961998416048E-15));
#136657=DIRECTION('center_axis',(-0.58778525229247,-0.80901699437495,-5.6493354773342E-15));
#136658=DIRECTION('ref_axis',(-0.80901699437495,0.58778525229247,3.41480999208022E-15));
#136659=DIRECTION('center_axis',(-2.23587008033241E-16,-7.09688594845552E-15,
1.));
#136660=DIRECTION('ref_axis',(-1.,1.70692667996567E-30,-2.25214287886E-16));
#136661=DIRECTION('center_axis',(0.808865212939984,-0.587994104813606,-4.10594088861296E-15));
#136662=DIRECTION('ref_axis',(-0.587994104813606,-0.808865212939984,-6.82961998416048E-15));
#136663=DIRECTION('center_axis',(-0.587785252292466,-0.809016994374953,
-5.73210557847754E-15));
#136664=DIRECTION('ref_axis',(-0.809016994374953,0.587785252292466,3.41480999208036E-15));
#136665=DIRECTION('center_axis',(-0.509008435042705,-0.700641118228387,
0.50001243634839));
#136666=DIRECTION('ref_axis',(-0.294700492572351,-0.403936649458133,-0.866017784402925));
#136667=DIRECTION('center_axis',(0.31148194826325,0.428718122142734,-0.848044673146726));
#136668=DIRECTION('ref_axis',(-2.26428405615115E-15,0.89244180593476,0.451162523953291));
#136669=DIRECTION('center_axis',(0.293895578898316,0.404512544092887,-0.866022511471569));
#136670=DIRECTION('ref_axis',(0.512651652655376,0.697988741334513,0.499999999999974));
#136671=DIRECTION('center_axis',(-0.293895578599974,-0.404512560891429,
0.866022503726344));
#136672=DIRECTION('ref_axis',(-1.18885620953251E-15,-0.906035256115503,
-0.423202214875719));
#136673=DIRECTION('center_axis',(0.311481949380855,0.428718080653442,-0.848044693710615));
#136674=DIRECTION('ref_axis',(0.502130522406322,0.683410939232379,0.529919264233214));
#136675=DIRECTION('center_axis',(0.311481909863867,0.428718069290587,-0.848044713969322));
#136676=DIRECTION('ref_axis',(1.35835357911667E-15,0.892441837073374,0.451162462358185));
#136677=DIRECTION('center_axis',(-0.58778525229247,-0.80901699437495,-5.6493354773342E-15));
#136678=DIRECTION('ref_axis',(-0.80901699437495,0.58778525229247,3.41480999208022E-15));
#136679=DIRECTION('center_axis',(0.587785252292496,0.809016994374931,5.64933547733406E-15));
#136680=DIRECTION('ref_axis',(0.809016994374931,-0.587785252292496,-3.41480999208037E-15));
#136681=DIRECTION('center_axis',(-0.587785252292466,-0.809016994374953,
-5.73210557847754E-15));
#136682=DIRECTION('ref_axis',(-0.809016994374953,0.587785252292466,3.41480999208036E-15));
#136683=DIRECTION('center_axis',(-0.58778525229247,-0.80901699437495,-1.77367652921915E-14));
#136684=DIRECTION('ref_axis',(-0.80901699437495,0.58778525229247,3.41480999208022E-15));
#136685=DIRECTION('center_axis',(-0.587785252292466,-0.809016994374953,
-5.73210557847754E-15));
#136686=DIRECTION('ref_axis',(-0.809016994374953,0.587785252292466,3.41480999208036E-15));
#136687=DIRECTION('center_axis',(0.509016097474163,0.70065917669004,0.499979330204968));
#136688=DIRECTION('ref_axis',(-0.293100449223401,-0.405058175806119,0.866036951219553));
#136689=DIRECTION('center_axis',(-0.293895658256093,-0.404512670528659,
-0.866022425483307));
#136690=DIRECTION('ref_axis',(3.08674820555281E-15,0.906035197473506,-0.423202340422574));
#136691=DIRECTION('center_axis',(-0.293895663531409,-0.404512677789524,
-0.866022420301566));
#136692=DIRECTION('ref_axis',(0.809016994376599,-0.5877852522902,-1.62599592197905E-12));
#136693=DIRECTION('center_axis',(0.250002507179564,0.433017044454593,-0.866022508723498));
#136694=DIRECTION('ref_axis',(-0.866025403783392,0.500000000001813,1.20201311999016E-12));
#136695=DIRECTION('center_axis',(0.433035128830174,0.749978760162262,-0.500012436349849));
#136696=DIRECTION('ref_axis',(0.249149002239919,0.433518133164162,0.866017784402095));
#136697=DIRECTION('center_axis',(-0.25000251150716,-0.433017051950299,0.866022503726309));
#136698=DIRECTION('ref_axis',(1.53376353322716E-15,-0.894424794863775,-0.447218387740144));
#136699=DIRECTION('center_axis',(-0.500000000000022,-0.866025403784426,
-6.04742307255483E-15));
#136700=DIRECTION('ref_axis',(-0.866025403784426,0.500000000000022,3.41480999208042E-15));
#136701=DIRECTION('center_axis',(0.499999999999992,0.866025403784443,6.1178315259999E-15));
#136702=DIRECTION('ref_axis',(0.866025403784443,-0.499999999999992,-3.41480999208033E-15));
#136703=DIRECTION('center_axis',(0.50000000000001,0.866025403784433,-7.61181689576648E-15));
#136704=DIRECTION('ref_axis',(0.866025403784433,-0.50000000000001,-3.41480999208034E-15));
#136705=DIRECTION('center_axis',(0.499999999999992,0.866025403784443,6.1178315259999E-15));
#136706=DIRECTION('ref_axis',(0.866025403784443,-0.499999999999992,-3.41480999208033E-15));
#136707=DIRECTION('center_axis',(-0.50000000000001,-0.866025403784433,-6.04742307255487E-15));
#136708=DIRECTION('ref_axis',(-0.866025403784433,0.50000000000001,3.41480999208034E-15));
#136709=DIRECTION('center_axis',(0.264962106632875,0.458927830768604,0.848045003637597));
#136710=DIRECTION('ref_axis',(-1.67218023172745E-15,-0.879478602053344,
0.475938429348058));
#136711=DIRECTION('center_axis',(-0.25000257926675,-0.433017169313239,-0.866022425483268));
#136712=DIRECTION('ref_axis',(-1.10825904974603E-15,0.894424730216403,-0.447218517033133));
#136713=DIRECTION('center_axis',(-0.264962073768116,-0.458927817109621,
-0.848045021297512));
#136714=DIRECTION('ref_axis',(-0.420286434051416,-0.736576463611834,0.529919264233175));
#136715=DIRECTION('center_axis',(0.264962078570529,0.458927782163195,0.84804503870865));
#136716=DIRECTION('ref_axis',(-1.38504843431592E-15,-0.879478631391255,
0.475938375135021));
#136717=DIRECTION('center_axis',(-0.250002577085399,-0.433017186567401,
-0.866022417485778));
#136718=DIRECTION('ref_axis',(-0.4290675619629,-0.752263934580973,0.499999999999966));
#136719=DIRECTION('center_axis',(-0.433048509462545,-0.749993105181572,
-0.499979330205131));
#136720=DIRECTION('ref_axis',(0.250824363776163,0.432512586705598,-0.866036951219471));
#136721=DIRECTION('center_axis',(0.866146626230631,-0.499789977759954,-3.49001476137941E-15));
#136722=DIRECTION('ref_axis',(-0.499789977759954,-0.866146626230631,-6.82961998416062E-15));
#136723=DIRECTION('center_axis',(0.499999999999992,0.866025403784443,6.1178315259999E-15));
#136724=DIRECTION('ref_axis',(0.866025403784443,-0.499999999999992,-3.41480999208033E-15));
#136725=DIRECTION('center_axis',(-0.499999999999998,-0.86602540378444,-6.04742307255492E-15));
#136726=DIRECTION('ref_axis',(-0.86602540378444,0.499999999999998,3.41480999208026E-15));
#136727=DIRECTION('center_axis',(-2.11225360334865E-16,-7.10491369633528E-15,
1.));
#136728=DIRECTION('ref_axis',(-1.,1.60344088833289E-30,-2.11560228140819E-16));
#136729=DIRECTION('center_axis',(0.865904130412297,-0.500209992837931,-3.49294771099299E-15));
#136730=DIRECTION('ref_axis',(-0.500209992837931,-0.865904130412297,-6.82961998416051E-15));
#136731=DIRECTION('center_axis',(-0.264962338412774,-0.45892823222322,0.848044713969319));
#136732=DIRECTION('ref_axis',(2.43676345907576E-15,-0.879478359737737,-0.475938877118711));
#136733=DIRECTION('center_axis',(-0.264962078570521,-0.458927782163195,
-0.848045038708653));
#136734=DIRECTION('ref_axis',(1.53522557929348E-15,0.879478631391256,-0.475938375135021));
#136735=DIRECTION('center_axis',(-0.264962376555394,-0.458928247861462,
0.848044693589274));
#136736=DIRECTION('ref_axis',(0.420092076167741,0.736687329153681,0.529919264233235));
#136737=DIRECTION('center_axis',(-0.264962371077221,-0.458928288799658,
0.848044673146736));
#136738=DIRECTION('ref_axis',(1.01699383191385E-17,-0.879478325588507,-0.475938940222416));
#136739=DIRECTION('center_axis',(0.264962073791877,0.458927817278717,0.848045021198581));
#136740=DIRECTION('ref_axis',(-0.42775071226141,-0.732266960578161,0.529919264233221));
#136741=DIRECTION('center_axis',(-0.264962106632886,-0.458927830768637,
-0.848045003637576));
#136742=DIRECTION('ref_axis',(-2.90135607278746E-16,0.879478602053325,-0.475938429348093));
#136743=DIRECTION('center_axis',(0.86615446498511,-0.499776392786171,-3.48991989801451E-15));
#136744=DIRECTION('ref_axis',(-0.499776392786171,-0.86615446498511,-6.82961998416069E-15));
#136745=DIRECTION('center_axis',(-0.50000000000001,-0.866025403784433,-6.04742307255487E-15));
#136746=DIRECTION('ref_axis',(-0.866025403784433,0.50000000000001,3.41480999208034E-15));
#136747=DIRECTION('center_axis',(-2.11225360334865E-16,-7.10491369633528E-15,
1.));
#136748=DIRECTION('ref_axis',(-1.,1.70692667996567E-30,-2.10200002026934E-16));
#136749=DIRECTION('center_axis',(0.865896284857143,-0.500223573885315,2.38376527871029E-14));
#136750=DIRECTION('ref_axis',(-0.500223573885315,-0.865896284857143,-6.82961998416031E-15));
#136751=DIRECTION('center_axis',(-0.499999999999992,-0.866025403784443,
-6.1178315259999E-15));
#136752=DIRECTION('ref_axis',(-0.866025403784443,0.499999999999992,3.41480999208041E-15));
#136753=DIRECTION('center_axis',(-0.432983094186217,-0.750008802379052,
0.500012436348207));
#136754=DIRECTION('ref_axis',(-0.250863215223843,-0.432528431834534,-0.866017784403019));
#136755=DIRECTION('center_axis',(0.264962371077185,0.45892828879969,-0.84804467314673));
#136756=DIRECTION('ref_axis',(-2.01281341115834E-15,0.879478325588492,0.475938940222443));
#136757=DIRECTION('center_axis',(0.250002513555436,0.433017035277449,-0.866022511471551));
#136758=DIRECTION('ref_axis',(0.436883602746975,0.747751775424735,0.499999999999979));
#136759=DIRECTION('center_axis',(-0.250002511507164,-0.433017051950226,
0.866022503726344));
#136760=DIRECTION('ref_axis',(-2.52000272705874E-15,-0.894424794863812,
-0.44721838774007));
#136761=DIRECTION('center_axis',(0.26496237652361,0.458928247655632,-0.848044693710592));
#136762=DIRECTION('ref_axis',(0.427943903597026,0.732154074473812,0.529919264233274));
#136763=DIRECTION('center_axis',(0.264962338412787,0.4589282322232,-0.848044713969326));
#136764=DIRECTION('ref_axis',(-1.36968032163284E-15,0.879478359737747,0.475938877118692));
#136765=DIRECTION('center_axis',(-0.50000000000001,-0.866025403784433,-6.70236582766912E-14));
#136766=DIRECTION('ref_axis',(-0.866025403784433,0.50000000000001,3.41480999208034E-15));
#136767=DIRECTION('center_axis',(0.499999999999998,0.86602540378444,6.04742307255492E-15));
#136768=DIRECTION('ref_axis',(0.86602540378444,-0.499999999999998,-3.41480999208026E-15));
#136769=DIRECTION('center_axis',(-0.499999999999992,-0.866025403784443,
-6.1178315259999E-15));
#136770=DIRECTION('ref_axis',(-0.866025403784443,0.499999999999992,3.41480999208041E-15));
#136771=DIRECTION('center_axis',(-0.50000000000001,-0.866025403784433,2.12710568640878E-14));
#136772=DIRECTION('ref_axis',(-0.866025403784433,0.50000000000001,3.41480999208034E-15));
#136773=DIRECTION('center_axis',(-0.499999999999992,-0.866025403784443,
-6.1178315259999E-15));
#136774=DIRECTION('ref_axis',(-0.866025403784443,0.499999999999992,3.41480999208041E-15));
#136775=DIRECTION('center_axis',(0.432988827019022,0.750027562856532,0.499979330204942));
#136776=DIRECTION('ref_axis',(-0.249154705652333,-0.433476564272626,0.866036951219576));
#136777=DIRECTION('center_axis',(-0.250002579266693,-0.43301716931316,-0.866022425483324));
#136778=DIRECTION('ref_axis',(-2.14154226504039E-15,0.894424730216448,-0.447218517033044));
#136779=DIRECTION('center_axis',(-0.250002583752831,-0.433017177083424,
-0.866022420303084));
#136780=DIRECTION('ref_axis',(0.866025403788155,-0.499999999993563,-4.2922795574701E-12));
#136781=DIRECTION('center_axis',(0.203370361062878,0.456777309669372,-0.866022508721549));
#136782=DIRECTION('ref_axis',(-0.913545457643545,0.40673664307368,-1.36373852159054E-12));
#136783=DIRECTION('center_axis',(0.352268789801635,0.791134794600313,-0.500012436349749));
#136784=DIRECTION('ref_axis',(0.202469153692936,0.457186437793193,0.866017784402166));
#136785=DIRECTION('center_axis',(-0.203370364581913,-0.456777317573281,
0.866022503726305));
#136786=DIRECTION('ref_axis',(-9.65527517661163E-16,-0.884507036382094,
-0.466526850878452));
#136787=DIRECTION('center_axis',(-0.406736643075807,-0.913545457642598,
-6.37925383508808E-15));
#136788=DIRECTION('ref_axis',(-0.913545457642598,0.406736643075807,3.4148099920803E-15));
#136789=DIRECTION('center_axis',(0.406736643075792,0.913545457642605,6.43652923108485E-15));
#136790=DIRECTION('ref_axis',(0.913545457642605,-0.406736643075792,-3.41480999208033E-15));
#136791=DIRECTION('center_axis',(0.406736643075807,0.913545457642598,6.37925383508808E-15));
#136792=DIRECTION('ref_axis',(0.913545457642598,-0.406736643075807,-3.4148099920803E-15));
#136793=DIRECTION('center_axis',(0.406736643075792,0.913545457642605,6.43652923108485E-15));
#136794=DIRECTION('ref_axis',(0.913545457642605,-0.406736643075792,-3.41480999208033E-15));
#136795=DIRECTION('center_axis',(-0.406736643075751,-0.913545457642623,
-6.37925383508826E-15));
#136796=DIRECTION('ref_axis',(-0.913545457642623,0.406736643075751,3.41480999208029E-15));
#136797=DIRECTION('center_axis',(0.215539595588322,0.4841098579238,0.848045003637555));
#136798=DIRECTION('ref_axis',(2.30068443353737E-15,-0.868458021515977,0.495762710240045));
#136799=DIRECTION('center_axis',(-0.20337041970245,-0.456777441376071,-0.866022425483301));
#136800=DIRECTION('ref_axis',(-1.81723778193288E-15,0.884506966812061,-0.466526982779054));
#136801=DIRECTION('center_axis',(-0.215539564333521,-0.484109840903322,
-0.848045021297499));
#136802=DIRECTION('ref_axis',(-0.340990855200675,-0.776473315744986,0.52991926423324));
#136803=DIRECTION('center_axis',(0.215539572760323,0.484109806651273,0.848045038708655));
#136804=DIRECTION('ref_axis',(-1.36803287013151E-15,-0.868458052949966,
0.49576265517519));
#136805=DIRECTION('center_axis',(-0.203370415729637,-0.456777458307746,
-0.866022417485754));
#136806=DIRECTION('ref_axis',(-0.348084091918547,-0.792992726923284,0.500000000000014));
#136807=DIRECTION('center_axis',(-0.352280597671235,-0.791150459692768,
-0.499979330205079));
#136808=DIRECTION('ref_axis',(0.204240445642775,0.456361522793153,-0.866036951219493));
#136809=DIRECTION('center_axis',(0.913644062717554,-0.406515100163527,2.21206872242239E-14));
#136810=DIRECTION('ref_axis',(-0.406515100163527,-0.913644062717554,-6.82961998416096E-15));
#136811=DIRECTION('center_axis',(0.406736643075792,0.913545457642605,6.43652923108485E-15));
#136812=DIRECTION('ref_axis',(0.913545457642605,-0.406736643075792,-3.41480999208033E-15));
#136813=DIRECTION('center_axis',(-0.406736643075807,-0.913545457642598,
-6.37925383508808E-15));
#136814=DIRECTION('ref_axis',(-0.913545457642598,0.406736643075807,3.4148099920803E-15));
#136815=DIRECTION('center_axis',(-1.98092302886629E-16,-7.11160532333483E-15,
1.));
#136816=DIRECTION('ref_axis',(-1.,1.60344088833289E-30,-1.97456212931431E-16));
#136817=DIRECTION('center_axis',(0.913446798847323,-0.406958162070229,-2.84177365711621E-15));
#136818=DIRECTION('ref_axis',(-0.406958162070229,-0.913446798847323,-6.82961998416051E-15));
#136819=DIRECTION('center_axis',(-0.215539784135063,-0.484110281406773,
0.848044713969297));
#136820=DIRECTION('ref_axis',(1.36848187759281E-15,-0.868457761888255,-0.495763165045612));
#136821=DIRECTION('center_axis',(-0.215539572760323,-0.484109806651275,
-0.848045038708654));
#136822=DIRECTION('ref_axis',(1.54244339943813E-15,0.868458052949965,-0.495762655175192));
#136823=DIRECTION('center_axis',(-0.215539820432031,-0.484110300947188,
0.848044693589289));
#136824=DIRECTION('ref_axis',(0.340785973391266,0.776563258037815,0.529919264233205));
#136825=DIRECTION('center_axis',(-0.215539810706713,-0.484110341087614,
0.848044673146733));
#136826=DIRECTION('ref_axis',(-2.60145221568461E-16,-0.868457725299267,
-0.495763229140709));
#136827=DIRECTION('center_axis',(0.215539564341324,0.484109841073138,0.848045021198576));
#136828=DIRECTION('ref_axis',(-0.348864709028221,-0.772967650156986,0.529919264233187));
#136829=DIRECTION('center_axis',(-0.215539595588306,-0.484109857923764,
-0.84804500363758));
#136830=DIRECTION('ref_axis',(1.59176767299167E-16,0.868458021515999,-0.495762710240007));
#136831=DIRECTION('center_axis',(0.913650438514074,-0.406500770236713,-2.83857970701369E-15));
#136832=DIRECTION('ref_axis',(-0.406500770236713,-0.913650438514073,-6.82961998416048E-15));
#136833=DIRECTION('center_axis',(-0.406736643075807,-0.913545457642598,
-4.51811735233643E-14));
#136834=DIRECTION('ref_axis',(-0.913545457642598,0.406736643075807,3.41480999208031E-15));
#136835=DIRECTION('center_axis',(-1.98092302886629E-16,-7.11160532333483E-15,
1.));
#136836=DIRECTION('ref_axis',(-1.,1.28019500997425E-30,-1.95185716167867E-16));
#136837=DIRECTION('center_axis',(0.913440415876957,-0.406972488803028,2.21119299742975E-14));
#136838=DIRECTION('ref_axis',(-0.406972488803028,-0.913440415876957,-6.82961998416073E-15));
#136839=DIRECTION('center_axis',(-0.406736643075792,-0.913545457642605,
-6.43652923108485E-15));
#136840=DIRECTION('ref_axis',(-0.913545457642605,0.406736643075792,3.4148099920804E-15));
#136841=DIRECTION('center_axis',(-0.352213899942465,-0.791159233140713,
0.500012436348855));
#136842=DIRECTION('ref_axis',(-0.204277427961246,-0.456381342217048,-0.866017784402667));
#136843=DIRECTION('center_axis',(0.215539810706706,0.484110341087612,-0.848044673146735));
#136844=DIRECTION('ref_axis',(8.90622427310465E-16,0.868457725299268,0.495763229140707));
#136845=DIRECTION('center_axis',(0.203370368364315,0.456777301204695,-0.866022511471566));
#136846=DIRECTION('ref_axis',(0.356328964674119,0.789322284579817,0.49999999999997));
#136847=DIRECTION('center_axis',(-0.203370364581893,-0.456777317573237,
0.866022503726333));
#136848=DIRECTION('ref_axis',(1.98101988738834E-15,-0.884507036382119,-0.466526850878405));
#136849=DIRECTION('center_axis',(0.215539820424864,0.484110300737865,-0.848044693710603));
#136850=DIRECTION('ref_axis',(0.349068641867812,0.772875576441078,0.529919264233178));
#136851=DIRECTION('center_axis',(0.215539784134997,0.484110281406756,-0.848044713969323));
#136852=DIRECTION('ref_axis',(1.51050753005434E-16,0.868457761888269,0.495763165045588));
#136853=DIRECTION('center_axis',(-0.406736643075807,-0.913545457642598,
-1.74906806584517E-14));
#136854=DIRECTION('ref_axis',(-0.913545457642598,0.406736643075807,3.4148099920803E-15));
#136855=DIRECTION('center_axis',(0.406736643075751,0.913545457642623,6.37925383508826E-15));
#136856=DIRECTION('ref_axis',(0.913545457642623,-0.406736643075751,-3.41480999208029E-15));
#136857=DIRECTION('center_axis',(-0.406736643075792,-0.913545457642605,
-6.43652923108485E-15));
#136858=DIRECTION('ref_axis',(-0.913545457642605,0.406736643075792,3.4148099920804E-15));
#136859=DIRECTION('center_axis',(-0.406736643075807,-0.913545457642598,
-3.40697467000007E-14));
#136860=DIRECTION('ref_axis',(-0.913545457642598,0.406736643075807,3.4148099920803E-15));
#136861=DIRECTION('center_axis',(-0.406736643075792,-0.913545457642605,
-6.43652923108485E-15));
#136862=DIRECTION('ref_axis',(-0.913545457642605,0.406736643075792,3.4148099920804E-15));
#136863=DIRECTION('center_axis',(0.352217640366581,0.791178490090709,0.499979330205143));
#136864=DIRECTION('ref_axis',(-0.202479170975218,-0.457145692797927,0.866036951219457));
#136865=DIRECTION('center_axis',(-0.203370419702468,-0.456777441376064,
-0.8660224254833));
#136866=DIRECTION('ref_axis',(-1.18383422398248E-15,0.884506966812064,-0.466526982779048));
#136867=DIRECTION('center_axis',(-0.203370423354184,-0.456777449577961,
-0.866022420299725));
#136868=DIRECTION('ref_axis',(0.913545457639069,-0.406736643083733,5.02660029640274E-12));
#136869=DIRECTION('center_axis',(0.154510046711354,0.475533027091701,-0.866022508720332));
#136870=DIRECTION('ref_axis',(-0.95105651629323,0.309016994380866,3.59292648953259E-12));
#136871=DIRECTION('center_axis',(0.267642920194089,0.823622990673941,-0.500012436348632));
#136872=DIRECTION('ref_axis',(0.153571010675692,0.475845712156948,0.866017784402776));
#136873=DIRECTION('center_axis',(-0.154510049384264,-0.475533035318161,
0.8660225037263));
#136874=DIRECTION('ref_axis',(-1.50358015652835E-15,-0.876548788012424,
-0.481313018974088));
#136875=DIRECTION('center_axis',(-0.309016994374914,-0.951056516295165,
-6.64119215765945E-15));
#136876=DIRECTION('ref_axis',(-0.951056516295164,0.309016994374914,3.41480999208033E-15));
#136877=DIRECTION('center_axis',(0.309016994374938,0.951056516295157,6.68470697498369E-15));
#136878=DIRECTION('ref_axis',(0.951056516295157,-0.309016994374938,-3.41480999208033E-15));
#136879=DIRECTION('center_axis',(0.309016994374914,0.951056516295164,6.70459034366198E-14));
#136880=DIRECTION('ref_axis',(0.951056516295164,-0.309016994374914,-3.41480999208034E-15));
#136881=DIRECTION('center_axis',(0.309016994374938,0.951056516295157,6.68470697498369E-15));
#136882=DIRECTION('ref_axis',(0.951056516295157,-0.309016994374938,-3.41480999208033E-15));
#136883=DIRECTION('center_axis',(-0.30901699437498,-0.951056516295143,-6.64119215765931E-15));
#136884=DIRECTION('ref_axis',(-0.951056516295143,0.30901699437498,3.41480999208042E-15));
#136885=DIRECTION('center_axis',(0.163755587629875,0.503987876168979,0.848045003637588));
#136886=DIRECTION('ref_axis',(-4.64722749497856E-16,-0.859649462041492,
0.510884333691857));
#136887=DIRECTION('center_axis',(-0.154510091261946,-0.475533164204402,
-0.866022425483298));
#136888=DIRECTION('ref_axis',(-5.65902027059014E-17,0.876548714628842,-0.481313152617425));
#136889=DIRECTION('center_axis',(-0.163755558328224,-0.503987855973834,
-0.848045021297519));
#136890=DIRECTION('ref_axis',(-0.257959309140581,-0.807862963764457,0.529919264233168));
#136891=DIRECTION('center_axis',(0.163755570286389,0.503987822791218,0.848045038708646));
#136892=DIRECTION('ref_axis',(-1.41598484853067E-15,-0.859649495083696,
0.510884278092747));
#136893=DIRECTION('center_axis',(-0.154510085548364,-0.475533180625675,
-0.866022417485752));
#136894=DIRECTION('ref_axis',(-0.263286939714892,-0.825033325009111,0.499999999999978));
#136895=DIRECTION('center_axis',(-0.267653025932247,-0.823639804208766,
-0.499979330205016));
#136896=DIRECTION('ref_axis',(0.15541882643971,0.475210466541391,-0.866036951219529));
#136897=DIRECTION('center_axis',(0.951131423661017,-0.308786358060986,-2.15624361371854E-15));
#136898=DIRECTION('ref_axis',(-0.308786358060986,-0.951131423661017,-6.82961998416067E-15));
#136899=DIRECTION('center_axis',(0.309016994374938,0.951056516295157,6.68470697498369E-15));
#136900=DIRECTION('ref_axis',(0.951056516295157,-0.309016994374938,-3.41480999208033E-15));
#136901=DIRECTION('center_axis',(-0.309016994374914,-0.951056516295165,
-6.64119215765945E-15));
#136902=DIRECTION('ref_axis',(-0.951056516295164,0.309016994374914,3.41480999208033E-15));
#136903=DIRECTION('center_axis',(-1.84331724214206E-16,-7.11688751458844E-15,
1.));
#136904=DIRECTION('ref_axis',(-1.,1.20258066624967E-30,-1.83352197722043E-16));
#136905=DIRECTION('center_axis',(0.95098155300316,-0.309247612517378,-2.15946453637244E-15));
#136906=DIRECTION('ref_axis',(-0.309247612517378,-0.95098155300316,-6.82961998416082E-15));
#136907=DIRECTION('center_axis',(-0.163755730877748,-0.503988317040613,
0.848044713969296));
#136908=DIRECTION('ref_axis',(-2.05932374345746E-15,-0.859649189130447,
-0.510884792910658));
#136909=DIRECTION('center_axis',(-0.163755570286382,-0.503987822791197,
-0.848045038708659));
#136910=DIRECTION('ref_axis',(-2.40920520154009E-15,0.859649495083709,-0.510884278092725));
#136911=DIRECTION('center_axis',(-0.163755764928173,-0.503988340269717,
0.848044693589297));
#136912=DIRECTION('ref_axis',(0.257746148181657,0.807930997358076,0.529919264233245));
#136913=DIRECTION('center_axis',(-0.163755751065481,-0.503988379172018,
0.848044673146729));
#136914=DIRECTION('ref_axis',(-1.44619219902002E-15,-0.859649150669456,
-0.510884857627707));
#136915=DIRECTION('center_axis',(0.163755558317298,0.503987856143866,0.84804502119858));
#136916=DIRECTION('ref_axis',(-0.266156471020706,-0.805199544416383,0.529919264233198));
#136917=DIRECTION('center_axis',(-0.163755587629886,-0.503987876169014,
-0.848045003637565));
#136918=DIRECTION('ref_axis',(-1.56939166226977E-15,0.859649462041471,-0.510884333691893));
#136919=DIRECTION('center_axis',(0.951136266645031,-0.308771440182787,1.47141933445522E-14));
#136920=DIRECTION('ref_axis',(-0.308771440182787,-0.951136266645031,-6.82961998416084E-15));
#136921=DIRECTION('center_axis',(-0.309016994374914,-0.951056516295165,
-6.64119215765945E-15));
#136922=DIRECTION('ref_axis',(-0.951056516295164,0.309016994374914,3.41480999208033E-15));
#136923=DIRECTION('center_axis',(-1.84331724214206E-16,-7.11688751458844E-15,
1.));
#136924=DIRECTION('ref_axis',(-1.,1.28019500997425E-30,-1.87678573238334E-16));
#136925=DIRECTION('center_axis',(0.950976702550726,-0.309262527968953,1.4737595640537E-14));
#136926=DIRECTION('ref_axis',(-0.309262527968953,-0.950976702550726,-6.82961998416076E-15));
#136927=DIRECTION('center_axis',(-0.309016994374938,-0.951056516295157,
-6.68470697498369E-15));
#136928=DIRECTION('ref_axis',(-0.951056516295156,0.309016994374938,3.41480999208031E-15));
#136929=DIRECTION('center_axis',(-0.267585776506164,-0.823641557784294,
0.500012436347593));
#136930=DIRECTION('ref_axis',(-0.155453534446431,-0.475234043104139,-0.866017784403418));
#136931=DIRECTION('center_axis',(0.163755751065396,0.503988379172029,-0.848044673146739));
#136932=DIRECTION('ref_axis',(8.46156807197952E-16,0.859649150669455,0.51088485762771));
#136933=DIRECTION('center_axis',(0.154510054856538,0.475533019434788,-0.866022511471534));
#136934=DIRECTION('ref_axis',(0.271870311892821,0.822244813611669,0.500000000000011));
#136935=DIRECTION('center_axis',(-0.154510049384232,-0.47553303531805,0.866022503726367));
#136936=DIRECTION('ref_axis',(1.97566536568584E-15,-0.876548788012487,-0.481313018973972));
#136937=DIRECTION('center_axis',(0.163755764947861,0.503988340059225,-0.84804469371059));
#136938=DIRECTION('ref_axis',(0.266368910994597,0.805129291884236,0.52991926423328));
#136939=DIRECTION('center_axis',(0.163755730877703,0.503988317040579,-0.848044713969325));
#136940=DIRECTION('ref_axis',(-3.52263469559639E-16,0.85964918913047,0.510884792910619));
#136941=DIRECTION('center_axis',(-0.309016994374914,-0.951056516295164,
-1.50830667185725E-14));
#136942=DIRECTION('ref_axis',(-0.951056516295164,0.309016994374914,3.41480999208034E-15));
#136943=DIRECTION('center_axis',(0.309016994374914,0.951056516295165,6.64119215765945E-15));
#136944=DIRECTION('ref_axis',(0.951056516295164,-0.309016994374914,-3.41480999208033E-15));
#136945=DIRECTION('center_axis',(-0.309016994374938,-0.951056516295157,
-6.68470697498369E-15));
#136946=DIRECTION('ref_axis',(-0.951056516295156,0.309016994374938,3.41480999208031E-15));
#136947=DIRECTION('center_axis',(-0.309016994374914,-0.951056516295164,
1.80068240325357E-15));
#136948=DIRECTION('ref_axis',(-0.951056516295164,0.309016994374914,3.41480999208033E-15));
#136949=DIRECTION('center_axis',(-0.309016994374938,-0.951056516295157,
-6.68470697498369E-15));
#136950=DIRECTION('ref_axis',(-0.951056516295156,0.309016994374938,3.41480999208031E-15));
#136951=DIRECTION('center_axis',(0.267587483539828,0.823661100222926,0.499979330205141));
#136952=DIRECTION('ref_axis',(-0.153585232154563,-0.475806237439678,0.866036951219476));
#136953=DIRECTION('center_axis',(-0.154510091261949,-0.475533164204398,
-0.8660224254833));
#136954=DIRECTION('ref_axis',(-2.91289309623471E-16,0.876548714628845,-0.481313152617421));
#136955=DIRECTION('center_axis',(-0.1545100940345,-0.475533172737467,-0.866022420303128));
#136956=DIRECTION('ref_axis',(0.951056516295032,-0.309016994375322,2.70999320328836E-13));
#136957=DIRECTION('center_axis',(0.103956887954599,0.489078705158833,-0.866022508718425));
#136958=DIRECTION('ref_axis',(-0.978147600732856,0.207911690822227,2.63131599354494E-12));
#136959=DIRECTION('center_axis',(0.180084698745615,0.847087400906804,-0.500012436347994));
#136960=DIRECTION('ref_axis',(0.102990311575353,0.489291521303063,0.866017784403153));
#136961=DIRECTION('center_axis',(-0.103956889752271,-0.489078713616376,
0.866022503726309));
#136962=DIRECTION('ref_axis',(3.36406328257384E-16,-0.8707403454847,-0.491743073916843));
#136963=DIRECTION('center_axis',(-0.207911690817757,-0.978147600733806,
-6.83036818919254E-15));
#136964=DIRECTION('ref_axis',(-0.978147600733806,0.207911690817757,-2.9624920046404E-32));
#136965=DIRECTION('center_axis',(0.207911690817749,0.978147600733808,6.85964567039975E-15));
#136966=DIRECTION('ref_axis',(0.978147600733808,-0.207911690817749,-5.45082275808818E-31));
#136967=DIRECTION('center_axis',(0.207911690817754,0.978147600733807,6.83036818919254E-15));
#136968=DIRECTION('ref_axis',(0.978147600733807,-0.207911690817754,1.95361542122215E-29));
#136969=DIRECTION('center_axis',(0.207911690817749,0.978147600733808,6.85964567039975E-15));
#136970=DIRECTION('ref_axis',(0.978147600733808,-0.207911690817749,6.12351326823131E-31));
#136971=DIRECTION('center_axis',(-0.207911690817754,-0.978147600733807,
-6.83036818919254E-15));
#136972=DIRECTION('ref_axis',(-0.978147600733807,0.207911690817754,-1.95800148050649E-29));
#136973=DIRECTION('center_axis',(0.110177439185349,0.518344097776633,0.848045003637594));
#136974=DIRECTION('ref_axis',(6.77677416945363E-16,-0.853239582811881,0.521519140898018));
#136975=DIRECTION('center_axis',(-0.103956917928284,-0.489078846173993,
-0.866022425483294));
#136976=DIRECTION('ref_axis',(1.37107671501608E-16,0.870740269393781,-0.491743208652692));
#136977=DIRECTION('center_axis',(-0.110177412158605,-0.518344074628572,
-0.848045021297503));
#136978=DIRECTION('ref_axis',(-0.172101506927857,-0.830401496089509,0.529919264233209));
#136979=DIRECTION('center_axis',(0.110177427516376,0.518344042878429,0.848045038708628));
#136980=DIRECTION('ref_axis',(-1.64656692434778E-15,-0.853239616987284,
0.52151908498481));
#136981=DIRECTION('center_axis',(-0.103956910521484,-0.489078861909693,
-0.866022417485799));
#136982=DIRECTION('ref_axis',(-0.175605160694143,-0.848034685338789,0.499999999999924));
#136983=DIRECTION('center_axis',(-0.180092991631242,-0.847105178672024,
-0.499979330205107));
#136984=DIRECTION('ref_axis',(0.104894406044524,0.488852904975547,-0.866036951219482));
#136985=DIRECTION('center_axis',(0.978197989689811,-0.207674488001809,1.19112578788782E-14));
#136986=DIRECTION('ref_axis',(-0.207674488001809,-0.97819798968981,-6.82961998416062E-15));
#136987=DIRECTION('center_axis',(0.207911690817749,0.978147600733808,6.85964567039975E-15));
#136988=DIRECTION('ref_axis',(0.978147600733808,-0.207911690817749,-5.45082275808818E-31));
#136989=DIRECTION('center_axis',(-0.207911690817754,-0.978147600733807,
-6.83036818919254E-15));
#136990=DIRECTION('ref_axis',(-0.978147600733807,0.207911690817754,-1.95800148050649E-29));
#136991=DIRECTION('center_axis',(-1.70094388097117E-16,-7.12070239730339E-15,
1.));
#136992=DIRECTION('ref_axis',(-1.,1.20258066624967E-30,-1.69248182512655E-16));
#136993=DIRECTION('center_axis',(0.978097154258596,-0.208148881407602,-1.45349587027143E-15));
#136994=DIRECTION('ref_axis',(-0.208148881407602,-0.978097154258596,-6.82961998416085E-15));
#136995=DIRECTION('center_axis',(-0.110177535564893,-0.518344551206603,
0.8480447139693));
#136996=DIRECTION('ref_axis',(-2.8516928717058E-16,-0.853239300541027,-0.521519602711403));
#136997=DIRECTION('center_axis',(-0.11017742751637,-0.5183440428784,-0.848045038708647));
#136998=DIRECTION('ref_axis',(-5.45915083851553E-16,0.853239616987302,-0.52151908498478));
#136999=DIRECTION('center_axis',(-0.1101775670102,-0.518344577865721,0.848044693589271));
#137000=DIRECTION('ref_axis',(0.171882402212669,0.830446875606248,0.529919264233169));
#137001=DIRECTION('center_axis',(-0.110177549147491,-0.518344615107845,
0.848044673146735));
#137002=DIRECTION('ref_axis',(-1.38217757861089E-15,-0.853239260760969,
-0.521519667794107));
#137003=DIRECTION('center_axis',(0.110177412119122,0.518344074798825,0.84804502119857));
#137004=DIRECTION('ref_axis',(-0.180532167035008,-0.828609503964449,0.529919264233179));
#137005=DIRECTION('center_axis',(-0.110177439185351,-0.51834409777664,-0.84804500363759));
#137006=DIRECTION('ref_axis',(-9.47944080834145E-16,0.853239582811877,-0.521519140898025));
#137007=DIRECTION('center_axis',(0.978201246800566,-0.207659145615641,-1.45007606351424E-15));
#137008=DIRECTION('ref_axis',(-0.207659145615641,-0.978201246800566,-6.82961998416063E-15));
#137009=DIRECTION('center_axis',(-0.207911690817754,-0.978147600733807,
-3.9904525120933E-15));
#137010=DIRECTION('ref_axis',(-0.978147600733807,0.207911690817754,-1.14772778150505E-29));
#137011=DIRECTION('center_axis',(-1.70094388097117E-16,-7.12070239730339E-15,
1.));
#137012=DIRECTION('ref_axis',(-1.,1.28019500997425E-30,-1.72664287379267E-16));
#137013=DIRECTION('center_axis',(0.978093889466684,-0.208164222161096,-1.48136221419545E-14));
#137014=DIRECTION('ref_axis',(-0.208164222161096,-0.978093889466684,-6.8296199841606E-15));
#137015=DIRECTION('center_axis',(-0.207911690817749,-0.978147600733808,
-6.85964567039975E-15));
#137016=DIRECTION('ref_axis',(-0.978147600733808,0.207911690817749,-4.42564229104924E-29));
#137017=DIRECTION('center_axis',(-0.180025927304208,-0.847099893161378,
0.500012436349579));
#137018=DIRECTION('ref_axis',(-0.10492645952785,-0.488879980353024,-0.866017784402247));
#137019=DIRECTION('center_axis',(0.110177549147416,0.518344615107856,-0.848044673146738));
#137020=DIRECTION('ref_axis',(1.22718678990651E-15,0.853239260760965,0.521519667794113));
#137021=DIRECTION('center_axis',(0.103956896853785,0.489078698392239,-0.866022511471547));
#137022=DIRECTION('ref_axis',(0.184432991077372,0.846158656400951,0.499999999999992));
#137023=DIRECTION('center_axis',(-0.103956889752269,-0.489078713616277,
0.866022503726365));
#137024=DIRECTION('ref_axis',(1.91503290536032E-16,-0.870740345484756,-0.491743073916743));
#137025=DIRECTION('center_axis',(0.110177567037555,0.518344577661421,-0.84804469371059));
#137026=DIRECTION('ref_axis',(0.180750786626522,0.828561842307743,0.529919264233235));
#137027=DIRECTION('center_axis',(0.110177535564769,0.518344551206602,-0.848044713969317));
#137028=DIRECTION('ref_axis',(4.66838780246052E-16,0.853239300541032,0.521519602711394));
#137029=DIRECTION('center_axis',(-0.207911690817754,-0.978147600733807,
-6.83036818919254E-15));
#137030=DIRECTION('ref_axis',(-0.978147600733807,0.207911690817754,-1.95361542122215E-29));
#137031=DIRECTION('center_axis',(0.207911690817757,0.978147600733806,6.83036818919254E-15));
#137032=DIRECTION('ref_axis',(0.978147600733806,-0.207911690817757,2.9624920046404E-32));
#137033=DIRECTION('center_axis',(-0.207911690817749,-0.978147600733808,
-6.85964567039975E-15));
#137034=DIRECTION('ref_axis',(-0.978147600733808,0.207911690817749,-4.42564229104924E-29));
#137035=DIRECTION('center_axis',(-0.207911690817754,-0.978147600733807,
-1.15053683499437E-15));
#137036=DIRECTION('ref_axis',(-0.978147600733807,0.207911690817754,-3.31272147910634E-30));
#137037=DIRECTION('center_axis',(-0.207911690817749,-0.978147600733808,
-6.85964567039975E-15));
#137038=DIRECTION('ref_axis',(-0.978147600733808,0.207911690817749,-4.42564229104924E-29));
#137039=DIRECTION('center_axis',(0.180025582246976,0.847119506979154,0.499979330204792));
#137040=DIRECTION('ref_axis',(-0.103008581358723,-0.489253749386354,0.866036951219668));
#137041=DIRECTION('center_axis',(-0.103956917928285,-0.489078846173996,
-0.866022425483293));
#137042=DIRECTION('ref_axis',(7.50813757209353E-17,0.87074026939378,-0.491743208652695));
#137043=DIRECTION('center_axis',(-0.103956919794064,-0.489078854951829,
-0.866022420302118));
#137044=DIRECTION('ref_axis',(0.978147600734944,-0.207911690812404,-3.14708888126906E-12));
#137045=DIRECTION('center_axis',(0.052264755777796,0.497265934580814,-0.866022508719581));
#137046=DIRECTION('ref_axis',(-0.994521895368699,0.1045284632636,-2.36468762881567E-12));
#137047=DIRECTION('center_axis',(0.0905534316544205,0.86127094430961,-0.500012436348978));
#137048=DIRECTION('ref_axis',(0.0512812291455777,0.497376550146495,0.866017784402658));
#137049=DIRECTION('center_axis',(-0.052264756681742,-0.497265943181931,
0.866022503726308));
#137050=DIRECTION('ref_axis',(-5.67711925317034E-16,-0.867207748104371,
-0.497946504785149));
#137051=DIRECTION('center_axis',(-0.104528463267628,-0.994521895368276,
-6.94470927749848E-15));
#137052=DIRECTION('ref_axis',(-0.994521895368276,0.104528463267628,-1.09814391166396E-31));
#137053=DIRECTION('center_axis',(0.104528463267644,0.994521895368274,6.95942865237777E-15));
#137054=DIRECTION('ref_axis',(0.994521895368274,-0.104528463267644,2.54964018847027E-31));
#137055=DIRECTION('center_axis',(0.104528463267629,0.994521895368276,7.65859895914467E-15));
#137056=DIRECTION('ref_axis',(0.994521895368276,-0.104528463267629,-5.54203336120443E-30));
#137057=DIRECTION('center_axis',(0.104528463267644,0.994521895368274,6.95942865237777E-15));
#137058=DIRECTION('ref_axis',(0.994521895368274,-0.104528463267644,-3.92382721438483E-32));
#137059=DIRECTION('center_axis',(-0.10452846326763,-0.994521895368276,-6.94470927749848E-15));
#137060=DIRECTION('ref_axis',(-0.994521895368276,0.10452846326763,9.84955453724887E-30));
#137061=DIRECTION('center_axis',(0.0553921636609794,0.527021232978621,0.848045003637572));
#137062=DIRECTION('ref_axis',(8.12865720800958E-16,-0.849349030019372,0.527831625809927));
#137063=DIRECTION('center_axis',(-0.0522647708473857,-0.497266077958567,
-0.866022425483298));
#137064=DIRECTION('ref_axis',(1.39086404037747E-16,0.867207670398085,-0.497946640115912));
#137065=DIRECTION('center_axis',(-0.05539213919652,-0.527021207132817,-0.848045021297515));
#137066=DIRECTION('ref_axis',(-0.0843581245622004,-0.84384197585503,0.529919264233172));
#137067=DIRECTION('center_axis',(0.0553921577943494,0.527021177161365,0.848045038708638));
#137068=DIRECTION('ref_axis',(-7.11135774336482E-17,-0.849349064867508,
0.527831569734788));
#137069=DIRECTION('center_axis',(-0.052264761839755,-0.497266092833514,
-0.866022417485786));
#137070=DIRECTION('ref_axis',(-0.0859994148074141,-0.861744800189027,0.499999999999957));
#137071=DIRECTION('center_axis',(-0.0905598208270387,-0.861289491529733,
-0.499979330204988));
#137072=DIRECTION('ref_axis',(0.0532207405876983,0.4971393686821,-0.866036951219554));
#137073=DIRECTION('center_axis',(0.994547213842469,-0.104287292793425,1.2856524780366E-14));
#137074=DIRECTION('ref_axis',(-0.104287292793425,-0.994547213842469,-6.82961998416055E-15));
#137075=DIRECTION('center_axis',(0.104528463267644,0.994521895368274,6.95942865237777E-15));
#137076=DIRECTION('ref_axis',(0.994521895368274,-0.104528463267644,2.54964018847027E-31));
#137077=DIRECTION('center_axis',(-0.104528463267628,-0.994521895368276,
-6.94470927749848E-15));
#137078=DIRECTION('ref_axis',(-0.994521895368276,0.104528463267628,-1.09814391166396E-31));
#137079=DIRECTION('center_axis',(-1.55536281769216E-16,-7.12300817482632E-15,
1.));
#137080=DIRECTION('ref_axis',(-1.,1.20258066624967E-30,-1.55144167303267E-16));
#137081=DIRECTION('center_axis',(0.994496518411992,-0.104769627595152,-7.31602399252034E-16));
#137082=DIRECTION('ref_axis',(-0.104769627595152,-0.994496518411992,-6.82961998416046E-15));
#137083=DIRECTION('center_axis',(-0.055392212116204,-0.527021693999024,
0.848044713969301));
#137084=DIRECTION('ref_axis',(-3.41086766092002E-17,-0.849348742192385,
-0.527832088960318));
#137085=DIRECTION('center_axis',(-0.0553921577943474,-0.527021177161346,
-0.84804503870865));
#137086=DIRECTION('ref_axis',(3.58151228089054E-16,0.84934906486752,-0.527831569734768));
#137087=DIRECTION('center_axis',(-0.0553922405964155,-0.527021723799658,
0.848044693589286));
#137088=DIRECTION('ref_axis',(0.0841354767083805,0.843864204095404,0.529919264233227));
#137089=DIRECTION('center_axis',(-0.0553922189449436,-0.527021758969977,
0.848044673146732));
#137090=DIRECTION('ref_axis',(-5.11211380535554E-17,-0.849348701629307,
-0.527832154231447));
#137091=DIRECTION('center_axis',(0.0553921391546639,0.5270212072964,0.848045021198589));
#137092=DIRECTION('ref_axis',(-0.0929299148097542,-0.842941044396323,0.52991926423323));
#137093=DIRECTION('center_axis',(-0.0553921636609763,-0.527021232978591,
-0.848045003637591));
#137094=DIRECTION('ref_axis',(-1.63069853500586E-16,0.849349030019391,-0.527831625809898));
#137095=DIRECTION('center_axis',(0.994548849394384,-0.104271693993661,3.67176988899929E-16));
#137096=DIRECTION('ref_axis',(-0.104271693993661,-0.994548849394384,-6.82961998416081E-15));
#137097=DIRECTION('center_axis',(-0.104528463267629,-0.994521895368276,
-6.94470927749848E-15));
#137098=DIRECTION('ref_axis',(-0.994521895368276,0.104528463267629,4.91917387961755E-30));
#137099=DIRECTION('center_axis',(-1.55536281769216E-16,-7.12300817482632E-15,
1.));
#137100=DIRECTION('ref_axis',(-1.,1.28019500997425E-30,-1.576500015202E-16));
#137101=DIRECTION('center_axis',(0.99449487505034,-0.104785225574074,-7.31711319356696E-16));
#137102=DIRECTION('ref_axis',(-0.104785225574074,-0.994494875050339,-6.82961998416066E-15));
#137103=DIRECTION('center_axis',(-0.104528463267644,-0.994521895368274,
-6.95942865237777E-15));
#137104=DIRECTION('ref_axis',(-0.994521895368274,0.104528463267644,9.55177901418214E-30));
#137105=DIRECTION('center_axis',(-0.0904936763714717,-0.861277224842458,
0.500012436349786));
#137106=DIRECTION('ref_axis',(-0.053249788305639,-0.497169646242195,-0.866017784402154));
#137107=DIRECTION('center_axis',(0.0553922189448982,0.527021758969989,-0.848044673146727));
#137108=DIRECTION('ref_axis',(-1.85765759131825E-16,0.8493487016293,0.527832154231458));
#137109=DIRECTION('center_axis',(0.052264765337821,0.497265928783258,-0.866022511471559));
#137110=DIRECTION('ref_axis',(0.0949749838233155,0.860801807879023,0.499999999999967));
#137111=DIRECTION('center_axis',(-0.0522647566817781,-0.497265943181826,
0.866022503726366));
#137112=DIRECTION('ref_axis',(7.61153916252116E-16,-0.867207748104431,-0.497946504785044));
#137113=DIRECTION('center_axis',(0.0553922406558896,0.527021723598192,-0.848044693710603));
#137114=DIRECTION('ref_axis',(0.0931523188145091,0.842916495801343,0.529919264233209));
#137115=DIRECTION('center_axis',(0.0553922121161434,0.527021693999006,-0.848044713969316));
#137116=DIRECTION('ref_axis',(3.67189309331813E-16,0.849348742192398,0.527832088960298));
#137117=DIRECTION('center_axis',(-0.104528463267629,-0.994521895368276,
-6.23081959585225E-15));
#137118=DIRECTION('ref_axis',(-0.994521895368276,0.104528463267629,4.46057211924954E-30));
#137119=DIRECTION('center_axis',(0.104528463267629,0.994521895368276,6.94470927749848E-15));
#137120=DIRECTION('ref_axis',(0.994521895368276,-0.104528463267629,-4.99922698313062E-30));
#137121=DIRECTION('center_axis',(-0.104528463267644,-0.994521895368274,
-6.95942865237777E-15));
#137122=DIRECTION('ref_axis',(-0.994521895368274,0.104528463267644,9.55177901418214E-30));
#137123=DIRECTION('center_axis',(-0.104528463267629,-0.994521895368276,
-6.94470927749848E-15));
#137124=DIRECTION('ref_axis',(-0.994521895368276,0.104528463267629,4.99922698313062E-30));
#137125=DIRECTION('center_axis',(-0.104528463267644,-0.994521895368274,
-6.95942865237777E-15));
#137126=DIRECTION('ref_axis',(-0.994521895368274,0.104528463267644,9.55177901418214E-30));
#137127=DIRECTION('center_axis',(0.0904912830026074,0.861296695145313,0.499979330205064));
#137128=DIRECTION('ref_axis',(-0.0513033469953135,-0.497340894869405,0.866036951219507));
#137129=DIRECTION('center_axis',(-0.0522647708473827,-0.497266077958539,
-0.866022425483315));
#137130=DIRECTION('ref_axis',(6.35438415383309E-16,0.867207670398102,-0.497946640115884));
#137131=DIRECTION('center_axis',(-0.0522647717855476,-0.497266086884524,
-0.866022420301436));
#137132=DIRECTION('ref_axis',(0.994521895367887,-0.104528463271327,2.15051073550011E-12));
#137133=DIRECTION('center_axis',(-5.08733525851855E-15,0.500005014362956,
-0.86602250872128));
#137134=DIRECTION('ref_axis',(-1.,-2.37780049919996E-12,-1.38122234879998E-12));
#137135=DIRECTION('center_axis',(3.00422159424583E-5,0.866018223014576,
-0.500012436349478));
#137136=DIRECTION('ref_axis',(-0.000989701280057339,0.500012217440974,0.866017784402339));
#137137=DIRECTION('center_axis',(-2.73187543788774E-14,-0.500005023014378,
0.866022503726313));
#137138=DIRECTION('ref_axis',(1.77159806316853E-29,-0.866022503726313,-0.500005023014378));
#137139=DIRECTION('center_axis',(0.,-1.,-6.98296267768627E-15));
#137140=DIRECTION('ref_axis',(0.,6.98296267768627E-15,-1.));
#137141=DIRECTION('center_axis',(-1.04744440165294E-14,1.,6.98296267768627E-15));
#137142=DIRECTION('ref_axis',(1.,1.04744440165294E-14,-1.12103877145985E-44));
#137143=DIRECTION('center_axis',(0.,1.,6.98296267768627E-15));
#137144=DIRECTION('ref_axis',(0.,-6.98296267768627E-15,1.));
#137145=DIRECTION('center_axis',(-1.04744440165294E-14,1.,6.98296267768627E-15));
#137146=DIRECTION('ref_axis',(1.,1.04744440165294E-14,-1.12103877145985E-44));
#137147=DIRECTION('center_axis',(0.,-1.,-6.98296267768627E-15));
#137148=DIRECTION('ref_axis',(0.,6.98296267768627E-15,-1.));
#137149=DIRECTION('center_axis',(0.,0.529924213265784,0.848045003637567));
#137150=DIRECTION('ref_axis',(0.,-0.848045003637567,0.529924213265784));
#137151=DIRECTION('center_axis',(0.,-0.500005158533416,-0.866022425483298));
#137152=DIRECTION('ref_axis',(0.,0.866022425483298,-0.500005158533416));
#137153=DIRECTION('center_axis',(2.16260202548866E-8,-0.529924185004347,
-0.848045021297501));
#137154=DIRECTION('ref_axis',(0.00430950302111146,-0.848037146343372,0.529919264233243));
#137155=DIRECTION('center_axis',(0.,0.529924157141045,0.848045038708648));
#137156=DIRECTION('ref_axis',(0.,-0.848045038708648,0.529924157141045));
#137157=DIRECTION('center_axis',(1.05155814435434E-8,-0.500005172385354,
-0.866022417485767));
#137158=DIRECTION('ref_axis',(0.00454855868473161,-0.866013458679421,0.499999999999998));
#137159=DIRECTION('center_axis',(-3.44576747652515E-5,-0.86603733648169,
-0.499979330205127));
#137160=DIRECTION('ref_axis',(0.000963977567144606,0.499979069431645,-0.866036951219471));
#137161=DIRECTION('center_axis',(-1.04744440165294E-14,1.,6.98296267768627E-15));
#137162=DIRECTION('ref_axis',(1.,1.04744440165294E-14,-1.12103877145985E-44));
#137163=DIRECTION('center_axis',(0.,-1.,-6.98296267768627E-15));
#137164=DIRECTION('ref_axis',(0.,6.98296267768627E-15,-1.));
#137165=DIRECTION('center_axis',(-2.89534733035821E-14,-0.529924676825572,
0.848044713969324));
#137166=DIRECTION('ref_axis',(6.94515430910295E-29,-0.848044713969324,-0.529924676825572));
#137167=DIRECTION('center_axis',(0.,-0.529924157141035,-0.848045038708655));
#137168=DIRECTION('ref_axis',(0.,0.848045038708655,-0.529924157141035));
#137169=DIRECTION('center_axis',(-2.52127146216552E-8,-0.529924709439994,
0.848044693589281));
#137170=DIRECTION('ref_axis',(-0.00453325470002202,0.848035979777022,0.529919264233195));
#137171=DIRECTION('center_axis',(-4.63345827774717E-14,-0.529924742154438,
0.848044673146735));
#137172=DIRECTION('ref_axis',(-3.13786732617605E-28,-0.848044673146735,
-0.529924742154438));
#137173=DIRECTION('center_axis',(-2.16960312490591E-8,0.529924185162669,
0.848045021198569));
#137174=DIRECTION('ref_axis',(-0.00430950303215927,-0.848037146343347,0.529919264233193));
#137175=DIRECTION('center_axis',(0.,-0.529924213265784,-0.848045003637567));
#137176=DIRECTION('ref_axis',(0.,0.848045003637567,-0.529924213265784));
#137177=DIRECTION('center_axis',(0.,-1.,-6.98296267768627E-15));
#137178=DIRECTION('ref_axis',(0.,6.98296267768627E-15,-1.));
#137179=DIRECTION('center_axis',(1.04744440165294E-14,-1.,-6.98296267768627E-15));
#137180=DIRECTION('ref_axis',(-1.,-1.04744440165294E-14,-1.34524652575182E-42));
#137181=DIRECTION('center_axis',(3.00422162114182E-5,-0.86601822301478,
0.500012436349125));
#137182=DIRECTION('ref_axis',(-0.000989701260860521,-0.50001221744063,-0.86601778440256));
#137183=DIRECTION('center_axis',(0.,0.529924742154438,-0.848044673146735));
#137184=DIRECTION('ref_axis',(0.,0.848044673146735,0.529924742154438));
#137185=DIRECTION('center_axis',(1.01126011638448E-8,0.500005009599381,
-0.866022511471569));
#137186=DIRECTION('ref_axis',(0.00447641076763253,0.866013834616223,0.499999999999945));
#137187=DIRECTION('center_axis',(0.,-0.500005023014361,0.866022503726323));
#137188=DIRECTION('ref_axis',(0.,-0.866022503726323,-0.500005023014361));
#137189=DIRECTION('center_axis',(2.52898507296124E-8,0.529924709245839,
-0.848044693710604));
#137190=DIRECTION('ref_axis',(0.0045332546887403,0.848035979777057,0.529919264233236));
#137191=DIRECTION('center_axis',(-2.89534733035821E-14,0.529924676825572,
-0.848044713969324));
#137192=DIRECTION('ref_axis',(6.64353622666922E-29,0.848044713969324,0.529924676825572));
#137193=DIRECTION('center_axis',(0.,-1.,-6.98296267768627E-15));
#137194=DIRECTION('ref_axis',(0.,6.98296267768627E-15,-1.));
#137195=DIRECTION('center_axis',(0.,1.,6.98296267768627E-15));
#137196=DIRECTION('ref_axis',(0.,-6.98296267768627E-15,1.));
#137197=DIRECTION('center_axis',(1.04744440165294E-14,-1.,-6.98296267768627E-15));
#137198=DIRECTION('ref_axis',(-1.,-1.04744440165294E-14,-1.34524652575182E-42));
#137199=DIRECTION('center_axis',(0.,-1.,-6.98296267768627E-15));
#137200=DIRECTION('ref_axis',(0.,6.98296267768627E-15,-1.));
#137201=DIRECTION('center_axis',(1.04744440165294E-14,-1.,-6.98296267768627E-15));
#137202=DIRECTION('ref_axis',(-1.,-1.04744440165294E-14,-1.34524652575182E-42));
#137203=DIRECTION('center_axis',(-3.44576744698565E-5,0.866037336481585,
0.49997933020531));
#137204=DIRECTION('ref_axis',(0.000963977573258117,-0.499979069431825,0.86603695121936));
#137205=DIRECTION('center_axis',(0.,-0.500005158533416,-0.866022425483298));
#137206=DIRECTION('ref_axis',(0.,0.866022425483298,-0.500005158533416));
#137207=DIRECTION('center_axis',(5.43770948728685E-15,-0.500005167508441,
-0.866022420301493));
#137208=DIRECTION('ref_axis',(1.,-1.39870616943407E-13,6.99353084717037E-14));
#137209=DIRECTION('center_axis',(-0.0522647557774501,0.49726593457756,-0.866022508721471));
#137210=DIRECTION('ref_axis',(-0.99452189536814,-0.104528463268923,-7.21207871993735E-13));
#137211=DIRECTION('center_axis',(-0.090493676372131,0.86127722484266,-0.50001243634932));
#137212=DIRECTION('ref_axis',(-0.0532497883196993,0.497169646240241,0.866017784402411));
#137213=DIRECTION('center_axis',(0.0522647566817887,-0.49726594318193,0.866022503726306));
#137214=DIRECTION('ref_axis',(5.67333325818785E-16,-0.867207748104371,-0.497946504785149));
#137215=DIRECTION('center_axis',(0.104528463267683,-0.99452189536827,-6.94470927749844E-15));
#137216=DIRECTION('ref_axis',(-0.99452189536827,-0.104528463267683,5.29715191372443E-32));
#137217=DIRECTION('center_axis',(-0.104528463267664,0.994521895368272,6.92998990261914E-15));
#137218=DIRECTION('ref_axis',(0.994521895368272,0.104528463267664,9.86230019548369E-32));
#137219=DIRECTION('center_axis',(-0.104528463267683,0.99452189536827,6.94470927749844E-15));
#137220=DIRECTION('ref_axis',(0.99452189536827,0.104528463267683,-5.29715191372443E-32));
#137221=DIRECTION('center_axis',(-0.104528463267664,0.994521895368272,6.92998990261914E-15));
#137222=DIRECTION('ref_axis',(0.994521895368272,0.104528463267664,-1.95579289036037E-31));
#137223=DIRECTION('center_axis',(0.104528463267682,-0.994521895368271,-6.94470927749844E-15));
#137224=DIRECTION('ref_axis',(-0.994521895368271,-0.104528463267682,9.97523142827348E-30));
#137225=DIRECTION('center_axis',(-0.055392163661009,0.527021232978627,0.848045003637566));
#137226=DIRECTION('ref_axis',(6.51171922772032E-16,-0.849349030019368,0.527831625809934));
#137227=DIRECTION('center_axis',(0.052264770847414,-0.497266077958576,-0.866022425483291));
#137228=DIRECTION('ref_axis',(-4.78888614370566E-17,0.86720767039808,-0.497946640115922));
#137229=DIRECTION('center_axis',(0.0553921822204516,-0.527021202610803,
-0.848045021297525));
#137230=DIRECTION('ref_axis',(0.092929914822725,-0.842941044394914,0.529919264233196));
#137231=DIRECTION('center_axis',(-0.0553921577943759,0.527021177161342,
0.848045038708651));
#137232=DIRECTION('ref_axis',(4.28784163588954E-16,-0.849349064867522,0.527831569734765));
#137233=DIRECTION('center_axis',(0.0522647827543777,-0.497266090635353,
-0.866022417485755));
#137234=DIRECTION('ref_axis',(0.0950466972129526,-0.860793892490479,0.5));
#137235=DIRECTION('center_axis',(0.0904912830030132,-0.861296695145195,
-0.499979330205193));
#137236=DIRECTION('ref_axis',(-0.0513033469930341,0.497340894869774,-0.86603695121943));
#137237=DIRECTION('center_axis',(0.994496518411991,0.104769627595163,-6.0604308970725E-15));
#137238=DIRECTION('ref_axis',(0.104769627595163,-0.994496518411991,-6.82961998416045E-15));
#137239=DIRECTION('center_axis',(-0.104528463267664,0.994521895368272,6.92998990261914E-15));
#137240=DIRECTION('ref_axis',(0.994521895368272,0.104528463267664,9.86230019548369E-32));
#137241=DIRECTION('center_axis',(0.104528463267628,-0.994521895368276,-6.94470927749848E-15));
#137242=DIRECTION('ref_axis',(-0.994521895368276,-0.104528463267628,1.09814391166396E-31));
#137243=DIRECTION('center_axis',(-1.26097532010602E-16,-7.12300817482632E-15,
1.));
#137244=DIRECTION('ref_axis',(0.,-1.,-7.12252768074091E-15));
#137245=DIRECTION('center_axis',(0.994547213842467,0.104287292793444,7.28234273333559E-16));
#137246=DIRECTION('ref_axis',(0.104287292793444,-0.994547213842467,-6.82961998416053E-15));
#137247=DIRECTION('center_axis',(0.0553922121162013,-0.527021693998998,
0.848044713969317));
#137248=DIRECTION('ref_axis',(4.11774601795882E-16,-0.849348742192401,-0.527832088960292));
#137249=DIRECTION('center_axis',(0.0553921577943754,-0.527021177161337,
-0.848045038708654));
#137250=DIRECTION('ref_axis',(-5.92818387691785E-16,0.849349064867525,-0.52783156973476));
#137251=DIRECTION('center_axis',(0.055392190456375,-0.527021729069563,0.848044693589302));
#137252=DIRECTION('ref_axis',(-0.0931523188057552,0.842916495802302,0.529919264233221));
#137253=DIRECTION('center_axis',(0.0553922189449272,-0.527021758969985,
0.848044673146728));
#137254=DIRECTION('ref_axis',(-1.43295946606909E-16,-0.849348701629302,
-0.527832154231455));
#137255=DIRECTION('center_axis',(-0.0553921822983099,0.527021202761856,
0.848045021198567));
#137256=DIRECTION('ref_axis',(0.0843581245724762,-0.843841975853982,0.529919264233205));
#137257=DIRECTION('center_axis',(0.0553921636610064,-0.527021232978603,
-0.848045003637582));
#137258=DIRECTION('ref_axis',(4.73641288854564E-16,0.849349030019383,-0.52783162580991));
#137259=DIRECTION('center_axis',(0.994494875050337,0.104785225574097,1.79858722714094E-15));
#137260=DIRECTION('ref_axis',(0.104785225574097,-0.994494875050337,-6.82961998416065E-15));
#137261=DIRECTION('center_axis',(0.104528463267683,-0.99452189536827,-7.658598959145E-15));
#137262=DIRECTION('ref_axis',(-0.99452189536827,-0.104528463267683,5.02333238162146E-32));
#137263=DIRECTION('center_axis',(-1.26097532010602E-16,-7.12300817482632E-15,
1.));
#137264=DIRECTION('ref_axis',(0.,-1.,-7.12427864012715E-15));
#137265=DIRECTION('center_axis',(0.994548849394382,0.104271693993677,-3.67176988898936E-16));
#137266=DIRECTION('ref_axis',(0.104271693993677,-0.994548849394382,-6.82961998416079E-15));
#137267=DIRECTION('center_axis',(0.104528463267664,-0.994521895368272,-6.92998990261914E-15));
#137268=DIRECTION('ref_axis',(-0.994521895368272,-0.104528463267664,-5.68846653078145E-30));
#137269=DIRECTION('center_axis',(0.090553431653363,-0.861270944310248,0.50001243634807));
#137270=DIRECTION('ref_axis',(0.0512812291155024,-0.497376550148729,-0.866017784403157));
#137271=DIRECTION('center_axis',(-0.0553922189449268,0.527021758969978,
-0.848044673146732));
#137272=DIRECTION('ref_axis',(-1.82739123987317E-17,0.849348701629307,0.527832154231448));
#137273=DIRECTION('center_axis',(-0.0522647452170547,0.497265930897975,
-0.866022511471594));
#137274=DIRECTION('ref_axis',(-0.0860712067688574,0.861737632557287,0.499999999999914));
#137275=DIRECTION('center_axis',(0.0522647566818046,-0.497265943181818,
0.866022503726369));
#137276=DIRECTION('ref_axis',(-6.46601314095184E-16,-0.867207748104435,
-0.497946504785037));
#137277=DIRECTION('center_axis',(-0.0553921903530692,0.527021728885246,
-0.848044693710594));
#137278=DIRECTION('ref_axis',(-0.0841354767237599,0.843864204093855,0.529919264233251));
#137279=DIRECTION('center_axis',(-0.0553922121162459,0.527021693998979,
-0.848044713969325));
#137280=DIRECTION('ref_axis',(-7.69598135871256E-16,0.849348742192412,0.527832088960275));
#137281=DIRECTION('center_axis',(0.104528463267683,-0.99452189536827,4.66790539311939E-14));
#137282=DIRECTION('ref_axis',(-0.99452189536827,-0.104528463267683,4.68802147627136E-31));
#137283=DIRECTION('center_axis',(-0.104528463267684,0.99452189536827,6.94470927749844E-15));
#137284=DIRECTION('ref_axis',(0.99452189536827,0.104528463267684,4.95746224200719E-30));
#137285=DIRECTION('center_axis',(0.104528463267664,-0.994521895368272,-6.92998990261914E-15));
#137286=DIRECTION('ref_axis',(-0.994521895368272,-0.104528463267664,-5.68846653078145E-30));
#137287=DIRECTION('center_axis',(0.104528463267683,-0.99452189536827,-1.62252751389037E-14));
#137288=DIRECTION('ref_axis',(-0.99452189536827,-0.104528463267683,2.5477722298887E-32));
#137289=DIRECTION('center_axis',(0.104528463267664,-0.994521895368272,-6.92998990261914E-15));
#137290=DIRECTION('ref_axis',(-0.994521895368272,-0.104528463267664,-5.68846653078145E-30));
#137291=DIRECTION('center_axis',(-0.0905598208268657,0.861289491529602,
0.499979330205246));
#137292=DIRECTION('ref_axis',(0.0532207405971731,-0.497139368681358,0.866036951219397));
#137293=DIRECTION('center_axis',(0.0522647708474102,-0.49726607795854,-0.866022425483312));
#137294=DIRECTION('ref_axis',(-4.9818014384587E-16,0.8672076703981,-0.497946640115886));
#137295=DIRECTION('center_axis',(0.0522647717853422,-0.497266086882506,
-0.866022420302607));
#137296=DIRECTION('ref_axis',(0.994521895368341,0.104528463267008,3.93386110152788E-13));
#137297=DIRECTION('center_axis',(-0.103956887952778,0.489078705150286,-0.86602250872347));
#137298=DIRECTION('ref_axis',(-0.97814760073492,-0.207911690812515,3.12086315513693E-12));
#137299=DIRECTION('center_axis',(-0.180025927304753,0.847099893162251,-0.500012436347904));
#137300=DIRECTION('ref_axis',(-0.104926459563228,0.488879980343774,0.866017784403182));
#137301=DIRECTION('center_axis',(0.103956889752339,-0.48907871361637,0.866022503726305));
#137302=DIRECTION('ref_axis',(2.04314265460328E-17,-0.870740345484702,-0.49174307391684));
#137303=DIRECTION('center_axis',(0.207911690817757,-0.978147600733806,-6.3113295077734E-14));
#137304=DIRECTION('ref_axis',(-0.978147600733806,-0.207911690817757,-1.09041577388121E-30));
#137305=DIRECTION('center_axis',(-0.20791169081777,0.978147600733803,6.80109070798531E-15));
#137306=DIRECTION('ref_axis',(0.978147600733803,0.20791169081777,2.06817330173051E-31));
#137307=DIRECTION('center_axis',(-0.207911690817757,0.978147600733806,9.67028386629166E-15));
#137308=DIRECTION('ref_axis',(0.978147600733806,0.207911690817757,2.88043565065189E-31));
#137309=DIRECTION('center_axis',(-0.20791169081777,0.978147600733803,6.80109070798531E-15));
#137310=DIRECTION('ref_axis',(0.978147600733803,0.20791169081777,-3.71899471142921E-31));
#137311=DIRECTION('center_axis',(0.207911690817754,-0.978147600733807,-6.83036818919254E-15));
#137312=DIRECTION('ref_axis',(-0.978147600733807,-0.207911690817754,1.95800148050649E-29));
#137313=DIRECTION('center_axis',(-0.110177439185351,0.518344097776635,0.848045003637592));
#137314=DIRECTION('ref_axis',(-7.54079398017999E-16,-0.853239582811879,
0.521519140898021));
#137315=DIRECTION('center_axis',(0.103956917928287,-0.489078846173993,-0.866022425483294));
#137316=DIRECTION('ref_axis',(-1.22527346747099E-16,0.870740269393781,-0.491743208652692));
#137317=DIRECTION('center_axis',(0.110177454462975,-0.518344065636496,-0.848045021297506));
#137318=DIRECTION('ref_axis',(0.180532167026837,-0.828609503966227,0.529919264233183));
#137319=DIRECTION('center_axis',(-0.110177427516368,0.518344042878384,0.848045038708657));
#137320=DIRECTION('ref_axis',(1.77194910663906E-17,-0.853239616987312,0.521519084984763));
#137321=DIRECTION('center_axis',(0.103956931096973,-0.489078857536295,-0.866022417485767));
#137322=DIRECTION('ref_axis',(0.184503484229001,-0.846143288283582,0.500000000000006));
#137323=DIRECTION('center_axis',(0.180025582247408,-0.847119506978821,-0.4999793302052));
#137324=DIRECTION('ref_axis',(-0.1030085813648,0.489253749385483,-0.866036951219438));
#137325=DIRECTION('center_axis',(0.978097154258593,0.208148881407615,1.45349587027152E-15));
#137326=DIRECTION('ref_axis',(0.208148881407615,-0.978097154258593,-6.82961998416083E-15));
#137327=DIRECTION('center_axis',(-0.20791169081777,0.978147600733803,6.80109070798531E-15));
#137328=DIRECTION('ref_axis',(0.978147600733803,0.20791169081777,2.06817330173051E-31));
#137329=DIRECTION('center_axis',(0.207911690817809,-0.978147600733795,-6.83036818919246E-15));
#137330=DIRECTION('ref_axis',(-0.978147600733795,-0.207911690817809,-7.01020655912049E-32));
#137331=DIRECTION('center_axis',(-1.11539425682701E-16,-7.12070239730339E-15,
1.));
#137332=DIRECTION('ref_axis',(0.,-1.,-7.12252768074091E-15));
#137333=DIRECTION('center_axis',(0.978197989689803,0.207674488001846,1.45018319882449E-15));
#137334=DIRECTION('ref_axis',(0.207674488001846,-0.978197989689803,-6.82961998416081E-15));
#137335=DIRECTION('center_axis',(0.110177535564859,-0.51834455120658,0.848044713969319));
#137336=DIRECTION('ref_axis',(1.07836950919692E-15,-0.853239300541042,-0.521519602711377));
#137337=DIRECTION('center_axis',(0.110177427516366,-0.518344042878376,-0.848045038708663));
#137338=DIRECTION('ref_axis',(-4.28442985045855E-16,0.853239616987318,-0.521519084984755));
#137339=DIRECTION('center_axis',(0.110177517683837,-0.51834458835035,0.848044693589279));
#137340=DIRECTION('ref_axis',(-0.180750786636256,0.828561842305646,0.529919264233193));
#137341=DIRECTION('center_axis',(0.110177549147491,-0.518344615107838,0.848044673146739));
#137342=DIRECTION('ref_axis',(-1.48578503604637E-15,-0.853239260760973,
-0.5215196677941));
#137343=DIRECTION('center_axis',(-0.110177454559654,0.518344065777824,0.848045021198563));
#137344=DIRECTION('ref_axis',(0.172101506923684,-0.83040149609036,0.529919264233232));
#137345=DIRECTION('center_axis',(0.110177439185354,-0.518344097776646,-0.848045003637586));
#137346=DIRECTION('ref_axis',(1.16028044961569E-15,0.853239582811873,-0.521519140898032));
#137347=DIRECTION('center_axis',(0.978093889466681,0.20816422216111,1.68001810364593E-14));
#137348=DIRECTION('ref_axis',(0.20816422216111,-0.978093889466681,-6.82961998416056E-15));
#137349=DIRECTION('center_axis',(0.207911690817757,-0.978147600733806,-6.02733794006349E-14));
#137350=DIRECTION('ref_axis',(-0.978147600733806,-0.207911690817757,-7.42579907703451E-31));
#137351=DIRECTION('center_axis',(-1.11539425682701E-16,-7.12070239730339E-15,
1.));
#137352=DIRECTION('ref_axis',(0.,-1.,-7.11677149719761E-15));
#137353=DIRECTION('center_axis',(0.978201246800563,0.207659145615657,-5.65545097522343E-16));
#137354=DIRECTION('ref_axis',(0.207659145615657,-0.978201246800563,-6.8296199841606E-15));
#137355=DIRECTION('center_axis',(0.20791169081777,-0.978147600733803,-6.80109070798531E-15));
#137356=DIRECTION('ref_axis',(-0.978147600733803,-0.20791169081777,-3.10040133675291E-30));
#137357=DIRECTION('center_axis',(0.18008469874673,-0.847087400907193,0.500012436346933));
#137358=DIRECTION('ref_axis',(0.102990311599812,-0.489291521296793,-0.866017784403787));
#137359=DIRECTION('center_axis',(-0.110177549147563,0.518344615107829,-0.848044673146735));
#137360=DIRECTION('ref_axis',(1.43134731509193E-15,0.853239260760976,0.521519667794094));
#137361=DIRECTION('center_axis',(-0.103956877074907,0.489078702596384,-0.866022511471538));
#137362=DIRECTION('ref_axis',(-0.175675810178005,0.84802005266285,0.499999999999998));
#137363=DIRECTION('center_axis',(0.103956889752269,-0.489078713616267,0.866022503726371));
#137364=DIRECTION('ref_axis',(1.23480565415998E-16,-0.870740345484762,-0.491743073916733));
#137365=DIRECTION('center_axis',(-0.110177517565485,0.518344588177,-0.848044693710611));
#137366=DIRECTION('ref_axis',(-0.171882402212725,0.830446875606225,0.529919264233187));
#137367=DIRECTION('center_axis',(-0.110177535564811,0.518344551206578,-0.848044713969326));
#137368=DIRECTION('ref_axis',(-1.34557089476936E-15,0.853239300541045,0.521519602711372));
#137369=DIRECTION('center_axis',(0.207911690817757,-0.978147600733806,-6.02733794006349E-14));
#137370=DIRECTION('ref_axis',(-0.978147600733806,-0.207911690817757,-7.42579907703451E-31));
#137371=DIRECTION('center_axis',(-0.207911690817757,0.978147600733806,6.83036818919254E-15));
#137372=DIRECTION('ref_axis',(0.978147600733806,0.207911690817757,-2.9624920046404E-32));
#137373=DIRECTION('center_axis',(0.20791169081777,-0.978147600733803,-6.80109070798531E-15));
#137374=DIRECTION('ref_axis',(-0.978147600733803,-0.20791169081777,-3.10040133675291E-30));
#137375=DIRECTION('center_axis',(0.207911690817757,-0.978147600733806,6.64920527619437E-14));
#137376=DIRECTION('ref_axis',(-0.978147600733806,-0.207911690817757,-8.88628001461481E-31));
#137377=DIRECTION('center_axis',(0.20791169081777,-0.978147600733803,-6.80109070798531E-15));
#137378=DIRECTION('ref_axis',(-0.978147600733803,-0.20791169081777,-3.10040133675291E-30));
#137379=DIRECTION('center_axis',(-0.180092991631637,0.847105178672107,0.499979330204825));
#137380=DIRECTION('ref_axis',(0.104894406035295,-0.488852904977225,0.866036951219652));
#137381=DIRECTION('center_axis',(0.103956917928286,-0.489078846173992,-0.866022425483294));
#137382=DIRECTION('ref_axis',(-1.63962562710755E-16,0.870740269393781,-0.491743208652692));
#137383=DIRECTION('center_axis',(0.103956919794063,-0.489078854951801,-0.866022420302134));
#137384=DIRECTION('ref_axis',(0.978147600733311,0.207911690820085,-1.38559329909464E-12));
#137385=DIRECTION('center_axis',(-0.154510046710727,0.475533027089821,-0.866022508721477));
#137386=DIRECTION('ref_axis',(-0.951056516296016,-0.309016994372293,1.60414114558784E-12));
#137387=DIRECTION('center_axis',(-0.267585776505592,0.823641557783929,-0.5000124363485));
#137388=DIRECTION('ref_axis',(-0.15545353447606,0.475234043095452,0.866017784402867));
#137389=DIRECTION('center_axis',(0.154510049384266,-0.475533035318153,0.866022503726304));
#137390=DIRECTION('ref_axis',(2.11507007819763E-15,-0.876548788012429,-0.481313018974079));
#137391=DIRECTION('center_axis',(0.309016994374964,-0.951056516295148,-6.64119215765934E-15));
#137392=DIRECTION('ref_axis',(-0.951056516295148,-0.309016994374964,-3.41480999208031E-15));
#137393=DIRECTION('center_axis',(-0.309016994374957,0.95105651629515,6.59767734033506E-15));
#137394=DIRECTION('ref_axis',(0.95105651629515,0.309016994374957,3.41480999208033E-15));
#137395=DIRECTION('center_axis',(-0.309016994374964,0.951056516295148,6.64119215765934E-15));
#137396=DIRECTION('ref_axis',(0.951056516295148,0.309016994374964,3.41480999208031E-15));
#137397=DIRECTION('center_axis',(-0.309016994374957,0.95105651629515,6.59767734033506E-15));
#137398=DIRECTION('ref_axis',(0.95105651629515,0.309016994374957,3.41480999208033E-15));
#137399=DIRECTION('center_axis',(0.309016994374914,-0.951056516295165,-6.64119215765945E-15));
#137400=DIRECTION('ref_axis',(-0.951056516295164,-0.309016994374914,-3.41480999208033E-15));
#137401=DIRECTION('center_axis',(-0.163755587629897,0.50398787616896,0.848045003637595));
#137402=DIRECTION('ref_axis',(1.40487114752366E-15,-0.859649462041503,0.510884333691839));
#137403=DIRECTION('center_axis',(0.154510091262001,-0.475533164204444,-0.866022425483265));
#137404=DIRECTION('ref_axis',(-1.76891705781139E-15,0.876548714628816,-0.481313152617472));
#137405=DIRECTION('center_axis',(0.163755599459163,-0.503987842609615,-0.848045021297499));
#137406=DIRECTION('ref_axis',(0.266156471021525,-0.805199544416117,0.529919264233191));
#137407=DIRECTION('center_axis',(-0.163755570286403,0.503987822791173,0.848045038708669));
#137408=DIRECTION('ref_axis',(-1.1219235501908E-15,-0.859649495083722,0.510884278092703));
#137409=DIRECTION('center_axis',(0.154510105545767,-0.475533174128097,-0.866022417485768));
#137410=DIRECTION('ref_axis',(0.271938812468096,-0.822222161142252,0.500000000000006));
#137411=DIRECTION('center_axis',(0.267587483540088,-0.823661100222747,-0.499979330205296));
#137412=DIRECTION('ref_axis',(-0.153585232136767,0.475806237445614,-0.866036951219371));
#137413=DIRECTION('center_axis',(0.950981553003154,0.309247612517397,2.15946453637257E-15));
#137414=DIRECTION('ref_axis',(0.309247612517397,-0.950981553003154,-6.82961998416078E-15));
#137415=DIRECTION('center_axis',(-0.309016994374957,0.95105651629515,6.59767734033506E-15));
#137416=DIRECTION('ref_axis',(0.95105651629515,0.309016994374957,3.41480999208033E-15));
#137417=DIRECTION('center_axis',(0.309016994374964,-0.951056516295148,-6.64119215765934E-15));
#137418=DIRECTION('ref_axis',(-0.951056516295148,-0.309016994374964,-3.41480999208031E-15));
#137419=DIRECTION('center_axis',(-9.73020895656121E-17,-7.11688751458844E-15,
1.));
#137420=DIRECTION('ref_axis',(0.,-1.,-7.11547567313622E-15));
#137421=DIRECTION('center_axis',(0.951131423661011,0.308786358061005,2.15624361371867E-15));
#137422=DIRECTION('ref_axis',(0.308786358061005,-0.95113142366101,-6.82961998416062E-15));
#137423=DIRECTION('center_axis',(0.16375573087775,-0.503988317040604,0.848044713969301));
#137424=DIRECTION('ref_axis',(-1.79468021185938E-15,-0.859649189130452,
-0.510884792910649));
#137425=DIRECTION('center_axis',(0.163755570286399,-0.503987822791161,-0.848045038708677));
#137426=DIRECTION('ref_axis',(5.47345787009395E-16,0.85964949508373,-0.51088427809269));
#137427=DIRECTION('center_axis',(0.163755716972381,-0.503988355851568,0.848044693589256));
#137428=DIRECTION('ref_axis',(-0.266368911014076,0.805129291877831,0.52991926423322));
#137429=DIRECTION('center_axis',(0.163755751065492,-0.503988379171997,0.848044673146739));
#137430=DIRECTION('ref_axis',(2.0062615550087E-15,-0.859649150669469,-0.510884857627686));
#137431=DIRECTION('center_axis',(-0.163755599576498,0.503987842737942,0.848045021198578));
#137432=DIRECTION('ref_axis',(0.257959309144535,-0.807862963763176,0.529919264233196));
#137433=DIRECTION('center_axis',(0.1637555876299,-0.503987876168967,-0.84804500363759));
#137434=DIRECTION('ref_axis',(-9.1753207598515E-16,0.859649462041498,-0.510884333691847));
#137435=DIRECTION('center_axis',(0.95097670255072,0.309262527968972,2.15956869041424E-15));
#137436=DIRECTION('ref_axis',(0.309262527968972,-0.95097670255072,-6.82961998416085E-15));
#137437=DIRECTION('center_axis',(0.309016994374964,-0.951056516295148,-1.50830667185733E-14));
#137438=DIRECTION('ref_axis',(-0.951056516295148,-0.309016994374964,-3.41480999208024E-15));
#137439=DIRECTION('center_axis',(-9.73020895656121E-17,-7.11688751458844E-15,
1.));
#137440=DIRECTION('ref_axis',(0.,-1.,-7.11677149719761E-15));
#137441=DIRECTION('center_axis',(0.951136266645023,0.308771440182812,-6.95712478733879E-15));
#137442=DIRECTION('ref_axis',(0.308771440182812,-0.951136266645023,-6.82961998416072E-15));
#137443=DIRECTION('center_axis',(0.309016994374957,-0.95105651629515,-6.59767734033506E-15));
#137444=DIRECTION('ref_axis',(-0.95105651629515,-0.309016994374957,-3.41480999208025E-15));
#137445=DIRECTION('center_axis',(0.267642920194009,-0.823622990674208,0.500012436348234));
#137446=DIRECTION('ref_axis',(0.153571010716873,-0.47584571214317,-0.866017784403044));
#137447=DIRECTION('center_axis',(-0.163755751065471,0.503988379172021,-0.848044673146729));
#137448=DIRECTION('ref_axis',(-1.04962869149324E-15,0.859649150669455,0.510884857627709));
#137449=DIRECTION('center_axis',(-0.15451003561906,0.475533025685345,-0.866022511471577));
#137450=DIRECTION('ref_axis',(-0.263355672632978,0.825011387613578,0.49999999999995));
#137451=DIRECTION('center_axis',(0.154510049384271,-0.475533035318085,0.86602250372634));
#137452=DIRECTION('ref_axis',(8.3687170438306E-16,-0.876548788012466,-0.481313018974011));
#137453=DIRECTION('center_axis',(-0.163755716852405,0.5039883556864,-0.848044693710582));
#137454=DIRECTION('ref_axis',(-0.257746148189121,0.807930997355695,0.529919264233246));
#137455=DIRECTION('center_axis',(-0.163755730877757,0.503988317040565,-0.848044713969323));
#137456=DIRECTION('ref_axis',(9.15490063314203E-17,0.859649189130475,0.51088479291061));
#137457=DIRECTION('center_axis',(0.309016994374964,-0.951056516295148,-6.64119215765934E-15));
#137458=DIRECTION('ref_axis',(-0.951056516295148,-0.309016994374964,-3.41480999208031E-15));
#137459=DIRECTION('center_axis',(-0.309016994374964,0.951056516295148,6.64119215765934E-15));
#137460=DIRECTION('ref_axis',(0.951056516295148,0.309016994374964,3.41480999208031E-15));
#137461=DIRECTION('center_axis',(0.309016994374957,-0.95105651629515,-6.59767734033506E-15));
#137462=DIRECTION('ref_axis',(-0.95105651629515,-0.309016994374957,-3.41480999208025E-15));
#137463=DIRECTION('center_axis',(0.309016994374964,-0.951056516295148,-2.35249412794872E-14));
#137464=DIRECTION('ref_axis',(-0.951056516295148,-0.309016994374964,-3.41480999208017E-15));
#137465=DIRECTION('center_axis',(0.309016994374957,-0.95105651629515,-6.59767734033506E-15));
#137466=DIRECTION('ref_axis',(-0.95105651629515,-0.309016994374957,-3.41480999208025E-15));
#137467=DIRECTION('center_axis',(-0.267653025932585,0.823639804208793,0.499979330204792));
#137468=DIRECTION('ref_axis',(0.155418826429222,-0.475210466544568,0.866036951219668));
#137469=DIRECTION('center_axis',(0.154510091261982,-0.475533164204414,-0.866022425483285));
#137470=DIRECTION('ref_axis',(8.44054174721563E-16,0.876548714628834,-0.48131315261744));
#137471=DIRECTION('center_axis',(0.154510094034416,-0.475533172737053,-0.866022420303371));
#137472=DIRECTION('ref_axis',(0.951056516293818,0.309016994379058,-2.46959058042575E-12));
#137473=DIRECTION('center_axis',(-0.203370361063309,0.456777309670355,-0.866022508720929));
#137474=DIRECTION('ref_axis',(-0.913545457642283,-0.406736643076513,-4.37095680000764E-13));
#137475=DIRECTION('center_axis',(-0.352213899942317,0.791159233140904,-0.500012436348658));
#137476=DIRECTION('ref_axis',(-0.20427742789601,0.456381342245913,0.866017784402843));
#137477=DIRECTION('center_axis',(0.203370364581912,-0.456777317573279,0.866022503726306));
#137478=DIRECTION('ref_axis',(8.71792903940306E-16,-0.884507036382095,-0.46652685087845));
#137479=DIRECTION('center_axis',(0.406736643075807,-0.913545457642598,-6.37925383508808E-15));
#137480=DIRECTION('ref_axis',(-0.913545457642598,-0.406736643075807,-3.4148099920803E-15));
#137481=DIRECTION('center_axis',(-0.40673664307581,0.913545457642596,6.32197843909135E-15));
#137482=DIRECTION('ref_axis',(0.913545457642596,0.40673664307581,3.41480999208033E-15));
#137483=DIRECTION('center_axis',(-0.406736643075807,0.913545457642598,6.37925383508808E-15));
#137484=DIRECTION('ref_axis',(0.913545457642598,0.406736643075807,3.4148099920803E-15));
#137485=DIRECTION('center_axis',(-0.40673664307581,0.913545457642596,6.32197843909135E-15));
#137486=DIRECTION('ref_axis',(0.913545457642596,0.40673664307581,3.41480999208033E-15));
#137487=DIRECTION('center_axis',(0.406736643075817,-0.913545457642594,-6.37925383508805E-15));
#137488=DIRECTION('ref_axis',(-0.913545457642593,-0.406736643075817,-3.41480999208037E-15));
#137489=DIRECTION('center_axis',(-0.215539595588313,0.484109857923779,0.848045003637569));
#137490=DIRECTION('ref_axis',(-7.52396283484213E-16,-0.868458021515989,
0.495762710240023));
#137491=DIRECTION('center_axis',(0.20337041970248,-0.456777441376077,-0.866022425483291));
#137492=DIRECTION('ref_axis',(2.06048551024826E-15,0.884506966812056,-0.466526982779063));
#137493=DIRECTION('center_axis',(0.215539603854002,-0.484109823307635,-0.84804502129752));
#137494=DIRECTION('ref_axis',(0.348864709048125,-0.772967650148034,0.529919264233141));
#137495=DIRECTION('center_axis',(-0.21553957276031,0.484109806651245,0.848045038708674));
#137496=DIRECTION('ref_axis',(-2.70827771329659E-15,-0.868458052949983,
0.495762655175159));
#137497=DIRECTION('center_axis',(0.203370434941407,-0.456777449754108,-0.866022417485758));
#137498=DIRECTION('ref_axis',(0.356394722166398,-0.789292595943951,0.499999999999994));
#137499=DIRECTION('center_axis',(0.352217640366812,-0.791178490090451,-0.499979330205389));
#137500=DIRECTION('ref_axis',(-0.202479170973359,0.457145692799023,-0.866036951219313));
#137501=DIRECTION('center_axis',(0.913446798847318,0.406958162070241,2.77957517046168E-14));
#137502=DIRECTION('ref_axis',(0.406958162070241,-0.913446798847317,-6.82961998416E-15));
#137503=DIRECTION('center_axis',(-0.40673664307581,0.913545457642596,6.32197843909135E-15));
#137504=DIRECTION('ref_axis',(0.913545457642596,0.40673664307581,3.41480999208033E-15));
#137505=DIRECTION('center_axis',(0.406736643075817,-0.913545457642594,-6.37925383508805E-15));
#137506=DIRECTION('ref_axis',(-0.913545457642593,-0.406736643075817,-3.41480999208037E-15));
#137507=DIRECTION('center_axis',(-8.35415108931894E-17,-7.11160532333482E-15,
1.));
#137508=DIRECTION('ref_axis',(0.,-1.,-7.10842366553152E-15));
#137509=DIRECTION('center_axis',(0.913644062717548,0.406515100163541,2.8386797723579E-15));
#137510=DIRECTION('ref_axis',(0.406515100163541,-0.913644062717548,-6.82961998416062E-15));
#137511=DIRECTION('center_axis',(0.215539784135082,-0.484110281406718,0.848044713969323));
#137512=DIRECTION('ref_axis',(1.68888390132495E-15,-0.868457761888286,-0.495763165045559));
#137513=DIRECTION('center_axis',(0.215539572760321,-0.484109806651269,-0.848045038708658));
#137514=DIRECTION('ref_axis',(-1.90731993212003E-15,0.868458052949969,-0.495762655175185));
#137515=DIRECTION('center_axis',(0.215539774370431,-0.484110321455134,0.848044693589289));
#137516=DIRECTION('ref_axis',(-0.349068641859116,0.772875576444986,0.529919264233206));
#137517=DIRECTION('center_axis',(0.215539810706709,-0.484110341087605,0.848044673146739));
#137518=DIRECTION('ref_axis',(1.28899452946971E-15,-0.868457725299272,-0.4957632291407));
#137519=DIRECTION('center_axis',(-0.215539603976693,0.484109823426323,0.848045021198583));
#137520=DIRECTION('ref_axis',(0.340990855195057,-0.776473315747487,0.529919264233192));
#137521=DIRECTION('center_axis',(0.215539595588318,-0.484109857923791,-0.848045003637562));
#137522=DIRECTION('ref_axis',(1.78938953355032E-15,0.868458021515983,-0.495762710240035));
#137523=DIRECTION('center_axis',(0.913440415876953,0.406972488803039,5.55993783434714E-15));
#137524=DIRECTION('ref_axis',(0.406972488803039,-0.913440415876953,-6.82961998416052E-15));
#137525=DIRECTION('center_axis',(0.406736643075807,-0.913545457642598,-1.74906806584517E-14));
#137526=DIRECTION('ref_axis',(-0.913545457642598,-0.406736643075807,-3.4148099920803E-15));
#137527=DIRECTION('center_axis',(-8.35415108931894E-17,-7.11160532333482E-15,
1.));
#137528=DIRECTION('ref_axis',(0.,-1.,-7.10926435426808E-15));
#137529=DIRECTION('center_axis',(0.913650438514062,0.40650077023674,2.83857970701388E-15));
#137530=DIRECTION('ref_axis',(0.40650077023674,-0.913650438514061,-6.8296199841608E-15));
#137531=DIRECTION('center_axis',(0.40673664307581,-0.913545457642596,-6.32197843909135E-15));
#137532=DIRECTION('ref_axis',(-0.913545457642596,-0.40673664307581,-3.41480999208034E-15));
#137533=DIRECTION('center_axis',(0.352268789801391,-0.791134794600527,0.500012436349583));
#137534=DIRECTION('ref_axis',(0.202469153669914,-0.457186437803249,-0.86601778440224));
#137535=DIRECTION('center_axis',(-0.215539810706676,0.484110341087625,-0.848044673146736));
#137536=DIRECTION('ref_axis',(1.37118570194245E-16,0.868457725299263,0.495763229140716));
#137537=DIRECTION('center_axis',(-0.203370349886521,0.456777309431526,-0.866022511471572));
#137538=DIRECTION('ref_axis',(-0.348150155226398,0.79296372515764,0.499999999999954));
#137539=DIRECTION('center_axis',(0.203370364581896,-0.456777317573244,0.866022503726329));
#137540=DIRECTION('ref_axis',(-2.3251588633511E-15,-0.884507036382115,-0.466526850878411));
#137541=DIRECTION('center_axis',(-0.215539774219281,0.484110321309935,-0.848044693710592));
#137542=DIRECTION('ref_axis',(-0.340785973386751,0.776563258039779,0.529919264233231));
#137543=DIRECTION('center_axis',(-0.215539784135111,0.484110281406703,-0.848044713969324));
#137544=DIRECTION('ref_axis',(-2.77729088551537E-15,0.868457761888292,0.495763165045546));
#137545=DIRECTION('center_axis',(0.406736643075807,-0.913545457642598,-6.37925383508808E-15));
#137546=DIRECTION('ref_axis',(-0.913545457642598,-0.406736643075807,-3.4148099920803E-15));
#137547=DIRECTION('center_axis',(-0.406736643075817,0.913545457642594,6.37925383508805E-15));
#137548=DIRECTION('ref_axis',(0.913545457642593,0.406736643075817,3.41480999208037E-15));
#137549=DIRECTION('center_axis',(0.40673664307581,-0.913545457642596,-6.32197843909135E-15));
#137550=DIRECTION('ref_axis',(-0.913545457642596,-0.40673664307581,-3.41480999208034E-15));
#137551=DIRECTION('center_axis',(0.406736643075807,-0.913545457642598,4.73217298827553E-15));
#137552=DIRECTION('ref_axis',(-0.913545457642598,-0.406736643075807,-3.4148099920803E-15));
#137553=DIRECTION('center_axis',(0.40673664307581,-0.913545457642596,-6.32197843909135E-15));
#137554=DIRECTION('ref_axis',(-0.913545457642596,-0.40673664307581,-3.41480999208034E-15));
#137555=DIRECTION('center_axis',(-0.352280597670873,0.791150459692824,0.499979330205246));
#137556=DIRECTION('ref_axis',(0.204240445635154,-0.456361522796734,0.866036951219404));
#137557=DIRECTION('center_axis',(0.203370419702468,-0.456777441376063,-0.866022425483301));
#137558=DIRECTION('ref_axis',(1.64733859252707E-15,0.884506966812064,-0.466526982779048));
#137559=DIRECTION('center_axis',(0.203370423353679,-0.456777449576814,-0.866022420300448));
#137560=DIRECTION('ref_axis',(0.913545457642565,0.406736643075882,-5.24514813535308E-14));
#137561=DIRECTION('center_axis',(-0.250002507181017,0.433017044457075,-0.866022508721838));
#137562=DIRECTION('ref_axis',(-0.866025403783246,-0.500000000002066,-1.35499660801461E-12));
#137563=DIRECTION('center_axis',(-0.432983094186388,0.750008802378924,-0.50001243634825));
#137564=DIRECTION('ref_axis',(-0.250863215143673,0.432528431880919,0.866017784403076));
#137565=DIRECTION('center_axis',(0.250002511507219,-0.433017051950273,0.866022503726305));
#137566=DIRECTION('ref_axis',(-3.84832814192959E-16,-0.894424794863785,
-0.447218387740124));
#137567=DIRECTION('center_axis',(0.499999999999998,-0.86602540378444,-6.04742307255492E-15));
#137568=DIRECTION('ref_axis',(-0.86602540378444,-0.499999999999998,-3.41480999208026E-15));
#137569=DIRECTION('center_axis',(-0.50000000000001,0.866025403784433,5.97701461910992E-15));
#137570=DIRECTION('ref_axis',(0.866025403784433,0.50000000000001,3.41480999208033E-15));
#137571=DIRECTION('center_axis',(-0.50000000000001,0.866025403784433,6.04742307255487E-15));
#137572=DIRECTION('ref_axis',(0.866025403784433,0.50000000000001,3.41480999208034E-15));
#137573=DIRECTION('center_axis',(-0.50000000000001,0.866025403784433,5.97701461910992E-15));
#137574=DIRECTION('ref_axis',(0.866025403784433,0.50000000000001,3.41480999208033E-15));
#137575=DIRECTION('center_axis',(0.499999999999998,-0.86602540378444,-6.04742307255492E-15));
#137576=DIRECTION('ref_axis',(-0.86602540378444,-0.499999999999998,-3.41480999208026E-15));
#137577=DIRECTION('center_axis',(-0.264962106632877,0.458927830768622,0.848045003637587));
#137578=DIRECTION('ref_axis',(9.35163036390063E-16,-0.879478602053334,0.475938429348076));
#137579=DIRECTION('center_axis',(0.250002579266714,-0.433017169313211,-0.866022425483292));
#137580=DIRECTION('ref_axis',(-1.20805579666634E-15,0.894424730216419,-0.447218517033101));
#137581=DIRECTION('center_axis',(0.264962111232149,-0.458927795479733,-0.848045021297522));
#137582=DIRECTION('ref_axis',(0.427750712282121,-0.732266960566111,0.529919264233154));
#137583=DIRECTION('center_axis',(-0.264962078570518,0.45892778216319,0.848045038708656));
#137584=DIRECTION('ref_axis',(1.63750655949806E-15,-0.879478631391259,0.475938375135015));
#137585=DIRECTION('center_axis',(0.250002595299433,-0.433017176051559,-0.86602241748576));
#137586=DIRECTION('ref_axis',(0.436945896705958,-0.747715375896346,0.500000000000012));
#137587=DIRECTION('center_axis',(0.432988827019088,-0.750027562856358,-0.499979330205146));
#137588=DIRECTION('ref_axis',(-0.249154705663389,0.433476564266486,-0.866036951219469));
#137589=DIRECTION('center_axis',(0.865904130412325,0.500209992837883,3.49294771099265E-15));
#137590=DIRECTION('ref_axis',(0.500209992837883,-0.865904130412325,-6.82961998416073E-15));
#137591=DIRECTION('center_axis',(-0.50000000000001,0.866025403784433,5.97701461910992E-15));
#137592=DIRECTION('ref_axis',(0.866025403784433,0.50000000000001,3.41480999208033E-15));
#137593=DIRECTION('center_axis',(0.50000000000001,-0.866025403784433,-6.04742307255487E-15));
#137594=DIRECTION('ref_axis',(-0.866025403784433,-0.50000000000001,-3.41480999208034E-15));
#137595=DIRECTION('center_axis',(-7.04084534449538E-17,-7.10491369633528E-15,
1.));
#137596=DIRECTION('ref_axis',(0.,-1.,-7.10137165792683E-15));
#137597=DIRECTION('center_axis',(0.866146626230604,0.499789977760002,3.49001476137974E-15));
#137598=DIRECTION('ref_axis',(0.499789977760002,-0.866146626230603,-6.82961998416084E-15));
#137599=DIRECTION('center_axis',(0.264962338412816,-0.4589282322232,0.848044713969317));
#137600=DIRECTION('ref_axis',(-1.10874842197371E-15,-0.879478359737745,
-0.475938877118696));
#137601=DIRECTION('center_axis',(0.264962078570517,-0.458927782163174,-0.848045038708665));
#137602=DIRECTION('ref_axis',(-2.83667081435709E-15,0.879478631391268,-0.475938375134998));
#137603=DIRECTION('center_axis',(0.264962332884999,-0.45892827307457,0.848044693589278));
#137604=DIRECTION('ref_axis',(-0.427943903624788,0.732154074457648,0.529919264233188));
#137605=DIRECTION('center_axis',(0.264962371077225,-0.458928288799667,0.84804467314673));
#137606=DIRECTION('ref_axis',(-1.18836456492387E-15,-0.879478325588502,
-0.475938940222425));
#137607=DIRECTION('center_axis',(-0.264962111371018,0.458927795582427,0.84804502119856));
#137608=DIRECTION('ref_axis',(0.420286434057206,-0.736576463608523,0.529919264233185));
#137609=DIRECTION('center_axis',(0.264962106632849,-0.45892783076856,-0.848045003637629));
#137610=DIRECTION('ref_axis',(1.23612151778348E-15,0.879478602053371,-0.475938429348007));
#137611=DIRECTION('center_axis',(0.86589628485713,0.500223573885338,-2.01619277381436E-14));
#137612=DIRECTION('ref_axis',(0.500223573885338,-0.86589628485713,-6.82961998416088E-15));
#137613=DIRECTION('center_axis',(0.50000000000001,-0.866025403784433,-6.04742307255487E-15));
#137614=DIRECTION('ref_axis',(-0.866025403784433,-0.50000000000001,-3.41480999208034E-15));
#137615=DIRECTION('center_axis',(-7.04084534449538E-17,-7.10491369633528E-15,
1.));
#137616=DIRECTION('ref_axis',(0.,-1.,-7.10175721133855E-15));
#137617=DIRECTION('center_axis',(0.866154464985094,0.499776392786199,3.4899198980147E-15));
#137618=DIRECTION('ref_axis',(0.499776392786199,-0.866154464985094,-6.82961998416057E-15));
#137619=DIRECTION('center_axis',(0.50000000000001,-0.866025403784433,-5.97701461910992E-15));
#137620=DIRECTION('ref_axis',(-0.866025403784433,-0.50000000000001,-3.41480999208034E-15));
#137621=DIRECTION('center_axis',(0.433035128828067,-0.749978760164922,0.500012436347684));
#137622=DIRECTION('ref_axis',(0.249149002219344,-0.433518133173526,-0.866017784403326));
#137623=DIRECTION('center_axis',(-0.264962371077261,0.458928288799635,-0.848044673146736));
#137624=DIRECTION('ref_axis',(-7.08699178131369E-16,0.879478325588517,0.475938940222397));
#137625=DIRECTION('center_axis',(-0.250002496036225,0.433017045392176,-0.866022511471548));
#137626=DIRECTION('ref_axis',(-0.429130231857386,0.752228186194869,0.500000000000003));
#137627=DIRECTION('center_axis',(0.250002511507148,-0.433017051950198,0.866022503726363));
#137628=DIRECTION('ref_axis',(-1.69037570385203E-15,-0.894424794863828,
-0.447218387740038));
#137629=DIRECTION('center_axis',(-0.264962332727107,0.458928272941578,-0.848044693710579));
#137630=DIRECTION('ref_axis',(-0.42009207616774,0.736687329153668,0.529919264233253));
#137631=DIRECTION('center_axis',(-0.264962338412833,0.458928232223187,-0.848044713969319));
#137632=DIRECTION('ref_axis',(7.6134706593656E-16,0.879478359737751,0.475938877118685));
#137633=DIRECTION('center_axis',(0.50000000000001,-0.866025403784433,-1.9706663040877E-14));
#137634=DIRECTION('ref_axis',(-0.866025403784433,-0.50000000000001,-3.41480999208034E-15));
#137635=DIRECTION('center_axis',(-0.500000000000034,0.866025403784419,6.04742307255478E-15));
#137636=DIRECTION('ref_axis',(0.866025403784419,0.500000000000034,3.4148099920805E-15));
#137637=DIRECTION('center_axis',(0.50000000000001,-0.866025403784433,-5.97701461910992E-15));
#137638=DIRECTION('ref_axis',(-0.866025403784433,-0.50000000000001,-3.41480999208034E-15));
#137639=DIRECTION('center_axis',(0.50000000000001,-0.866025403784433,-3.97051783400485E-14));
#137640=DIRECTION('ref_axis',(-0.866025403784433,-0.50000000000001,-3.41480999208034E-15));
#137641=DIRECTION('center_axis',(0.50000000000001,-0.866025403784433,-5.97701461910992E-15));
#137642=DIRECTION('ref_axis',(-0.866025403784433,-0.50000000000001,-3.41480999208034E-15));
#137643=DIRECTION('center_axis',(-0.433048509462458,0.749993105181527,0.499979330205273));
#137644=DIRECTION('ref_axis',(0.25082436377922,-0.432512586703996,0.866036951219385));
#137645=DIRECTION('center_axis',(0.250002579266705,-0.433017169313181,-0.86602242548331));
#137646=DIRECTION('ref_axis',(-2.67459257803907E-15,0.894424730216435,-0.447218517033068));
#137647=DIRECTION('center_axis',(0.250002583751534,-0.433017177081167,-0.866022420304587));
#137648=DIRECTION('ref_axis',(0.866025403782456,0.500000000003435,-2.2860103956705E-12));
#137649=DIRECTION('center_axis',(-0.293895573515241,0.404512553892875,-0.866022508720883));
#137650=DIRECTION('ref_axis',(-0.809016994377429,-0.587785252289058,2.43025198077899E-12));
#137651=DIRECTION('center_axis',(-0.509008435042384,0.700641118228627,-0.500012436348379));
#137652=DIRECTION('ref_axis',(-0.294700492557513,0.403936649468912,0.866017784402947));
#137653=DIRECTION('center_axis',(0.293895578599988,-0.404512560891486,0.866022503726312));
#137654=DIRECTION('ref_axis',(-2.42787896315404E-15,-0.906035256115475,
-0.42320221487578));
#137655=DIRECTION('center_axis',(0.587785252292496,-0.809016994374931,-5.64933547733406E-15));
#137656=DIRECTION('ref_axis',(-0.809016994374931,-0.587785252292496,-3.41480999208037E-15));
#137657=DIRECTION('center_axis',(-0.587785252292482,0.809016994374941,5.5665653761908E-15));
#137658=DIRECTION('ref_axis',(0.809016994374941,0.587785252292482,3.41480999208033E-15));
#137659=DIRECTION('center_axis',(-0.587785252292496,0.809016994374931,3.77641347209492E-14));
#137660=DIRECTION('ref_axis',(0.809016994374931,0.587785252292496,3.41480999208037E-15));
#137661=DIRECTION('center_axis',(-0.587785252292482,0.809016994374941,5.5665653761908E-15));
#137662=DIRECTION('ref_axis',(0.809016994374941,0.587785252292482,3.41480999208033E-15));
#137663=DIRECTION('center_axis',(0.58778525229247,-0.80901699437495,-5.6493354773342E-15));
#137664=DIRECTION('ref_axis',(-0.80901699437495,-0.58778525229247,-3.41480999208022E-15));
#137665=DIRECTION('center_axis',(-0.31148163739031,0.42871769426275,0.848045003637591));
#137666=DIRECTION('ref_axis',(1.10162827415622E-15,-0.892442058026276,0.451162025292273));
#137667=DIRECTION('center_axis',(0.293895658256118,-0.404512670528665,-0.866022425483296));
#137668=DIRECTION('ref_axis',(-1.88316153394377E-15,0.906035197473502,-0.423202340422584));
#137669=DIRECTION('center_axis',(0.311481638275178,-0.428717658686835,-0.848045021297507));
#137670=DIRECTION('ref_axis',(0.501950189207944,-0.683543400925387,0.529919264233208));
#137671=DIRECTION('center_axis',(-0.311481604401037,0.428717648856911,0.848045038708652));
#137672=DIRECTION('ref_axis',(1.88777093301588E-15,-0.89244208477774,0.451161972375289));
#137673=DIRECTION('center_axis',(0.293895674908356,-0.404512675552017,-0.866022417485778));
#137674=DIRECTION('ref_axis',(0.512709800578015,-0.697946029712376,0.499999999999983));
#137675=DIRECTION('center_axis',(0.509016097474398,-0.700659176689513,-0.499979330205468));
#137676=DIRECTION('ref_axis',(-0.293100449228649,0.405058175802929,-0.866036951219269));
#137677=DIRECTION('center_axis',(0.808874435122379,0.587981418248444,4.10585229880193E-15));
#137678=DIRECTION('ref_axis',(0.587981418248444,-0.808874435122379,-6.82961998416087E-15));
#137679=DIRECTION('center_axis',(-0.587785252292482,0.809016994374941,5.5665653761908E-15));
#137680=DIRECTION('ref_axis',(0.809016994374941,0.587785252292482,3.41480999208033E-15));
#137681=DIRECTION('center_axis',(0.58778525229247,-0.80901699437495,-5.6493354773342E-15));
#137682=DIRECTION('ref_axis',(-0.80901699437495,-0.58778525229247,-3.41480999208022E-15));
#137683=DIRECTION('center_axis',(-5.80468057465775E-17,-7.09688594845552E-15,
1.));
#137684=DIRECTION('ref_axis',(0.,-1.,-7.09431965032213E-15));
#137685=DIRECTION('center_axis',(0.809159506053906,0.587589051772239,4.10311241834261E-15));
#137686=DIRECTION('ref_axis',(0.587589051772239,-0.809159506053906,-6.82961998416078E-15));
#137687=DIRECTION('center_axis',(0.3114819098639,-0.428718069290563,0.848044713969322));
#137688=DIRECTION('ref_axis',(2.56903958782145E-15,-0.892441837073384,-0.451162462358166));
#137689=DIRECTION('center_axis',(0.311481604401026,-0.428717648856896,-0.848045038708663));
#137690=DIRECTION('ref_axis',(-3.17710353883337E-15,0.892442084777749,-0.451161972375272));
#137691=DIRECTION('center_axis',(0.311481908636171,-0.428718110496195,0.848044693589283));
#137692=DIRECTION('ref_axis',(-0.502130522419991,0.683410939222361,0.529919264233183));
#137693=DIRECTION('center_axis',(0.311481948263223,-0.428718122142737,0.848044673146735));
#137694=DIRECTION('ref_axis',(-2.52135914302017E-15,-0.892441805934762,
-0.451162523953289));
#137695=DIRECTION('center_axis',(-0.311481638421796,0.428717658776018,0.84804502119857));
#137696=DIRECTION('ref_axis',(0.494977266825156,-0.688609525580972,0.529919264233192));
#137697=DIRECTION('center_axis',(0.311481637390356,-0.428717694262813,-0.848045003637543));
#137698=DIRECTION('ref_axis',(-3.15651889012676E-15,0.892442058026239,-0.451162025292347));
#137699=DIRECTION('center_axis',(0.808865212939996,0.58799410481359,3.62321511990407E-14));
#137700=DIRECTION('ref_axis',(0.58799410481359,-0.808865212939996,-6.82961998416104E-15));
#137701=DIRECTION('center_axis',(0.587785252292496,-0.809016994374931,2.64654637662811E-14));
#137702=DIRECTION('ref_axis',(-0.809016994374931,-0.587785252292496,-3.41480999208037E-15));
#137703=DIRECTION('center_axis',(-5.80468057465775E-17,-7.09688594845552E-15,
1.));
#137704=DIRECTION('ref_axis',(0.,-1.,-7.09425006840901E-15));
#137705=DIRECTION('center_axis',(0.80916872188328,0.587576360591353,3.62064098324204E-14));
#137706=DIRECTION('ref_axis',(0.587576360591353,-0.80916872188328,-6.82961998416123E-15));
#137707=DIRECTION('center_axis',(0.587785252292482,-0.809016994374941,-5.5665653761908E-15));
#137708=DIRECTION('ref_axis',(-0.809016994374941,-0.587785252292482,-3.41480999208029E-15));
#137709=DIRECTION('center_axis',(0.509057044368145,-0.700605801485404,0.500012436349499));
#137710=DIRECTION('ref_axis',(0.293099122177626,-0.40510011315436,-0.866017784402278));
#137711=DIRECTION('center_axis',(-0.311481948263288,0.428718122142708,-0.848044673146725));
#137712=DIRECTION('ref_axis',(1.36579927504424E-15,0.892441805934771,0.451162523953269));
#137713=DIRECTION('center_axis',(-0.293895562539147,0.404512555978629,-0.866022511471518));
#137714=DIRECTION('ref_axis',(-0.505408667900667,0.703251077788578,0.500000000000076));
#137715=DIRECTION('center_axis',(0.293895578599968,-0.404512560891393,0.866022503726362));
#137716=DIRECTION('ref_axis',(2.61834824672012E-15,-0.906035256115521,-0.423202214875681));
#137717=DIRECTION('center_axis',(-0.311481908458697,0.428718110385103,-0.848044693710629));
#137718=DIRECTION('ref_axis',(-0.494795562240512,0.688740099734032,0.529919264233196));
#137719=DIRECTION('center_axis',(-0.311481909863969,0.428718069290501,-0.848044713969328));
#137720=DIRECTION('ref_axis',(9.41989347612634E-16,0.892441837073413,0.45116246235811));
#137721=DIRECTION('center_axis',(0.587785252292496,-0.809016994374931,-5.64933547733406E-15));
#137722=DIRECTION('ref_axis',(-0.809016994374931,-0.587785252292496,-3.41480999208037E-15));
#137723=DIRECTION('center_axis',(-0.587785252292496,0.809016994374931,5.64933547733406E-15));
#137724=DIRECTION('ref_axis',(0.809016994374931,0.587785252292496,3.41480999208037E-15));
#137725=DIRECTION('center_axis',(0.587785252292482,-0.809016994374941,-5.5665653761908E-15));
#137726=DIRECTION('ref_axis',(-0.809016994374941,-0.587785252292482,-3.41480999208029E-15));
#137727=DIRECTION('center_axis',(0.587785252292496,-0.809016994374931,3.85528935811342E-14));
#137728=DIRECTION('ref_axis',(-0.809016994374931,-0.587785252292496,-3.41480999208037E-15));
#137729=DIRECTION('center_axis',(0.587785252292482,-0.809016994374941,-5.5665653761908E-15));
#137730=DIRECTION('ref_axis',(-0.809016994374941,-0.587785252292482,-3.41480999208029E-15));
#137731=DIRECTION('center_axis',(-0.50907185116305,0.700618669263803,0.499979330205204));
#137732=DIRECTION('ref_axis',(0.294660197697693,-0.403924952206856,0.86603695121943));
#137733=DIRECTION('center_axis',(0.293895658256114,-0.40451267052866,-0.8660224254833));
#137734=DIRECTION('ref_axis',(-2.92311624756912E-15,0.906035197473505,-0.423202340422578));
#137735=DIRECTION('center_axis',(0.293895663531775,-0.404512677789947,-0.866022420301244));
#137736=DIRECTION('ref_axis',(0.809016994371858,0.587785252296726,-2.98536348044732E-12));
#137737=DIRECTION('center_axis',(-0.334568658444528,0.371576139138116,-0.866022508720091));
#137738=DIRECTION('ref_axis',(-0.743144825479581,-0.669130606356429,1.87514046718231E-12));
#137739=DIRECTION('center_axis',(-0.579456972967815,0.64359706336816,-0.500012436348195));
#137740=DIRECTION('ref_axis',(-0.335308969634739,0.370919252641439,0.866017784403072));
#137741=DIRECTION('center_axis',(0.334568664232119,-0.371576145565826,0.866022503726306));
#137742=DIRECTION('ref_axis',(3.65930929999324E-16,-0.918982183096522,-0.394299058014537));
#137743=DIRECTION('center_axis',(0.669130606358875,-0.743144825477379,-5.18935258042421E-15));
#137744=DIRECTION('ref_axis',(-0.743144825477379,-0.669130606358875,-3.41480999208015E-15));
#137745=DIRECTION('center_axis',(-0.669130606358867,0.743144825477386,5.09512767813144E-15));
#137746=DIRECTION('ref_axis',(0.743144825477386,0.669130606358867,3.41480999208033E-15));
#137747=DIRECTION('center_axis',(-0.669130606358845,0.743144825477406,-3.54138214292235E-14));
#137748=DIRECTION('ref_axis',(0.743144825477406,0.669130606358845,3.41480999208033E-15));
#137749=DIRECTION('center_axis',(-0.669130606358867,0.743144825477386,5.09512767813144E-15));
#137750=DIRECTION('ref_axis',(0.743144825477386,0.669130606358867,3.41480999208033E-15));
#137751=DIRECTION('center_axis',(0.669130606358845,-0.743144825477406,-5.1893525804244E-15));
#137752=DIRECTION('ref_axis',(-0.743144825477406,-0.669130606358845,-3.41480999208033E-15));
#137753=DIRECTION('center_axis',(-0.354588510146749,0.393810436983626,0.848045003637587));
#137754=DIRECTION('ref_axis',(-2.37537055868933E-15,-0.906978223357771,
0.421177518814551));
#137755=DIRECTION('center_axis',(0.334568754912034,-0.371576246276106,-0.866022425483295));
#137756=DIRECTION('ref_axis',(1.32125764084643E-15,0.91898213146365,-0.394299178353857));
#137757=DIRECTION('center_axis',(0.354588507311481,-0.393810401507025,-0.848045021297509));
#137758=DIRECTION('ref_axis',(0.570650194834968,-0.627330796732771,0.529919264233185));
#137759=DIRECTION('center_axis',(-0.354588472592004,0.393810395274856,0.848045038708635));
#137760=DIRECTION('ref_axis',(1.94126359720515E-15,-0.906978247051288,0.421177467792109));
#137761=DIRECTION('center_axis',(0.334568771994927,-0.371576249534259,-0.866022417485749));
#137762=DIRECTION('ref_axis',(0.582856348568798,-0.640529840782626,0.500000000000032));
#137763=DIRECTION('center_axis',(0.579466481046765,-0.643614221961121,-0.49997933020542));
#137764=DIRECTION('ref_axis',(-0.333834922954767,0.372201885189424,-0.866036951219302));
#137765=DIRECTION('center_axis',(0.742982542253377,0.669310796197633,8.18371867718752E-14));
#137766=DIRECTION('ref_axis',(0.669310796197633,-0.742982542253377,-6.82961998416045E-15));
#137767=DIRECTION('center_axis',(-0.669130606358867,0.743144825477386,5.09512767813144E-15));
#137768=DIRECTION('ref_axis',(0.743144825477386,0.669130606358867,3.41480999208033E-15));
#137769=DIRECTION('center_axis',(0.669130606358845,-0.743144825477406,-5.1893525804244E-15));
#137770=DIRECTION('ref_axis',(-0.743144825477406,-0.669130606358845,-3.41480999208033E-15));
#137771=DIRECTION('center_axis',(-4.65920045970846E-17,-7.08761003338124E-15,
1.));
#137772=DIRECTION('ref_axis',(0.,-1.,-7.08726764271744E-15));
#137773=DIRECTION('center_axis',(0.743307065001304,0.668950377172438,4.67125551701929E-15));
#137774=DIRECTION('ref_axis',(0.668950377172438,-0.743307065001304,-6.82961998416086E-15));
#137775=DIRECTION('center_axis',(0.354588820328836,-0.393810781475676,0.84804471396933));
#137776=DIRECTION('ref_axis',(-9.24151213041885E-16,-0.906978027661855,
-0.421177940232642));
#137777=DIRECTION('center_axis',(0.354588472592016,-0.39381039527487,-0.848045038708624));
#137778=DIRECTION('ref_axis',(-1.09907770159185E-15,0.90697824705128,-0.421177467792125));
#137779=DIRECTION('center_axis',(0.354588823405941,-0.393810822592156,0.848044693589247));
#137780=DIRECTION('ref_axis',(-0.570815694152314,0.627180210708223,0.529919264233149));
#137781=DIRECTION('center_axis',(0.354588864042302,-0.393810830024569,0.848044673146734));
#137782=DIRECTION('ref_axis',(-3.45243234032312E-15,-0.906978000082629,
-0.421177999622623));
#137783=DIRECTION('center_axis',(-0.35458850746671,0.393810401580338,0.848045021198559));
#137784=DIRECTION('ref_axis',(0.564245025061867,-0.633098037500908,0.529919264233177));
#137785=DIRECTION('center_axis',(0.354588510146734,-0.393810436983609,-0.848045003637601));
#137786=DIRECTION('ref_axis',(1.15170691571856E-15,0.90697822335778,-0.421177518814531));
#137787=DIRECTION('center_axis',(0.742972044483923,0.669322449283885,6.49863705058814E-16));
#137788=DIRECTION('ref_axis',(0.669322449283885,-0.742972044483923,-6.82961998416066E-15));
#137789=DIRECTION('center_axis',(0.669130606358845,-0.743144825477406,-4.57925265900746E-14));
#137790=DIRECTION('ref_axis',(-0.743144825477406,-0.669130606358845,-3.41480999208032E-15));
#137791=DIRECTION('center_axis',(-4.65920045970846E-17,-7.08761003338124E-15,
1.));
#137792=DIRECTION('ref_axis',(0.,-1.,-7.08674292547948E-15));
#137793=DIRECTION('center_axis',(0.743317556935059,0.668938718831625,4.6711741072605E-15));
#137794=DIRECTION('ref_axis',(0.668938718831625,-0.743317556935059,-6.82961998416081E-15));
#137795=DIRECTION('center_axis',(0.669130606358867,-0.743144825477386,-5.09512767813144E-15));
#137796=DIRECTION('ref_axis',(-0.743144825477386,-0.669130606358867,-3.41480999208029E-15));
#137797=DIRECTION('center_axis',(0.579501624400542,-0.643556859037129,0.500012436348735));
#137798=DIRECTION('ref_axis',(0.333837986832196,-0.372243731506654,-0.866017784402739));
#137799=DIRECTION('center_axis',(-0.354588864042398,0.393810830024473,-0.848044673146738));
#137800=DIRECTION('ref_axis',(-2.5025141110171E-15,0.906978000082668,0.421177999622539));
#137801=DIRECTION('center_axis',(-0.334568647735589,0.371576142367659,-0.866022511471583));
#137802=DIRECTION('ref_axis',(-0.576149740773897,0.646569003437538,0.49999999999996));
#137803=DIRECTION('center_axis',(0.334568664232095,-0.371576145565871,0.866022503726296));
#137804=DIRECTION('ref_axis',(-1.84625828909707E-15,-0.918982183096503,
-0.39429905801458));
#137805=DIRECTION('center_axis',(-0.354588823230568,0.39381082248875,-0.848044693710594));
#137806=DIRECTION('ref_axis',(-0.564077964602082,0.633246889644838,0.529919264233251));
#137807=DIRECTION('center_axis',(-0.354588820328848,0.393810781475689,-0.848044713969318));
#137808=DIRECTION('ref_axis',(1.80372274773434E-15,0.906978027661848,0.421177940232658));
#137809=DIRECTION('center_axis',(0.669130606358845,-0.743144825477406,-4.1748614670039E-14));
#137810=DIRECTION('ref_axis',(-0.743144825477406,-0.669130606358845,-3.41480999208033E-15));
#137811=DIRECTION('center_axis',(-0.669130606358872,0.743144825477382,5.18935258042423E-15));
#137812=DIRECTION('ref_axis',(0.743144825477382,0.669130606358872,3.41480999208052E-15));
#137813=DIRECTION('center_axis',(0.669130606358867,-0.743144825477386,-5.09512767813144E-15));
#137814=DIRECTION('ref_axis',(-0.743144825477386,-0.669130606358867,-3.41480999208029E-15));
#137815=DIRECTION('center_axis',(0.669130606358845,-0.743144825477406,-4.1748614670037E-14));
#137816=DIRECTION('ref_axis',(-0.743144825477406,-0.669130606358845,-3.41480999208033E-15));
#137817=DIRECTION('center_axis',(0.669130606358867,-0.743144825477386,-5.09512767813144E-15));
#137818=DIRECTION('ref_axis',(-0.743144825477386,-0.669130606358867,-3.41480999208029E-15));
#137819=DIRECTION('center_axis',(-0.579517695131704,0.643568108591944,0.499979330205385));
#137820=DIRECTION('ref_axis',(0.335267672838309,-0.370911831399768,0.86603695121932));
#137821=DIRECTION('center_axis',(0.33456875491201,-0.371576246276107,-0.866022425483304));
#137822=DIRECTION('ref_axis',(1.31994420604537E-15,0.918982131463651,-0.394299178353854));
#137823=DIRECTION('center_axis',(0.334568760915655,-0.371576252943814,-0.866022420303076));
#137824=DIRECTION('ref_axis',(0.74314482547369,0.669130606362972,-3.1907984490043E-12));
#137825=DIRECTION('center_axis',(-0.371576139135394,0.334568658442094,-0.866022508722199));
#137826=DIRECTION('ref_axis',(-0.669130606360631,-0.743144825475798,1.34625469437943E-12));
#137827=DIRECTION('center_axis',(-0.643556859037041,0.57950162440116,-0.500012436348132));
#137828=DIRECTION('ref_axis',(-0.372243731510656,0.333837986826846,0.866017784403081));
#137829=DIRECTION('center_axis',(0.371576145565853,-0.334568664232091,0.866022503726306));
#137830=DIRECTION('ref_axis',(-0.918982183096511,-1.05744342495379E-15,
0.394299058014561));
#137831=DIRECTION('center_axis',(0.743144825477379,-0.669130606358875,-4.67251405070161E-15));
#137832=DIRECTION('ref_axis',(-0.669130606358875,-0.743144825477379,-6.82961998416085E-15));
#137833=DIRECTION('center_axis',(-0.743144825477402,0.66913060635885,4.56786669500646E-15));
#137834=DIRECTION('ref_axis',(0.669130606358849,0.743144825477402,6.82961998416066E-15));
#137835=DIRECTION('center_axis',(-0.743144825477406,0.669130606358845,4.6725140507014E-15));
#137836=DIRECTION('ref_axis',(0.669130606358845,0.743144825477406,6.82961998416065E-15));
#137837=DIRECTION('center_axis',(-0.743144825477402,0.66913060635885,4.56786669500646E-15));
#137838=DIRECTION('ref_axis',(0.66913060635885,0.743144825477402,6.82961998416066E-15));
#137839=DIRECTION('center_axis',(0.743144825477382,-0.669130606358872,-4.67251405070159E-15));
#137840=DIRECTION('ref_axis',(-0.669130606358872,-0.743144825477382,-6.82961998416048E-15));
#137841=DIRECTION('center_axis',(-0.393810436983627,0.354588510146739,0.84804500363759));
#137842=DIRECTION('ref_axis',(-0.906978223357771,-2.42620968147434E-15,
-0.421177518814551));
#137843=DIRECTION('center_axis',(0.371576246276117,-0.334568754912008,-0.866022425483301));
#137844=DIRECTION('ref_axis',(0.918982131463646,9.92141015011441E-16,0.394299178353865));
#137845=DIRECTION('center_axis',(0.393810430453619,-0.354588475163049,-0.848045021297501));
#137846=DIRECTION('ref_axis',(0.633098037503659,-0.564245025058769,0.529919264233188));
#137847=DIRECTION('center_axis',(-0.393810395274859,0.354588472591995,0.848045038708638));
#137848=DIRECTION('ref_axis',(-0.906978247051287,2.6316557495518E-15,-0.421177467792111));
#137849=DIRECTION('center_axis',(0.37157626360364,-0.334568756369229,-0.866022417485775));
#137850=DIRECTION('ref_axis',(0.646617000436438,-0.576095872877601,0.499999999999978));
#137851=DIRECTION('center_axis',(0.64356810859173,-0.579517695132084,-0.49997933020522));
#137852=DIRECTION('ref_axis',(-0.370911831406173,0.335267672830955,-0.866036951219423));
#137853=DIRECTION('center_axis',(0.668950377172403,0.743307065001336,5.19048549296485E-15));
#137854=DIRECTION('ref_axis',(0.743307065001336,-0.668950377172402,-3.41480999208038E-15));
#137855=DIRECTION('center_axis',(-0.743144825477402,0.66913060635885,4.56786669500646E-15));
#137856=DIRECTION('ref_axis',(0.669130606358849,0.743144825477402,6.82961998416066E-15));
#137857=DIRECTION('center_axis',(0.743144825477409,-0.669130606358842,-4.67251405070138E-15));
#137858=DIRECTION('ref_axis',(-0.669130606358842,-0.743144825477409,-6.82961998416067E-15));
#137859=DIRECTION('center_axis',(-3.61695511949404E-17,-7.07718757997909E-15,
1.));
#137860=DIRECTION('ref_axis',(0.,-1.,-7.08021563511275E-15));
#137861=DIRECTION('center_axis',(0.669310796197601,0.742982542253406,5.18821936272799E-15));
#137862=DIRECTION('ref_axis',(0.742982542253406,-0.669310796197601,-3.41480999208024E-15));
#137863=DIRECTION('center_axis',(0.393810781475729,-0.354588820328862,0.848044713969294));
#137864=DIRECTION('ref_axis',(-0.906978027661826,2.76586647871208E-15,0.421177940232704));
#137865=DIRECTION('center_axis',(0.393810395274862,-0.354588472591998,-0.848045038708635));
#137866=DIRECTION('ref_axis',(0.906978247051285,-1.98629810325044E-15,0.421177467792115));
#137867=DIRECTION('center_axis',(0.393810788840124,-0.354588860891335,0.848044693589262));
#137868=DIRECTION('ref_axis',(-0.633246889658985,0.564077964586254,0.529919264233195));
#137869=DIRECTION('center_axis',(0.393810830024499,-0.354588864042367,0.848044673146739));
#137870=DIRECTION('ref_axis',(-0.906978000082658,2.87858588363672E-16,0.421177999622561));
#137871=DIRECTION('center_axis',(-0.393810430617737,0.354588475217419,0.848045021198555));
#137872=DIRECTION('ref_axis',(0.627330796736552,-0.570650194830793,0.529919264233205));
#137873=DIRECTION('center_axis',(0.39381043698369,-0.354588510146796,-0.848045003637538));
#137874=DIRECTION('ref_axis',(0.906978223357735,-7.84757798853097E-16,0.421177518814629));
#137875=DIRECTION('center_axis',(0.668938718831589,0.743317556935091,5.19055875774668E-15));
#137876=DIRECTION('ref_axis',(0.743317556935091,-0.668938718831589,-3.41480999208028E-15));
#137877=DIRECTION('center_axis',(0.743144825477406,-0.669130606358845,-4.6725140507014E-15));
#137878=DIRECTION('ref_axis',(-0.669130606358845,-0.743144825477406,-6.82961998416065E-15));
#137879=DIRECTION('center_axis',(-3.61695511949404E-17,-7.07718757997909E-15,
1.));
#137880=DIRECTION('ref_axis',(0.,-1.,-7.07923578254995E-15));
#137881=DIRECTION('center_axis',(0.669322449283883,0.742972044483925,5.18814605719551E-15));
#137882=DIRECTION('ref_axis',(0.742972044483925,-0.669322449283883,-3.41480999208044E-15));
#137883=DIRECTION('center_axis',(0.743144825477402,-0.66913060635885,-4.56786669500646E-15));
#137884=DIRECTION('ref_axis',(-0.66913060635885,-0.743144825477402,-6.82961998416062E-15));
#137885=DIRECTION('center_axis',(0.64359706336872,-0.579456972965919,0.500012436349672));
#137886=DIRECTION('ref_axis',(0.370919252638004,-0.33530896964076,-0.866017784402213));
#137887=DIRECTION('center_axis',(-0.393810830024549,0.354588864042324,-0.848044673146734));
#137888=DIRECTION('ref_axis',(0.906978000082637,1.97446543713211E-15,-0.421177999622606));
#137889=DIRECTION('center_axis',(-0.371576128832093,0.334568662768457,-0.866022511471545));
#137890=DIRECTION('ref_axis',(-0.640578396537782,0.582802983768183,0.499999999999987));
#137891=DIRECTION('center_axis',(0.371576145565796,-0.33456866423204,0.866022503726349));
#137892=DIRECTION('ref_axis',(-0.91898218309654,2.29774910071685E-15,0.394299058014495));
#137893=DIRECTION('center_axis',(-0.393810788650038,0.354588860812297,-0.848044693710581));
#137894=DIRECTION('ref_axis',(-0.627180210742338,0.57081569411471,0.529919264233278));
#137895=DIRECTION('center_axis',(-0.393810781475744,0.354588820328784,-0.848044713969319));
#137896=DIRECTION('ref_axis',(0.906978027661825,-2.63639073947388E-15,-0.421177940232707));
#137897=DIRECTION('center_axis',(0.743144825477406,-0.669130606358845,-8.7164259707347E-15));
#137898=DIRECTION('ref_axis',(-0.669130606358845,-0.743144825477406,-6.82961998416065E-15));
#137899=DIRECTION('center_axis',(-0.743144825477406,0.669130606358845,4.6725140507014E-15));
#137900=DIRECTION('ref_axis',(0.669130606358845,0.743144825477406,6.82961998416065E-15));
#137901=DIRECTION('center_axis',(0.743144825477402,-0.66913060635885,-4.56786669500646E-15));
#137902=DIRECTION('ref_axis',(-0.66913060635885,-0.743144825477402,-6.82961998416062E-15));
#137903=DIRECTION('center_axis',(0.743144825477406,-0.669130606358845,-8.71642597073447E-15));
#137904=DIRECTION('ref_axis',(-0.669130606358845,-0.743144825477406,-6.82961998416065E-15));
#137905=DIRECTION('center_axis',(0.743144825477402,-0.66913060635885,-4.56786669500646E-15));
#137906=DIRECTION('ref_axis',(-0.66913060635885,-0.743144825477402,-6.82961998416062E-15));
#137907=DIRECTION('center_axis',(-0.643614221961265,0.579466481046755,0.499979330205245));
#137908=DIRECTION('ref_axis',(0.372201885190247,-0.333834922953591,0.866036951219402));
#137909=DIRECTION('center_axis',(0.371576246276125,-0.334568754912015,-0.866022425483295));
#137910=DIRECTION('ref_axis',(0.918982131463643,2.05752676658029E-15,0.394299178353873));
#137911=DIRECTION('center_axis',(0.371576252947017,-0.334568760918514,-0.866022420300598));
#137912=DIRECTION('ref_axis',(0.669130606357726,0.743144825478414,-8.82933269452628E-13));
#137913=DIRECTION('center_axis',(-0.404512553894895,0.293895573516703,-0.866022508719443));
#137914=DIRECTION('ref_axis',(-0.587785252300532,-0.809016994369093,5.74780819192983E-12));
#137915=DIRECTION('center_axis',(-0.700605801486583,0.509057044367303,-0.500012436348706));
#137916=DIRECTION('ref_axis',(-0.405100113146689,0.293099122186841,0.866017784402747));
#137917=DIRECTION('center_axis',(0.404512560891477,-0.293895578600012,0.866022503726308));
#137918=DIRECTION('ref_axis',(-0.906035256115478,-2.30820235819247E-15,
0.423202214875774));
#137919=DIRECTION('center_axis',(0.80901699437495,-0.58778525229247,-4.10448247925272E-15));
#137920=DIRECTION('ref_axis',(-0.58778525229247,-0.80901699437495,-6.82961998416043E-15));
#137921=DIRECTION('center_axis',(-0.809016994374955,0.587785252292463,3.99055920848342E-15));
#137922=DIRECTION('ref_axis',(0.587785252292463,0.809016994374955,6.82961998416066E-15));
#137923=DIRECTION('center_axis',(-0.80901699437495,0.58778525229247,4.10448247925272E-15));
#137924=DIRECTION('ref_axis',(0.58778525229247,0.80901699437495,6.82961998416043E-15));
#137925=DIRECTION('center_axis',(-0.809016994374955,0.587785252292463,3.99055920848342E-15));
#137926=DIRECTION('ref_axis',(0.587785252292463,0.809016994374955,6.82961998416066E-15));
#137927=DIRECTION('center_axis',(0.80901699437495,-0.58778525229247,-4.10448247925272E-15));
#137928=DIRECTION('ref_axis',(-0.58778525229247,-0.80901699437495,-6.82961998416043E-15));
#137929=DIRECTION('center_axis',(-0.428717694262757,0.311481637390284,0.848045003637597));
#137930=DIRECTION('ref_axis',(-0.892442058026274,8.07292141989185E-16,-0.451162025292277));
#137931=DIRECTION('center_axis',(0.404512670528679,-0.29389565825609,-0.866022425483299));
#137932=DIRECTION('ref_axis',(0.906035197473497,-2.09617485499778E-15,0.423202340422594));
#137933=DIRECTION('center_axis',(0.428717684111651,-0.311481603280926,-0.848045021297505));
#137934=DIRECTION('ref_axis',(0.68860952557847,-0.494977266828602,0.529919264233224));
#137935=DIRECTION('center_axis',(-0.428717648856936,0.311481604401024,0.848045038708643));
#137936=DIRECTION('ref_axis',(-0.892442084777728,6.67310720912807E-18,-0.451161972375313));
#137937=DIRECTION('center_axis',(0.404512687917536,-0.293895657888627,-0.866022417485796));
#137938=DIRECTION('ref_axis',(0.703293181139598,-0.505350078027689,0.499999999999954));
#137939=DIRECTION('center_axis',(0.700618669263885,-0.509071851163053,-0.499979330205085));
#137940=DIRECTION('ref_axis',(-0.403924952202812,0.29466019770305,-0.866036951219493));
#137941=DIRECTION('center_axis',(0.587589051772177,0.809159506053951,-3.85596848322865E-14));
#137942=DIRECTION('ref_axis',(0.809159506053951,-0.587589051772177,-3.41480999208123E-15));
#137943=DIRECTION('center_axis',(-0.809016994374955,0.587785252292463,3.99055920848342E-15));
#137944=DIRECTION('ref_axis',(0.587785252292463,0.809016994374955,6.82961998416066E-15));
#137945=DIRECTION('center_axis',(0.80901699437495,-0.58778525229247,-4.10448247925272E-15));
#137946=DIRECTION('ref_axis',(-0.58778525229247,-0.80901699437495,-6.82961998416043E-15));
#137947=DIRECTION('center_axis',(-2.68936361206573E-17,-7.0657327788296E-15,
1.));
#137948=DIRECTION('ref_axis',(0.,-1.,-7.06611161990336E-15));
#137949=DIRECTION('center_axis',(0.587981418248456,0.808874435122371,5.64833999139408E-15));
#137950=DIRECTION('ref_axis',(0.808874435122371,-0.587981418248456,-3.41480999208034E-15));
#137951=DIRECTION('center_axis',(0.428718069290566,-0.311481909863969,0.848044713969295));
#137952=DIRECTION('ref_axis',(-0.892441837073378,9.13395690474326E-16,0.451162462358178));
#137953=DIRECTION('center_axis',(0.428717648856939,-0.311481604401026,-0.848045038708642));
#137954=DIRECTION('ref_axis',(0.892442084777727,-9.59323760580522E-17,0.451161972375316));
#137955=DIRECTION('center_axis',(0.428718080851877,-0.31148194943812,0.848044693589266));
#137956=DIRECTION('ref_axis',(-0.688740099740449,0.494795562231596,0.529919264233179));
#137957=DIRECTION('center_axis',(0.428718122142669,-0.311481948263306,0.848044673146739));
#137958=DIRECTION('ref_axis',(-0.89244180593479,1.4497682461611E-15,0.451162523953232));
#137959=DIRECTION('center_axis',(-0.428717684279575,0.311481603319163,0.848045021198569));
#137960=DIRECTION('ref_axis',(0.683543400920389,-0.501950189214795,0.529919264233165));
#137961=DIRECTION('center_axis',(0.42871769426279,-0.311481637390308,-0.848045003637572));
#137962=DIRECTION('ref_axis',(0.892442058026255,1.78135499927075E-15,0.451162025292313));
#137963=DIRECTION('center_axis',(0.587576360591332,0.809168721883295,-6.45673796727378E-15));
#137964=DIRECTION('ref_axis',(0.809168721883294,-0.587576360591332,-3.41480999208043E-15));
#137965=DIRECTION('center_axis',(0.80901699437495,-0.58778525229247,2.8010316764361E-14));
#137966=DIRECTION('ref_axis',(-0.58778525229247,-0.80901699437495,-6.82961998416043E-15));
#137967=DIRECTION('center_axis',(-2.68936361206573E-17,-7.0657327788296E-15,
1.));
#137968=DIRECTION('ref_axis',(0.,-1.,-7.06422149669088E-15));
#137969=DIRECTION('center_axis',(0.587994104813612,0.80886521293998,1.77160014651075E-14));
#137970=DIRECTION('ref_axis',(0.80886521293998,-0.587994104813612,-3.41480999208048E-15));
#137971=DIRECTION('center_axis',(0.809016994374955,-0.587785252292463,-3.99055920848342E-15));
#137972=DIRECTION('ref_axis',(-0.587785252292463,-0.809016994374955,-6.82961998416068E-15));
#137973=DIRECTION('center_axis',(0.700641118228849,-0.50900843504249,0.50001243634796));
#137974=DIRECTION('ref_axis',(0.40393664952349,-0.294700492481754,-0.86601778440327));
#137975=DIRECTION('center_axis',(-0.428718122142697,0.311481948263298,-0.848044673146727));
#137976=DIRECTION('ref_axis',(0.892441805934776,8.55497766242104E-16,-0.45116252395326));
#137977=DIRECTION('center_axis',(-0.404512544094918,0.293895578895568,-0.866022511471553));
#137978=DIRECTION('ref_axis',(-0.697988741330392,0.512651652660993,0.499999999999968));
#137979=DIRECTION('center_axis',(0.404512560891374,-0.293895578599945,0.866022503726379));
#137980=DIRECTION('ref_axis',(-0.906035256115532,-1.99991727152335E-15,
0.423202214875657));
#137981=DIRECTION('center_axis',(-0.428718080659361,0.311481949372824,-0.848044693710573));
#137982=DIRECTION('ref_axis',(-0.683410939245724,0.502130522388065,0.529919264233304));
#137983=DIRECTION('center_axis',(-0.428718069290593,0.311481909863882,-0.848044713969314));
#137984=DIRECTION('ref_axis',(0.89244183707337,-4.01305572582718E-16,-0.451162462358193));
#137985=DIRECTION('center_axis',(0.80901699437495,-0.58778525229247,2.80103167643593E-14));
#137986=DIRECTION('ref_axis',(-0.58778525229247,-0.80901699437495,-6.82961998416043E-15));
#137987=DIRECTION('center_axis',(-0.809016994374976,0.587785252292434,4.10448247925247E-15));
#137988=DIRECTION('ref_axis',(0.587785252292434,0.809016994374976,6.82961998416065E-15));
#137989=DIRECTION('center_axis',(0.809016994374955,-0.587785252292463,-3.99055920848342E-15));
#137990=DIRECTION('ref_axis',(-0.587785252292463,-0.809016994374955,-6.82961998416068E-15));
#137991=DIRECTION('center_axis',(0.80901699437495,-0.58778525229247,-4.10448247925272E-15));
#137992=DIRECTION('ref_axis',(-0.58778525229247,-0.80901699437495,-6.82961998416043E-15));
#137993=DIRECTION('center_axis',(0.809016994374955,-0.587785252292463,-3.99055920848342E-15));
#137994=DIRECTION('ref_axis',(-0.587785252292463,-0.809016994374955,-6.82961998416068E-15));
#137995=DIRECTION('center_axis',(-0.700659176689953,0.509016097474098,0.499979330205156));
#137996=DIRECTION('ref_axis',(0.405058175796856,-0.293100449236484,0.866036951219458));
#137997=DIRECTION('center_axis',(0.404512670528659,-0.293895658256083,-0.866022425483311));
#137998=DIRECTION('ref_axis',(0.906035197473507,-2.80279631697786E-15,0.423202340422572));
#137999=DIRECTION('center_axis',(0.404512677794142,-0.293895663534851,-0.866022420298241));
#138000=DIRECTION('ref_axis',(0.587785252294639,0.809016994373374,1.48175434825272E-12));
#138001=DIRECTION('center_axis',(-0.433017044458074,0.250002507181587,-0.866022508721173));
#138002=DIRECTION('ref_axis',(-0.500000000002247,-0.866025403783142,1.47738339837865E-12));
#138003=DIRECTION('center_axis',(-0.749978760163501,0.433035128829403,-0.500012436348657));
#138004=DIRECTION('ref_axis',(-0.433518133169102,0.249149002228967,0.866017784402773));
#138005=DIRECTION('center_axis',(0.43301705195027,-0.250002511507207,0.86602250372631));
#138006=DIRECTION('ref_axis',(-0.894424794863787,-7.00304685398516E-16,
0.44721838774012));
#138007=DIRECTION('center_axis',(0.866025403784433,-0.50000000000001,-3.4914813388432E-15));
#138008=DIRECTION('ref_axis',(-0.50000000000001,-0.866025403784433,-6.82961998416068E-15));
#138009=DIRECTION('center_axis',(-0.866025403784445,0.499999999999989,3.36953032019404E-15));
#138010=DIRECTION('ref_axis',(0.499999999999989,0.866025403784445,6.82961998416066E-15));
#138011=DIRECTION('center_axis',(-0.86602540378444,0.499999999999998,1.71507213071642E-14));
#138012=DIRECTION('ref_axis',(0.499999999999998,0.86602540378444,6.82961998416091E-15));
#138013=DIRECTION('center_axis',(-0.866025403784445,0.499999999999989,3.36953032019404E-15));
#138014=DIRECTION('ref_axis',(0.499999999999989,0.866025403784445,6.82961998416066E-15));
#138015=DIRECTION('center_axis',(0.866025403784463,-0.499999999999957,-3.49148133884283E-15));
#138016=DIRECTION('ref_axis',(-0.499999999999957,-0.866025403784463,-6.8296199841607E-15));
#138017=DIRECTION('center_axis',(-0.458927830768608,0.26496210663286,0.8480450036376));
#138018=DIRECTION('ref_axis',(-0.879478602053343,1.78405630805235E-15,-0.47593842934806));
#138019=DIRECTION('center_axis',(0.43301716931321,-0.250002579266712,-0.866022425483294));
#138020=DIRECTION('ref_axis',(0.89442473021642,-1.02528410709423E-15,0.447218517033099));
#138021=DIRECTION('center_axis',(0.458927817106631,-0.264962073773304,-0.84804502129751));
#138022=DIRECTION('ref_axis',(0.736576463600031,-0.420286434072047,0.529919264233217));
#138023=DIRECTION('center_axis',(-0.458927782163189,0.264962078570508,0.84804503870866));
#138024=DIRECTION('ref_axis',(-0.87947863139126,1.76485634666569E-15,-0.475938375135012));
#138025=DIRECTION('center_axis',(0.433017186567159,-0.250002577085787,-0.866022417485787));
#138026=DIRECTION('ref_axis',(0.752263934581057,-0.429067561962785,0.499999999999939));
#138027=DIRECTION('center_axis',(0.749993105181555,-0.433048509462383,-0.499979330205297));
#138028=DIRECTION('ref_axis',(-0.43251258670008,0.250824363786042,-0.866036951219365));
#138029=DIRECTION('center_axis',(0.499789977759954,0.866146626230631,6.04826956437238E-15));
#138030=DIRECTION('ref_axis',(0.866146626230631,-0.499789977759954,-3.41480999208016E-15));
#138031=DIRECTION('center_axis',(-0.866025403784445,0.499999999999989,3.36953032019404E-15));
#138032=DIRECTION('ref_axis',(0.499999999999989,0.866025403784445,6.82961998416066E-15));
#138033=DIRECTION('center_axis',(0.86602540378444,-0.499999999999998,-3.49148133884312E-15));
#138034=DIRECTION('ref_axis',(-0.499999999999998,-0.86602540378444,-6.82961998416073E-15));
#138035=DIRECTION('center_axis',(-1.88658882408992E-17,-7.05337113113122E-15,
1.));
#138036=DIRECTION('ref_axis',(0.,-1.,-7.05200760469397E-15));
#138037=DIRECTION('center_axis',(0.500209992837931,0.865904130412297,6.04657622512345E-15));
#138038=DIRECTION('ref_axis',(0.865904130412297,-0.500209992837931,-3.41480999208038E-15));
#138039=DIRECTION('center_axis',(0.458928232223227,-0.264962338412759,0.848044713969321));
#138040=DIRECTION('ref_axis',(-0.879478359737734,-3.02123578176224E-15,
0.475938877118716));
#138041=DIRECTION('center_axis',(0.458927782163212,-0.264962078570521,-0.848045038708643));
#138042=DIRECTION('ref_axis',(0.879478631391247,-3.81712923167341E-16,0.475938375135038));
#138043=DIRECTION('center_axis',(0.458928247861605,-0.264962376555123,0.848044693589282));
#138044=DIRECTION('ref_axis',(-0.736687329166148,0.420092076145952,0.529919264233176));
#138045=DIRECTION('center_axis',(0.458928288799633,-0.264962371077261,0.848044673146737));
#138046=DIRECTION('ref_axis',(-0.879478325588518,6.87163476984199E-16,0.475938940222395));
#138047=DIRECTION('center_axis',(-0.458927817275418,0.264962073797621,0.848045021198571));
#138048=DIRECTION('ref_axis',(0.732266960588852,-0.427750712242988,0.529919264233318));
#138049=DIRECTION('center_axis',(0.458927830768628,-0.264962106632871,-0.848045003637586));
#138050=DIRECTION('ref_axis',(0.879478602053331,-1.57823178879883E-16,0.475938429348081));
#138051=DIRECTION('center_axis',(0.499776392786184,0.866154464985103,2.97103476758322E-14));
#138052=DIRECTION('ref_axis',(0.866154464985103,-0.499776392786184,-3.4148099920807E-15));
#138053=DIRECTION('center_axis',(0.86602540378444,-0.499999999999998,-3.49148133884312E-15));
#138054=DIRECTION('ref_axis',(-0.499999999999998,-0.86602540378444,-6.82961998416073E-15));
#138055=DIRECTION('center_axis',(-1.88658882408992E-17,-7.05337113113122E-15,
1.));
#138056=DIRECTION('ref_axis',(0.,-1.,-7.05671435376135E-15));
#138057=DIRECTION('center_axis',(0.500223573885301,0.865896284857152,6.04652143990469E-15));
#138058=DIRECTION('ref_axis',(0.865896284857152,-0.500223573885301,-3.41480999208034E-15));
#138059=DIRECTION('center_axis',(0.866025403784445,-0.499999999999989,-3.36953032019404E-15));
#138060=DIRECTION('ref_axis',(-0.499999999999989,-0.866025403784445,-6.82961998416055E-15));
#138061=DIRECTION('center_axis',(0.750008802379763,-0.432983094187063,0.500012436346408));
#138062=DIRECTION('ref_axis',(0.432528431901353,-0.250863215104638,-0.866017784404178));
#138063=DIRECTION('center_axis',(-0.458928288799654,0.264962371077256,-0.848044673146728));
#138064=DIRECTION('ref_axis',(0.879478325588507,7.27534261071945E-16,-0.475938940222415));
#138065=DIRECTION('center_axis',(-0.433017035277113,0.250002513556067,-0.866022511471537));
#138066=DIRECTION('ref_axis',(-0.747751775423434,0.436883602749162,0.500000000000014));
#138067=DIRECTION('center_axis',(0.433017051950193,-0.250002511507147,0.866022503726365));
#138068=DIRECTION('ref_axis',(-0.894424794863831,-1.74682411385781E-15,
0.447218387740033));
#138069=DIRECTION('center_axis',(-0.45892824765206,0.264962376529661,-0.848044693710634));
#138070=DIRECTION('ref_axis',(-0.732154074452537,0.4279439036336,0.529919264233132));
#138071=DIRECTION('center_axis',(-0.458928232223214,0.264962338412759,-0.848044713969328));
#138072=DIRECTION('ref_axis',(0.879478359737742,2.18132396275747E-15,-0.475938877118703));
#138073=DIRECTION('center_axis',(0.86602540378444,-0.499999999999998,-3.71492366063374E-14));
#138074=DIRECTION('ref_axis',(-0.499999999999998,-0.86602540378444,-6.82961998416119E-15));
#138075=DIRECTION('center_axis',(-0.866025403784433,0.50000000000001,3.4914813388432E-15));
#138076=DIRECTION('ref_axis',(0.50000000000001,0.866025403784433,6.82961998416068E-15));
#138077=DIRECTION('center_axis',(0.866025403784445,-0.499999999999989,-3.36953032019404E-15));
#138078=DIRECTION('ref_axis',(-0.499999999999989,-0.866025403784445,-6.82961998416055E-15));
#138079=DIRECTION('center_axis',(0.86602540378444,-0.499999999999998,2.38269985977989E-14));
#138080=DIRECTION('ref_axis',(-0.499999999999998,-0.86602540378444,-6.82961998416036E-15));
#138081=DIRECTION('center_axis',(0.866025403784445,-0.499999999999989,-3.36953032019404E-15));
#138082=DIRECTION('ref_axis',(-0.499999999999989,-0.866025403784445,-6.82961998416055E-15));
#138083=DIRECTION('center_axis',(-0.750027562856428,0.43298882701908,0.499979330205047));
#138084=DIRECTION('ref_axis',(0.43347656427264,-0.24915470565252,0.866036951219516));
#138085=DIRECTION('center_axis',(0.433017169313169,-0.250002579266681,-0.866022425483323));
#138086=DIRECTION('ref_axis',(0.894424730216443,2.17074162788549E-15,0.447218517033052));
#138087=DIRECTION('center_axis',(0.433017177085757,-0.250002583754148,-0.866022420301537));
#138088=DIRECTION('ref_axis',(0.499999999999688,0.866025403784619,-1.44241573722197E-13));
#138089=DIRECTION('center_axis',(-0.45677730966968,0.203370361063029,-0.866022508721351));
#138090=DIRECTION('ref_axis',(-0.406736643071311,-0.9135454576446,-2.85423479040283E-12));
#138091=DIRECTION('center_axis',(-0.79113479460122,0.352268789800861,-0.500012436348859));
#138092=DIRECTION('ref_axis',(0.457186437780581,-0.202469153719109,-0.866017784402706));
#138093=DIRECTION('center_axis',(0.456777317573273,-0.203370364581924,0.866022503726307));
#138094=DIRECTION('ref_axis',(-0.884507036382098,8.12886901361279E-16,0.466526850878445));
#138095=DIRECTION('center_axis',(0.913545457642598,-0.406736643075807,-2.84022679824576E-15));
#138096=DIRECTION('ref_axis',(-0.406736643075807,-0.913545457642598,-6.8296199841606E-15));
#138097=DIRECTION('center_axis',(-0.913545457642606,0.406736643075789,2.71158415259707E-15));
#138098=DIRECTION('ref_axis',(0.406736643075789,0.913545457642606,6.82961998416066E-15));
#138099=DIRECTION('center_axis',(-0.913545457642598,0.406736643075807,1.39516536216094E-14));
#138100=DIRECTION('ref_axis',(0.406736643075807,0.913545457642598,6.8296199841606E-15));
#138101=DIRECTION('center_axis',(-0.913545457642606,0.406736643075789,2.71158415259707E-15));
#138102=DIRECTION('ref_axis',(0.406736643075789,0.913545457642606,6.82961998416066E-15));
#138103=DIRECTION('center_axis',(0.913545457642598,-0.406736643075807,-2.84022679824576E-15));
#138104=DIRECTION('ref_axis',(-0.406736643075807,-0.913545457642598,-6.8296199841606E-15));
#138105=DIRECTION('center_axis',(-0.484109857923765,0.215539595588298,0.848045003637581));
#138106=DIRECTION('ref_axis',(-0.868458021515998,4.63801329176873E-17,-0.495762710240007));
#138107=DIRECTION('center_axis',(0.456777441376074,-0.203370419702464,-0.866022425483296));
#138108=DIRECTION('ref_axis',(0.884506966812059,1.56015689162916E-15,0.466526982779058));
#138109=DIRECTION('center_axis',(0.484109840903269,-0.215539564333573,-0.848045021297516));
#138110=DIRECTION('ref_axis',(0.776473315755943,-0.340990855175849,0.52991926423316));
#138111=DIRECTION('center_axis',(-0.484109806651279,0.215539572760317,0.848045038708653));
#138112=DIRECTION('ref_axis',(-0.868458052949963,1.30155882390688E-15,-0.495762655175195));
#138113=DIRECTION('center_axis',(0.456777458308535,-0.203370415727759,-0.866022417485779));
#138114=DIRECTION('ref_axis',(0.792992726925666,-0.348084091913183,0.49999999999997));
#138115=DIRECTION('center_axis',(0.791150459692744,-0.352280597670873,-0.499979330205373));
#138116=DIRECTION('ref_axis',(0.456361522796686,-0.204240445635572,0.86603695121933));
#138117=DIRECTION('center_axis',(0.406515100163541,0.913644062717548,6.37994239064629E-15));
#138118=DIRECTION('ref_axis',(0.913644062717548,-0.406515100163541,-3.41480999208033E-15));
#138119=DIRECTION('center_axis',(-0.913545457642606,0.406736643075789,2.71158415259707E-15));
#138120=DIRECTION('ref_axis',(0.406736643075789,0.913545457642606,6.82961998416066E-15));
#138121=DIRECTION('center_axis',(0.913545457642618,-0.406736643075761,-2.84022679824544E-15));
#138122=DIRECTION('ref_axis',(-0.406736643075761,-0.913545457642618,-6.82961998416076E-15));
#138123=DIRECTION('center_axis',(-1.2174261241351E-17,-7.04023807368298E-15,
1.));
#138124=DIRECTION('ref_axis',(0.,-1.,-7.03790358948458E-15));
#138125=DIRECTION('center_axis',(0.406958162070199,0.913446798847336,6.37856490440294E-15));
#138126=DIRECTION('ref_axis',(0.913446798847336,-0.406958162070199,-3.4148099920803E-15));
#138127=DIRECTION('center_axis',(0.484110281406754,-0.215539784135097,0.848044713969298));
#138128=DIRECTION('ref_axis',(-0.868457761888264,-7.52957874888421E-16,
0.495763165045596));
#138129=DIRECTION('center_axis',(0.484109806651376,-0.215539572760309,-0.8480450387086));
#138130=DIRECTION('ref_axis',(0.868458052949907,-1.21988200561595E-15,0.495762655175294));
#138131=DIRECTION('center_axis',(0.484110300947392,-0.215539820431551,0.848044693589294));
#138132=DIRECTION('ref_axis',(-0.776563258037247,0.340785973392536,0.529919264233221));
#138133=DIRECTION('center_axis',(0.484110341087594,-0.215539810706751,0.848044673146734));
#138134=DIRECTION('ref_axis',(-0.868457725299276,1.07363447275437E-15,0.495763229140693));
#138135=DIRECTION('center_axis',(-0.484109841074222,0.215539564339001,0.848045021198548));
#138136=DIRECTION('ref_axis',(0.772967650155928,-0.348864709030508,0.529919264233224));
#138137=DIRECTION('center_axis',(0.484109857923745,-0.215539595588289,-0.848045003637595));
#138138=DIRECTION('ref_axis',(0.868458021516011,-1.65169124191511E-15,0.495762710239986));
#138139=DIRECTION('center_axis',(0.406500770236715,0.913650438514073,9.12956181436392E-15));
#138140=DIRECTION('ref_axis',(0.913650438514073,-0.406500770236715,-3.41480999208026E-15));
#138141=DIRECTION('center_axis',(0.913545457642598,-0.406736643075807,-5.27535733098856E-14));
#138142=DIRECTION('ref_axis',(-0.406736643075807,-0.913545457642598,-6.8296199841606E-15));
#138143=DIRECTION('center_axis',(-1.2174261241351E-17,-7.04023807368298E-15,
1.));
#138144=DIRECTION('ref_axis',(0.,-1.,-7.04170006790228E-15));
#138145=DIRECTION('center_axis',(0.406972488803016,0.913440415876963,9.09658446655107E-15));
#138146=DIRECTION('ref_axis',(0.913440415876963,-0.406972488803016,-3.41480999208023E-15));
#138147=DIRECTION('center_axis',(0.913545457642606,-0.406736643075789,-2.71158415259707E-15));
#138148=DIRECTION('ref_axis',(-0.406736643075789,-0.913545457642606,-6.82961998416066E-15));
#138149=DIRECTION('center_axis',(0.791159233141483,-0.35221389994137,0.500012436348408));
#138150=DIRECTION('ref_axis',(0.45638134222745,-0.204277427936816,-0.866017784402948));
#138151=DIRECTION('center_axis',(-0.484110341087625,0.21553981070667,-0.848044673146737));
#138152=DIRECTION('ref_axis',(0.868457725299263,1.08885966448668E-16,-0.495763229140716));
#138153=DIRECTION('center_axis',(-0.456777301207149,0.203370368358987,-0.866022511471523));
#138154=DIRECTION('ref_axis',(-0.789322284581999,0.356328964669224,0.500000000000013));
#138155=DIRECTION('center_axis',(0.456777317573189,-0.203370364581881,0.866022503726361));
#138156=DIRECTION('ref_axis',(-0.884507036382145,2.90703320888221E-16,0.466526850878355));
#138157=DIRECTION('center_axis',(-0.484110300735212,0.215539820430766,-0.848044693710618));
#138158=DIRECTION('ref_axis',(-0.77287557643843,0.349068641873687,0.529919264233171));
#138159=DIRECTION('center_axis',(-0.484110281406742,0.215539784135022,-0.848044713969325));
#138160=DIRECTION('ref_axis',(0.868457761888276,-5.66899354755573E-16,-0.495763165045576));
#138161=DIRECTION('center_axis',(0.913545457642598,-0.406736643075807,-1.39516536216094E-14));
#138162=DIRECTION('ref_axis',(-0.406736643075807,-0.913545457642598,-6.8296199841606E-15));
#138163=DIRECTION('center_axis',(-0.913545457642594,0.406736643075817,2.84022679824583E-15));
#138164=DIRECTION('ref_axis',(0.406736643075817,0.913545457642593,6.82961998416057E-15));
#138165=DIRECTION('center_axis',(0.913545457642606,-0.406736643075789,-2.71158415259707E-15));
#138166=DIRECTION('ref_axis',(-0.406736643075789,-0.913545457642606,-6.82961998416066E-15));
#138167=DIRECTION('center_axis',(0.913545457642598,-0.406736643075807,5.81845465367577E-14));
#138168=DIRECTION('ref_axis',(-0.406736643075807,-0.913545457642598,-6.8296199841606E-15));
#138169=DIRECTION('center_axis',(0.913545457642606,-0.406736643075789,-2.71158415259707E-15));
#138170=DIRECTION('ref_axis',(-0.406736643075789,-0.913545457642606,-6.82961998416066E-15));
#138171=DIRECTION('center_axis',(-0.791178490090691,0.352217640366613,0.499979330205149));
#138172=DIRECTION('ref_axis',(0.457145692800845,-0.202479170968668,0.866036951219448));
#138173=DIRECTION('center_axis',(0.45677744137607,-0.203370419702462,-0.866022425483298));
#138174=DIRECTION('ref_axis',(0.884506966812061,1.8264828060639E-15,0.466526982779054));
#138175=DIRECTION('center_axis',(0.456777449574815,-0.203370423352742,-0.866022420301723));
#138176=DIRECTION('ref_axis',(0.406736643081688,0.913545457639979,3.74590996000316E-12));
#138177=DIRECTION('center_axis',(-0.475533027088392,0.154510046710294,-0.866022508722339));
#138178=DIRECTION('ref_axis',(-0.309016994372082,-0.951056516296084,-1.77460846079056E-12));
#138179=DIRECTION('center_axis',(-0.823622990674915,0.267642920194302,-0.500012436346914));
#138180=DIRECTION('ref_axis',(0.475845712136155,-0.153571010734221,-0.866017784403823));
#138181=DIRECTION('center_axis',(0.475533035318122,-0.1545100493843,0.866022503726315));
#138182=DIRECTION('ref_axis',(-0.876548788012444,-1.07841122773221E-15,
0.481313018974051));
#138183=DIRECTION('center_axis',(0.951056516295165,-0.309016994374914,5.82468571404663E-14));
#138184=DIRECTION('ref_axis',(-0.309016994374914,-0.951056516295164,-6.82961998416066E-15));
#138185=DIRECTION('center_axis',(-0.951056516295158,0.309016994374935,2.02392930158878E-15));
#138186=DIRECTION('ref_axis',(0.309016994374935,0.951056516295158,6.82961998416066E-15));
#138187=DIRECTION('center_axis',(-0.951056516295165,0.309016994374914,5.41206908565353E-14));
#138188=DIRECTION('ref_axis',(0.309016994374914,0.951056516295164,6.82961998416067E-15));
#138189=DIRECTION('center_axis',(-0.951056516295158,0.309016994374935,2.02392930158878E-15));
#138190=DIRECTION('ref_axis',(0.309016994374935,0.951056516295158,6.82961998416066E-15));
#138191=DIRECTION('center_axis',(0.951056516295165,-0.309016994374914,-2.15785413849081E-15));
#138192=DIRECTION('ref_axis',(-0.309016994374914,-0.951056516295164,-6.82961998416067E-15));
#138193=DIRECTION('center_axis',(-0.503987876168997,0.163755587629873,0.848045003637578));
#138194=DIRECTION('ref_axis',(-0.859649462041482,-4.46729327993359E-16,
-0.510884333691874));
#138195=DIRECTION('center_axis',(0.475533164204451,-0.154510091261954,-0.86602242548327));
#138196=DIRECTION('ref_axis',(0.876548714628815,-1.69396669624288E-15,0.481313152617475));
#138197=DIRECTION('center_axis',(0.503987855975045,-0.163755558324557,-0.848045021297508));
#138198=DIRECTION('ref_axis',(0.807862963765421,-0.257959309137511,0.529919264233192));
#138199=DIRECTION('center_axis',(-0.503987822791223,0.163755570286383,0.848045038708643));
#138200=DIRECTION('ref_axis',(-0.859649495083693,8.62473446481745E-16,-0.510884278092752));
#138201=DIRECTION('center_axis',(0.475533180627887,-0.154510085541456,-0.86602241748577));
#138202=DIRECTION('ref_axis',(0.825033325009512,-0.26328693971363,0.49999999999998));
#138203=DIRECTION('center_axis',(0.823639804208726,-0.267653025932087,-0.499979330205169));
#138204=DIRECTION('ref_axis',(0.475210466543723,-0.155418826433036,0.866036951219447));
#138205=DIRECTION('center_axis',(0.308786358060973,0.951131423661021,-1.9341749481394E-14));
#138206=DIRECTION('ref_axis',(0.951131423661021,-0.308786358060973,-3.41480999208049E-15));
#138207=DIRECTION('center_axis',(-0.951056516295158,0.309016994374935,2.02392930158878E-15));
#138208=DIRECTION('ref_axis',(0.309016994374935,0.951056516295158,6.82961998416066E-15));
#138209=DIRECTION('center_axis',(0.951056516295165,-0.309016994374914,-2.15785413849081E-15));
#138210=DIRECTION('ref_axis',(-0.309016994374914,-0.951056516295164,-6.82961998416067E-15));
#138211=DIRECTION('center_axis',(-6.89206998773264E-18,-7.02647749501056E-15,
1.));
#138212=DIRECTION('ref_axis',(0.,-1.,-7.02379957427519E-15));
#138213=DIRECTION('center_axis',(0.309247612517378,0.95098155300316,6.64066869178919E-15));
#138214=DIRECTION('ref_axis',(0.95098155300316,-0.309247612517378,-3.41480999208029E-15));
#138215=DIRECTION('center_axis',(0.503988317040571,-0.163755730877738,0.848044713969323));
#138216=DIRECTION('ref_axis',(-0.859649189130473,-2.30534688053848E-17,
0.510884792910614));
#138217=DIRECTION('center_axis',(0.503987822791218,-0.163755570286381,-0.848045038708647));
#138218=DIRECTION('ref_axis',(0.859649495083696,-1.39187210333192E-15,0.510884278092747));
#138219=DIRECTION('center_axis',(0.503988340265106,-0.163755764942529,0.848044693589265));
#138220=DIRECTION('ref_axis',(-0.807930997365388,0.257746148158916,0.529919264233158));
#138221=DIRECTION('center_axis',(0.503988379172015,-0.163755751065492,0.848044673146729));
#138222=DIRECTION('ref_axis',(-0.859649150669458,1.48905909758926E-15,0.510884857627704));
#138223=DIRECTION('center_axis',(-0.503987856145286,0.163755558312952,0.848045021198575));
#138224=DIRECTION('ref_axis',(0.805199544412657,-0.266156471032046,0.529919264233163));
#138225=DIRECTION('center_axis',(0.503987876168979,-0.163755587629867,-0.84804500363759));
#138226=DIRECTION('ref_axis',(0.859649462041493,-6.96683555657854E-16,0.510884333691856));
#138227=DIRECTION('center_axis',(0.308771440182783,0.951136266645033,1.57550132814483E-14));
#138228=DIRECTION('ref_axis',(0.951136266645033,-0.308771440182783,-3.41480999208041E-15));
#138229=DIRECTION('center_axis',(0.951056516295165,-0.309016994374914,-1.05997286994034E-14));
#138230=DIRECTION('ref_axis',(-0.309016994374914,-0.951056516295164,-6.82961998416067E-15));
#138231=DIRECTION('center_axis',(-6.89206998773264E-18,-7.02647749501056E-15,
1.));
#138232=DIRECTION('ref_axis',(0.,-1.,-7.02668578204321E-15));
#138233=DIRECTION('center_axis',(0.309262527968943,0.95097670255073,6.6406348212609E-15));
#138234=DIRECTION('ref_axis',(0.950976702550729,-0.309262527968943,-3.4148099920803E-15));
#138235=DIRECTION('center_axis',(0.951056516295158,-0.309016994374935,-2.02392930158878E-15));
#138236=DIRECTION('ref_axis',(-0.309016994374935,-0.951056516295158,-6.82961998416063E-15));
#138237=DIRECTION('center_axis',(0.823641557783743,-0.267585776504145,0.50001243634958));
#138238=DIRECTION('ref_axis',(0.475234043086884,-0.155453534505877,-0.866017784402216));
#138239=DIRECTION('center_axis',(-0.503988379172015,0.163755751065439,-0.848044673146739));
#138240=DIRECTION('ref_axis',(0.859649150669461,-1.39074635011745E-15,-0.510884857627699));
#138241=DIRECTION('center_axis',(-0.475533019435549,0.154510054854217,-0.86602251147153));
#138242=DIRECTION('ref_axis',(-0.822244813613241,0.271870311888071,0.50000000000001));
#138243=DIRECTION('center_axis',(0.475533035318005,-0.154510049384226,0.866022503726392));
#138244=DIRECTION('ref_axis',(-0.876548788012513,1.21600309223843E-16,0.481313018973926));
#138245=DIRECTION('center_axis',(-0.503988340058923,0.163755764948669,-0.848044693710613));
#138246=DIRECTION('ref_axis',(-0.805129291876817,0.266368911017192,0.529919264233195));
#138247=DIRECTION('center_axis',(-0.503988317040557,0.163755730877758,-0.848044713969328));
#138248=DIRECTION('ref_axis',(0.85964918913048,-5.66681152953988E-16,-0.510884792910601));
#138249=DIRECTION('center_axis',(0.951056516295165,-0.309016994374914,5.82468571404663E-14));
#138250=DIRECTION('ref_axis',(-0.309016994374914,-0.951056516295164,-6.82961998416066E-15));
#138251=DIRECTION('center_axis',(-0.951056516295165,0.309016994374914,2.15785413849081E-15));
#138252=DIRECTION('ref_axis',(0.309016994374914,0.951056516295164,6.82961998416067E-15));
#138253=DIRECTION('center_axis',(0.951056516295158,-0.309016994374935,-2.02392930158878E-15));
#138254=DIRECTION('ref_axis',(-0.309016994374935,-0.951056516295158,-6.82961998416063E-15));
#138255=DIRECTION('center_axis',(0.951056516295165,-0.309016994374914,4.13631080186411E-14));
#138256=DIRECTION('ref_axis',(-0.309016994374914,-0.951056516295164,-6.82961998416067E-15));
#138257=DIRECTION('center_axis',(0.951056516295158,-0.309016994374935,-2.02392930158878E-15));
#138258=DIRECTION('ref_axis',(-0.309016994374935,-0.951056516295158,-6.82961998416063E-15));
#138259=DIRECTION('center_axis',(-0.823661100222748,0.267587483540072,0.499979330205304));
#138260=DIRECTION('ref_axis',(0.475806237447156,-0.153585232132039,0.866036951219362));
#138261=DIRECTION('center_axis',(0.475533164204429,-0.154510091261951,-0.866022425483282));
#138262=DIRECTION('ref_axis',(0.876548714628827,1.19088306137351E-15,0.481313152617452));
#138263=DIRECTION('center_axis',(0.475533172742175,-0.154510094036062,-0.866022420300265));
#138264=DIRECTION('ref_axis',(0.309016994373383,0.951056516295662,-9.35384750808893E-13));
#138265=DIRECTION('center_axis',(-0.489078705150942,0.103956887952922,-0.866022508723083));
#138266=DIRECTION('ref_axis',(-0.207911690818889,-0.978147600733565,6.4690160639327E-13));
#138267=DIRECTION('center_axis',(-0.847087400906983,0.18008469874679,-0.500012436347268));
#138268=DIRECTION('ref_axis',(0.489291521289685,-0.102990311634942,-0.866017784403625));
#138269=DIRECTION('center_axis',(0.489078713616366,-0.103956889752297,0.866022503726312));
#138270=DIRECTION('ref_axis',(-0.870740345484705,1.09228964843654E-16,0.491743073916834));
#138271=DIRECTION('center_axis',(0.978147600733806,-0.207911690817757,-1.45183957723504E-15));
#138272=DIRECTION('ref_axis',(-0.207911690817757,-0.978147600733806,-6.8296199841607E-15));
#138273=DIRECTION('center_axis',(-0.978147600733808,0.207911690817747,1.31409985761785E-15));
#138274=DIRECTION('ref_axis',(0.207911690817747,0.978147600733808,6.82961998416066E-15));
#138275=DIRECTION('center_axis',(-0.978147600733807,0.207911690817754,4.29175525433411E-15));
#138276=DIRECTION('ref_axis',(0.207911690817754,0.978147600733807,6.82961998416071E-15));
#138277=DIRECTION('center_axis',(-0.978147600733808,0.207911690817747,1.31409985761785E-15));
#138278=DIRECTION('ref_axis',(0.207911690817747,0.978147600733808,6.82961998416066E-15));
#138279=DIRECTION('center_axis',(0.978147600733806,-0.207911690817757,-1.45183957723504E-15));
#138280=DIRECTION('ref_axis',(-0.207911690817757,-0.978147600733806,-6.8296199841607E-15));
#138281=DIRECTION('center_axis',(-0.518344097776651,0.110177439185346,0.848045003637584));
#138282=DIRECTION('ref_axis',(-0.85323958281187,-1.42754706638066E-15,-0.521519140898036));
#138283=DIRECTION('center_axis',(0.489078846174035,-0.103956917928307,-0.866022425483268));
#138284=DIRECTION('ref_axis',(0.870740269393757,1.01377976619987E-15,0.491743208652735));
#138285=DIRECTION('center_axis',(0.518344074629046,-0.110177412156386,-0.848045021297502));
#138286=DIRECTION('ref_axis',(0.830401496087484,-0.172101506937531,0.529919264233242));
#138287=DIRECTION('center_axis',(-0.518344042878405,0.110177427516364,0.848045038708645));
#138288=DIRECTION('ref_axis',(-0.853239616987299,-8.10318245671903E-16,
-0.521519084984784));
#138289=DIRECTION('center_axis',(0.489078861909158,-0.103956910524381,-0.866022417485753));
#138290=DIRECTION('ref_axis',(0.848034685338132,-0.175605160697131,0.49999999999999));
#138291=DIRECTION('center_axis',(0.847105178672072,-0.180092991630959,-0.499979330205128));
#138292=DIRECTION('ref_axis',(0.488852904976457,-0.104894406040358,0.866036951219473));
#138293=DIRECTION('center_axis',(0.207674488001815,0.978197989689809,6.83072005339167E-15));
#138294=DIRECTION('ref_axis',(0.978197989689809,-0.207674488001815,-2.10582014878174E-29));
#138295=DIRECTION('center_axis',(-0.978147600733808,0.207911690817747,1.31409985761785E-15));
#138296=DIRECTION('ref_axis',(0.207911690817747,0.978147600733808,6.82961998416066E-15));
#138297=DIRECTION('center_axis',(0.978147600733806,-0.207911690817757,-1.45183957723504E-15));
#138298=DIRECTION('ref_axis',(-0.207911690817757,-0.978147600733806,-6.8296199841607E-15));
#138299=DIRECTION('center_axis',(-3.07718727278846E-18,-7.01224015889347E-15,
1.));
#138300=DIRECTION('ref_axis',(0.,-1.,-7.00969555906581E-15));
#138301=DIRECTION('center_axis',(0.208148881407602,0.978097154258596,6.83001592333892E-15));
#138302=DIRECTION('ref_axis',(0.978097154258596,-0.208148881407602,-3.24411496833464E-30));
#138303=DIRECTION('center_axis',(0.518344551206563,-0.110177535564874,0.848044713969327));
#138304=DIRECTION('ref_axis',(-0.853239300541052,-1.56430135117269E-15,
0.521519602711361));
#138305=DIRECTION('center_axis',(0.51834404287839,-0.11017742751636,-0.848045038708654));
#138306=DIRECTION('ref_axis',(0.853239616987309,1.0828167418591E-16,0.521519084984769));
#138307=DIRECTION('center_axis',(0.518344577866913,-0.110177567004444,0.84804469358929));
#138308=DIRECTION('ref_axis',(-0.830446875604022,0.171882402223312,0.529919264233206));
#138309=DIRECTION('center_axis',(0.518344615107839,-0.110177549147496,0.848044673146738));
#138310=DIRECTION('ref_axis',(-0.853239260760972,-1.65434113834715E-15,
0.521519667794101));
#138311=DIRECTION('center_axis',(-0.518344074799165,0.110177412117555,0.848045021198566));
#138312=DIRECTION('ref_axis',(0.828609503962607,-0.180532167043603,0.529919264233131));
#138313=DIRECTION('center_axis',(0.518344097776644,-0.110177439185345,-0.848045003637588));
#138314=DIRECTION('ref_axis',(0.853239582811875,1.17437859349562E-15,0.521519140898029));
#138315=DIRECTION('center_axis',(0.207659145615641,0.978201246800566,6.83074279767453E-15));
#138316=DIRECTION('ref_axis',(0.978201246800566,-0.207659145615641,-3.71317093631252E-29));
#138317=DIRECTION('center_axis',(0.978147600733807,-0.207911690817754,-1.45183957723502E-15));
#138318=DIRECTION('ref_axis',(-0.207911690817754,-0.978147600733807,-6.8296199841607E-15));
#138319=DIRECTION('center_axis',(-3.07718727278846E-18,-7.01224015889347E-15,
1.));
#138320=DIRECTION('ref_axis',(0.,-1.,-7.01167149618415E-15));
#138321=DIRECTION('center_axis',(0.208164222161082,0.978093889466687,-4.54346712784961E-15));
#138322=DIRECTION('ref_axis',(0.978093889466687,-0.208164222161082,-1.72376173614108E-29));
#138323=DIRECTION('center_axis',(0.978147600733808,-0.207911690817747,-1.31409985761785E-15));
#138324=DIRECTION('ref_axis',(-0.207911690817747,-0.978147600733808,-6.82961998416061E-15));
#138325=DIRECTION('center_axis',(0.847099893161665,-0.180025927305153,0.500012436348753));
#138326=DIRECTION('ref_axis',(0.48887998035015,-0.104926459537374,-0.866017784402716));
#138327=DIRECTION('center_axis',(-0.518344615107841,0.110177549147469,-0.84804467314674));
#138328=DIRECTION('ref_axis',(0.853239260760972,1.65387964661466E-15,-0.521519667794101));
#138329=DIRECTION('center_axis',(-0.489078698392291,0.103956896853528,-0.866022511471548));
#138330=DIRECTION('ref_axis',(-0.846158656401361,0.18443299107549,0.499999999999992));
#138331=DIRECTION('center_axis',(0.489078713616248,-0.103956889752271,0.866022503726381));
#138332=DIRECTION('ref_axis',(-0.870740345484772,7.4899534609633E-16,0.491743073916715));
#138333=DIRECTION('center_axis',(-0.518344577661002,0.110177567039477,-0.848044693710596));
#138334=DIRECTION('ref_axis',(-0.828561842309103,0.180750786620236,0.529919264233252));
#138335=DIRECTION('center_axis',(-0.518344551206586,0.11017753556482,-0.84804471396932));
#138336=DIRECTION('ref_axis',(0.85323930054104,-8.46008946842943E-16,-0.521519602711381));
#138337=DIRECTION('center_axis',(0.978147600733807,-0.207911690817754,-1.45183957723502E-15));
#138338=DIRECTION('ref_axis',(-0.207911690817754,-0.978147600733807,-6.8296199841607E-15));
#138339=DIRECTION('center_axis',(-0.978147600733807,0.207911690817754,1.45183957723502E-15));
#138340=DIRECTION('ref_axis',(0.207911690817754,0.978147600733807,6.8296199841607E-15));
#138341=DIRECTION('center_axis',(0.978147600733808,-0.207911690817747,-1.31409985761785E-15));
#138342=DIRECTION('ref_axis',(-0.207911690817747,-0.978147600733808,-6.82961998416061E-15));
#138343=DIRECTION('center_axis',(0.978147600733807,-0.207911690817754,-5.48948507886774E-14));
#138344=DIRECTION('ref_axis',(-0.207911690817754,-0.978147600733807,-6.82961998416085E-15));
#138345=DIRECTION('center_axis',(0.978147600733808,-0.207911690817747,-1.31409985761785E-15));
#138346=DIRECTION('ref_axis',(-0.207911690817747,-0.978147600733808,-6.82961998416061E-15));
#138347=DIRECTION('center_axis',(-0.847119506978909,0.180025582247284,0.499979330205096));
#138348=DIRECTION('ref_axis',(0.489253749388308,-0.103008581350974,0.866036951219486));
#138349=DIRECTION('center_axis',(0.489078846174003,-0.103956917928279,-0.866022425483289));
#138350=DIRECTION('ref_axis',(0.870740269393776,1.33909771088141E-16,0.491743208652702));
#138351=DIRECTION('center_axis',(0.489078854947432,-0.103956919793121,-0.866022420304715));
#138352=DIRECTION('ref_axis',(0.207911690812507,0.978147600734922,-3.08152452956608E-12));
#138353=DIRECTION('center_axis',(-0.497265934578267,0.0522647557775134,
-0.86602250872106));
#138354=DIRECTION('ref_axis',(-0.104528463268336,-0.994521895368201,3.84644198399901E-13));
#138355=DIRECTION('center_axis',(-0.861270944310119,0.0905534316538301,
-0.500012436348208));
#138356=DIRECTION('ref_axis',(0.497376550147982,-0.0512812291239624,-0.866017784403084));
#138357=DIRECTION('center_axis',(0.497265943181925,-0.0522647566817473,
0.866022503726311));
#138358=DIRECTION('ref_axis',(-0.867207748104374,-6.20026837782905E-15,
0.497946504785143));
#138359=DIRECTION('center_axis',(0.994521895368276,-0.104528463267629,-7.29918357753754E-16));
#138360=DIRECTION('ref_axis',(-0.104528463267629,-0.994521895368276,-6.82961998416064E-15));
#138361=DIRECTION('center_axis',(-0.994521895368275,0.10452846326764,5.89872860613779E-16));
#138362=DIRECTION('ref_axis',(0.10452846326764,0.994521895368275,6.82961998416066E-15));
#138363=DIRECTION('center_axis',(-0.994521895368276,0.104528463267629,7.29918357753754E-16));
#138364=DIRECTION('ref_axis',(0.104528463267629,0.994521895368276,6.82961998416064E-15));
#138365=DIRECTION('center_axis',(-0.994521895368275,0.10452846326764,5.89872860613779E-16));
#138366=DIRECTION('ref_axis',(0.10452846326764,0.994521895368275,6.82961998416066E-15));
#138367=DIRECTION('center_axis',(0.994521895368276,-0.10452846326763,-7.29918357753759E-16));
#138368=DIRECTION('ref_axis',(-0.10452846326763,-0.994521895368276,-6.82961998416064E-15));
#138369=DIRECTION('center_axis',(-0.527021232978627,0.0553921636609735,
0.848045003637569));
#138370=DIRECTION('ref_axis',(-0.849349030019368,7.51365298055634E-15,-0.527831625809934));
#138371=DIRECTION('center_axis',(0.497266077958573,-0.0522647708473797,
-0.866022425483295));
#138372=DIRECTION('ref_axis',(0.867207670398082,-6.90944293724234E-15,0.497946640115919));
#138373=DIRECTION('center_axis',(0.527021207133031,-0.0553921391946541,
-0.848045021297503));
#138374=DIRECTION('ref_axis',(0.843841975853669,-0.0843581245756499,0.529919264233199));
#138375=DIRECTION('center_axis',(-0.527021177161347,0.055392157794341,0.84804503870865));
#138376=DIRECTION('ref_axis',(-0.849349064867519,7.13597841401006E-15,-0.527831569734769));
#138377=DIRECTION('center_axis',(0.497266092833649,-0.0522647618388216,
-0.866022417485765));
#138378=DIRECTION('ref_axis',(0.861744800189553,-0.0859994148019896,0.499999999999982));
#138379=DIRECTION('center_axis',(0.861289491529666,-0.0905598208266563,
-0.499979330205173));
#138380=DIRECTION('ref_axis',(0.497139368682358,-0.0532207405870175,0.866036951219448));
#138381=DIRECTION('center_axis',(0.104287292793425,0.994547213842469,6.94488607545883E-15));
#138382=DIRECTION('ref_axis',(0.994547213842469,-0.104287292793425,-7.04137303703978E-30));
#138383=DIRECTION('center_axis',(-0.994521895368275,0.10452846326764,5.89872860613779E-16));
#138384=DIRECTION('ref_axis',(0.10452846326764,0.994521895368275,6.82961998416066E-15));
#138385=DIRECTION('center_axis',(0.994521895368276,-0.10452846326763,-7.29918357753759E-16));
#138386=DIRECTION('ref_axis',(-0.10452846326763,-0.994521895368276,-6.82961998416064E-15));
#138387=DIRECTION('center_axis',(-7.71409749858844E-19,-6.99768205256557E-15,
1.));
#138388=DIRECTION('ref_axis',(0.,-1.,-6.99559154385642E-15));
#138389=DIRECTION('center_axis',(0.104769627595152,0.994496518411992,6.94453207115987E-15));
#138390=DIRECTION('ref_axis',(0.994496518411992,-0.104769627595152,-1.55544708777506E-29));
#138391=DIRECTION('center_axis',(0.527021693999021,-0.0553922121161813,
0.848044713969304));
#138392=DIRECTION('ref_axis',(-0.849348742192388,-6.71201041252531E-15,
0.527832088960314));
#138393=DIRECTION('center_axis',(0.527021177161445,-0.0553921577943047,
-0.848045038708591));
#138394=DIRECTION('ref_axis',(0.849349064867459,-7.06533916556894E-15,0.527831569734866));
#138395=DIRECTION('center_axis',(0.527021723799459,-0.0553922405982832,
0.848044693589288));
#138396=DIRECTION('ref_axis',(-0.843864204095891,0.084135476703687,0.529919264233196));
#138397=DIRECTION('center_axis',(0.527021758969976,-0.0553922189449034,
0.848044673146735));
#138398=DIRECTION('ref_axis',(-0.849348701629309,-6.7822964013418E-15,0.527832154231445));
#138399=DIRECTION('center_axis',(-0.52702120729681,0.0553921391509293,0.848045021198578));
#138400=DIRECTION('ref_axis',(0.842941044393908,-0.0929299148319318,0.529919264233183));
#138401=DIRECTION('center_axis',(0.527021232978636,-0.0553921636609745,
-0.848045003637563));
#138402=DIRECTION('ref_axis',(0.849349030019363,-7.39781141104914E-15,0.527831625809943));
#138403=DIRECTION('center_axis',(0.10427169399366,0.994548849394384,1.94343765541562E-14));
#138404=DIRECTION('ref_axis',(0.994548849394384,-0.10427169399366,1.05093255583232E-28));
#138405=DIRECTION('center_axis',(0.994521895368276,-0.104528463267629,-7.29918357753754E-16));
#138406=DIRECTION('ref_axis',(-0.104528463267629,-0.994521895368276,-6.82961998416064E-15));
#138407=DIRECTION('center_axis',(-7.71409749858844E-19,-6.99768205256557E-15,
1.));
#138408=DIRECTION('ref_axis',(0.,-1.,-6.99665721032508E-15));
#138409=DIRECTION('center_axis',(0.104785225574074,0.99449487505034,6.94452059562679E-15));
#138410=DIRECTION('ref_axis',(0.994494875050339,-0.104785225574074,2.30312721721348E-29));
#138411=DIRECTION('center_axis',(0.994521895368275,-0.10452846326764,-5.89872860613779E-16));
#138412=DIRECTION('ref_axis',(-0.10452846326764,-0.994521895368275,-6.82961998416068E-15));
#138413=DIRECTION('center_axis',(0.861277224843014,-0.0904936763731455,
0.500012436348527));
#138414=DIRECTION('ref_axis',(0.49716964624011,-0.0532497883133837,-0.866017784402875));
#138415=DIRECTION('center_axis',(-0.527021758969983,0.0553922189449046,
-0.84804467314673));
#138416=DIRECTION('ref_axis',(0.849348701629304,6.78821573216834E-15,-0.527832154231452));
#138417=DIRECTION('center_axis',(-0.497265928783043,0.0522647653398099,
-0.866022511471563));
#138418=DIRECTION('ref_axis',(-0.86080180787837,0.0949749838292013,0.499999999999973));
#138419=DIRECTION('center_axis',(0.497265943181779,-0.0522647566817799,
0.866022503726393));
#138420=DIRECTION('ref_axis',(-0.867207748104458,-6.7740073172956E-15,0.497946504784997));
#138421=DIRECTION('center_axis',(-0.527021723597956,0.0553922406580129,
-0.848044693710611));
#138422=DIRECTION('ref_axis',(-0.842916495801727,0.0931523188110504,0.529919264233205));
#138423=DIRECTION('center_axis',(-0.527021693999002,0.0553922121161323,
-0.848044713969319));
#138424=DIRECTION('ref_axis',(0.849348742192401,6.32826558914321E-15,-0.527832088960293));
#138425=DIRECTION('center_axis',(0.994521895368276,-0.104528463267629,-2.15769772104614E-15));
#138426=DIRECTION('ref_axis',(-0.104528463267629,-0.994521895368276,-6.82961998416064E-15));
#138427=DIRECTION('center_axis',(-0.994521895368276,0.104528463267628,7.29918357753744E-16));
#138428=DIRECTION('ref_axis',(0.104528463267628,0.994521895368276,6.82961998416064E-15));
#138429=DIRECTION('center_axis',(0.994521895368275,-0.10452846326764,-5.89872860613779E-16));
#138430=DIRECTION('ref_axis',(-0.10452846326764,-0.994521895368275,-6.82961998416068E-15));
#138431=DIRECTION('center_axis',(0.994521895368276,-0.104528463267629,-1.60286761075628E-17));
#138432=DIRECTION('ref_axis',(-0.104528463267629,-0.994521895368276,-6.82961998416064E-15));
#138433=DIRECTION('center_axis',(0.994521895368275,-0.10452846326764,-5.89872860613779E-16));
#138434=DIRECTION('ref_axis',(-0.10452846326764,-0.994521895368275,-6.82961998416068E-15));
#138435=DIRECTION('center_axis',(-0.861296695145334,0.0904912830026632,
0.499979330205017));
#138436=DIRECTION('ref_axis',(0.497340894868541,-0.0513033470031167,0.86603695121954));
#138437=DIRECTION('center_axis',(0.497266077958562,-0.0522647708473785,
-0.866022425483302));
#138438=DIRECTION('ref_axis',(0.867207670398088,-6.98667298451095E-15,0.497946640115907));
#138439=DIRECTION('center_axis',(0.49726608688627,-0.0522647717857253,-0.866022420300423));
#138440=DIRECTION('ref_axis',(0.104528463273401,0.994521895367669,3.35252384984286E-12));
#138441=DIRECTION('center_axis',(0.,0.,1.));
#138442=DIRECTION('ref_axis',(1.,0.,0.));
#138443=DIRECTION('center_axis',(0.,0.,1.));
#138444=DIRECTION('ref_axis',(1.,0.,0.));
#138445=DIRECTION('center_axis',(1.22464679914735E-16,-1.,0.));
#138446=DIRECTION('ref_axis',(-1.,-1.22464679914735E-16,0.));
#138447=DIRECTION('center_axis',(0.,0.,-1.));
#138448=DIRECTION('ref_axis',(1.,0.,0.));
#138449=DIRECTION('center_axis',(0.,0.,1.));
#138450=DIRECTION('ref_axis',(1.,0.,0.));
#138451=DIRECTION('center_axis',(0.,0.,1.));
#138452=DIRECTION('ref_axis',(1.,0.,0.));
#138453=DIRECTION('center_axis',(-1.22464679914735E-16,1.,0.));
#138454=DIRECTION('ref_axis',(-1.,-1.22464679914735E-16,0.));
#138455=DIRECTION('center_axis',(0.,0.,-1.));
#138456=DIRECTION('ref_axis',(1.,0.,0.));
#138457=DIRECTION('center_axis',(0.,0.,-1.));
#138458=DIRECTION('ref_axis',(-1.,0.,0.));
#138459=DIRECTION('center_axis',(0.,0.,-1.));
#138460=DIRECTION('ref_axis',(-1.,0.,0.));
#138461=DIRECTION('center_axis',(-1.22464679914735E-16,-1.,0.));
#138462=DIRECTION('ref_axis',(1.,-1.22464679914735E-16,0.));
#138463=DIRECTION('center_axis',(0.,0.,1.));
#138464=DIRECTION('ref_axis',(-1.,0.,0.));
#138465=DIRECTION('center_axis',(0.,0.,1.));
#138466=DIRECTION('ref_axis',(-1.,0.,0.));
#138467=DIRECTION('center_axis',(0.,0.,1.));
#138468=DIRECTION('ref_axis',(1.,0.,0.));
#138469=DIRECTION('center_axis',(0.,0.,1.));
#138470=DIRECTION('ref_axis',(1.,0.,0.));
#138471=DIRECTION('',(0.,0.,1.));
#138472=DIRECTION('center_axis',(0.,0.,1.));
#138473=DIRECTION('ref_axis',(1.,0.,0.));
#138474=DIRECTION('',(0.,0.,1.));
#138475=DIRECTION('center_axis',(0.,0.,1.));
#138476=DIRECTION('ref_axis',(1.,0.,0.));
#138477=DIRECTION('center_axis',(0.,0.,-1.));
#138478=DIRECTION('ref_axis',(-1.,0.,0.));
#138479=DIRECTION('',(0.,0.,-1.));
#138480=DIRECTION('center_axis',(0.,0.,-1.));
#138481=DIRECTION('ref_axis',(-1.,0.,0.));
#138482=DIRECTION('center_axis',(0.,0.,-1.));
#138483=DIRECTION('ref_axis',(-1.,0.,0.));
#138484=DIRECTION('center_axis',(0.,0.,-1.));
#138485=DIRECTION('ref_axis',(-1.,0.,0.));
#138486=DIRECTION('center_axis',(0.,0.,1.));
#138487=DIRECTION('ref_axis',(1.,0.,0.));
#138488=DIRECTION('center_axis',(0.,0.,1.));
#138489=DIRECTION('ref_axis',(1.,0.,0.));
#138490=DIRECTION('center_axis',(0.,0.,1.));
#138491=DIRECTION('ref_axis',(1.,0.,0.));
#138492=DIRECTION('center_axis',(1.22464679914735E-16,-1.,0.));
#138493=DIRECTION('ref_axis',(-1.,-1.22464679914735E-16,0.));
#138494=DIRECTION('center_axis',(0.,0.,-1.));
#138495=DIRECTION('ref_axis',(1.,0.,0.));
#138496=DIRECTION('center_axis',(0.,0.,1.));
#138497=DIRECTION('ref_axis',(1.,0.,0.));
#138498=DIRECTION('center_axis',(0.,0.,1.));
#138499=DIRECTION('ref_axis',(1.,0.,0.));
#138500=DIRECTION('center_axis',(1.22464679914735E-16,-1.,0.));
#138501=DIRECTION('ref_axis',(-1.,-1.22464679914735E-16,0.));
#138502=DIRECTION('center_axis',(0.,0.,-1.));
#138503=DIRECTION('ref_axis',(1.,0.,0.));
#138504=DIRECTION('center_axis',(0.,0.,1.));
#138505=DIRECTION('ref_axis',(1.,0.,0.));
#138506=DIRECTION('center_axis',(0.,0.,1.));
#138507=DIRECTION('ref_axis',(1.,0.,0.));
#138508=DIRECTION('',(0.,0.,1.));
#138509=DIRECTION('center_axis',(0.,0.,1.));
#138510=DIRECTION('ref_axis',(1.,0.,0.));
#138511=DIRECTION('',(0.,0.,-1.));
#138512=DIRECTION('center_axis',(0.,0.,1.));
#138513=DIRECTION('ref_axis',(1.,0.,0.));
#138514=DIRECTION('center_axis',(0.,0.,1.));
#138515=DIRECTION('ref_axis',(1.,0.,0.));
#138516=DIRECTION('center_axis',(0.,0.,1.));
#138517=DIRECTION('ref_axis',(1.,0.,0.));
#138518=DIRECTION('center_axis',(0.,0.,1.));
#138519=DIRECTION('ref_axis',(1.,0.,0.));
#138520=DIRECTION('center_axis',(0.,0.,-1.));
#138521=DIRECTION('ref_axis',(1.,0.,0.));
#138522=DIRECTION('center_axis',(1.22464679914735E-16,-1.,0.));
#138523=DIRECTION('ref_axis',(-1.,-1.22464679914735E-16,0.));
#138524=DIRECTION('center_axis',(0.,0.,-1.));
#138525=DIRECTION('ref_axis',(1.,0.,0.));
#138526=DIRECTION('center_axis',(0.,0.,1.));
#138527=DIRECTION('ref_axis',(-1.83697019872103E-16,-1.,0.));
#138528=DIRECTION('center_axis',(0.,0.,-1.));
#138529=DIRECTION('ref_axis',(-1.,0.,0.));
#138530=DIRECTION('center_axis',(-0.990048018535926,0.14072995769589,0.));
#138531=DIRECTION('ref_axis',(-0.14072995769589,-0.990048018535926,0.));
#138532=DIRECTION('center_axis',(0.,0.,1.));
#138533=DIRECTION('ref_axis',(1.,0.,0.));
#138534=DIRECTION('center_axis',(-0.990048018535926,-0.140729957695892,
0.));
#138535=DIRECTION('ref_axis',(0.140729957695892,-0.990048018535926,0.));
#138536=DIRECTION('center_axis',(0.,0.,1.));
#138537=DIRECTION('ref_axis',(1.,0.,0.));
#138538=DIRECTION('center_axis',(0.,0.,-1.));
#138539=DIRECTION('ref_axis',(1.,0.,0.));
#138540=DIRECTION('center_axis',(0.573576436351042,-0.819152044288994,-9.00692692729371E-16));
#138541=DIRECTION('ref_axis',(0.819152044288994,0.573576436351042,-6.35202185790921E-32));
#138542=DIRECTION('center_axis',(0.,0.,1.));
#138543=DIRECTION('ref_axis',(1.,0.,0.));
#138544=DIRECTION('center_axis',(-0.819152044288994,0.573576436351042,0.));
#138545=DIRECTION('ref_axis',(-0.573576436351042,-0.819152044288994,0.));
#138546=DIRECTION('center_axis',(0.,0.,1.));
#138547=DIRECTION('ref_axis',(1.,0.,0.));
#138548=DIRECTION('center_axis',(0.,0.,-1.));
#138549=DIRECTION('ref_axis',(1.,0.,0.));
#138550=DIRECTION('center_axis',(0.819152044288994,0.573576436351042,-2.6835009273527E-15));
#138551=DIRECTION('ref_axis',(-0.573576436351042,0.819152044288994,-8.18154877134231E-32));
#138552=DIRECTION('center_axis',(0.,0.,1.));
#138553=DIRECTION('ref_axis',(1.,0.,0.));
#138554=DIRECTION('center_axis',(-0.573576436351042,-0.819152044288994,
0.));
#138555=DIRECTION('ref_axis',(0.819152044288994,-0.573576436351042,0.));
#138556=DIRECTION('center_axis',(0.,0.,1.));
#138557=DIRECTION('ref_axis',(1.,0.,0.));
#138558=DIRECTION('center_axis',(-0.309478661079813,-0.950906387788118,
0.));
#138559=DIRECTION('ref_axis',(0.950906387788118,-0.309478661079813,0.));
#138560=DIRECTION('center_axis',(0.,0.,-1.));
#138561=DIRECTION('ref_axis',(1.,-4.09777199049639E-15,0.));
#138562=DIRECTION('center_axis',(0.573576436351045,-0.819152044288993,0.));
#138563=DIRECTION('ref_axis',(0.819152044288993,0.573576436351045,0.));
#138564=DIRECTION('center_axis',(0.,0.,1.));
#138565=DIRECTION('ref_axis',(1.,0.,0.));
#138566=DIRECTION('center_axis',(0.573576436351045,0.819152044288993,1.49186591246458E-15));
#138567=DIRECTION('ref_axis',(-0.819152044288993,0.573576436351045,-8.00341439460267E-32));
#138568=DIRECTION('center_axis',(0.,0.,-1.));
#138569=DIRECTION('ref_axis',(1.,1.36592399683213E-14,0.));
#138570=DIRECTION('center_axis',(0.309478661079813,-0.950906387788118,0.));
#138571=DIRECTION('ref_axis',(0.950906387788118,0.309478661079813,0.));
#138572=DIRECTION('center_axis',(0.,0.,1.));
#138573=DIRECTION('ref_axis',(1.,0.,0.));
#138574=DIRECTION('center_axis',(0.309478661079813,0.950906387788118,0.));
#138575=DIRECTION('ref_axis',(-0.950906387788118,0.309478661079813,0.));
#138576=DIRECTION('center_axis',(0.,0.,-1.));
#138577=DIRECTION('ref_axis',(1.,1.0927391974657E-14,0.));
#138578=DIRECTION('center_axis',(-0.573576436351046,0.819152044288992,0.));
#138579=DIRECTION('ref_axis',(-0.819152044288992,-0.573576436351046,0.));
#138580=DIRECTION('center_axis',(0.,0.,1.));
#138581=DIRECTION('ref_axis',(1.,0.,0.));
#138582=DIRECTION('center_axis',(0.,0.,1.));
#138583=DIRECTION('ref_axis',(1.,0.,0.));
#138584=DIRECTION('center_axis',(0.,0.,-1.));
#138585=DIRECTION('ref_axis',(1.,8.88178419700125E-16,0.));
#138586=DIRECTION('center_axis',(-0.309478661079813,0.950906387788118,0.));
#138587=DIRECTION('ref_axis',(-0.950906387788118,-0.309478661079813,0.));
#138588=DIRECTION('center_axis',(0.,0.,1.));
#138589=DIRECTION('ref_axis',(1.,0.,0.));
#138590=DIRECTION('center_axis',(-0.573576436351046,-0.819152044288992,
-1.49186591246457E-15));
#138591=DIRECTION('ref_axis',(0.819152044288992,-0.573576436351046,-5.52212474718673E-32));
#138592=DIRECTION('center_axis',(0.,0.,-1.));
#138593=DIRECTION('ref_axis',(1.,9.56146797782492E-15,0.));
#138594=DIRECTION('center_axis',(0.,0.,1.));
#138595=DIRECTION('ref_axis',(1.,0.,0.));
#138596=DIRECTION('',(0.,0.,-1.));
#138597=DIRECTION('center_axis',(0.,0.,-1.));
#138598=DIRECTION('ref_axis',(-1.,0.,0.));
#138599=DIRECTION('',(0.,0.,1.));
#138600=DIRECTION('center_axis',(0.,0.,1.));
#138601=DIRECTION('ref_axis',(1.,0.,0.));
#138602=DIRECTION('',(0.,0.,-1.));
#138603=DIRECTION('center_axis',(0.,0.,-1.));
#138604=DIRECTION('ref_axis',(-1.,0.,0.));
#138605=DIRECTION('',(0.,0.,1.));
#138606=DIRECTION('center_axis',(0.,0.,-1.));
#138607=DIRECTION('ref_axis',(-1.,0.,0.));
#138608=DIRECTION('center_axis',(0.,0.,1.));
#138609=DIRECTION('ref_axis',(-1.,0.,0.));
#138610=DIRECTION('center_axis',(0.,0.,-1.));
#138611=DIRECTION('ref_axis',(-1.,0.,0.));
#138612=DIRECTION('center_axis',(0.,0.,-1.));
#138613=DIRECTION('ref_axis',(-1.,0.,0.));
#138614=DIRECTION('center_axis',(0.,0.,-1.));
#138615=DIRECTION('ref_axis',(1.,0.,0.));
#138616=DIRECTION('',(0.,0.,-1.));
#138617=DIRECTION('center_axis',(0.,0.,-1.));
#138618=DIRECTION('ref_axis',(-1.,0.,0.));
#138619=DIRECTION('center_axis',(0.,0.,-1.));
#138620=DIRECTION('ref_axis',(-1.,0.,0.));
#138621=DIRECTION('center_axis',(0.,0.,1.));
#138622=DIRECTION('ref_axis',(1.,0.,0.));
#138623=DIRECTION('',(0.,0.,-1.));
#138624=DIRECTION('center_axis',(0.,0.,-1.));
#138625=DIRECTION('ref_axis',(-1.,0.,0.));
#138626=DIRECTION('center_axis',(0.,0.,-1.));
#138627=DIRECTION('ref_axis',(-1.,0.,0.));
#138628=DIRECTION('center_axis',(0.,0.,1.));
#138629=DIRECTION('ref_axis',(1.,0.,0.));
#138630=DIRECTION('',(0.,0.,-1.));
#138631=DIRECTION('center_axis',(0.,0.,-1.));
#138632=DIRECTION('ref_axis',(-1.,0.,0.));
#138633=DIRECTION('center_axis',(0.,0.,-1.));
#138634=DIRECTION('ref_axis',(-1.,0.,0.));
#138635=DIRECTION('center_axis',(0.,0.,1.));
#138636=DIRECTION('ref_axis',(1.,0.,0.));
#138637=DIRECTION('',(0.,0.,-1.));
#138638=DIRECTION('center_axis',(0.,0.,-1.));
#138639=DIRECTION('ref_axis',(-1.,0.,0.));
#138640=DIRECTION('center_axis',(0.,0.,-1.));
#138641=DIRECTION('ref_axis',(-1.,0.,0.));
#138642=DIRECTION('center_axis',(0.,0.,1.));
#138643=DIRECTION('ref_axis',(1.,0.,0.));
#138644=DIRECTION('',(0.,0.,-1.));
#138645=DIRECTION('center_axis',(0.,0.,-1.));
#138646=DIRECTION('ref_axis',(-1.,0.,0.));
#138647=DIRECTION('center_axis',(0.,0.,1.));
#138648=DIRECTION('ref_axis',(1.,0.,0.));
#138649=DIRECTION('',(0.,0.,1.));
#138650=DIRECTION('center_axis',(0.,0.,-1.));
#138651=DIRECTION('ref_axis',(-1.,0.,0.));
#138652=DIRECTION('',(0.,0.,-1.));
#138653=DIRECTION('center_axis',(0.,0.,-1.));
#138654=DIRECTION('ref_axis',(5.0532154980743E-16,-1.,0.));
#138655=DIRECTION('center_axis',(0.,0.,1.));
#138656=DIRECTION('ref_axis',(-1.,6.21724893790088E-15,0.));
#138657=DIRECTION('center_axis',(0.,0.,1.));
#138658=DIRECTION('ref_axis',(1.,0.,0.));
#138659=DIRECTION('center_axis',(0.,0.,1.));
#138660=DIRECTION('ref_axis',(1.,0.,0.));
#138661=DIRECTION('center_axis',(0.,0.,1.));
#138662=DIRECTION('ref_axis',(-1.,0.,0.));
#138663=DIRECTION('center_axis',(0.,0.,1.));
#138664=DIRECTION('ref_axis',(1.,0.,0.));
#138665=DIRECTION('center_axis',(0.,0.,1.));
#138666=DIRECTION('ref_axis',(-1.,4.44089209850063E-15,0.));
#138667=DIRECTION('center_axis',(0.,0.,1.));
#138668=DIRECTION('ref_axis',(1.,0.,0.));
#138669=DIRECTION('center_axis',(0.,0.,1.));
#138670=DIRECTION('ref_axis',(-1.,-5.32907051820075E-15,0.));
#138671=DIRECTION('center_axis',(0.,0.,-1.));
#138672=DIRECTION('ref_axis',(-1.,0.,0.));
#138673=DIRECTION('center_axis',(0.,0.,-1.));
#138674=DIRECTION('ref_axis',(1.,0.,0.));
#138675=DIRECTION('',(0.,0.,1.));
#138676=DIRECTION('center_axis',(0.,0.,1.));
#138677=DIRECTION('ref_axis',(-1.,0.,0.));
#138678=DIRECTION('',(0.,0.,-1.));
#138679=DIRECTION('center_axis',(0.,0.,-1.));
#138680=DIRECTION('ref_axis',(-1.,0.,0.));
#138681=DIRECTION('',(0.,0.,-1.));
#138682=DIRECTION('center_axis',(0.,0.,1.));
#138683=DIRECTION('ref_axis',(1.,0.,0.));
#138684=DIRECTION('',(0.,0.,1.));
#138685=DIRECTION('center_axis',(0.,0.,-1.));
#138686=DIRECTION('ref_axis',(-1.,0.,0.));
#138687=DIRECTION('center_axis',(0.,0.,-1.));
#138688=DIRECTION('ref_axis',(1.,1.11022302462516E-15,0.));
#138689=DIRECTION('',(0.,0.,1.));
#138690=DIRECTION('center_axis',(0.,0.,1.));
#138691=DIRECTION('ref_axis',(1.,0.,0.));
#138692=DIRECTION('',(0.,0.,-1.));
#138693=DIRECTION('center_axis',(0.,0.,-1.));
#138694=DIRECTION('ref_axis',(-1.,0.,0.));
#138695=DIRECTION('',(0.,0.,-1.));
#138696=DIRECTION('center_axis',(0.,0.,1.));
#138697=DIRECTION('ref_axis',(1.,0.,0.));
#138698=DIRECTION('',(0.,0.,1.));
#138699=DIRECTION('center_axis',(0.,1.,0.));
#138700=DIRECTION('ref_axis',(0.,0.,1.));
#138701=DIRECTION('',(0.,0.,-1.));
#138702=DIRECTION('',(-1.,0.,0.));
#138703=DIRECTION('',(-1.,0.,0.));
#138704=DIRECTION('center_axis',(1.,0.,0.));
#138705=DIRECTION('ref_axis',(0.,0.,-1.));
#138706=DIRECTION('',(0.,1.,0.));
#138707=DIRECTION('',(0.,1.,0.));
#138708=DIRECTION('center_axis',(-1.,0.,0.));
#138709=DIRECTION('ref_axis',(0.,0.,1.));
#138710=DIRECTION('',(0.,0.,-1.));
#138711=DIRECTION('',(0.,-1.,0.));
#138712=DIRECTION('',(0.,0.,-1.));
#138713=DIRECTION('',(0.,-1.,0.));
#138714=DIRECTION('center_axis',(0.,0.,-1.));
#138715=DIRECTION('ref_axis',(0.707106781186548,-0.707106781186547,0.));
#138716=DIRECTION('',(0.,0.,1.));
#138717=DIRECTION('',(0.,0.,1.));
#138718=DIRECTION('center_axis',(0.,0.,1.));
#138719=DIRECTION('ref_axis',(1.,0.,0.));
#138720=DIRECTION('center_axis',(0.,0.,-1.));
#138721=DIRECTION('ref_axis',(-1.,0.,0.));
#138722=DIRECTION('center_axis',(0.,0.,1.));
#138723=DIRECTION('ref_axis',(1.,0.,0.));
#138724=DIRECTION('center_axis',(0.,0.,-1.));
#138725=DIRECTION('ref_axis',(0.707106781186547,0.707106781186547,0.));
#138726=DIRECTION('',(0.,0.,1.));
#138727=DIRECTION('',(0.,0.,1.));
#138728=DIRECTION('center_axis',(0.,0.,1.));
#138729=DIRECTION('ref_axis',(1.,0.,0.));
#138730=DIRECTION('center_axis',(0.,0.,-1.));
#138731=DIRECTION('ref_axis',(-1.,0.,0.));
#138732=DIRECTION('',(0.,0.,-1.));
#138733=DIRECTION('center_axis',(0.,0.,1.));
#138734=DIRECTION('ref_axis',(1.,0.,0.));
#138735=DIRECTION('center_axis',(0.,-1.,0.));
#138736=DIRECTION('ref_axis',(0.,0.,-1.));
#138737=DIRECTION('',(1.,0.,0.));
#138738=DIRECTION('',(1.,0.,0.));
#138739=DIRECTION('',(1.,0.,0.));
#138740=DIRECTION('center_axis',(0.,0.,1.));
#138741=DIRECTION('ref_axis',(1.,0.,0.));
#138742=DIRECTION('',(0.,0.,1.));
#138743=DIRECTION('center_axis',(0.,0.,-1.));
#138744=DIRECTION('ref_axis',(-1.,0.,0.));
#138745=DIRECTION('',(0.,0.,1.));
#138746=DIRECTION('center_axis',(0.,0.,-1.));
#138747=DIRECTION('ref_axis',(-1.,0.,0.));
#138748=DIRECTION('center_axis',(1.,0.,0.));
#138749=DIRECTION('ref_axis',(0.,0.,-1.));
#138750=DIRECTION('',(0.,1.,0.));
#138751=DIRECTION('',(0.,0.,1.));
#138752=DIRECTION('',(0.,1.,0.));
#138753=DIRECTION('center_axis',(0.,0.,1.));
#138754=DIRECTION('ref_axis',(1.,0.,0.));
#138755=DIRECTION('center_axis',(0.,0.,-1.));
#138756=DIRECTION('ref_axis',(-1.,0.,0.));
#138757=DIRECTION('',(0.,0.,1.));
#138758=DIRECTION('center_axis',(0.,0.,-1.));
#138759=DIRECTION('ref_axis',(-1.,0.,0.));
#138760=DIRECTION('center_axis',(-1.5419764230905E-16,-1.,0.));
#138761=DIRECTION('ref_axis',(1.,-1.5419764230905E-16,0.));
#138762=DIRECTION('',(1.,-1.5419764230905E-16,0.));
#138763=DIRECTION('',(0.,0.,1.));
#138764=DIRECTION('',(1.,-1.5419764230905E-16,0.));
#138765=DIRECTION('center_axis',(0.,0.,1.));
#138766=DIRECTION('ref_axis',(1.,0.,0.));
#138767=DIRECTION('center_axis',(0.,0.,-1.));
#138768=DIRECTION('ref_axis',(-1.,0.,0.));
#138769=DIRECTION('',(0.,0.,1.));
#138770=DIRECTION('center_axis',(0.,0.,-1.));
#138771=DIRECTION('ref_axis',(-1.,0.,0.));
#138772=DIRECTION('center_axis',(-1.,7.70988211545247E-17,0.));
#138773=DIRECTION('ref_axis',(-7.70988211545247E-17,-1.,0.));
#138774=DIRECTION('',(-7.70988211545248E-17,-1.,0.));
#138775=DIRECTION('',(0.,0.,1.));
#138776=DIRECTION('',(-7.70988211545248E-17,-1.,0.));
#138777=DIRECTION('center_axis',(0.,0.,1.));
#138778=DIRECTION('ref_axis',(1.,0.,0.));
#138779=DIRECTION('center_axis',(0.,0.,-1.));
#138780=DIRECTION('ref_axis',(-1.,0.,0.));
#138781=DIRECTION('',(0.,0.,1.));
#138782=DIRECTION('center_axis',(0.,0.,-1.));
#138783=DIRECTION('ref_axis',(-1.,0.,0.));
#138784=DIRECTION('center_axis',(0.,1.,0.));
#138785=DIRECTION('ref_axis',(0.,0.,1.));
#138786=DIRECTION('',(-1.,0.,0.));
#138787=DIRECTION('',(-1.,0.,0.));
#138788=DIRECTION('center_axis',(0.,0.,1.));
#138789=DIRECTION('ref_axis',(1.,0.,0.));
#138790=DIRECTION('',(0.,1.,0.));
#138791=DIRECTION('center_axis',(0.,0.,1.));
#138792=DIRECTION('ref_axis',(1.,0.,0.));
#138793=DIRECTION('',(0.,-1.,0.));
#138794=DIRECTION('center_axis',(1.,0.,0.));
#138795=DIRECTION('ref_axis',(0.,0.,-1.));
#138796=DIRECTION('',(0.,1.,0.));
#138797=DIRECTION('',(0.,0.,1.));
#138798=DIRECTION('',(0.,0.,1.));
#138799=DIRECTION('center_axis',(1.,3.85138571020619E-14,3.57317646046073E-15));
#138800=DIRECTION('ref_axis',(-3.87079718928684E-14,0.99239999161251,0.123053877011211));
#138801=DIRECTION('center_axis',(1.,0.,0.));
#138802=DIRECTION('ref_axis',(0.,0.,-1.));
#138803=DIRECTION('',(0.,0.,1.));
#138804=DIRECTION('',(0.,-1.,0.));
#138805=DIRECTION('center_axis',(-1.,-3.85138571020628E-14,-3.57317646045933E-15));
#138806=DIRECTION('ref_axis',(-3.8560793292515E-14,0.999999998571857,-5.34442274211441E-5));
#138807=DIRECTION('',(0.,0.,-1.));
#138808=DIRECTION('center_axis',(0.,0.,1.));
#138809=DIRECTION('ref_axis',(1.,0.,0.));
#138810=DIRECTION('center_axis',(0.,0.,-1.));
#138811=DIRECTION('ref_axis',(1.,1.24344978758018E-14,0.));
#138812=DIRECTION('center_axis',(0.,0.,1.));
#138813=DIRECTION('ref_axis',(1.,0.,0.));
#138814=DIRECTION('center_axis',(0.,0.,1.));
#138815=DIRECTION('ref_axis',(1.,0.,0.));
#138816=DIRECTION('',(0.,0.,1.));
#138817=DIRECTION('center_axis',(0.,0.,-1.));
#138818=DIRECTION('ref_axis',(-1.,0.,0.));
#138819=DIRECTION('',(0.,0.,-1.));
#138820=DIRECTION('center_axis',(0.,0.,1.));
#138821=DIRECTION('ref_axis',(1.,0.,0.));
#138822=DIRECTION('',(-1.,0.,0.));
#138823=DIRECTION('center_axis',(0.,0.,1.));
#138824=DIRECTION('ref_axis',(1.,0.,0.));
#138825=DIRECTION('center_axis',(0.,0.,1.));
#138826=DIRECTION('ref_axis',(1.,0.,0.));
#138827=DIRECTION('',(-0.819152044288992,-0.573576436351046,0.));
#138828=DIRECTION('center_axis',(0.,0.,1.));
#138829=DIRECTION('ref_axis',(1.,0.,0.));
#138830=DIRECTION('center_axis',(0.,0.,1.));
#138831=DIRECTION('ref_axis',(1.,0.,0.));
#138832=DIRECTION('',(-1.,0.,0.));
#138833=DIRECTION('',(-0.819152044288992,0.573576436351046,0.));
#138834=DIRECTION('center_axis',(0.,0.,1.));
#138835=DIRECTION('ref_axis',(1.,0.,0.));
#138836=DIRECTION('center_axis',(0.,0.,1.));
#138837=DIRECTION('ref_axis',(1.,0.,0.));
#138838=DIRECTION('center_axis',(0.,0.,1.));
#138839=DIRECTION('ref_axis',(1.,0.,0.));
#138840=DIRECTION('center_axis',(0.,0.,-1.));
#138841=DIRECTION('ref_axis',(-1.,0.,0.));
#138842=DIRECTION('',(0.,0.,-1.));
#138843=DIRECTION('',(0.,0.,1.));
#138844=DIRECTION('center_axis',(0.,0.,1.));
#138845=DIRECTION('ref_axis',(1.,0.,0.));
#138846=DIRECTION('',(0.573576436351045,-0.819152044288992,0.));
#138847=DIRECTION('center_axis',(0.,0.,-1.));
#138848=DIRECTION('ref_axis',(1.,-8.88178419700125E-16,0.));
#138849=DIRECTION('',(-0.819152044288992,0.573576436351046,0.));
#138850=DIRECTION('center_axis',(0.,0.,1.));
#138851=DIRECTION('ref_axis',(1.,0.,0.));
#138852=DIRECTION('center_axis',(0.,0.,1.));
#138853=DIRECTION('ref_axis',(-1.,1.22464679914735E-16,0.));
#138854=DIRECTION('center_axis',(0.,0.,1.));
#138855=DIRECTION('ref_axis',(1.,0.,0.));
#138856=DIRECTION('center_axis',(0.,0.,1.));
#138857=DIRECTION('ref_axis',(1.,0.,0.));
#138858=DIRECTION('',(0.819152044288992,0.573576436351046,0.));
#138859=DIRECTION('center_axis',(0.,0.,-1.));
#138860=DIRECTION('ref_axis',(1.,8.88178419700125E-16,0.));
#138861=DIRECTION('',(-0.573576436351045,-0.819152044288992,0.));
#138862=DIRECTION('center_axis',(0.,0.,1.));
#138863=DIRECTION('ref_axis',(1.,0.,0.));
#138864=DIRECTION('center_axis',(0.,0.,1.));
#138865=DIRECTION('ref_axis',(1.,0.,0.));
#138866=DIRECTION('',(0.,0.,-1.));
#138867=DIRECTION('center_axis',(0.,0.,1.));
#138868=DIRECTION('ref_axis',(1.,0.,0.));
#138869=DIRECTION('',(0.,0.,1.));
#138870=DIRECTION('center_axis',(0.,0.,-1.));
#138871=DIRECTION('ref_axis',(-1.,0.,0.));
#138872=DIRECTION('center_axis',(0.,0.,1.));
#138873=DIRECTION('ref_axis',(1.,0.,0.));
#138874=DIRECTION('',(-0.573576436351046,0.819152044288992,0.));
#138875=DIRECTION('center_axis',(0.,0.,-1.));
#138876=DIRECTION('ref_axis',(1.,0.,0.));
#138877=DIRECTION('',(0.819152044288992,-0.573576436351045,0.));
#138878=DIRECTION('center_axis',(0.,0.,1.));
#138879=DIRECTION('ref_axis',(1.,0.,0.));
#138880=DIRECTION('',(-0.819152044288992,-0.573576436351046,0.));
#138881=DIRECTION('center_axis',(0.,0.,-1.));
#138882=DIRECTION('ref_axis',(1.,-4.44089209850063E-15,0.));
#138883=DIRECTION('',(0.573576436351045,0.819152044288992,0.));
#138884=DIRECTION('center_axis',(-0.573576436351046,0.819152044288992,0.));
#138885=DIRECTION('ref_axis',(-0.819152044288992,-0.573576436351046,0.));
#138886=DIRECTION('',(0.,0.,1.));
#138887=DIRECTION('',(0.819152044288992,0.573576436351046,0.));
#138888=DIRECTION('center_axis',(0.573576436351046,0.819152044288992,0.));
#138889=DIRECTION('ref_axis',(-0.819152044288992,0.573576436351046,0.));
#138890=DIRECTION('',(0.819152044288992,-0.573576436351046,0.));
#138891=DIRECTION('',(0.,0.,-1.));
#138892=DIRECTION('center_axis',(-0.819152044288992,-0.573576436351045,
0.));
#138893=DIRECTION('ref_axis',(0.573576436351045,-0.819152044288992,0.));
#138894=DIRECTION('',(-0.573576436351045,0.819152044288992,0.));
#138895=DIRECTION('',(0.573576436351045,-0.819152044288992,0.));
#138896=DIRECTION('center_axis',(0.,0.,1.));
#138897=DIRECTION('ref_axis',(1.,0.,0.));
#138898=DIRECTION('center_axis',(0.,0.,-1.));
#138899=DIRECTION('ref_axis',(1.,-1.59900175447779E-14,0.));
#138900=DIRECTION('',(0.,-1.,0.));
#138901=DIRECTION('center_axis',(0.,0.,-1.));
#138902=DIRECTION('ref_axis',(1.,0.,0.));
#138903=DIRECTION('',(0.573576436351045,0.819152044288992,0.));
#138904=DIRECTION('center_axis',(0.,0.,-1.));
#138905=DIRECTION('ref_axis',(1.,2.66453525910038E-15,0.));
#138906=DIRECTION('',(-0.573576436351045,0.819152044288992,0.));
#138907=DIRECTION('center_axis',(-0.819152044288992,0.573576436351045,0.));
#138908=DIRECTION('ref_axis',(-0.573576436351045,-0.819152044288992,0.));
#138909=DIRECTION('',(0.573576436351045,0.819152044288992,0.));
#138910=DIRECTION('',(-0.573576436351045,-0.819152044288992,0.));
#138911=DIRECTION('center_axis',(0.573576436351046,-0.819152044288992,0.));
#138912=DIRECTION('ref_axis',(0.819152044288992,0.573576436351046,0.));
#138913=DIRECTION('',(0.,0.,1.));
#138914=DIRECTION('',(-0.819152044288992,-0.573576436351046,0.));
#138915=DIRECTION('',(0.819152044288992,0.573576436351046,0.));
#138916=DIRECTION('center_axis',(0.,0.,1.));
#138917=DIRECTION('ref_axis',(1.,0.,0.));
#138918=DIRECTION('center_axis',(0.,0.,-1.));
#138919=DIRECTION('ref_axis',(1.,1.03161403514696E-15,0.));
#138920=DIRECTION('',(1.,0.,0.));
#138921=DIRECTION('center_axis',(0.,0.,-1.));
#138922=DIRECTION('ref_axis',(1.,1.34109824569105E-14,0.));
#138923=DIRECTION('',(-0.819152044288992,0.573576436351045,0.));
#138924=DIRECTION('center_axis',(0.,0.,1.));
#138925=DIRECTION('ref_axis',(1.,0.,0.));
#138926=DIRECTION('center_axis',(0.,0.,-1.));
#138927=DIRECTION('ref_axis',(1.,0.,0.));
#138928=DIRECTION('center_axis',(0.,0.,1.));
#138929=DIRECTION('ref_axis',(1.,0.,0.));
#138930=DIRECTION('',(-0.819152044288992,-0.573576436351046,0.));
#138931=DIRECTION('center_axis',(-0.573576436351045,-0.819152044288992,
0.));
#138932=DIRECTION('ref_axis',(0.819152044288992,-0.573576436351045,0.));
#138933=DIRECTION('',(-0.819152044288992,0.573576436351045,0.));
#138934=DIRECTION('',(0.,0.,-1.));
#138935=DIRECTION('',(0.819152044288992,-0.573576436351045,0.));
#138936=DIRECTION('center_axis',(0.819152044288992,0.573576436351046,0.));
#138937=DIRECTION('ref_axis',(-0.573576436351046,0.819152044288992,0.));
#138938=DIRECTION('',(0.,0.,1.));
#138939=DIRECTION('',(0.573576436351046,-0.819152044288992,0.));
#138940=DIRECTION('',(-0.573576436351046,0.819152044288992,0.));
#138941=DIRECTION('center_axis',(0.,0.,1.));
#138942=DIRECTION('ref_axis',(1.,0.,0.));
#138943=DIRECTION('center_axis',(0.,0.,-1.));
#138944=DIRECTION('ref_axis',(1.,3.45590701774231E-14,0.));
#138945=DIRECTION('',(0.,1.,0.));
#138946=DIRECTION('center_axis',(0.,0.,-1.));
#138947=DIRECTION('ref_axis',(1.,0.,0.));
#138948=DIRECTION('',(-0.573576436351045,-0.819152044288992,0.));
#138949=DIRECTION('',(0.573576436351046,-0.819152044288992,0.));
#138950=DIRECTION('center_axis',(0.819152044288993,-0.573576436351045,0.));
#138951=DIRECTION('ref_axis',(0.573576436351045,0.819152044288992,0.));
#138952=DIRECTION('',(-0.573576436351045,-0.819152044288993,0.));
#138953=DIRECTION('center_axis',(0.819152044299452,-0.573576436336108,-7.19288685875037E-12));
#138954=DIRECTION('ref_axis',(0.573575979835469,0.819151392348989,-0.00126165307995225));
#138955=DIRECTION('',(0.,0.,-1.));
#138956=DIRECTION('',(0.573576436351045,0.819152044288992,0.));
#138957=DIRECTION('center_axis',(0.,0.,-1.));
#138958=DIRECTION('ref_axis',(-1.,0.,0.));
#138959=DIRECTION('center_axis',(0.,0.,1.));
#138960=DIRECTION('ref_axis',(1.,0.,0.));
#138961=DIRECTION('center_axis',(0.,0.,-1.));
#138962=DIRECTION('ref_axis',(-1.,0.,0.));
#138963=DIRECTION('center_axis',(0.,0.,-1.));
#138964=DIRECTION('ref_axis',(-1.,0.,0.));
#138965=DIRECTION('center_axis',(0.999699861223894,0.0244987210755295,1.16013489275163E-5));
#138966=DIRECTION('ref_axis',(-0.0243127779752216,0.992053772369109,0.123443110603017));
#138967=DIRECTION('center_axis',(0.,0.,-1.));
#138968=DIRECTION('ref_axis',(-1.,0.,0.));
#138969=DIRECTION('center_axis',(-0.999699861223916,0.0244987210746371,
1.16013488461091E-5));
#138970=DIRECTION('ref_axis',(0.0244987211028544,0.999699861287902,2.29639131106108E-6));
#138971=DIRECTION('center_axis',(0.,0.,-1.));
#138972=DIRECTION('ref_axis',(-1.,0.,0.));
#138973=DIRECTION('center_axis',(0.,0.,-1.));
#138974=DIRECTION('ref_axis',(1.,1.22464679914735E-16,0.));
#138975=DIRECTION('center_axis',(0.,0.,1.));
#138976=DIRECTION('ref_axis',(1.,0.,0.));
#138977=DIRECTION('center_axis',(0.,0.,-1.));
#138978=DIRECTION('ref_axis',(-1.,0.,0.));
#138979=DIRECTION('center_axis',(0.,0.,-1.));
#138980=DIRECTION('ref_axis',(1.,5.46369598732852E-15,0.));
#138981=DIRECTION('center_axis',(0.,0.,1.));
#138982=DIRECTION('ref_axis',(1.,0.,0.));
#138983=DIRECTION('center_axis',(0.,0.,-1.));
#138984=DIRECTION('ref_axis',(-1.,0.,0.));
#138985=DIRECTION('center_axis',(0.,0.,-1.));
#138986=DIRECTION('ref_axis',(1.,0.,0.));
#138987=DIRECTION('center_axis',(0.,0.,1.));
#138988=DIRECTION('ref_axis',(-0.986793248448819,-0.161984828968107,0.));
#138989=DIRECTION('center_axis',(0.,0.,-1.));
#138990=DIRECTION('ref_axis',(-1.,0.,0.));
#138991=DIRECTION('center_axis',(0.,0.,1.));
#138992=DIRECTION('ref_axis',(-0.986792877850041,0.161987086597769,0.));
#138993=DIRECTION('center_axis',(0.,0.,-1.));
#138994=DIRECTION('ref_axis',(-1.,0.,0.));
#138995=DIRECTION('center_axis',(0.,0.,1.));
#138996=DIRECTION('ref_axis',(1.,0.,0.));
#138997=DIRECTION('center_axis',(0.,0.,-1.));
#138998=DIRECTION('ref_axis',(-1.,0.,0.));
#138999=DIRECTION('center_axis',(0.,0.,1.));
#139000=DIRECTION('ref_axis',(1.,0.,0.));
#139001=DIRECTION('center_axis',(0.,0.,-1.));
#139002=DIRECTION('ref_axis',(-1.,0.,0.));
#139003=DIRECTION('center_axis',(0.950906387788118,0.309478661079813,0.));
#139004=DIRECTION('ref_axis',(-0.309478661079813,0.950906387788118,0.));
#139005=DIRECTION('center_axis',(-0.819152044288992,0.573576436351046,0.));
#139006=DIRECTION('ref_axis',(-0.573576436351046,-0.819152044288992,0.));
#139007=DIRECTION('center_axis',(-0.819152044288992,0.573576436351045,0.));
#139008=DIRECTION('ref_axis',(-0.573576436351045,-0.819152044288992,0.));
#139009=DIRECTION('center_axis',(-0.819152044288993,0.573576436351045,0.));
#139010=DIRECTION('ref_axis',(-0.573576436351045,-0.819152044288993,0.));
#139011=DIRECTION('center_axis',(0.,0.,1.));
#139012=DIRECTION('ref_axis',(1.,0.,0.));
#139013=DIRECTION('center_axis',(0.950906387788118,-0.309478661079813,0.));
#139014=DIRECTION('ref_axis',(0.309478661079813,0.950906387788118,0.));
#139015=DIRECTION('center_axis',(0.,0.,1.));
#139016=DIRECTION('ref_axis',(1.,0.,0.));
#139017=DIRECTION('center_axis',(-0.858390633711205,0.51299660813389,-6.25331394795773E-15));
#139018=DIRECTION('ref_axis',(-0.51299660813389,-0.858390633711205,-1.03337427582459E-31));
#139019=DIRECTION('center_axis',(0.819152044288993,0.573576436351045,0.));
#139020=DIRECTION('ref_axis',(-0.573576436351045,0.819152044288993,0.));
#139021=DIRECTION('center_axis',(-0.819152044288992,-0.573576436351046,
0.));
#139022=DIRECTION('ref_axis',(0.573576436351046,-0.819152044288992,0.));
#139023=DIRECTION('center_axis',(0.819152044288993,0.573576436351045,0.));
#139024=DIRECTION('ref_axis',(-0.573576436351045,0.819152044288993,0.));
#139025=DIRECTION('center_axis',(-1.,0.,0.));
#139026=DIRECTION('ref_axis',(0.,0.,1.));
#139027=DIRECTION('center_axis',(0.,0.,1.));
#139028=DIRECTION('ref_axis',(1.,0.,0.));
#139029=DIRECTION('center_axis',(0.858390633711208,0.512996608133885,0.));
#139030=DIRECTION('ref_axis',(-0.512996608133885,0.858390633711208,0.));
#139031=DIRECTION('center_axis',(-0.573576436351045,-0.819152044288993,
0.));
#139032=DIRECTION('ref_axis',(0.819152044288992,-0.573576436351045,0.));
#139033=DIRECTION('center_axis',(-0.573576436351045,-0.819152044288993,
0.));
#139034=DIRECTION('ref_axis',(0.819152044288993,-0.573576436351045,0.));
#139035=DIRECTION('center_axis',(0.,0.,1.));
#139036=DIRECTION('ref_axis',(1.,0.,0.));
#139037=DIRECTION('center_axis',(-0.51299660813389,-0.858390633711205,0.));
#139038=DIRECTION('ref_axis',(0.858390633711205,-0.51299660813389,0.));
#139039=DIRECTION('center_axis',(0.573576436351046,-0.819152044288992,0.));
#139040=DIRECTION('ref_axis',(0.819152044288992,0.573576436351046,0.));
#139041=DIRECTION('center_axis',(-0.573576436351045,0.819152044288993,0.));
#139042=DIRECTION('ref_axis',(-0.819152044288993,-0.573576436351045,0.));
#139043=DIRECTION('center_axis',(0.,-1.,0.));
#139044=DIRECTION('ref_axis',(0.,0.,-1.));
#139045=DIRECTION('center_axis',(0.,0.,1.));
#139046=DIRECTION('ref_axis',(1.,0.,0.));
#139047=DIRECTION('center_axis',(-0.51299660813389,0.858390633711205,0.));
#139048=DIRECTION('ref_axis',(-0.858390633711205,-0.51299660813389,0.));
#139049=DIRECTION('center_axis',(0.573576436351045,0.819152044288992,0.));
#139050=DIRECTION('ref_axis',(-0.819152044288992,0.573576436351045,0.));
#139051=DIRECTION('center_axis',(0.573576436351045,0.819152044288993,0.));
#139052=DIRECTION('ref_axis',(-0.819152044288993,0.573576436351045,0.));
#139053=DIRECTION('center_axis',(0.,0.,1.));
#139054=DIRECTION('ref_axis',(-1.,-1.22464679914735E-16,0.));
#139055=DIRECTION('center_axis',(0.,0.,1.));
#139056=DIRECTION('ref_axis',(1.,0.,0.));
#139057=DIRECTION('center_axis',(0.51299660813389,0.858390633711205,0.));
#139058=DIRECTION('ref_axis',(-0.858390633711205,0.51299660813389,0.));
#139059=DIRECTION('center_axis',(-0.573576436351045,0.819152044288992,0.));
#139060=DIRECTION('ref_axis',(-0.819152044288992,-0.573576436351045,0.));
#139061=DIRECTION('center_axis',(0.573576436351045,-0.819152044288993,0.));
#139062=DIRECTION('ref_axis',(0.819152044288993,0.573576436351045,0.));
#139063=DIRECTION('center_axis',(0.,1.,0.));
#139064=DIRECTION('ref_axis',(0.,0.,1.));
#139065=DIRECTION('center_axis',(0.,0.,1.));
#139066=DIRECTION('ref_axis',(1.,0.,0.));
#139067=DIRECTION('center_axis',(0.51299660813389,-0.858390633711205,0.));
#139068=DIRECTION('ref_axis',(0.858390633711205,0.51299660813389,0.));
#139069=DIRECTION('center_axis',(1.,0.,0.));
#139070=DIRECTION('ref_axis',(0.,0.,-1.));
#139071=DIRECTION('center_axis',(-1.,0.,0.));
#139072=DIRECTION('ref_axis',(0.,0.,-1.));
#139073=DIRECTION('center_axis',(-0.926843172992801,0.,-0.37544870844982));
#139074=DIRECTION('ref_axis',(-0.37544870844982,0.,0.926843172992801));
#139075=DIRECTION('center_axis',(0.926843172992801,0.,-0.37544870844982));
#139076=DIRECTION('ref_axis',(0.37544870844982,0.,0.926843172992801));
#139077=DIRECTION('center_axis',(1.,0.,0.));
#139078=DIRECTION('ref_axis',(0.,0.,-1.));
#139079=DIRECTION('center_axis',(1.,0.,0.));
#139080=DIRECTION('ref_axis',(0.,0.,-1.));
#139081=DIRECTION('center_axis',(0.573576436351045,-0.819152044288992,0.));
#139082=DIRECTION('ref_axis',(-0.57922836252423,-0.405580065784332,0.707106296313275));
#139083=DIRECTION('center_axis',(-0.573576436351042,0.819152044288994,0.));
#139084=DIRECTION('ref_axis',(-0.819152044288994,-0.573576436351042,0.));
#139085=DIRECTION('center_axis',(0.,0.,1.));
#139086=DIRECTION('ref_axis',(-0.707106781186548,0.707106781186548,0.));
#139087=DIRECTION('center_axis',(0.819152044288994,-0.573576436351042,0.));
#139088=DIRECTION('ref_axis',(0.573576436351042,0.819152044288994,0.));
#139089=DIRECTION('center_axis',(-0.819152044288992,0.573576436351046,0.));
#139090=DIRECTION('ref_axis',(0.405580057474329,0.579228350656315,0.707106310801343));
#139091=DIRECTION('center_axis',(-0.819152044288992,-0.573576436351046,
0.));
#139092=DIRECTION('ref_axis',(-0.40558006578429,0.579228362524169,0.707106296313348));
#139093=DIRECTION('center_axis',(0.573576436351045,0.819152044288993,0.));
#139094=DIRECTION('ref_axis',(0.579228271576628,-0.405580002102135,0.707106407339931));
#139095=DIRECTION('center_axis',(-0.573576436351046,0.819152044288992,0.));
#139096=DIRECTION('ref_axis',(0.579228362524086,0.405580065784232,0.70710629631345));
#139097=DIRECTION('center_axis',(0.819152044288992,-0.573576436351045,0.));
#139098=DIRECTION('ref_axis',(-0.405580057474373,-0.579228350656379,0.707106310801265));
#139099=DIRECTION('center_axis',(0.819152044288992,0.573576436351046,0.));
#139100=DIRECTION('ref_axis',(0.405580065784262,-0.579228362524129,0.707106296313398));
#139101=DIRECTION('center_axis',(-0.819152044288994,-0.573576436351042,
0.));
#139102=DIRECTION('ref_axis',(0.573576436351042,-0.819152044288994,0.));
#139103=DIRECTION('center_axis',(0.,0.,1.));
#139104=DIRECTION('ref_axis',(-0.707106781186547,-0.707106781186548,0.));
#139105=DIRECTION('center_axis',(0.573576436351042,0.819152044288994,0.));
#139106=DIRECTION('ref_axis',(-0.819152044288994,0.573576436351042,0.));
#139107=DIRECTION('center_axis',(-0.573576436351045,-0.819152044288992,
0.));
#139108=DIRECTION('ref_axis',(-0.579228350656326,0.405580057474336,0.70710631080133));
#139109=DIRECTION('center_axis',(0.932736302061011,-0.360559275040251,3.939972528463E-15));
#139110=DIRECTION('ref_axis',(0.360559275040251,0.932736302061011,-2.72809344998311E-30));
#139111=DIRECTION('center_axis',(0.,0.,1.));
#139112=DIRECTION('ref_axis',(1.,0.,0.));
#139113=DIRECTION('center_axis',(0.360559275040245,-0.932736302061013,0.));
#139114=DIRECTION('ref_axis',(0.932736302061013,0.360559275040245,0.));
#139115=DIRECTION('center_axis',(0.36055927504025,0.932736302061011,-1.9699862642315E-15));
#139116=DIRECTION('ref_axis',(-0.932736302061011,0.36055927504025,4.58218097742534E-31));
#139117=DIRECTION('center_axis',(0.,0.,1.));
#139118=DIRECTION('ref_axis',(1.,0.,0.));
#139119=DIRECTION('center_axis',(0.932736302061012,0.360559275040248,0.));
#139120=DIRECTION('ref_axis',(-0.360559275040248,0.932736302061012,0.));
#139121=DIRECTION('center_axis',(-0.932736302061006,0.360559275040262,9.03616011926949E-15));
#139122=DIRECTION('ref_axis',(-0.360559275040262,-0.932736302061006,-4.62325821272544E-30));
#139123=DIRECTION('center_axis',(0.,0.,1.));
#139124=DIRECTION('ref_axis',(1.,0.,0.));
#139125=DIRECTION('center_axis',(-0.360559275040266,0.932736302061005,0.));
#139126=DIRECTION('ref_axis',(-0.932736302061005,-0.360559275040266,0.));
#139127=DIRECTION('center_axis',(-0.524947284506131,0.698415662498183,-0.486462651050277));
#139128=DIRECTION('ref_axis',(0.477697561100747,0.714799658786074,0.510750905939197));
#139129=DIRECTION('center_axis',(0.932736302061011,0.36055927504025,0.));
#139130=DIRECTION('ref_axis',(-0.36055927504025,0.932736302061011,0.));
#139131=DIRECTION('center_axis',(0.,0.,1.));
#139132=DIRECTION('ref_axis',(1.,0.,0.));
#139133=DIRECTION('center_axis',(0.36055927504025,0.932736302061011,-6.37023448850799E-15));
#139134=DIRECTION('ref_axis',(-0.932736302061011,0.36055927504025,-9.63555131444101E-31));
#139135=DIRECTION('center_axis',(0.,-0.1229930844099,0.992407527776437));
#139136=DIRECTION('ref_axis',(0.,-0.992407527776437,-0.1229930844099));
#139137=DIRECTION('center_axis',(0.,0.,1.));
#139138=DIRECTION('ref_axis',(1.,0.,0.));
#139139=DIRECTION('center_axis',(0.,0.,1.));
#139140=DIRECTION('ref_axis',(-0.753587189137082,-0.65734796597272,0.));
#139141=DIRECTION('center_axis',(0.,-0.122993084409903,0.992407527776437));
#139142=DIRECTION('ref_axis',(0.,-0.992407527776436,-0.122993084409903));
#139143=DIRECTION('center_axis',(0.,0.,1.));
#139144=DIRECTION('ref_axis',(1.,0.,0.));
#139145=DIRECTION('center_axis',(0.,0.,1.));
#139146=DIRECTION('ref_axis',(1.,0.,0.));
#139147=DIRECTION('center_axis',(0.29613474068235,0.955146174865919,-1.60736624536386E-14));
#139148=DIRECTION('ref_axis',(-0.955146174865919,0.29613474068235,-1.70032019875616E-29));
#139149=DIRECTION('center_axis',(0.,1.,0.));
#139150=DIRECTION('ref_axis',(1.,0.,0.));
#139151=DIRECTION('center_axis',(-0.296134740682398,0.955146174865905,0.));
#139152=DIRECTION('ref_axis',(-0.955146174865904,-0.296134740682398,0.));
#139153=DIRECTION('center_axis',(0.,1.,0.));
#139154=DIRECTION('ref_axis',(1.,0.,0.));
#139155=DIRECTION('center_axis',(0.14289314960746,0.192051979157228,0.970926148116865));
#139156=DIRECTION('ref_axis',(-1.42059255304153E-13,0.980992979553962,-0.194043227312473));
#139157=DIRECTION('center_axis',(0.134462341405205,-0.839995008085521,0.525669349625063));
#139158=DIRECTION('ref_axis',(-1.06456783153248E-16,-0.530486857586963,
-0.847693160245799));
#139159=DIRECTION('center_axis',(0.120848057364438,-0.6566208576434,0.744476189235685));
#139160=DIRECTION('ref_axis',(-7.75623579529732E-17,-0.749972726964935,
-0.661468751195987));
#139161=DIRECTION('center_axis',(-0.839995008085506,0.13446234140521,0.525669349625084));
#139162=DIRECTION('ref_axis',(0.530486857586985,7.38424576160362E-17,0.847693160245785));
#139163=DIRECTION('center_axis',(-0.656620857643591,0.120848057364596,0.744476189235491));
#139164=DIRECTION('ref_axis',(0.749972726964755,5.96486641503031E-17,0.661468751196192));
#139165=DIRECTION('center_axis',(0.839995008085611,0.134462341405169,0.525669349624927));
#139166=DIRECTION('ref_axis',(0.530486857586823,-1.49812135928454E-16,-0.847693160245886));
#139167=DIRECTION('center_axis',(0.65662085764469,0.120848057364753,0.744476189234497));
#139168=DIRECTION('ref_axis',(0.749972726963767,6.2356189333396E-17,-0.661468751197311));
#139169=DIRECTION('center_axis',(-0.134462341405213,-0.839995008085543,
0.525669349625026));
#139170=DIRECTION('ref_axis',(-1.21569156643707E-16,-0.530486857586926,
-0.847693160245822));
#139171=DIRECTION('center_axis',(-0.120848057364571,-0.656620857643531,
0.744476189235548));
#139172=DIRECTION('ref_axis',(3.55024582468309E-17,-0.74997272696481,-0.661468751196129));
#139173=DIRECTION('center_axis',(-0.134462341405157,0.839995008085507,0.525669349625097));
#139174=DIRECTION('ref_axis',(6.43633176795525E-17,-0.530486857586994,0.847693160245779));
#139175=DIRECTION('center_axis',(-0.120848057364642,0.656620857644208,0.744476189234939));
#139176=DIRECTION('ref_axis',(-5.23473322259609E-17,-0.749972726964203,
0.661468751196817));
#139177=DIRECTION('center_axis',(0.839995008085624,-0.134462341405244,0.525669349624888));
#139178=DIRECTION('ref_axis',(0.530486857586789,-2.55916400237815E-17,-0.847693160245908));
#139179=DIRECTION('center_axis',(0.656620857643605,-0.120848057364609,0.744476189235477));
#139180=DIRECTION('ref_axis',(0.749972726964742,-6.28921792063169E-17,-0.661468751196207));
#139181=DIRECTION('center_axis',(0.65662085764265,0.120848057364237,-0.744476189236379));
#139182=DIRECTION('ref_axis',(-0.749972726965616,-9.44663393319256E-17,
-0.661468751195215));
#139183=DIRECTION('center_axis',(0.839995008085555,0.134462341405231,-0.525669349625));
#139184=DIRECTION('ref_axis',(-0.530486857586902,2.38349706059343E-16,-0.847693160245837));
#139185=DIRECTION('center_axis',(0.134462341405206,0.839995008085575,0.525669349624976));
#139186=DIRECTION('ref_axis',(1.44832680552187E-16,-0.530486857586875,0.847693160245854));
#139187=DIRECTION('center_axis',(0.12084805736459,0.656620857643582,0.7444761892355));
#139188=DIRECTION('ref_axis',(-8.18770910965257E-17,-0.749972726964763,
0.661468751196182));
#139189=DIRECTION('center_axis',(1.09273919746571E-14,1.,0.));
#139190=DIRECTION('ref_axis',(-1.,1.09273919746571E-14,0.));
#139191=DIRECTION('center_axis',(0.,-1.,0.));
#139192=DIRECTION('ref_axis',(0.,0.,-1.));
#139193=DIRECTION('center_axis',(0.,1.,0.));
#139194=DIRECTION('ref_axis',(0.,0.,1.));
#139195=DIRECTION('center_axis',(0.,0.,1.));
#139196=DIRECTION('ref_axis',(1.,0.,0.));
#139197=DIRECTION('center_axis',(0.,1.,0.));
#139198=DIRECTION('ref_axis',(0.,0.,1.));
#139199=DIRECTION('center_axis',(-1.,0.,0.));
#139200=DIRECTION('ref_axis',(0.,1.,0.));
#139201=DIRECTION('center_axis',(0.,0.,1.));
#139202=DIRECTION('ref_axis',(0.,-1.,0.));
#139203=DIRECTION('center_axis',(0.0871557427476584,-0.996194698091746,
0.));
#139204=DIRECTION('ref_axis',(0.996194698091746,0.0871557427476567,0.));
#139205=DIRECTION('center_axis',(0.0871557427476584,-0.996194698091746,
0.));
#139206=DIRECTION('ref_axis',(0.996194698091746,0.0871557427476584,0.));
#139207=DIRECTION('center_axis',(0.,0.,-1.));
#139208=DIRECTION('ref_axis',(-0.996194698091746,-0.0871557427476585,0.));
#139209=DIRECTION('center_axis',(-0.0871557427476584,0.996194698091746,
0.));
#139210=DIRECTION('ref_axis',(0.996194698091745,0.0871557427476584,0.));
#139211=DIRECTION('center_axis',(0.0871557427476584,-0.996194698091746,
0.));
#139212=DIRECTION('ref_axis',(0.996194698091746,0.0871557427476584,0.));
#139213=DIRECTION('center_axis',(-0.0871557427476584,0.996194698091746,
1.2273002111418E-17));
#139214=DIRECTION('ref_axis',(-0.996194698091746,-0.0871557427476567,0.));
#139215=DIRECTION('center_axis',(-0.0871557427476584,0.996194698091746,
1.2273002111418E-17));
#139216=DIRECTION('ref_axis',(-0.996194698091746,-0.0871557427476584,-1.17790383141732E-32));
#139217=DIRECTION('center_axis',(-1.06966261476422E-18,1.22262996330634E-17,
-1.));
#139218=DIRECTION('ref_axis',(0.996194698091746,0.0871557427476585,0.));
#139219=DIRECTION('center_axis',(0.0871557427476584,-0.996194698091746,
-1.2273002111418E-17));
#139220=DIRECTION('ref_axis',(-0.996194698091746,-0.0871557427476584,3.71474908964093E-32));
#139221=DIRECTION('center_axis',(-0.0871557427476584,0.996194698091746,
1.2273002111418E-17));
#139222=DIRECTION('ref_axis',(-0.996194698091746,-0.0871557427476584,-1.17790383141732E-32));
#139223=DIRECTION('center_axis',(-0.990322420104686,-0.0881064801885017,
0.107232235763274));
#139224=DIRECTION('ref_axis',(0.107650883357545,-1.2725694566787E-17,0.994188758391655));
#139225=DIRECTION('center_axis',(0.087146257713358,-0.996105346075413,0.0134040772356536));
#139226=DIRECTION('ref_axis',(-0.00117066129865813,0.0133528590446799,0.999910161318234));
#139227=DIRECTION('center_axis',(0.990557289919919,0.0851973867025048,-0.107413503273888));
#139228=DIRECTION('ref_axis',(-0.107805473979535,-3.10296312186364E-18,
-0.994172007139634));
#139229=DIRECTION('center_axis',(-4.73068525233381E-16,6.98056821064309E-15,
-1.));
#139230=DIRECTION('ref_axis',(-0.0871557427476583,0.996194698091746,6.99523567979768E-15));
#139231=DIRECTION('center_axis',(-0.0871557427476584,0.996194698091746,
1.2273002111418E-17));
#139232=DIRECTION('ref_axis',(1.06966261476422E-18,-1.22262996330634E-17,
1.));
#139233=DIRECTION('center_axis',(0.0871557427476584,-0.996194698091746,
-1.2273002111418E-17));
#139234=DIRECTION('ref_axis',(-1.06966261476422E-18,1.22262996330634E-17,
-1.));
#139235=DIRECTION('',(0.0871557427476584,-0.996194698091746,-1.2273002111418E-17));
#139236=DIRECTION('center_axis',(-0.0869877574560655,0.996034814013987,
0.0186488424543453));
#139237=DIRECTION('ref_axis',(-0.109438987085954,0.00905210098230124,-0.993952296427453));
#139238=DIRECTION('center_axis',(0.0871557427476584,-0.996194698091746,
-1.2273002111418E-17));
#139239=DIRECTION('ref_axis',(-1.06966261476421E-18,1.22262996330634E-17,
-1.));
#139240=DIRECTION('',(-0.0871557427476584,0.996194698091746,1.2273002111418E-17));
#139241=DIRECTION('center_axis',(-0.0871557427476583,0.996194698091746,
0.));
#139242=DIRECTION('ref_axis',(0.996194698091745,0.08715574274766,0.));
#139243=DIRECTION('center_axis',(1.75242621800742E-16,3.01185978847313E-18,
1.));
#139244=DIRECTION('ref_axis',(-0.996194698091746,-0.0871557427476572,1.74838271594512E-16));
#139245=DIRECTION('center_axis',(-0.0871557427476584,0.996194698091746,
1.2273002111418E-17));
#139246=DIRECTION('ref_axis',(5.35850844502666E-19,-1.2273002111418E-17,
1.));
#139247=DIRECTION('center_axis',(-4.73068525233381E-16,6.98056821064309E-15,
-1.));
#139248=DIRECTION('ref_axis',(0.,1.,6.98056225145764E-15));
#139249=DIRECTION('center_axis',(-4.73068525233381E-16,6.98056821064309E-15,
-1.));
#139250=DIRECTION('ref_axis',(-1.72250008496352E-34,1.,6.98056821064309E-15));
#139251=DIRECTION('center_axis',(-1.,1.22464679914732E-16,4.73068525233382E-16));
#139252=DIRECTION('ref_axis',(-1.22464679914735E-16,-1.,-6.98139884808413E-15));
#139253=DIRECTION('center_axis',(4.73068525233381E-16,-6.98056821064309E-15,
1.));
#139254=DIRECTION('ref_axis',(-3.49817812003891E-35,1.,6.98056821064309E-15));
#139255=DIRECTION('center_axis',(-4.73068525233381E-16,6.98056821064309E-15,
-1.));
#139256=DIRECTION('ref_axis',(-1.72250008496352E-34,1.,6.98056821064309E-15));
#139257=DIRECTION('center_axis',(-4.73068525233381E-16,6.98056821064309E-15,
-1.));
#139258=DIRECTION('ref_axis',(0.,1.,6.98058702583013E-15));
#139259=DIRECTION('center_axis',(-4.73068525233381E-16,6.98056821064309E-15,
-1.));
#139260=DIRECTION('ref_axis',(1.01760986150651E-34,1.,6.98056821064309E-15));
#139261=DIRECTION('center_axis',(-1.,1.22464679914732E-16,4.73068525233382E-16));
#139262=DIRECTION('ref_axis',(-1.22464679914735E-16,-1.,-6.98058702583013E-15));
#139263=DIRECTION('center_axis',(4.73068525233381E-16,-6.98056821064309E-15,
1.));
#139264=DIRECTION('ref_axis',(2.37981304966787E-34,1.,6.98056821064309E-15));
#139265=DIRECTION('center_axis',(4.73068525233381E-16,-6.98056821064309E-15,
1.));
#139266=DIRECTION('ref_axis',(2.37981304966787E-34,1.,6.98056821064309E-15));
#139267=DIRECTION('center_axis',(-0.0871557427476584,0.996194698091746,
1.2273002111418E-17));
#139268=DIRECTION('ref_axis',(1.06966261476422E-18,-1.22262996330634E-17,
1.));
#139269=DIRECTION('',(-0.0871557427476584,0.996194698091746,1.2273002111418E-17));
#139270=DIRECTION('center_axis',(-4.73068525233381E-16,6.98056821064309E-15,
-1.));
#139271=DIRECTION('ref_axis',(-0.0871557427476584,0.996194698091745,6.99523567979768E-15));
#139272=DIRECTION('center_axis',(-4.73068525233381E-16,6.98056821064309E-15,
-1.));
#139273=DIRECTION('ref_axis',(-0.0871557427476584,0.996194698091745,6.99523567979768E-15));
#139274=DIRECTION('',(-4.73068525233381E-16,6.98056821064309E-15,-1.));
#139275=DIRECTION('center_axis',(-4.73068525233381E-16,6.98056821064309E-15,
-1.));
#139276=DIRECTION('ref_axis',(-0.0871557427476584,0.996194698091745,6.99523567979768E-15));
#139277=DIRECTION('',(4.73068525233381E-16,-6.98056821064309E-15,1.));
#139278=DIRECTION('center_axis',(-4.73068525233381E-16,6.98056821064309E-15,
-1.));
#139279=DIRECTION('ref_axis',(-0.996194698091745,-0.0871557427476584,-1.37128250527716E-16));
#139280=DIRECTION('center_axis',(-4.73068525233381E-16,6.98056821064309E-15,
-1.));
#139281=DIRECTION('ref_axis',(-0.0871557427476584,0.996194698091746,6.99523567979768E-15));
#139282=DIRECTION('center_axis',(-4.73068525233381E-16,6.98056821064309E-15,
-1.));
#139283=DIRECTION('ref_axis',(-0.0871557427476584,0.996194698091746,6.99523567979768E-15));
#139284=DIRECTION('center_axis',(1.4081690688991E-16,0.,1.));
#139285=DIRECTION('ref_axis',(1.,0.,-1.25828382064365E-16));
#139286=DIRECTION('center_axis',(1.4081690688991E-16,0.,1.));
#139287=DIRECTION('ref_axis',(1.,0.,-1.4081690688991E-16));
#139288=DIRECTION('center_axis',(-1.22464679914735E-16,1.,1.7245097428856E-32));
#139289=DIRECTION('ref_axis',(-1.,-1.22464679914735E-16,1.57285477580457E-16));
#139290=DIRECTION('center_axis',(-1.4081690688991E-16,0.,-1.));
#139291=DIRECTION('ref_axis',(1.,0.,-1.4081690688991E-16));
#139292=DIRECTION('center_axis',(0.,0.,1.));
#139293=DIRECTION('ref_axis',(1.,0.,0.));
#139294=DIRECTION('center_axis',(0.,0.,1.));
#139295=DIRECTION('ref_axis',(1.,0.,0.));
#139296=DIRECTION('center_axis',(1.22464679914735E-16,-1.,0.));
#139297=DIRECTION('ref_axis',(-1.,-1.22464679914735E-16,0.));
#139298=DIRECTION('center_axis',(0.,0.,-1.));
#139299=DIRECTION('ref_axis',(1.,0.,0.));
#139300=DIRECTION('center_axis',(0.,0.,-1.));
#139301=DIRECTION('ref_axis',(1.,0.,0.));
#139302=DIRECTION('center_axis',(0.,0.,1.));
#139303=DIRECTION('ref_axis',(1.,0.,0.));
#139304=DIRECTION('center_axis',(0.,0.,1.));
#139305=DIRECTION('ref_axis',(1.,0.,0.));
#139306=DIRECTION('center_axis',(0.,0.,1.));
#139307=DIRECTION('ref_axis',(1.,0.,0.));
#139308=DIRECTION('center_axis',(1.22464679914735E-16,-1.,0.));
#139309=DIRECTION('ref_axis',(-1.,-1.22464679914735E-16,0.));
#139310=DIRECTION('center_axis',(0.,0.,-1.));
#139311=DIRECTION('ref_axis',(1.,0.,0.));
#139312=DIRECTION('center_axis',(1.4081690688991E-16,0.,1.));
#139313=DIRECTION('ref_axis',(1.,0.,-1.24674611521858E-16));
#139314=DIRECTION('center_axis',(1.4081690688991E-16,0.,1.));
#139315=DIRECTION('ref_axis',(-1.,0.,1.4081690688991E-16));
#139316=DIRECTION('center_axis',(1.22464679914735E-16,-1.,-1.7245097428856E-32));
#139317=DIRECTION('ref_axis',(-1.,-1.22464679914735E-16,1.55843264402323E-16));
#139318=DIRECTION('center_axis',(-1.4081690688991E-16,0.,-1.));
#139319=DIRECTION('ref_axis',(1.,0.,-1.4081690688991E-16));
#139320=DIRECTION('center_axis',(1.4081690688991E-16,0.,1.));
#139321=DIRECTION('ref_axis',(1.,0.,-1.23223868360489E-16));
#139322=DIRECTION('center_axis',(1.4081690688991E-16,0.,1.));
#139323=DIRECTION('ref_axis',(1.,0.,-1.4081690688991E-16));
#139324=DIRECTION('center_axis',(1.22464679914735E-16,-1.,-1.7245097428856E-32));
#139325=DIRECTION('ref_axis',(-1.,-1.22464679914735E-16,1.54029835450611E-16));
#139326=DIRECTION('center_axis',(-1.4081690688991E-16,0.,-1.));
#139327=DIRECTION('ref_axis',(-1.,0.,1.4081690688991E-16));
#139328=DIRECTION('center_axis',(1.4081690688991E-16,0.,1.));
#139329=DIRECTION('ref_axis',(1.,0.,-1.4081690688991E-16));
#139330=DIRECTION('center_axis',(1.4081690688991E-16,0.,1.));
#139331=DIRECTION('ref_axis',(1.,0.,-1.4081690688991E-16));
#139332=DIRECTION('',(-1.40816906889911E-16,0.,-1.));
#139333=DIRECTION('center_axis',(1.4081690688991E-16,0.,1.));
#139334=DIRECTION('ref_axis',(1.,0.,-1.4081690688991E-16));
#139335=DIRECTION('center_axis',(1.4081690688991E-16,0.,1.));
#139336=DIRECTION('ref_axis',(1.,0.,-1.4081690688991E-16));
#139337=DIRECTION('',(-0.5299192642332,-6.48963930749709E-17,0.848048096156429));
#139338=DIRECTION('center_axis',(1.4081690688991E-16,0.,1.));
#139339=DIRECTION('ref_axis',(1.,0.,-1.4081690688991E-16));
#139340=DIRECTION('',(0.529919264233204,6.48963930749714E-17,-0.848048096156427));
#139341=DIRECTION('center_axis',(0.,0.,-1.));
#139342=DIRECTION('ref_axis',(-1.,0.,0.));
#139343=DIRECTION('center_axis',(1.4081690688991E-16,0.,1.));
#139344=DIRECTION('ref_axis',(1.,0.,-1.4081690688991E-16));
#139345=DIRECTION('',(0.,0.,1.));
#139346=DIRECTION('center_axis',(0.,0.,-1.));
#139347=DIRECTION('ref_axis',(-1.,0.,0.));
#139348=DIRECTION('',(0.,0.,-1.));
#139349=DIRECTION('center_axis',(0.,0.,-1.));
#139350=DIRECTION('ref_axis',(-1.,0.,0.));
#139351=DIRECTION('center_axis',(0.,0.,-1.));
#139352=DIRECTION('ref_axis',(-1.,0.,0.));
#139353=DIRECTION('center_axis',(0.,0.,-1.));
#139354=DIRECTION('ref_axis',(-1.,0.,0.));
#139355=DIRECTION('',(0.,0.,1.));
#139356=DIRECTION('center_axis',(0.,0.,-1.));
#139357=DIRECTION('ref_axis',(1.,0.,0.));
#139358=DIRECTION('center_axis',(0.,0.,1.));
#139359=DIRECTION('ref_axis',(1.,0.,0.));
#139360=DIRECTION('center_axis',(0.,0.,-1.));
#139361=DIRECTION('ref_axis',(-1.,0.,0.));
#139362=DIRECTION('center_axis',(0.,0.,1.));
#139363=DIRECTION('ref_axis',(1.,0.,0.));
#139364=DIRECTION('center_axis',(1.4081690688991E-16,0.,1.));
#139365=DIRECTION('ref_axis',(1.,0.,-1.40816906889911E-16));
#139366=DIRECTION('center_axis',(1.4081690688991E-16,0.,1.));
#139367=DIRECTION('ref_axis',(1.,0.,-1.40816906889911E-16));
#139368=DIRECTION('center_axis',(1.,-1.90843891001168E-31,-2.61618113230267E-16));
#139369=DIRECTION('ref_axis',(0.,1.,0.));
#139370=DIRECTION('',(1.,-1.90843891001168E-31,-2.61618113230267E-16));
#139371=DIRECTION('center_axis',(-1.,3.57620498399058E-12,-7.43666695244082E-12));
#139372=DIRECTION('ref_axis',(8.25152405459824E-12,0.441542383644494,-0.897240393342575));
#139373=DIRECTION('center_axis',(1.,-1.90843891001168E-31,-2.61618113230267E-16));
#139374=DIRECTION('ref_axis',(0.,1.,0.));
#139375=DIRECTION('',(1.,-1.90843891001168E-31,-2.61618113230267E-16));
#139376=DIRECTION('center_axis',(1.,-1.90843891001168E-31,-2.61618113230267E-16));
#139377=DIRECTION('ref_axis',(0.,1.,0.));
#139378=DIRECTION('',(1.,-1.90843891001168E-31,-2.61618113230267E-16));
#139379=DIRECTION('center_axis',(1.,-1.90843891001168E-31,-2.61618113230267E-16));
#139380=DIRECTION('ref_axis',(0.,1.,0.));
#139381=DIRECTION('',(1.,-1.90843891001168E-31,-2.61618113230267E-16));
#139382=DIRECTION('center_axis',(1.,-1.90843891001168E-31,-2.61618113230267E-16));
#139383=DIRECTION('ref_axis',(0.,1.,0.));
#139384=DIRECTION('',(1.,-1.90843891001168E-31,-2.61618113230267E-16));
#139385=DIRECTION('center_axis',(1.,-1.90843891001168E-31,-2.61618113230267E-16));
#139386=DIRECTION('ref_axis',(0.,1.,0.));
#139387=DIRECTION('',(1.,-1.90843891001168E-31,-2.61618113230267E-16));
#139388=DIRECTION('center_axis',(1.,-3.49148133884313E-15,0.));
#139389=DIRECTION('ref_axis',(0.,0.,1.));
#139390=DIRECTION('',(-1.,3.49148133884313E-15,0.));
#139391=DIRECTION('center_axis',(1.,-3.49148133884313E-15,0.));
#139392=DIRECTION('ref_axis',(0.,0.,1.));
#139393=DIRECTION('center_axis',(1.,-3.49148133884313E-15,0.));
#139394=DIRECTION('ref_axis',(0.,0.,1.));
#139395=DIRECTION('',(-1.,3.49148133884313E-15,0.));
#139396=DIRECTION('center_axis',(1.,-3.49148133884313E-15,0.));
#139397=DIRECTION('ref_axis',(0.,0.,1.));
#139398=DIRECTION('center_axis',(1.,-3.49148133884313E-15,0.));
#139399=DIRECTION('ref_axis',(0.,0.,1.));
#139400=DIRECTION('',(-1.,3.49148133884313E-15,0.));
#139401=DIRECTION('center_axis',(1.,-3.49148133884313E-15,0.));
#139402=DIRECTION('ref_axis',(0.,0.,1.));
#139403=DIRECTION('',(-1.,3.49148133884313E-15,0.));
#139404=DIRECTION('center_axis',(1.,-3.49148133884313E-15,0.));
#139405=DIRECTION('ref_axis',(0.,0.,1.));
#139406=DIRECTION('',(-1.,3.49148133884313E-15,0.));
#139407=DIRECTION('center_axis',(1.,-3.49148133884313E-15,0.));
#139408=DIRECTION('ref_axis',(0.,0.,1.));
#139409=DIRECTION('',(-1.,3.49148133884313E-15,0.));
#139410=DIRECTION('center_axis',(1.,-3.49148133884313E-15,0.));
#139411=DIRECTION('ref_axis',(0.,0.,1.));
#139412=DIRECTION('',(-1.,3.49148133884313E-15,0.));
#139413=DIRECTION('center_axis',(1.,-3.49148133884313E-15,0.));
#139414=DIRECTION('ref_axis',(0.,0.,1.));
#139415=DIRECTION('',(-1.,3.49148133884313E-15,0.));
#139416=DIRECTION('center_axis',(-1.,3.49148133884313E-15,0.));
#139417=DIRECTION('ref_axis',(0.,0.,1.));
#139418=DIRECTION('center_axis',(1.,-3.49148133884313E-15,0.));
#139419=DIRECTION('ref_axis',(0.,0.,1.));
#139420=DIRECTION('center_axis',(0.999733823610252,-0.00785201424948982,
0.0216939577268001));
#139421=DIRECTION('ref_axis',(0.000790766294128704,-0.928088776890918,-0.37235815674937));
#139422=DIRECTION('center_axis',(1.,7.68190179945482E-12,1.14262706414629E-12));
#139423=DIRECTION('ref_axis',(-4.47582277062776E-14,-0.141421341569384,
0.989949495756584));
#139424=DIRECTION('center_axis',(-0.99643212438083,0.0191622394024502,-0.0821938567229316));
#139425=DIRECTION('ref_axis',(-0.015721416758303,-0.998980952014553,-0.0423071455809782));
#139426=DIRECTION('',(-0.707106781186546,2.38225452545871E-15,0.707106781186549));
#139427=DIRECTION('center_axis',(-1.,3.49148133884313E-15,0.));
#139428=DIRECTION('ref_axis',(0.,0.,1.));
#139429=DIRECTION('center_axis',(-1.,3.49148133884313E-15,0.));
#139430=DIRECTION('ref_axis',(0.,0.,-1.));
#139431=DIRECTION('center_axis',(-1.,3.49148133884313E-15,0.));
#139432=DIRECTION('ref_axis',(0.,0.,1.));
#139433=DIRECTION('center_axis',(-0.999731535326071,-0.0209809681761542,
-0.00983139099868423));
#139434=DIRECTION('ref_axis',(-0.00512812960574839,-0.213430275538391,0.976944839676403));
#139435=DIRECTION('center_axis',(0.996321406376314,0.0724020542568729,0.0458431863607806));
#139436=DIRECTION('ref_axis',(-0.000636379506200249,-0.528690912836352,
0.848814180904978));
#139437=DIRECTION('center_axis',(-1.,3.49148133884313E-15,0.));
#139438=DIRECTION('ref_axis',(0.,0.,1.));
#139439=DIRECTION('',(0.707106781186545,-2.55544573670581E-15,-0.70710678118655));
#139440=DIRECTION('center_axis',(1.,-3.49148133884313E-15,0.));
#139441=DIRECTION('ref_axis',(0.,0.,1.));
#139442=DIRECTION('center_axis',(1.,-3.49148133884313E-15,0.));
#139443=DIRECTION('ref_axis',(0.,0.,1.));
#139444=DIRECTION('center_axis',(1.,-3.49148133884313E-15,0.));
#139445=DIRECTION('ref_axis',(0.,0.,1.));
#139446=DIRECTION('center_axis',(1.,-3.49148133884313E-15,0.));
#139447=DIRECTION('ref_axis',(0.,0.,1.));
#139448=DIRECTION('center_axis',(1.,-3.49148133884313E-15,0.));
#139449=DIRECTION('ref_axis',(0.,0.,1.));
#139450=DIRECTION('center_axis',(1.,-3.49148133884313E-15,0.));
#139451=DIRECTION('ref_axis',(0.,0.,1.));
#139452=DIRECTION('center_axis',(1.,-3.49148133884313E-15,0.));
#139453=DIRECTION('ref_axis',(0.,0.,1.));
#139454=DIRECTION('center_axis',(1.,-3.49148133884313E-15,0.));
#139455=DIRECTION('ref_axis',(0.,0.,1.));
#139456=DIRECTION('center_axis',(1.,-3.49148133884313E-15,0.));
#139457=DIRECTION('ref_axis',(0.,0.,1.));
#139458=DIRECTION('center_axis',(1.,-3.49148133884313E-15,0.));
#139459=DIRECTION('ref_axis',(0.,0.,1.));
#139460=DIRECTION('center_axis',(1.,-3.49148133884313E-15,0.));
#139461=DIRECTION('ref_axis',(0.,0.,1.));
#139462=DIRECTION('center_axis',(1.,-3.49148133884313E-15,0.));
#139463=DIRECTION('ref_axis',(0.,0.,1.));
#139464=DIRECTION('center_axis',(1.,-3.49148133884313E-15,0.));
#139465=DIRECTION('ref_axis',(0.,0.,1.));
#139466=DIRECTION('center_axis',(1.,-3.49148133884313E-15,0.));
#139467=DIRECTION('ref_axis',(0.,0.,1.));
#139468=DIRECTION('center_axis',(1.,-3.49148133884313E-15,0.));
#139469=DIRECTION('ref_axis',(0.,0.,1.));
#139470=DIRECTION('center_axis',(1.,-3.49148133884313E-15,0.));
#139471=DIRECTION('ref_axis',(0.,0.,1.));
#139472=DIRECTION('center_axis',(-1.,3.49148133884313E-15,0.));
#139473=DIRECTION('ref_axis',(0.,0.,-1.));
#139474=DIRECTION('',(-3.02371153627746E-15,-0.866025403784438,0.500000000000001));
#139475=DIRECTION('',(-3.02371153627746E-15,-0.866025403784438,-0.500000000000001));
#139476=DIRECTION('',(0.,0.,-1.));
#139477=DIRECTION('',(3.02371153627745E-15,0.866025403784437,-0.500000000000003));
#139478=DIRECTION('',(3.02371153627745E-15,0.866025403784437,0.500000000000003));
#139479=DIRECTION('',(0.,0.,1.));
#139480=DIRECTION('center_axis',(-1.74574066942157E-15,-0.500000000000001,
0.866025403784438));
#139481=DIRECTION('ref_axis',(-3.02371153627746E-15,-0.866025403784438,
-0.500000000000001));
#139482=DIRECTION('',(1.,-3.49148133884313E-15,0.));
#139483=DIRECTION('',(1.,-3.49148133884313E-15,0.));
#139484=DIRECTION('center_axis',(-3.49148133884313E-15,-1.,0.));
#139485=DIRECTION('ref_axis',(0.,0.,-1.));
#139486=DIRECTION('',(1.,-3.49148133884313E-15,0.));
#139487=DIRECTION('center_axis',(-1.74574066942158E-15,-0.500000000000003,
-0.866025403784437));
#139488=DIRECTION('ref_axis',(3.02371153627745E-15,0.866025403784437,-0.500000000000003));
#139489=DIRECTION('',(1.,-3.49148133884313E-15,0.));
#139490=DIRECTION('center_axis',(1.74574066942158E-15,0.500000000000003,
-0.866025403784437));
#139491=DIRECTION('ref_axis',(3.02371153627745E-15,0.866025403784437,0.500000000000003));
#139492=DIRECTION('',(1.,-3.49148133884313E-15,0.));
#139493=DIRECTION('center_axis',(3.49148133884313E-15,1.,0.));
#139494=DIRECTION('ref_axis',(0.,0.,1.));
#139495=DIRECTION('',(1.,-3.49148133884313E-15,0.));
#139496=DIRECTION('center_axis',(1.74574066942157E-15,0.500000000000001,
0.866025403784438));
#139497=DIRECTION('ref_axis',(-3.02371153627746E-15,-0.866025403784438,
0.500000000000001));
#139498=DIRECTION('center_axis',(1.,-1.90843891001168E-31,-2.61618113230267E-16));
#139499=DIRECTION('ref_axis',(0.,1.,0.));
#139500=DIRECTION('center_axis',(0.,1.,0.));
#139501=DIRECTION('ref_axis',(-1.,0.,0.));
#139502=DIRECTION('',(0.,1.,0.));
#139503=DIRECTION('center_axis',(-3.57620498398977E-12,-1.,-7.43666695243917E-12));
#139504=DIRECTION('ref_axis',(-0.441622759424804,8.25151731278174E-12,-0.897200835018571));
#139505=DIRECTION('center_axis',(0.,1.,0.));
#139506=DIRECTION('ref_axis',(-1.,0.,0.));
#139507=DIRECTION('',(0.,1.,0.));
#139508=DIRECTION('center_axis',(0.,1.,0.));
#139509=DIRECTION('ref_axis',(-1.,0.,0.));
#139510=DIRECTION('',(0.,1.,0.));
#139511=DIRECTION('center_axis',(0.,1.,0.));
#139512=DIRECTION('ref_axis',(-1.,0.,0.));
#139513=DIRECTION('',(0.,1.,0.));
#139514=DIRECTION('center_axis',(0.,1.,0.));
#139515=DIRECTION('ref_axis',(-1.,0.,0.));
#139516=DIRECTION('',(0.,1.,0.));
#139517=DIRECTION('center_axis',(0.,1.,0.));
#139518=DIRECTION('ref_axis',(-1.,0.,0.));
#139519=DIRECTION('',(0.,1.,0.));
#139520=DIRECTION('center_axis',(0.,1.,1.4081690688991E-16));
#139521=DIRECTION('ref_axis',(1.40816906889911E-16,-1.4081690688991E-16,
1.));
#139522=DIRECTION('',(0.,-1.,-1.4081690688991E-16));
#139523=DIRECTION('center_axis',(0.,1.,1.4081690688991E-16));
#139524=DIRECTION('ref_axis',(1.40816906889911E-16,-1.4081690688991E-16,
1.));
#139525=DIRECTION('center_axis',(0.,1.,1.4081690688991E-16));
#139526=DIRECTION('ref_axis',(1.40816906889911E-16,-1.4081690688991E-16,
1.));
#139527=DIRECTION('',(0.,-1.,-1.4081690688991E-16));
#139528=DIRECTION('center_axis',(0.,1.,1.4081690688991E-16));
#139529=DIRECTION('ref_axis',(1.40816906889911E-16,-1.4081690688991E-16,
1.));
#139530=DIRECTION('center_axis',(0.,1.,1.4081690688991E-16));
#139531=DIRECTION('ref_axis',(1.40816906889911E-16,-1.4081690688991E-16,
1.));
#139532=DIRECTION('',(0.,-1.,-1.4081690688991E-16));
#139533=DIRECTION('center_axis',(0.,1.,1.4081690688991E-16));
#139534=DIRECTION('ref_axis',(1.40816906889911E-16,-1.4081690688991E-16,
1.));
#139535=DIRECTION('',(0.,-1.,-1.4081690688991E-16));
#139536=DIRECTION('center_axis',(0.,1.,1.4081690688991E-16));
#139537=DIRECTION('ref_axis',(1.40816906889911E-16,-1.4081690688991E-16,
1.));
#139538=DIRECTION('',(0.,-1.,-1.4081690688991E-16));
#139539=DIRECTION('center_axis',(0.,1.,1.4081690688991E-16));
#139540=DIRECTION('ref_axis',(1.40816906889911E-16,-1.4081690688991E-16,
1.));
#139541=DIRECTION('',(0.,-1.,-1.4081690688991E-16));
#139542=DIRECTION('center_axis',(0.,1.,1.4081690688991E-16));
#139543=DIRECTION('ref_axis',(1.40816906889911E-16,-1.4081690688991E-16,
1.));
#139544=DIRECTION('',(0.,-1.,-1.4081690688991E-16));
#139545=DIRECTION('center_axis',(0.,1.,1.4081690688991E-16));
#139546=DIRECTION('ref_axis',(1.40816906889911E-16,-1.4081690688991E-16,
1.));
#139547=DIRECTION('',(0.,-1.,-1.4081690688991E-16));
#139548=DIRECTION('center_axis',(0.,-1.,-1.4081690688991E-16));
#139549=DIRECTION('ref_axis',(-7.47361512810214E-16,-1.4081690688991E-16,
1.));
#139550=DIRECTION('center_axis',(0.,1.,1.4081690688991E-16));
#139551=DIRECTION('ref_axis',(1.40816906889911E-16,-1.4081690688991E-16,
1.));
#139552=DIRECTION('center_axis',(0.00785201424984197,0.999733823610251,
0.0216939577266995));
#139553=DIRECTION('ref_axis',(0.928088776890915,0.000790766293764068,-0.372358156749379));
#139554=DIRECTION('center_axis',(-7.68190179945114E-12,1.,1.1426270641458E-12));
#139555=DIRECTION('ref_axis',(0.141219054307676,-4.63451743285696E-14,0.989978372844804));
#139556=DIRECTION('center_axis',(-0.0191622393999958,-0.996432124380861,
-0.0821938567231223));
#139557=DIRECTION('ref_axis',(0.998980952014602,-0.0157214167558561,-0.0423071455807097));
#139558=DIRECTION('',(1.8616819539112E-16,-0.707106781186547,0.707106781186548));
#139559=DIRECTION('center_axis',(0.,-1.,-1.4081690688991E-16));
#139560=DIRECTION('ref_axis',(1.40816906889911E-16,-1.4081690688991E-16,
1.));
#139561=DIRECTION('center_axis',(0.,-1.,-1.4081690688991E-16));
#139562=DIRECTION('ref_axis',(-1.40816906889911E-16,1.40816906889911E-16,
-1.));
#139563=DIRECTION('center_axis',(0.,-1.,-1.4081690688991E-16));
#139564=DIRECTION('ref_axis',(-7.47361512810214E-16,-1.4081690688991E-16,
1.));
#139565=DIRECTION('center_axis',(0.0209809681760068,-0.99973153532607,-0.0098313909991016));
#139566=DIRECTION('ref_axis',(0.213430275538422,-0.00512812960618709,0.976944839676394));
#139567=DIRECTION('center_axis',(-0.0724020542557579,0.996321406376306,
0.0458431863627102));
#139568=DIRECTION('ref_axis',(0.528690912836516,-0.000636379508420693,0.848814180904875));
#139569=DIRECTION('center_axis',(0.,-1.,-1.4081690688991E-16));
#139570=DIRECTION('ref_axis',(-7.47361512810214E-16,-1.4081690688991E-16,
1.));
#139571=DIRECTION('',(-1.29769841440215E-17,0.707106781186545,-0.70710678118655));
#139572=DIRECTION('center_axis',(0.,1.,1.4081690688991E-16));
#139573=DIRECTION('ref_axis',(1.40816906889911E-16,-1.40816906889911E-16,
1.));
#139574=DIRECTION('center_axis',(0.,1.,1.4081690688991E-16));
#139575=DIRECTION('ref_axis',(1.40816906889911E-16,-1.4081690688991E-16,
1.));
#139576=DIRECTION('center_axis',(0.,1.,1.4081690688991E-16));
#139577=DIRECTION('ref_axis',(1.40816906889911E-16,-1.40816906889911E-16,
1.));
#139578=DIRECTION('center_axis',(0.,1.,1.4081690688991E-16));
#139579=DIRECTION('ref_axis',(1.40816906889911E-16,-1.40816906889911E-16,
1.));
#139580=DIRECTION('center_axis',(0.,1.,1.4081690688991E-16));
#139581=DIRECTION('ref_axis',(1.40816906889911E-16,-1.4081690688991E-16,
1.));
#139582=DIRECTION('center_axis',(0.,1.,1.4081690688991E-16));
#139583=DIRECTION('ref_axis',(1.40816906889911E-16,-1.4081690688991E-16,
1.));
#139584=DIRECTION('center_axis',(0.,1.,1.4081690688991E-16));
#139585=DIRECTION('ref_axis',(1.40816906889911E-16,-1.4081690688991E-16,
1.));
#139586=DIRECTION('center_axis',(0.,1.,1.4081690688991E-16));
#139587=DIRECTION('ref_axis',(1.40816906889911E-16,-1.4081690688991E-16,
1.));
#139588=DIRECTION('center_axis',(0.,1.,1.4081690688991E-16));
#139589=DIRECTION('ref_axis',(1.40816906889911E-16,-1.4081690688991E-16,
1.));
#139590=DIRECTION('center_axis',(0.,1.,1.4081690688991E-16));
#139591=DIRECTION('ref_axis',(1.40816906889911E-16,-1.4081690688991E-16,
1.));
#139592=DIRECTION('center_axis',(0.,1.,1.4081690688991E-16));
#139593=DIRECTION('ref_axis',(1.40816906889911E-16,-1.4081690688991E-16,
1.));
#139594=DIRECTION('center_axis',(0.,1.,1.4081690688991E-16));
#139595=DIRECTION('ref_axis',(1.40816906889911E-16,-1.4081690688991E-16,
1.));
#139596=DIRECTION('center_axis',(0.,1.,1.4081690688991E-16));
#139597=DIRECTION('ref_axis',(1.40816906889911E-16,-1.4081690688991E-16,
1.));
#139598=DIRECTION('center_axis',(0.,1.,1.4081690688991E-16));
#139599=DIRECTION('ref_axis',(1.40816906889911E-16,-1.4081690688991E-16,
1.));
#139600=DIRECTION('center_axis',(0.,1.,1.4081690688991E-16));
#139601=DIRECTION('ref_axis',(1.40816906889911E-16,-1.4081690688991E-16,
1.));
#139602=DIRECTION('center_axis',(0.,1.,1.4081690688991E-16));
#139603=DIRECTION('ref_axis',(1.40816906889911E-16,-1.4081690688991E-16,
1.));
#139604=DIRECTION('center_axis',(0.,-1.,-1.4081690688991E-16));
#139605=DIRECTION('ref_axis',(-1.40816906889911E-16,1.40816906889911E-16,
-1.));
#139606=DIRECTION('',(0.866025403784438,-7.04084534449553E-17,0.500000000000001));
#139607=DIRECTION('',(0.866025403784438,7.04084534449553E-17,-0.500000000000001));
#139608=DIRECTION('',(-1.40816906889911E-16,1.40816906889911E-16,-1.));
#139609=DIRECTION('',(-0.866025403784437,7.04084534449556E-17,-0.500000000000002));
#139610=DIRECTION('',(-0.866025403784437,-7.04084534449556E-17,0.500000000000003));
#139611=DIRECTION('',(1.40816906889911E-16,-1.40816906889911E-16,1.));
#139612=DIRECTION('center_axis',(0.500000000000001,-1.2195101864901E-16,
0.866025403784438));
#139613=DIRECTION('ref_axis',(0.866025403784438,7.04084534449554E-17,-0.500000000000001));
#139614=DIRECTION('',(0.,1.,1.40816906889911E-16));
#139615=DIRECTION('',(0.,1.,1.40816906889911E-16));
#139616=DIRECTION('center_axis',(1.,0.,-1.40816906889911E-16));
#139617=DIRECTION('ref_axis',(-1.40816906889911E-16,1.40816906889911E-16,
-1.));
#139618=DIRECTION('',(0.,1.,1.40816906889911E-16));
#139619=DIRECTION('center_axis',(0.500000000000002,1.2195101864901E-16,
-0.866025403784437));
#139620=DIRECTION('ref_axis',(-0.866025403784437,7.04084534449556E-17,-0.500000000000002));
#139621=DIRECTION('',(0.,1.,1.40816906889911E-16));
#139622=DIRECTION('center_axis',(-0.500000000000003,1.2195101864901E-16,
-0.866025403784437));
#139623=DIRECTION('ref_axis',(-0.866025403784437,-7.04084534449556E-17,
0.500000000000003));
#139624=DIRECTION('',(0.,1.,1.40816906889911E-16));
#139625=DIRECTION('center_axis',(-1.,0.,1.40816906889911E-16));
#139626=DIRECTION('ref_axis',(1.40816906889911E-16,-1.40816906889911E-16,
1.));
#139627=DIRECTION('',(0.,1.,1.40816906889911E-16));
#139628=DIRECTION('center_axis',(-0.500000000000001,-1.2195101864901E-16,
0.866025403784438));
#139629=DIRECTION('ref_axis',(0.866025403784438,-7.04084534449554E-17,0.500000000000001));
#139630=DIRECTION('center_axis',(0.,1.,0.));
#139631=DIRECTION('ref_axis',(-1.,0.,0.));
#139632=DIRECTION('center_axis',(0.,0.,-1.));
#139633=DIRECTION('ref_axis',(-1.,0.,0.));
#139634=DIRECTION('center_axis',(0.,0.,-1.));
#139635=DIRECTION('ref_axis',(-1.,0.,0.));
#139636=DIRECTION('',(0.642787609686534,-7.87187788734192E-17,-0.766044443118983));
#139637=DIRECTION('center_axis',(0.,0.,1.));
#139638=DIRECTION('ref_axis',(-1.,0.,0.));
#139639=DIRECTION('center_axis',(0.,0.,1.));
#139640=DIRECTION('ref_axis',(1.,0.,0.));
#139641=DIRECTION('center_axis',(0.,0.,1.));
#139642=DIRECTION('ref_axis',(1.,0.,0.));
#139643=DIRECTION('center_axis',(0.,0.,1.));
#139644=DIRECTION('ref_axis',(1.,0.,0.));
#139645=DIRECTION('',(-0.642787609686546,-7.87187788734207E-17,0.766044443118972));
#139646=DIRECTION('center_axis',(0.,0.,-1.));
#139647=DIRECTION('ref_axis',(1.,0.,0.));
#139648=DIRECTION('center_axis',(0.,0.,-1.));
#139649=DIRECTION('ref_axis',(-1.,0.,0.));
#139650=DIRECTION('center_axis',(0.,0.,-1.));
#139651=DIRECTION('ref_axis',(1.,0.,0.));
#139652=DIRECTION('',(-0.766044443118973,9.38133875270267E-17,0.642787609686545));
#139653=DIRECTION('center_axis',(0.,0.,1.));
#139654=DIRECTION('ref_axis',(1.,0.,0.));
#139655=DIRECTION('center_axis',(0.,0.,1.));
#139656=DIRECTION('ref_axis',(1.,0.,0.));
#139657=DIRECTION('center_axis',(0.,0.,1.));
#139658=DIRECTION('ref_axis',(-1.,0.,0.));
#139659=DIRECTION('center_axis',(0.,0.,1.));
#139660=DIRECTION('ref_axis',(-1.,0.,0.));
#139661=DIRECTION('',(0.766044443118977,9.38133875270271E-17,-0.642787609686541));
#139662=DIRECTION('center_axis',(0.,0.,-1.));
#139663=DIRECTION('ref_axis',(-1.,0.,0.));
#139664=DIRECTION('center_axis',(0.,0.,-1.));
#139665=DIRECTION('ref_axis',(-1.,0.,0.));
#139666=DIRECTION('',(0.,0.,1.));
#139667=DIRECTION('',(0.,0.,1.));
#139668=DIRECTION('center_axis',(0.,-1.,0.));
#139669=DIRECTION('ref_axis',(0.,0.,-1.));
#139670=DIRECTION('',(0.,-1.,0.));
#139671=DIRECTION('center_axis',(-1.,3.49148133884313E-15,0.));
#139672=DIRECTION('ref_axis',(0.,0.,-1.));
#139673=DIRECTION('',(-1.,3.49148133884313E-15,0.));
#139674=DIRECTION('center_axis',(0.,0.,-1.));
#139675=DIRECTION('ref_axis',(-1.,0.,0.));
#139676=DIRECTION('',(0.,0.,-1.));
#139677=DIRECTION('',(0.,0.,-1.));
#139678=DIRECTION('center_axis',(0.,0.,1.));
#139679=DIRECTION('ref_axis',(1.,0.,0.));
#139680=DIRECTION('center_axis',(0.,0.,-1.));
#139681=DIRECTION('ref_axis',(-1.,0.,0.));
#139682=DIRECTION('center_axis',(-1.4081690688991E-16,0.,-1.));
#139683=DIRECTION('ref_axis',(-1.,0.,1.4081690688991E-16));
#139684=DIRECTION('center_axis',(-1.4081690688991E-16,0.,-1.));
#139685=DIRECTION('ref_axis',(-1.,0.,1.4081690688991E-16));
#139686=DIRECTION('',(1.4081690688991E-16,0.,1.));
#139687=DIRECTION('center_axis',(0.,0.,-1.));
#139688=DIRECTION('ref_axis',(-1.,0.,0.));
#139689=DIRECTION('center_axis',(0.,0.,1.));
#139690=DIRECTION('ref_axis',(1.,0.,0.));
#139691=DIRECTION('center_axis',(-1.4081690688991E-16,0.,-1.));
#139692=DIRECTION('ref_axis',(-1.,0.,1.4081690688991E-16));
#139693=DIRECTION('',(0.,0.,1.));
#139694=DIRECTION('center_axis',(0.,0.,-1.));
#139695=DIRECTION('ref_axis',(-1.,0.,0.));
#139696=DIRECTION('center_axis',(0.,0.,-1.));
#139697=DIRECTION('ref_axis',(-1.,0.,0.));
#139698=DIRECTION('center_axis',(0.,0.,-1.));
#139699=DIRECTION('ref_axis',(-1.,0.,0.));
#139700=DIRECTION('center_axis',(1.22464679914735E-16,1.,0.));
#139701=DIRECTION('ref_axis',(1.,-1.22464679914735E-16,0.));
#139702=DIRECTION('center_axis',(0.,0.,1.));
#139703=DIRECTION('ref_axis',(-1.,0.,0.));
#139704=DIRECTION('center_axis',(0.,0.,1.));
#139705=DIRECTION('ref_axis',(-1.,0.,0.));
#139706=DIRECTION('center_axis',(0.,0.,1.));
#139707=DIRECTION('ref_axis',(1.,0.,0.));
#139708=DIRECTION('center_axis',(0.,0.,-1.));
#139709=DIRECTION('ref_axis',(-1.,0.,0.));
#139710=DIRECTION('',(0.,0.,1.));
#139711=DIRECTION('center_axis',(0.,0.,1.));
#139712=DIRECTION('ref_axis',(1.,0.,0.));
#139713=DIRECTION('center_axis',(0.,0.,-1.));
#139714=DIRECTION('ref_axis',(-1.,0.,0.));
#139715=DIRECTION('',(0.,0.,-1.));
#139716=DIRECTION('center_axis',(0.,0.,1.));
#139717=DIRECTION('ref_axis',(-1.,0.,0.));
#139718=DIRECTION('',(0.,0.,-1.));
#139719=DIRECTION('center_axis',(0.,0.,1.));
#139720=DIRECTION('ref_axis',(1.,0.,0.));
#139721=DIRECTION('center_axis',(0.,0.,-1.));
#139722=DIRECTION('ref_axis',(-1.,0.,0.));
#139723=DIRECTION('',(0.,0.,-1.));
#139724=DIRECTION('center_axis',(0.,0.,-1.));
#139725=DIRECTION('ref_axis',(-1.,0.,0.));
#139726=DIRECTION('center_axis',(0.,0.,-1.));
#139727=DIRECTION('ref_axis',(-1.,0.,0.));
#139728=DIRECTION('center_axis',(0.,0.,-1.));
#139729=DIRECTION('ref_axis',(-1.,0.,0.));
#139730=DIRECTION('',(0.,0.,-1.));
#139731=DIRECTION('center_axis',(0.,0.,-1.));
#139732=DIRECTION('ref_axis',(-1.,0.,0.));
#139733=DIRECTION('center_axis',(0.,0.,-1.));
#139734=DIRECTION('ref_axis',(-1.,0.,0.));
#139735=DIRECTION('center_axis',(0.,0.,-1.));
#139736=DIRECTION('ref_axis',(-1.,0.,0.));
#139737=DIRECTION('',(0.,0.,-1.));
#139738=DIRECTION('center_axis',(0.,0.,-1.));
#139739=DIRECTION('ref_axis',(-1.,0.,0.));
#139740=DIRECTION('center_axis',(0.,0.,-1.));
#139741=DIRECTION('ref_axis',(-1.,0.,0.));
#139742=DIRECTION('center_axis',(0.,0.,-1.));
#139743=DIRECTION('ref_axis',(-1.,0.,0.));
#139744=DIRECTION('',(0.,0.,-1.));
#139745=DIRECTION('center_axis',(0.,0.,-1.));
#139746=DIRECTION('ref_axis',(-1.,0.,0.));
#139747=DIRECTION('center_axis',(0.,0.,-1.));
#139748=DIRECTION('ref_axis',(-1.,0.,0.));
#139749=DIRECTION('center_axis',(0.,0.,-1.));
#139750=DIRECTION('ref_axis',(-1.,0.,0.));
#139751=DIRECTION('',(0.,0.,-1.));
#139752=DIRECTION('center_axis',(0.,0.,-1.));
#139753=DIRECTION('ref_axis',(-1.,0.,0.));
#139754=DIRECTION('center_axis',(0.,0.,-1.));
#139755=DIRECTION('ref_axis',(-1.,0.,0.));
#139756=DIRECTION('center_axis',(0.,0.,-1.));
#139757=DIRECTION('ref_axis',(-1.,0.,0.));
#139758=DIRECTION('',(0.,0.,-1.));
#139759=DIRECTION('center_axis',(0.,0.,-1.));
#139760=DIRECTION('ref_axis',(-1.,0.,0.));
#139761=DIRECTION('center_axis',(0.,0.,1.));
#139762=DIRECTION('ref_axis',(1.,0.,0.));
#139763=DIRECTION('center_axis',(0.,0.,-1.));
#139764=DIRECTION('ref_axis',(-1.,0.,0.));
#139765=DIRECTION('',(0.,0.,1.));
#139766=DIRECTION('center_axis',(0.,0.,-1.));
#139767=DIRECTION('ref_axis',(-1.,0.,0.));
#139768=DIRECTION('center_axis',(0.,0.,1.));
#139769=DIRECTION('ref_axis',(1.,0.,0.));
#139770=DIRECTION('center_axis',(0.,0.,-1.));
#139771=DIRECTION('ref_axis',(-1.,0.,0.));
#139772=DIRECTION('',(0.,0.,1.));
#139773=DIRECTION('center_axis',(0.,0.,-1.));
#139774=DIRECTION('ref_axis',(-1.,0.,0.));
#139775=DIRECTION('center_axis',(0.,0.,1.));
#139776=DIRECTION('ref_axis',(1.,0.,0.));
#139777=DIRECTION('center_axis',(0.,0.,-1.));
#139778=DIRECTION('ref_axis',(-1.,0.,0.));
#139779=DIRECTION('',(0.,0.,1.));
#139780=DIRECTION('center_axis',(0.,0.,-1.));
#139781=DIRECTION('ref_axis',(-1.,0.,0.));
#139782=DIRECTION('center_axis',(0.,0.,1.));
#139783=DIRECTION('ref_axis',(1.,0.,0.));
#139784=DIRECTION('center_axis',(0.,0.,-1.));
#139785=DIRECTION('ref_axis',(-1.,0.,0.));
#139786=DIRECTION('',(0.,0.,1.));
#139787=DIRECTION('center_axis',(0.,0.,-1.));
#139788=DIRECTION('ref_axis',(-1.,0.,0.));
#139789=DIRECTION('center_axis',(0.,0.,1.));
#139790=DIRECTION('ref_axis',(1.,0.,0.));
#139791=DIRECTION('',(0.,0.,1.));
#139792=DIRECTION('center_axis',(0.,0.,-1.));
#139793=DIRECTION('ref_axis',(-1.,0.,0.));
#139794=DIRECTION('',(0.,0.,1.));
#139795=DIRECTION('center_axis',(0.,0.,-1.));
#139796=DIRECTION('ref_axis',(-1.,0.,0.));
#139797=DIRECTION('center_axis',(1.,0.,0.));
#139798=DIRECTION('ref_axis',(0.,0.,-1.));
#139799=DIRECTION('',(0.,1.,0.));
#139800=DIRECTION('',(0.,0.,1.));
#139801=DIRECTION('',(0.,1.,0.));
#139802=DIRECTION('center_axis',(0.,0.,1.));
#139803=DIRECTION('ref_axis',(1.,0.,0.));
#139804=DIRECTION('center_axis',(0.,0.,-1.));
#139805=DIRECTION('ref_axis',(-1.,0.,0.));
#139806=DIRECTION('',(0.,0.,1.));
#139807=DIRECTION('center_axis',(0.,0.,-1.));
#139808=DIRECTION('ref_axis',(-1.,0.,0.));
#139809=DIRECTION('center_axis',(0.,-1.,0.));
#139810=DIRECTION('ref_axis',(0.,0.,-1.));
#139811=DIRECTION('',(1.,0.,0.));
#139812=DIRECTION('',(0.,0.,1.));
#139813=DIRECTION('',(1.,0.,0.));
#139814=DIRECTION('center_axis',(0.,0.,1.));
#139815=DIRECTION('ref_axis',(1.,0.,0.));
#139816=DIRECTION('center_axis',(0.,0.,-1.));
#139817=DIRECTION('ref_axis',(-1.,0.,0.));
#139818=DIRECTION('',(0.,0.,1.));
#139819=DIRECTION('center_axis',(0.,0.,-1.));
#139820=DIRECTION('ref_axis',(-1.,0.,0.));
#139821=DIRECTION('center_axis',(-1.,1.5419764230905E-16,0.));
#139822=DIRECTION('ref_axis',(-1.5419764230905E-16,-1.,0.));
#139823=DIRECTION('',(-1.5419764230905E-16,-1.,0.));
#139824=DIRECTION('',(0.,0.,1.));
#139825=DIRECTION('',(-1.5419764230905E-16,-1.,0.));
#139826=DIRECTION('center_axis',(0.,0.,1.));
#139827=DIRECTION('ref_axis',(1.,0.,0.));
#139828=DIRECTION('center_axis',(0.,0.,-1.));
#139829=DIRECTION('ref_axis',(-1.,0.,0.));
#139830=DIRECTION('',(0.,0.,1.));
#139831=DIRECTION('center_axis',(0.,0.,-1.));
#139832=DIRECTION('ref_axis',(-1.,0.,0.));
#139833=DIRECTION('center_axis',(0.,1.,0.));
#139834=DIRECTION('ref_axis',(0.,0.,1.));
#139835=DIRECTION('',(-1.,0.,0.));
#139836=DIRECTION('',(-1.,0.,0.));
#139837=DIRECTION('center_axis',(0.,0.,-1.));
#139838=DIRECTION('ref_axis',(-1.,0.,0.));
#139839=DIRECTION('',(0.,-1.,0.));
#139840=DIRECTION('center_axis',(0.,0.,1.));
#139841=DIRECTION('ref_axis',(-1.,0.,0.));
#139842=DIRECTION('',(1.,0.,0.));
#139843=DIRECTION('center_axis',(0.,0.,1.));
#139844=DIRECTION('ref_axis',(-1.,0.,0.));
#139845=DIRECTION('',(1.5419764230905E-16,1.,0.));
#139846=DIRECTION('center_axis',(0.,0.,1.));
#139847=DIRECTION('ref_axis',(-1.,0.,0.));
#139848=DIRECTION('',(-1.,0.,0.));
#139849=DIRECTION('center_axis',(0.,0.,1.));
#139850=DIRECTION('ref_axis',(-1.,0.,0.));
#139851=DIRECTION('center_axis',(0.,0.,-1.));
#139852=DIRECTION('ref_axis',(-1.,0.,0.));
#139853=DIRECTION('center_axis',(0.,0.,-1.));
#139854=DIRECTION('ref_axis',(-1.,0.,0.));
#139855=DIRECTION('center_axis',(0.,0.,-1.));
#139856=DIRECTION('ref_axis',(-1.,0.,0.));
#139857=DIRECTION('center_axis',(0.,0.,-1.));
#139858=DIRECTION('ref_axis',(-1.,0.,0.));
#139859=DIRECTION('center_axis',(0.,0.,-1.));
#139860=DIRECTION('ref_axis',(-1.,0.,0.));
#139861=DIRECTION('center_axis',(0.,0.,-1.));
#139862=DIRECTION('ref_axis',(-1.,0.,0.));
#139863=DIRECTION('',(1.,0.,0.));
#139864=DIRECTION('center_axis',(0.,0.,-1.));
#139865=DIRECTION('ref_axis',(-1.,0.,0.));
#139866=DIRECTION('',(0.,1.,0.));
#139867=DIRECTION('center_axis',(0.,0.,-1.));
#139868=DIRECTION('ref_axis',(-1.,0.,0.));
#139869=DIRECTION('',(-1.,0.,0.));
#139870=DIRECTION('center_axis',(0.,0.,-1.));
#139871=DIRECTION('ref_axis',(-1.,0.,0.));
#139872=DIRECTION('',(0.,-1.,0.));
#139873=DIRECTION('center_axis',(0.,0.,1.));
#139874=DIRECTION('ref_axis',(1.,0.,0.));
#139875=DIRECTION('',(0.,0.,1.));
#139876=DIRECTION('center_axis',(0.,0.,-1.));
#139877=DIRECTION('ref_axis',(-1.,0.,0.));
#139878=DIRECTION('',(0.,0.,1.));
#139879=DIRECTION('center_axis',(-1.,0.,0.));
#139880=DIRECTION('ref_axis',(0.,0.,1.));
#139881=DIRECTION('',(0.,0.,1.));
#139882=DIRECTION('',(1.5419764230905E-16,-1.,0.));
#139883=DIRECTION('center_axis',(0.,0.,1.));
#139884=DIRECTION('ref_axis',(1.,0.,0.));
#139885=DIRECTION('',(0.,0.,1.));
#139886=DIRECTION('center_axis',(0.,0.,-1.));
#139887=DIRECTION('ref_axis',(-1.,0.,0.));
#139888=DIRECTION('center_axis',(0.,1.,0.));
#139889=DIRECTION('ref_axis',(0.,0.,1.));
#139890=DIRECTION('',(0.,0.,1.));
#139891=DIRECTION('',(-1.,-1.5419764230905E-16,0.));
#139892=DIRECTION('center_axis',(0.,0.,1.));
#139893=DIRECTION('ref_axis',(1.,0.,0.));
#139894=DIRECTION('',(0.,0.,1.));
#139895=DIRECTION('center_axis',(0.,0.,-1.));
#139896=DIRECTION('ref_axis',(-1.,0.,0.));
#139897=DIRECTION('center_axis',(1.,0.,0.));
#139898=DIRECTION('ref_axis',(0.,0.,-1.));
#139899=DIRECTION('',(0.,0.,1.));
#139900=DIRECTION('',(0.,1.,0.));
#139901=DIRECTION('center_axis',(0.,0.,1.));
#139902=DIRECTION('ref_axis',(1.,0.,0.));
#139903=DIRECTION('',(0.,0.,1.));
#139904=DIRECTION('center_axis',(0.,0.,-1.));
#139905=DIRECTION('ref_axis',(-1.,0.,0.));
#139906=DIRECTION('center_axis',(0.,-1.,0.));
#139907=DIRECTION('ref_axis',(0.,0.,-1.));
#139908=DIRECTION('',(1.,0.,0.));
#139909=DIRECTION('center_axis',(0.,0.,-1.));
#139910=DIRECTION('ref_axis',(-1.,0.,0.));
#139911=DIRECTION('center_axis',(-1.,0.,0.));
#139912=DIRECTION('ref_axis',(0.,0.,1.));
#139913=DIRECTION('center_axis',(0.,-1.,0.));
#139914=DIRECTION('ref_axis',(0.,0.,-1.));
#139915=DIRECTION('center_axis',(-1.5419764230905E-16,-1.,0.));
#139916=DIRECTION('ref_axis',(1.,-1.5419764230905E-16,0.));
#139917=DIRECTION('center_axis',(0.,-1.,0.));
#139918=DIRECTION('ref_axis',(0.,0.,-1.));
#139919=DIRECTION('center_axis',(1.,0.,0.));
#139920=DIRECTION('ref_axis',(0.,0.,-1.));
#139921=DIRECTION('center_axis',(-1.,0.,0.));
#139922=DIRECTION('ref_axis',(0.,0.,1.));
#139923=DIRECTION('center_axis',(0.,0.,-1.));
#139924=DIRECTION('ref_axis',(-1.,0.,0.));
#139925=DIRECTION('center_axis',(-1.,0.,0.));
#139926=DIRECTION('ref_axis',(0.,0.,1.));
#139927=DIRECTION('center_axis',(0.,0.,-1.));
#139928=DIRECTION('ref_axis',(-1.,0.,0.));
#139929=DIRECTION('center_axis',(0.,-1.,0.));
#139930=DIRECTION('ref_axis',(0.,0.,-1.));
#139931=DIRECTION('center_axis',(-1.,0.,0.));
#139932=DIRECTION('ref_axis',(0.,0.,1.));
#139933=DIRECTION('center_axis',(-1.,0.,0.));
#139934=DIRECTION('ref_axis',(0.,0.,1.));
#139935=DIRECTION('center_axis',(0.,1.,0.));
#139936=DIRECTION('ref_axis',(0.,0.,1.));
#139937=DIRECTION('center_axis',(0.,-1.,0.));
#139938=DIRECTION('ref_axis',(0.,0.,-1.));
#139939=DIRECTION('center_axis',(0.,0.,-1.));
#139940=DIRECTION('ref_axis',(-1.,0.,0.));
#139941=DIRECTION('center_axis',(0.,0.,-1.));
#139942=DIRECTION('ref_axis',(-1.,0.,0.));
#139943=DIRECTION('center_axis',(0.,0.,1.));
#139944=DIRECTION('ref_axis',(-1.,-1.22464679914735E-16,0.));
#139945=DIRECTION('',(0.,0.,-1.));
#139946=DIRECTION('center_axis',(0.,0.,-1.));
#139947=DIRECTION('ref_axis',(-1.,0.,0.));
#139948=DIRECTION('',(0.,0.,-1.));
#139949=DIRECTION('center_axis',(0.,0.,1.));
#139950=DIRECTION('ref_axis',(-1.,0.,0.));
#139951=DIRECTION('center_axis',(0.,0.,-1.));
#139952=DIRECTION('ref_axis',(-1.,0.,0.));
#139953=DIRECTION('',(0.,-1.,0.));
#139954=DIRECTION('center_axis',(0.,0.,1.));
#139955=DIRECTION('ref_axis',(1.,0.,0.));
#139956=DIRECTION('',(1.00849943089951E-15,1.,0.));
#139957=DIRECTION('',(1.00849943089951E-15,-1.,0.));
#139958=DIRECTION('center_axis',(0.,0.,-1.));
#139959=DIRECTION('ref_axis',(1.,0.,0.));
#139960=DIRECTION('',(0.,1.,0.));
#139961=DIRECTION('center_axis',(0.,0.,-1.));
#139962=DIRECTION('ref_axis',(-1.,0.,0.));
#139963=DIRECTION('center_axis',(0.,0.,-1.));
#139964=DIRECTION('ref_axis',(-1.,0.,0.));
#139965=DIRECTION('center_axis',(-1.4081690688991E-16,0.,-1.));
#139966=DIRECTION('ref_axis',(-1.,0.,1.40816906889911E-16));
#139967=DIRECTION('center_axis',(0.,0.,-1.));
#139968=DIRECTION('ref_axis',(-1.,0.,0.));
#139969=DIRECTION('',(0.,0.,-1.));
#139970=DIRECTION('center_axis',(0.,0.,-1.));
#139971=DIRECTION('ref_axis',(1.,0.,0.));
#139972=DIRECTION('',(0.,0.,-1.));
#139973=DIRECTION('center_axis',(-1.,0.,0.));
#139974=DIRECTION('ref_axis',(0.,0.,1.));
#139975=DIRECTION('',(0.,1.,0.));
#139976=DIRECTION('center_axis',(1.,1.00849943089951E-15,0.));
#139977=DIRECTION('ref_axis',(-1.00849943089951E-15,1.,0.));
#139978=DIRECTION('',(1.00849943089951E-15,-1.,0.));
#139979=DIRECTION('center_axis',(0.,0.,1.));
#139980=DIRECTION('ref_axis',(1.,0.,0.));
#139981=DIRECTION('',(1.00849943089951E-15,1.,0.));
#139982=DIRECTION('center_axis',(0.,0.,1.));
#139983=DIRECTION('ref_axis',(1.,0.,0.));
#139984=DIRECTION('',(0.,-1.,0.));
#139985=DIRECTION('center_axis',(0.,0.,-1.));
#139986=DIRECTION('ref_axis',(-1.,0.,0.));
#139987=DIRECTION('',(0.,0.,-1.));
#139988=DIRECTION('',(0.,0.,-1.));
#139989=DIRECTION('center_axis',(-1.,0.,0.));
#139990=DIRECTION('ref_axis',(0.,0.,1.));
#139991=DIRECTION('center_axis',(1.,-1.00849943089951E-15,0.));
#139992=DIRECTION('ref_axis',(-1.00849943089951E-15,-1.,0.));
#139993=DIRECTION('axis',(0.,0.,1.));
#139994=DIRECTION('refdir',(1.,0.,0.));
#139995=DIRECTION('',(0.,-0.861627801655617,0.507540669714367));
#139996=DIRECTION('',(0.981067125781876,-0.193668001254952,0.));
#139997=DIRECTION('',(1.,3.18032637262414E-16,0.));
#139998=DIRECTION('',(0.,0.861627801655617,-0.507540669714367));
#139999=DIRECTION('',(-0.923312500482147,0.384049510419433,-4.73695157173399E-15));
#140000=DIRECTION('',(-1.,-3.18032637262414E-16,0.));
#140001=DIRECTION('center_axis',(1.61414497707192E-16,-0.507540669714368,
-0.861627801655617));
#140002=DIRECTION('ref_axis',(1.4032263518717E-32,0.861627801655617,-0.507540669714367));
#140003=DIRECTION('center_axis',(0.,0.,1.));
#140004=DIRECTION('ref_axis',(1.,0.,0.));
#140005=DIRECTION('',(0.,-0.861627801655622,-0.507540669714359));
#140006=DIRECTION('',(0.923312500482125,-0.384049510419485,0.));
#140007=DIRECTION('',(1.,2.13949228703806E-15,-3.70074341541719E-15));
#140008=DIRECTION('',(0.,0.861627801655622,0.507540669714359));
#140009=DIRECTION('',(-0.981067125781872,0.193668001254975,2.368475785867E-15));
#140010=DIRECTION('',(-1.,-2.13949228703806E-15,3.70074341541719E-15));
#140011=DIRECTION('center_axis',(-4.27454276172943E-15,0.507540669714359,
-0.861627801655622));
#140012=DIRECTION('ref_axis',(-3.1205381319799E-31,0.861627801655622,0.507540669714359));
#140013=DIRECTION('center_axis',(0.,0.,1.));
#140014=DIRECTION('ref_axis',(1.,0.,0.));
#140015=DIRECTION('center_axis',(0.,0.,1.));
#140016=DIRECTION('ref_axis',(1.,0.,0.));
#140017=DIRECTION('center_axis',(0.,0.,1.));
#140018=DIRECTION('ref_axis',(1.,0.,0.));
#140019=DIRECTION('',(0.,0.,1.));
#140020=DIRECTION('center_axis',(0.,0.,1.));
#140021=DIRECTION('ref_axis',(1.,0.,0.));
#140022=DIRECTION('center_axis',(0.,0.,1.));
#140023=DIRECTION('ref_axis',(1.,0.,0.));
#140024=DIRECTION('',(-0.857167300702112,-1.04972719113862E-16,0.515038074910054));
#140025=DIRECTION('center_axis',(1.,0.,0.));
#140026=DIRECTION('ref_axis',(0.,0.,-1.));
#140027=DIRECTION('',(-1.,0.,0.));
#140028=DIRECTION('center_axis',(1.,0.,0.));
#140029=DIRECTION('ref_axis',(0.,0.,-1.));
#140030=DIRECTION('center_axis',(1.,0.,0.));
#140031=DIRECTION('ref_axis',(0.,0.,-1.));
#140032=DIRECTION('',(-1.,0.,0.));
#140033=DIRECTION('center_axis',(1.,0.,0.));
#140034=DIRECTION('ref_axis',(0.,0.,-1.));
#140035=DIRECTION('center_axis',(-1.,0.,0.));
#140036=DIRECTION('ref_axis',(0.,0.,1.));
#140037=DIRECTION('',(1.,0.,0.));
#140038=DIRECTION('center_axis',(1.,0.,0.));
#140039=DIRECTION('ref_axis',(0.,0.,-1.));
#140040=DIRECTION('center_axis',(-1.,0.,0.));
#140041=DIRECTION('ref_axis',(0.,0.,1.));
#140042=DIRECTION('',(1.,0.,0.));
#140043=DIRECTION('center_axis',(1.,0.,0.));
#140044=DIRECTION('ref_axis',(0.,0.,-1.));
#140045=DIRECTION('center_axis',(-1.,0.,0.));
#140046=DIRECTION('ref_axis',(0.,0.,1.));
#140047=DIRECTION('',(1.,0.,0.));
#140048=DIRECTION('center_axis',(1.,0.,0.));
#140049=DIRECTION('ref_axis',(0.,0.,-1.));
#140050=DIRECTION('center_axis',(1.,0.,0.));
#140051=DIRECTION('ref_axis',(0.,0.,-1.));
#140052=DIRECTION('',(-1.,0.,0.));
#140053=DIRECTION('center_axis',(1.,0.,0.));
#140054=DIRECTION('ref_axis',(0.,0.,-1.));
#140055=DIRECTION('center_axis',(0.,0.,-1.));
#140056=DIRECTION('ref_axis',(-1.,0.,0.));
#140057=DIRECTION('center_axis',(0.,0.,1.));
#140058=DIRECTION('ref_axis',(1.,0.,0.));
#140059=DIRECTION('',(0.,0.,1.));
#140060=DIRECTION('',(0.,0.,1.));
#140061=DIRECTION('',(0.,0.,1.));
#140062=DIRECTION('center_axis',(0.,0.,-1.));
#140063=DIRECTION('ref_axis',(-1.,0.,0.));
#140064=DIRECTION('center_axis',(0.,0.,1.));
#140065=DIRECTION('ref_axis',(1.,0.,0.));
#140066=DIRECTION('center_axis',(1.,0.,0.));
#140067=DIRECTION('ref_axis',(0.,0.,-1.));
#140068=DIRECTION('',(0.,0.861627801655622,0.507540669714359));
#140069=DIRECTION('',(0.,-0.861627801655622,-0.507540669714359));
#140070=DIRECTION('center_axis',(0.0081151995614808,-0.157069337498387,
-0.987554234841761));
#140071=DIRECTION('ref_axis',(-0.999613692707062,0.0249787695829795,-0.0121871416941057));
#140072=DIRECTION('center_axis',(-0.00811519956086331,-0.157069337498389,
-0.987554234841765));
#140073=DIRECTION('ref_axis',(-0.999613692707067,0.0275272506419769,0.00383612104018571));
#140074=DIRECTION('center_axis',(1.,0.,0.));
#140075=DIRECTION('ref_axis',(0.,0.,-1.));
#140076=DIRECTION('',(0.,-0.861627801655617,0.507540669714367));
#140077=DIRECTION('',(0.,0.861627801655617,-0.507540669714367));
#140078=DIRECTION('center_axis',(-0.00811519956275127,0.157069337498393,
-0.987554234841749));
#140079=DIRECTION('ref_axis',(0.999613692707052,-0.0249787695827683,-0.0121871416953586));
#140080=DIRECTION('center_axis',(0.0081151995614462,0.15706933749836,-0.987554234841765));
#140081=DIRECTION('ref_axis',(0.99961369270706,-0.027527250642151,0.0038361210407496));
#140082=DIRECTION('center_axis',(1.,0.,0.));
#140083=DIRECTION('ref_axis',(0.,0.,-1.));
#140084=DIRECTION('',(0.,0.861627801655617,-0.507540669714367));
#140085=DIRECTION('center_axis',(-0.00811519956150803,0.157069337498411,
-0.987554234841757));
#140086=DIRECTION('ref_axis',(0.999613692707061,-0.0249787695829988,-0.012187141694134));
#140087=DIRECTION('center_axis',(1.,0.,0.));
#140088=DIRECTION('ref_axis',(0.,0.,-1.));
#140089=DIRECTION('',(0.,-0.861627801655617,0.507540669714367));
#140090=DIRECTION('center_axis',(0.00811519956086742,0.157069337498383,
-0.987554234841766));
#140091=DIRECTION('ref_axis',(0.999613692707066,-0.027527250642027,0.00383612104018404));
#140092=DIRECTION('center_axis',(1.,0.,0.));
#140093=DIRECTION('ref_axis',(0.,0.,-1.));
#140094=DIRECTION('',(0.,-0.861627801655622,-0.507540669714359));
#140095=DIRECTION('center_axis',(0.00811519956148901,-0.157069337498403,
-0.987554234841758));
#140096=DIRECTION('ref_axis',(-0.999613692707061,0.0249787695830125,-0.012187141694119));
#140097=DIRECTION('center_axis',(1.,0.,0.));
#140098=DIRECTION('ref_axis',(0.,0.,-1.));
#140099=DIRECTION('',(0.,0.861627801655622,0.507540669714359));
#140100=DIRECTION('center_axis',(-0.00811519956206617,-0.157069337498402,
-0.987554234841754));
#140101=DIRECTION('ref_axis',(-0.999613692707057,0.0275272506421834,0.00383612104137151));
#140102=DIRECTION('center_axis',(0.,0.,-1.));
#140103=DIRECTION('ref_axis',(-1.,0.,0.));
#140104=DIRECTION('center_axis',(0.,0.,1.));
#140105=DIRECTION('ref_axis',(1.,0.,0.));
#140106=DIRECTION('axis',(0.,0.,1.));
#140107=DIRECTION('refdir',(1.,0.,0.));
#140108=DIRECTION('center_axis',(0.,0.,1.));
#140109=DIRECTION('ref_axis',(1.,0.,0.));
#140110=DIRECTION('',(1.,0.,0.));
#140111=DIRECTION('',(0.,-1.,0.));
#140112=DIRECTION('',(-1.,0.,0.));
#140113=DIRECTION('',(0.,1.,0.));
#140114=DIRECTION('center_axis',(0.,0.,1.));
#140115=DIRECTION('ref_axis',(1.,0.,0.));
#140116=DIRECTION('',(0.,1.,0.));
#140117=DIRECTION('center_axis',(0.,0.,1.));
#140118=DIRECTION('ref_axis',(1.,0.,0.));
#140119=DIRECTION('',(-1.,0.,0.));
#140120=DIRECTION('',(0.,1.,0.));
#140121=DIRECTION('',(1.,0.,0.));
#140122=DIRECTION('center_axis',(0.,0.,1.));
#140123=DIRECTION('ref_axis',(1.,0.,0.));
#140124=DIRECTION('center_axis',(1.,0.,0.));
#140125=DIRECTION('ref_axis',(0.,0.,-1.));
#140126=DIRECTION('',(0.,0.,1.));
#140127=DIRECTION('',(0.,1.,0.));
#140128=DIRECTION('',(0.,0.,-1.));
#140129=DIRECTION('',(-4.08120948402688E-16,1.,0.));
#140130=DIRECTION('',(0.,0.,1.));
#140131=DIRECTION('',(0.,0.,1.));
#140132=DIRECTION('',(4.10921029238558E-16,1.,0.));
#140133=DIRECTION('center_axis',(0.,1.,0.));
#140134=DIRECTION('ref_axis',(0.,0.,1.));
#140135=DIRECTION('',(0.,0.,1.));
#140136=DIRECTION('',(-1.,0.,0.));
#140137=DIRECTION('',(0.,0.,-1.));
#140138=DIRECTION('',(-1.,0.,0.));
#140139=DIRECTION('center_axis',(-1.,0.,0.));
#140140=DIRECTION('ref_axis',(0.,0.,1.));
#140141=DIRECTION('',(0.,0.,1.));
#140142=DIRECTION('',(0.,-1.,0.));
#140143=DIRECTION('',(0.,0.,-1.));
#140144=DIRECTION('',(0.,-1.,0.));
#140145=DIRECTION('',(0.,0.,1.));
#140146=DIRECTION('',(0.,0.,1.));
#140147=DIRECTION('',(0.,-1.,0.));
#140148=DIRECTION('center_axis',(0.,-1.,0.));
#140149=DIRECTION('ref_axis',(0.,0.,-1.));
#140150=DIRECTION('',(0.,0.,1.));
#140151=DIRECTION('',(1.,0.,0.));
#140152=DIRECTION('',(0.,0.,-1.));
#140153=DIRECTION('',(1.,0.,0.));
#140154=DIRECTION('center_axis',(0.,0.,1.));
#140155=DIRECTION('ref_axis',(1.,0.,0.));
#140156=DIRECTION('',(0.,1.,0.));
#140157=DIRECTION('center_axis',(0.,0.,1.));
#140158=DIRECTION('ref_axis',(1.,0.,0.));
#140159=DIRECTION('',(-1.,0.,0.));
#140160=DIRECTION('center_axis',(0.,0.,1.));
#140161=DIRECTION('ref_axis',(1.,0.,0.));
#140162=DIRECTION('',(0.,-1.,0.));
#140163=DIRECTION('center_axis',(0.,0.,1.));
#140164=DIRECTION('ref_axis',(1.,0.,0.));
#140165=DIRECTION('',(1.,0.,0.));
#140166=DIRECTION('center_axis',(0.,0.,1.));
#140167=DIRECTION('ref_axis',(1.,0.,0.));
#140168=DIRECTION('',(1.,0.,0.));
#140169=DIRECTION('center_axis',(0.,0.,-1.));
#140170=DIRECTION('ref_axis',(1.,0.,0.));
#140171=DIRECTION('',(0.,-1.,0.));
#140172=DIRECTION('center_axis',(0.,0.,-1.));
#140173=DIRECTION('ref_axis',(1.,0.,0.));
#140174=DIRECTION('',(-1.,0.,0.));
#140175=DIRECTION('center_axis',(0.,0.,-1.));
#140176=DIRECTION('ref_axis',(1.,0.,0.));
#140177=DIRECTION('',(0.,1.,0.));
#140178=DIRECTION('center_axis',(0.,0.,-1.));
#140179=DIRECTION('ref_axis',(1.,0.,0.));
#140180=DIRECTION('center_axis',(-1.,0.,0.));
#140181=DIRECTION('ref_axis',(0.,0.,1.));
#140182=DIRECTION('',(0.,0.,-1.));
#140183=DIRECTION('',(0.,1.,0.));
#140184=DIRECTION('',(0.,0.,1.));
#140185=DIRECTION('',(0.,-1.,0.));
#140186=DIRECTION('center_axis',(0.,-1.,0.));
#140187=DIRECTION('ref_axis',(0.,0.,-1.));
#140188=DIRECTION('',(0.,0.,1.));
#140189=DIRECTION('',(1.,0.,0.));
#140190=DIRECTION('',(0.,0.,-1.));
#140191=DIRECTION('',(-1.,0.,0.));
#140192=DIRECTION('center_axis',(1.,0.,0.));
#140193=DIRECTION('ref_axis',(0.,0.,-1.));
#140194=DIRECTION('',(0.,0.,-1.));
#140195=DIRECTION('',(0.,-1.,0.));
#140196=DIRECTION('',(0.,0.,1.));
#140197=DIRECTION('',(0.,1.,0.));
#140198=DIRECTION('center_axis',(0.,1.,0.));
#140199=DIRECTION('ref_axis',(0.,0.,1.));
#140200=DIRECTION('',(0.,0.,-1.));
#140201=DIRECTION('',(1.,0.,0.));
#140202=DIRECTION('',(0.,0.,1.));
#140203=DIRECTION('',(-1.,0.,0.));
#140204=DIRECTION('center_axis',(0.,0.,-1.));
#140205=DIRECTION('ref_axis',(-1.,0.,0.));
#140206=DIRECTION('center_axis',(0.,0.,-1.));
#140207=DIRECTION('ref_axis',(1.,0.,0.));
#140208=DIRECTION('center_axis',(0.,0.,-1.));
#140209=DIRECTION('ref_axis',(-1.,0.,0.));
#140210=DIRECTION('center_axis',(0.,0.,-1.));
#140211=DIRECTION('ref_axis',(-1.,0.,0.));
#140212=DIRECTION('center_axis',(0.,0.,-1.));
#140213=DIRECTION('ref_axis',(1.,0.,0.));
#140214=DIRECTION('center_axis',(0.,0.,-1.));
#140215=DIRECTION('ref_axis',(-1.,0.,0.));
#140216=DIRECTION('center_axis',(0.,0.,-1.));
#140217=DIRECTION('ref_axis',(-1.,0.,0.));
#140218=DIRECTION('center_axis',(0.,0.,-1.));
#140219=DIRECTION('ref_axis',(1.,0.,0.));
#140220=DIRECTION('center_axis',(0.,0.,-1.));
#140221=DIRECTION('ref_axis',(-1.,0.,0.));
#140222=DIRECTION('center_axis',(0.,0.,-1.));
#140223=DIRECTION('ref_axis',(-1.,0.,0.));
#140224=DIRECTION('center_axis',(0.,0.,-1.));
#140225=DIRECTION('ref_axis',(1.,0.,0.));
#140226=DIRECTION('center_axis',(0.,0.,-1.));
#140227=DIRECTION('ref_axis',(-1.,0.,0.));
#140228=DIRECTION('center_axis',(0.,1.,0.));
#140229=DIRECTION('ref_axis',(0.,0.,1.));
#140230=DIRECTION('center_axis',(1.,0.,0.));
#140231=DIRECTION('ref_axis',(0.,0.,-1.));
#140232=DIRECTION('center_axis',(-1.,0.,0.));
#140233=DIRECTION('ref_axis',(0.,0.,1.));
#140234=DIRECTION('center_axis',(1.,2.31296463463574E-15,0.));
#140235=DIRECTION('ref_axis',(-2.31296463463574E-15,1.,0.));
#140236=DIRECTION('center_axis',(0.,1.,0.));
#140237=DIRECTION('ref_axis',(0.,0.,1.));
#140238=DIRECTION('center_axis',(0.,1.,0.));
#140239=DIRECTION('ref_axis',(0.,0.,1.));
#140240=DIRECTION('center_axis',(0.,1.,0.));
#140241=DIRECTION('ref_axis',(0.,0.,1.));
#140242=DIRECTION('center_axis',(1.,0.,0.));
#140243=DIRECTION('ref_axis',(0.,0.,-1.));
#140244=DIRECTION('center_axis',(0.,-1.,0.));
#140245=DIRECTION('ref_axis',(0.,0.,-1.));
#140246=DIRECTION('center_axis',(0.,1.,0.));
#140247=DIRECTION('ref_axis',(0.,0.,1.));
#140248=DIRECTION('center_axis',(1.,0.,0.));
#140249=DIRECTION('ref_axis',(0.,0.,-1.));
#140250=DIRECTION('center_axis',(1.,0.,0.));
#140251=DIRECTION('ref_axis',(0.,0.,-1.));
#140252=DIRECTION('center_axis',(0.,0.,-1.));
#140253=DIRECTION('ref_axis',(-1.,0.,0.));
#140254=DIRECTION('center_axis',(0.,0.,1.));
#140255=DIRECTION('ref_axis',(1.,0.,0.));
#140256=DIRECTION('center_axis',(0.,0.,-1.));
#140257=DIRECTION('ref_axis',(1.,0.,0.));
#140258=DIRECTION('center_axis',(0.,0.,-1.));
#140259=DIRECTION('ref_axis',(-1.,0.,0.));
#140260=DIRECTION('center_axis',(0.,0.,1.));
#140261=DIRECTION('ref_axis',(1.,0.,0.));
#140262=DIRECTION('center_axis',(0.,0.,-1.));
#140263=DIRECTION('ref_axis',(1.,0.,0.));
#140264=DIRECTION('center_axis',(0.,0.,-1.));
#140265=DIRECTION('ref_axis',(-1.,0.,0.));
#140266=DIRECTION('center_axis',(0.,0.,1.));
#140267=DIRECTION('ref_axis',(1.,0.,0.));
#140268=DIRECTION('center_axis',(0.,0.,-1.));
#140269=DIRECTION('ref_axis',(1.,0.,0.));
#140270=DIRECTION('center_axis',(0.,0.,-1.));
#140271=DIRECTION('ref_axis',(-1.,0.,0.));
#140272=DIRECTION('center_axis',(0.,0.,1.));
#140273=DIRECTION('ref_axis',(1.,0.,0.));
#140274=DIRECTION('center_axis',(0.,0.,-1.));
#140275=DIRECTION('ref_axis',(1.,0.,0.));
#140276=DIRECTION('center_axis',(-1.,0.,0.));
#140277=DIRECTION('ref_axis',(0.,0.,1.));
#140278=DIRECTION('',(0.,0.,-1.));
#140279=DIRECTION('',(0.,1.,0.));
#140280=DIRECTION('',(0.,0.,-1.));
#140281=DIRECTION('center_axis',(0.,-1.,0.));
#140282=DIRECTION('ref_axis',(0.,0.,-1.));
#140283=DIRECTION('',(-1.,0.,0.));
#140284=DIRECTION('',(-1.,0.,0.));
#140285=DIRECTION('',(-1.,0.,0.));
#140286=DIRECTION('',(-1.,0.,0.));
#140287=DIRECTION('',(0.,0.,-1.));
#140288=DIRECTION('',(-1.,0.,0.));
#140289=DIRECTION('center_axis',(1.,0.,0.));
#140290=DIRECTION('ref_axis',(0.,0.,-1.));
#140291=DIRECTION('',(0.,-1.,0.));
#140292=DIRECTION('',(0.,0.,-1.));
#140293=DIRECTION('',(0.,-1.,0.));
#140294=DIRECTION('center_axis',(0.,1.,0.));
#140295=DIRECTION('ref_axis',(0.,0.,1.));
#140296=DIRECTION('',(1.,0.,0.));
#140297=DIRECTION('',(1.,0.,0.));
#140298=DIRECTION('',(1.,0.,0.));
#140299=DIRECTION('',(1.,0.,0.));
#140300=DIRECTION('',(1.,0.,0.));
#140301=DIRECTION('center_axis',(0.,0.,1.));
#140302=DIRECTION('ref_axis',(1.,0.,0.));
#140303=DIRECTION('',(0.,-1.,0.));
#140304=DIRECTION('center_axis',(0.,0.,1.));
#140305=DIRECTION('ref_axis',(1.,0.,0.));
#140306=DIRECTION('center_axis',(0.,0.,1.));
#140307=DIRECTION('ref_axis',(1.,0.,0.));
#140308=DIRECTION('center_axis',(0.,0.,1.));
#140309=DIRECTION('ref_axis',(1.,0.,0.));
#140310=DIRECTION('center_axis',(-1.,0.,0.));
#140311=DIRECTION('ref_axis',(0.,0.,1.));
#140312=DIRECTION('center_axis',(0.,-1.,0.));
#140313=DIRECTION('ref_axis',(0.,0.,-1.));
#140314=DIRECTION('center_axis',(0.,-1.,0.));
#140315=DIRECTION('ref_axis',(0.,0.,-1.));
#140316=DIRECTION('center_axis',(0.,-1.,0.));
#140317=DIRECTION('ref_axis',(0.,0.,-1.));
#140318=DIRECTION('center_axis',(1.,0.,0.));
#140319=DIRECTION('ref_axis',(0.,0.,-1.));
#140320=DIRECTION('center_axis',(-1.,0.,1.38777878078145E-15));
#140321=DIRECTION('ref_axis',(1.38777878078145E-15,0.,1.));
#140322=DIRECTION('center_axis',(0.,0.,1.));
#140323=DIRECTION('ref_axis',(1.,0.,0.));
#140324=DIRECTION('center_axis',(-1.,0.,0.));
#140325=DIRECTION('ref_axis',(0.,0.,1.));
#140326=DIRECTION('center_axis',(0.,0.,1.));
#140327=DIRECTION('ref_axis',(1.,0.,0.));
#140328=DIRECTION('center_axis',(0.,-1.,0.));
#140329=DIRECTION('ref_axis',(0.,0.,-1.));
#140330=DIRECTION('center_axis',(-1.,0.,0.));
#140331=DIRECTION('ref_axis',(0.,0.,1.));
#140332=DIRECTION('center_axis',(-1.,0.,0.));
#140333=DIRECTION('ref_axis',(0.,0.,1.));
#140334=DIRECTION('center_axis',(0.,1.,0.));
#140335=DIRECTION('ref_axis',(0.,0.,1.));
#140336=DIRECTION('center_axis',(0.,-1.,0.));
#140337=DIRECTION('ref_axis',(0.,0.,-1.));
#140338=DIRECTION('center_axis',(0.,0.,1.));
#140339=DIRECTION('ref_axis',(1.,0.,0.));
#140340=DIRECTION('center_axis',(0.,0.,1.));
#140341=DIRECTION('ref_axis',(1.,0.,0.));
#140342=DIRECTION('center_axis',(0.,-1.,0.));
#140343=DIRECTION('ref_axis',(0.,0.,-1.));
#140344=DIRECTION('center_axis',(-0.98587196814397,0.167500634112039,0.));
#140345=DIRECTION('ref_axis',(-0.167500634112039,-0.98587196814397,0.));
#140346=DIRECTION('center_axis',(-1.,0.,0.));
#140347=DIRECTION('ref_axis',(0.,0.,-1.));
#140348=DIRECTION('center_axis',(0.,1.,0.));
#140349=DIRECTION('ref_axis',(0.,0.,1.));
#140350=DIRECTION('center_axis',(0.,-1.,0.));
#140351=DIRECTION('ref_axis',(0.,0.,-1.));
#140352=DIRECTION('center_axis',(-1.,0.,0.));
#140353=DIRECTION('ref_axis',(0.,0.,1.));
#140354=DIRECTION('center_axis',(-1.,0.,0.));
#140355=DIRECTION('ref_axis',(0.,0.,1.));
#140356=DIRECTION('center_axis',(0.,0.,1.));
#140357=DIRECTION('ref_axis',(1.,0.,0.));
#140358=DIRECTION('center_axis',(-0.98587196814397,-0.16750063411204,1.36817219795744E-15));
#140359=DIRECTION('ref_axis',(0.16750063411204,-0.98587196814397,-7.32459110897286E-33));
#140360=DIRECTION('center_axis',(-0.98587196814397,-0.16750063411204,0.));
#140361=DIRECTION('ref_axis',(0.16750063411204,-0.98587196814397,0.));
#140362=DIRECTION('center_axis',(-1.,0.,0.));
#140363=DIRECTION('ref_axis',(0.,0.,-1.));
#140364=DIRECTION('center_axis',(0.,0.,1.));
#140365=DIRECTION('ref_axis',(1.,0.,0.));
#140366=DIRECTION('center_axis',(0.,-1.,0.));
#140367=DIRECTION('ref_axis',(0.,0.,-1.));
#140368=DIRECTION('center_axis',(1.,0.,0.));
#140369=DIRECTION('ref_axis',(0.,0.,-1.));
#140370=DIRECTION('center_axis',(-1.,0.,0.));
#140371=DIRECTION('ref_axis',(0.,0.,1.));
#140372=DIRECTION('center_axis',(0.,-1.,0.));
#140373=DIRECTION('ref_axis',(0.,0.,-1.));
#140374=DIRECTION('center_axis',(0.,-1.,0.));
#140375=DIRECTION('ref_axis',(0.,0.,-1.));
#140376=DIRECTION('center_axis',(-0.98587196814397,0.167500634112039,0.));
#140377=DIRECTION('ref_axis',(-0.167500634112039,-0.98587196814397,0.));
#140378=DIRECTION('center_axis',(0.,0.,1.));
#140379=DIRECTION('ref_axis',(1.,0.,0.));
#140380=DIRECTION('center_axis',(0.,0.,1.));
#140381=DIRECTION('ref_axis',(1.,0.,0.));
#140382=DIRECTION('',(0.,1.,0.));
#140383=DIRECTION('',(1.,0.,0.));
#140384=DIRECTION('',(0.,-1.,0.));
#140385=DIRECTION('',(-1.,0.,0.));
#140386=DIRECTION('center_axis',(-1.,0.,0.));
#140387=DIRECTION('ref_axis',(0.,0.,1.));
#140388=DIRECTION('',(0.,0.,-1.));
#140389=DIRECTION('',(0.,1.,0.));
#140390=DIRECTION('',(0.,0.,-1.));
#140391=DIRECTION('center_axis',(0.,-1.,0.));
#140392=DIRECTION('ref_axis',(0.,0.,-1.));
#140393=DIRECTION('',(0.,0.,-1.));
#140394=DIRECTION('',(-1.,0.,0.));
#140395=DIRECTION('center_axis',(1.,0.,0.));
#140396=DIRECTION('ref_axis',(0.,0.,-1.));
#140397=DIRECTION('',(0.,0.,-1.));
#140398=DIRECTION('',(0.,-1.,0.));
#140399=DIRECTION('center_axis',(0.,1.,0.));
#140400=DIRECTION('ref_axis',(0.,0.,1.));
#140401=DIRECTION('',(1.,0.,0.));
#140402=DIRECTION('center_axis',(0.,0.,1.));
#140403=DIRECTION('ref_axis',(1.,0.,0.));
#140404=DIRECTION('center_axis',(0.,1.,0.));
#140405=DIRECTION('ref_axis',(0.,0.,1.));
#140406=DIRECTION('',(-1.,0.,0.));
#140407=DIRECTION('center_axis',(0.,0.,-1.));
#140408=DIRECTION('ref_axis',(-1.,0.,0.));
#140409=DIRECTION('center_axis',(0.,-1.,0.));
#140410=DIRECTION('ref_axis',(0.,0.,-1.));
#140411=DIRECTION('',(1.,0.,0.));
#140412=DIRECTION('center_axis',(0.,0.,-1.));
#140413=DIRECTION('ref_axis',(-1.,0.,0.));
#140414=DIRECTION('axis',(0.,0.,1.));
#140415=DIRECTION('refdir',(1.,0.,0.));
#140416=DIRECTION('center_axis',(1.83697019872103E-16,1.83697019872101E-16,
-1.));
#140417=DIRECTION('ref_axis',(-1.,3.37445951098914E-32,-1.83697019872103E-16));
#140418=DIRECTION('center_axis',(0.,0.,1.));
#140419=DIRECTION('ref_axis',(1.,0.,0.));
#140420=DIRECTION('',(1.83697019872103E-16,1.83697019872101E-16,-1.));
#140421=DIRECTION('center_axis',(-1.83697019872103E-16,-1.83697019872101E-16,
1.));
#140422=DIRECTION('ref_axis',(1.04634114423998E-14,1.,1.83697019872103E-16));
#140423=DIRECTION('',(1.83697019872103E-16,1.83697019872101E-16,-1.));
#140424=DIRECTION('center_axis',(0.,0.,-1.));
#140425=DIRECTION('ref_axis',(-1.,0.,0.));
#140426=DIRECTION('center_axis',(-1.83697019872103E-16,-1.83697019872101E-16,
1.));
#140427=DIRECTION('ref_axis',(1.04905870583987E-14,1.,1.83697019872103E-16));
#140428=DIRECTION('',(0.767165151815313,0.641449631569141,2.58758337855511E-16));
#140429=DIRECTION('center_axis',(-1.83697019872103E-16,-1.83697019872101E-16,
1.));
#140430=DIRECTION('ref_axis',(-1.04634114423998E-14,-1.,-1.83697019872103E-16));
#140431=DIRECTION('',(0.7671651518153,-0.641449631569158,2.30935664208886E-17));
#140432=DIRECTION('center_axis',(-1.83697019872103E-16,-1.83697019872101E-16,
1.));
#140433=DIRECTION('ref_axis',(-1.04905870583987E-14,-1.,-1.83697019872103E-16));
#140434=DIRECTION('',(-0.641449631569148,0.767165151815307,2.30935664208889E-17));
#140435=DIRECTION('center_axis',(-1.83697019872103E-16,-1.83697019872101E-16,
1.));
#140436=DIRECTION('ref_axis',(-1.04634114423998E-14,-1.,-1.83697019872103E-16));
#140437=DIRECTION('',(0.641449631569153,0.767165151815304,2.58758337855511E-16));
#140438=DIRECTION('center_axis',(-1.83697019872103E-16,-1.83697019872101E-16,
1.));
#140439=DIRECTION('ref_axis',(-1.04905870583987E-14,-1.,-1.83697019872103E-16));
#140440=DIRECTION('',(-0.767165151815303,-0.641449631569154,-2.58758337855511E-16));
#140441=DIRECTION('center_axis',(-1.83697019872103E-16,-1.83697019872101E-16,
1.));
#140442=DIRECTION('ref_axis',(-1.04634114423998E-14,-1.,-1.83697019872103E-16));
#140443=DIRECTION('',(-0.767165151815289,0.64144963156917,-2.30935664208844E-17));
#140444=DIRECTION('center_axis',(-1.83697019872103E-16,-1.83697019872101E-16,
1.));
#140445=DIRECTION('ref_axis',(1.04905870583987E-14,1.,1.83697019872103E-16));
#140446=DIRECTION('',(0.641449631569137,-0.767165151815317,-2.3093566420893E-17));
#140447=DIRECTION('',(-0.641449631569165,-0.767165151815294,-2.58758337855512E-16));
#140448=DIRECTION('center_axis',(0.767165151815294,-0.641449631569165,2.30935664208862E-17));
#140449=DIRECTION('ref_axis',(0.641449631569165,0.767165151815294,6.40920668176173E-34));
#140450=DIRECTION('',(-0.641449631569165,-0.767165151815294,0.));
#140451=DIRECTION('',(1.83697019872103E-16,1.83697019872101E-16,-1.));
#140452=DIRECTION('center_axis',(0.767165151815317,0.641449631569137,2.58758337855511E-16));
#140453=DIRECTION('ref_axis',(-0.641449631569137,0.767165151815317,1.60642344084382E-32));
#140454=DIRECTION('',(1.83697019872103E-16,1.83697019872101E-16,-1.));
#140455=DIRECTION('',(0.641449631569137,-0.767165151815317,0.));
#140456=DIRECTION('center_axis',(1.83697019872103E-16,1.83697019872101E-16,
-1.));
#140457=DIRECTION('ref_axis',(-1.,3.37445951098915E-32,-1.83697019872103E-16));
#140458=DIRECTION('',(1.83697019872103E-16,1.83697019872101E-16,-1.));
#140459=DIRECTION('center_axis',(0.,0.,1.));
#140460=DIRECTION('ref_axis',(1.,0.,0.));
#140461=DIRECTION('center_axis',(-0.64144963156917,-0.76716515181529,-2.58758337855512E-16));
#140462=DIRECTION('ref_axis',(0.76716515181529,-0.64144963156917,1.85826510350639E-32));
#140463=DIRECTION('',(1.83697019872103E-16,1.83697019872101E-16,-1.));
#140464=DIRECTION('',(-0.767165151815289,0.64144963156917,0.));
#140465=DIRECTION('center_axis',(1.83697019872103E-16,1.83697019872101E-16,
-1.));
#140466=DIRECTION('ref_axis',(-1.,3.37445951098914E-32,-1.83697019872103E-16));
#140467=DIRECTION('',(1.83697019872103E-16,1.83697019872101E-16,-1.));
#140468=DIRECTION('center_axis',(0.,0.,1.));
#140469=DIRECTION('ref_axis',(1.,0.,0.));
#140470=DIRECTION('center_axis',(0.641449631569154,-0.767165151815303,-2.30935664208871E-17));
#140471=DIRECTION('ref_axis',(0.767165151815303,0.641449631569154,7.36235815021269E-34));
#140472=DIRECTION('',(1.83697019872103E-16,1.83697019872101E-16,-1.));
#140473=DIRECTION('',(-0.767165151815303,-0.641449631569154,0.));
#140474=DIRECTION('center_axis',(1.83697019872103E-16,1.83697019872101E-16,
-1.));
#140475=DIRECTION('ref_axis',(-1.,3.37445951098915E-32,-1.83697019872103E-16));
#140476=DIRECTION('',(1.83697019872103E-16,1.83697019872101E-16,-1.));
#140477=DIRECTION('center_axis',(0.,0.,1.));
#140478=DIRECTION('ref_axis',(1.,0.,0.));
#140479=DIRECTION('center_axis',(-0.767165151815304,0.641449631569153,-2.30935664208902E-17));
#140480=DIRECTION('ref_axis',(-0.641449631569153,-0.767165151815304,1.00176035722907E-34));
#140481=DIRECTION('',(1.83697019872103E-16,1.83697019872101E-16,-1.));
#140482=DIRECTION('',(0.641449631569153,0.767165151815304,0.));
#140483=DIRECTION('center_axis',(1.83697019872103E-16,1.83697019872101E-16,
-1.));
#140484=DIRECTION('ref_axis',(1.,-1.22464679914735E-16,1.83697019872103E-16));
#140485=DIRECTION('',(1.83697019872103E-16,1.83697019872101E-16,-1.));
#140486=DIRECTION('center_axis',(0.,0.,1.));
#140487=DIRECTION('ref_axis',(1.,0.,0.));
#140488=DIRECTION('center_axis',(-0.767165151815307,-0.641449631569149,
-2.58758337855511E-16));
#140489=DIRECTION('ref_axis',(0.641449631569149,-0.767165151815307,1.72189280676572E-33));
#140490=DIRECTION('',(1.83697019872103E-16,1.83697019872101E-16,-1.));
#140491=DIRECTION('',(-0.641449631569149,0.767165151815307,0.));
#140492=DIRECTION('center_axis',(1.83697019872103E-16,1.83697019872101E-16,
-1.));
#140493=DIRECTION('ref_axis',(-1.,3.37445951098915E-32,-1.83697019872103E-16));
#140494=DIRECTION('',(1.83697019872103E-16,1.83697019872101E-16,-1.));
#140495=DIRECTION('center_axis',(0.,0.,1.));
#140496=DIRECTION('ref_axis',(1.,0.,0.));
#140497=DIRECTION('center_axis',(0.641449631569158,0.7671651518153,2.58758337855511E-16));
#140498=DIRECTION('ref_axis',(-0.7671651518153,0.641449631569158,3.71248381684349E-33));
#140499=DIRECTION('',(1.83697019872103E-16,1.83697019872101E-16,-1.));
#140500=DIRECTION('',(0.7671651518153,-0.641449631569157,0.));
#140501=DIRECTION('center_axis',(1.83697019872103E-16,1.83697019872101E-16,
-1.));
#140502=DIRECTION('ref_axis',(-1.,3.37445951098914E-32,-1.83697019872103E-16));
#140503=DIRECTION('',(1.83697019872103E-16,1.83697019872101E-16,-1.));
#140504=DIRECTION('center_axis',(0.,0.,1.));
#140505=DIRECTION('ref_axis',(1.,0.,0.));
#140506=DIRECTION('center_axis',(-0.641449631569142,0.767165151815313,2.30935664208913E-17));
#140507=DIRECTION('ref_axis',(-0.767165151815313,-0.641449631569142,-1.08468999085769E-33));
#140508=DIRECTION('',(1.83697019872103E-16,1.83697019872101E-16,-1.));
#140509=DIRECTION('',(0.767165151815313,0.641449631569142,0.));
#140510=DIRECTION('center_axis',(1.83697019872103E-16,1.83697019872101E-16,
-1.));
#140511=DIRECTION('ref_axis',(-1.,3.37445951098914E-32,-1.83697019872103E-16));
#140512=DIRECTION('center_axis',(0.,0.,1.));
#140513=DIRECTION('ref_axis',(1.,0.,0.));
#140514=DIRECTION('center_axis',(0.,0.,1.));
#140515=DIRECTION('ref_axis',(1.,0.,0.));
#140516=DIRECTION('center_axis',(0.,0.,-1.));
#140517=DIRECTION('ref_axis',(-1.,0.,0.));
#140518=DIRECTION('center_axis',(-1.83697019872103E-16,-1.83697019872101E-16,
1.));
#140519=DIRECTION('ref_axis',(1.15648231731787E-14,1.,1.83697019872103E-16));
#140520=DIRECTION('',(1.04744440165294E-14,1.,1.83697019872103E-16));
#140521=DIRECTION('center_axis',(-1.83697019872103E-16,-1.83697019872101E-16,
1.));
#140522=DIRECTION('ref_axis',(1.15648231731787E-14,1.,1.83697019872103E-16));
#140523=DIRECTION('',(-1.,1.04744440165294E-14,-1.83697019872101E-16));
#140524=DIRECTION('center_axis',(-1.83697019872103E-16,-1.83697019872101E-16,
1.));
#140525=DIRECTION('ref_axis',(1.15648231731787E-14,1.,1.83697019872103E-16));
#140526=DIRECTION('',(-8.90384784090525E-15,-1.,-1.83697019872103E-16));
#140527=DIRECTION('center_axis',(-1.83697019872103E-16,-1.83697019872101E-16,
1.));
#140528=DIRECTION('ref_axis',(1.15648231731787E-14,1.,1.83697019872103E-16));
#140529=DIRECTION('',(1.,-1.04744440165294E-14,1.83697019872101E-16));
#140530=DIRECTION('center_axis',(1.04744440165294E-14,1.,1.83697019872103E-16));
#140531=DIRECTION('ref_axis',(-1.,1.04744440165294E-14,0.));
#140532=DIRECTION('',(1.83697019872103E-16,1.83697019872101E-16,-1.));
#140533=DIRECTION('',(1.,-1.04744440165294E-14,0.));
#140534=DIRECTION('',(1.83697019872103E-16,1.83697019872101E-16,-1.));
#140535=DIRECTION('center_axis',(1.83697019872103E-16,1.83697019872101E-16,
-1.));
#140536=DIRECTION('ref_axis',(-1.,3.37445951098915E-32,-1.83697019872103E-16));
#140537=DIRECTION('',(1.83697019872103E-16,1.83697019872101E-16,-1.));
#140538=DIRECTION('center_axis',(0.,0.,1.));
#140539=DIRECTION('ref_axis',(1.,0.,0.));
#140540=DIRECTION('center_axis',(1.,-8.90384784090525E-15,1.83697019872101E-16));
#140541=DIRECTION('ref_axis',(8.90384784090525E-15,1.,1.26229010772883E-47));
#140542=DIRECTION('',(1.83697019872103E-16,1.83697019872101E-16,-1.));
#140543=DIRECTION('',(-8.90384784090525E-15,-1.,0.));
#140544=DIRECTION('center_axis',(1.83697019872103E-16,1.83697019872101E-16,
-1.));
#140545=DIRECTION('ref_axis',(-1.,3.37445951098915E-32,-1.83697019872103E-16));
#140546=DIRECTION('',(1.83697019872103E-16,1.83697019872101E-16,-1.));
#140547=DIRECTION('center_axis',(0.,0.,1.));
#140548=DIRECTION('ref_axis',(1.,0.,0.));
#140549=DIRECTION('center_axis',(-1.04744440165294E-14,-1.,-1.83697019872103E-16));
#140550=DIRECTION('ref_axis',(1.,-1.04744440165294E-14,0.));
#140551=DIRECTION('',(1.83697019872103E-16,1.83697019872101E-16,-1.));
#140552=DIRECTION('',(-1.,1.04744440165294E-14,0.));
#140553=DIRECTION('center_axis',(1.83697019872103E-16,1.83697019872101E-16,
-1.));
#140554=DIRECTION('ref_axis',(-1.,3.37445951098915E-32,-1.83697019872103E-16));
#140555=DIRECTION('',(1.83697019872103E-16,1.83697019872101E-16,-1.));
#140556=DIRECTION('center_axis',(0.,0.,1.));
#140557=DIRECTION('ref_axis',(1.,0.,0.));
#140558=DIRECTION('center_axis',(-1.,1.04744440165294E-14,-1.83697019872101E-16));
#140559=DIRECTION('ref_axis',(-1.04744440165294E-14,-1.,-1.01856090860782E-46));
#140560=DIRECTION('',(1.83697019872103E-16,1.83697019872101E-16,-1.));
#140561=DIRECTION('',(1.04744440165294E-14,1.,0.));
#140562=DIRECTION('center_axis',(1.83697019872103E-16,1.83697019872101E-16,
-1.));
#140563=DIRECTION('ref_axis',(-1.,3.37445951098915E-32,-1.83697019872103E-16));
#140564=DIRECTION('center_axis',(0.,0.,1.));
#140565=DIRECTION('ref_axis',(1.,0.,0.));
#140566=DIRECTION('center_axis',(0.,0.,1.));
#140567=DIRECTION('ref_axis',(1.,0.,0.));
#140568=DIRECTION('center_axis',(0.,0.,1.));
#140569=DIRECTION('ref_axis',(1.,0.,0.));
#140570=DIRECTION('center_axis',(0.,0.,-1.));
#140571=DIRECTION('ref_axis',(1.,0.,0.));
#140572=DIRECTION('',(1.28023872765816E-15,1.,0.));
#140573=DIRECTION('center_axis',(0.,0.,-1.));
#140574=DIRECTION('ref_axis',(1.,0.,0.));
#140575=DIRECTION('',(1.,0.,0.));
#140576=DIRECTION('center_axis',(0.,0.,1.));
#140577=DIRECTION('ref_axis',(1.,0.,0.));
#140578=DIRECTION('',(0.707106781186549,0.707106781186546,0.));
#140579=DIRECTION('center_axis',(0.,0.,-1.));
#140580=DIRECTION('ref_axis',(1.,-5.13992141030166E-15,0.));
#140581=DIRECTION('',(1.,5.01365166467286E-16,0.));
#140582=DIRECTION('',(0.707106781186547,0.707106781186547,0.));
#140583=DIRECTION('',(7.80891617653129E-15,1.,0.));
#140584=DIRECTION('center_axis',(0.,0.,-1.));
#140585=DIRECTION('ref_axis',(1.,5.13992141030166E-15,0.));
#140586=DIRECTION('',(0.707106781186551,0.707106781186544,0.));
#140587=DIRECTION('center_axis',(0.,0.,1.));
#140588=DIRECTION('ref_axis',(1.,0.,0.));
#140589=DIRECTION('',(7.66554070360109E-15,1.,0.));
#140590=DIRECTION('center_axis',(0.,0.,-1.));
#140591=DIRECTION('ref_axis',(1.,0.,0.));
#140592=DIRECTION('',(1.,-5.12095491063264E-15,0.));
#140593=DIRECTION('center_axis',(0.,0.,-1.));
#140594=DIRECTION('ref_axis',(1.,1.54197642309049E-14,0.));
#140595=DIRECTION('',(-3.49148133884313E-15,-1.,0.));
#140596=DIRECTION('center_axis',(0.,0.,1.));
#140597=DIRECTION('ref_axis',(1.,0.,0.));
#140598=DIRECTION('',(0.707106781186544,-0.707106781186551,0.));
#140599=DIRECTION('center_axis',(0.,0.,-1.));
#140600=DIRECTION('ref_axis',(1.,-2.56996070515083E-15,0.));
#140601=DIRECTION('',(-2.99011617237585E-15,-1.,0.));
#140602=DIRECTION('',(0.707106781186545,-0.70710678118655,0.));
#140603=DIRECTION('',(1.,-1.13003975153744E-14,0.));
#140604=DIRECTION('center_axis',(0.,0.,-1.));
#140605=DIRECTION('ref_axis',(1.,3.85494105772625E-15,0.));
#140606=DIRECTION('',(0.707106781186541,-0.707106781186554,0.));
#140607=DIRECTION('center_axis',(0.,0.,1.));
#140608=DIRECTION('ref_axis',(1.,0.,0.));
#140609=DIRECTION('',(1.,-1.11570220424442E-14,0.));
#140610=DIRECTION('center_axis',(0.,0.,-1.));
#140611=DIRECTION('ref_axis',(1.,3.91919007535501E-14,0.));
#140612=DIRECTION('',(-8.61243624947577E-15,-1.,0.));
#140613=DIRECTION('center_axis',(0.,0.,-1.));
#140614=DIRECTION('ref_axis',(1.,0.,0.));
#140615=DIRECTION('',(-1.,0.,0.));
#140616=DIRECTION('center_axis',(0.,0.,1.));
#140617=DIRECTION('ref_axis',(1.,0.,0.));
#140618=DIRECTION('',(-0.707106781186549,-0.707106781186546,0.));
#140619=DIRECTION('center_axis',(0.,0.,-1.));
#140620=DIRECTION('ref_axis',(1.,6.42490176287708E-16,0.));
#140621=DIRECTION('',(-1.,-5.01365166467286E-16,0.));
#140622=DIRECTION('',(-0.707106781186547,-0.707106781186547,0.));
#140623=DIRECTION('',(-7.80891617653129E-15,-1.,0.));
#140624=DIRECTION('center_axis',(0.,0.,-1.));
#140625=DIRECTION('ref_axis',(1.,-1.02798428206033E-14,0.));
#140626=DIRECTION('',(-0.707106781186551,-0.707106781186544,0.));
#140627=DIRECTION('center_axis',(0.,0.,1.));
#140628=DIRECTION('ref_axis',(1.,0.,0.));
#140629=DIRECTION('',(-7.66554070360109E-15,-1.,0.));
#140630=DIRECTION('center_axis',(0.,0.,-1.));
#140631=DIRECTION('ref_axis',(1.,-7.70988211545247E-15,0.));
#140632=DIRECTION('',(-1.,5.12095491063264E-15,0.));
#140633=DIRECTION('center_axis',(0.,0.,-1.));
#140634=DIRECTION('ref_axis',(1.,0.,0.));
#140635=DIRECTION('',(1.04744440165294E-14,1.,0.));
#140636=DIRECTION('center_axis',(0.,0.,1.));
#140637=DIRECTION('ref_axis',(1.,0.,0.));
#140638=DIRECTION('',(-0.707106781186539,0.707106781186556,0.));
#140639=DIRECTION('center_axis',(0.,0.,-1.));
#140640=DIRECTION('ref_axis',(1.,2.56996070515083E-15,0.));
#140641=DIRECTION('',(9.97307885006211E-15,1.,0.));
#140642=DIRECTION('',(-0.70710678118654,0.707106781186555,0.));
#140643=DIRECTION('',(-1.,1.82833601930607E-14,0.));
#140644=DIRECTION('center_axis',(0.,0.,-1.));
#140645=DIRECTION('ref_axis',(1.,6.42490176287708E-16,0.));
#140646=DIRECTION('',(-0.707106781186536,0.707106781186559,0.));
#140647=DIRECTION('center_axis',(0.,0.,1.));
#140648=DIRECTION('ref_axis',(1.,0.,0.));
#140649=DIRECTION('',(-1.,1.81399847201305E-14,0.));
#140650=DIRECTION('center_axis',(0.,0.,-1.));
#140651=DIRECTION('ref_axis',(-1.,0.,0.));
#140652=DIRECTION('center_axis',(0.,0.,-1.));
#140653=DIRECTION('ref_axis',(-1.,0.,0.));
#140654=DIRECTION('',(1.28023872765816E-15,1.,0.));
#140655=DIRECTION('center_axis',(1.83697019872103E-16,1.83697019872101E-16,
-1.));
#140656=DIRECTION('ref_axis',(1.02798428206033E-14,1.,1.83697019872103E-16));
#140657=DIRECTION('',(-1.,1.81399847201305E-14,-1.836970198721E-16));
#140658=DIRECTION('center_axis',(-1.83697019872103E-16,-1.83697019872101E-16,
1.));
#140659=DIRECTION('ref_axis',(-1.02798428206033E-14,-1.,-1.83697019872103E-16));
#140660=DIRECTION('',(-0.707106781186536,0.707106781186559,2.81031697484985E-30));
#140661=DIRECTION('center_axis',(1.83697019872103E-16,1.83697019872101E-16,
-1.));
#140662=DIRECTION('ref_axis',(1.02798428206033E-14,1.,1.83697019872103E-16));
#140663=DIRECTION('',(-1.,1.82833601930607E-14,-1.836970198721E-16));
#140664=DIRECTION('',(-0.70710678118654,0.707106781186555,1.35585468084861E-30));
#140665=DIRECTION('',(9.97307885006212E-15,1.,1.83697019872103E-16));
#140666=DIRECTION('center_axis',(1.83697019872103E-16,1.83697019872101E-16,
-1.));
#140667=DIRECTION('ref_axis',(-1.02798428206033E-14,-1.,-1.83697019872103E-16));
#140668=DIRECTION('',(-0.707106781186539,0.707106781186556,1.75028513345912E-30));
#140669=DIRECTION('center_axis',(-1.83697019872103E-16,-1.83697019872101E-16,
1.));
#140670=DIRECTION('ref_axis',(1.02798428206033E-14,1.,1.83697019872103E-16));
#140671=DIRECTION('',(1.04744440165294E-14,1.,1.83697019872103E-16));
#140672=DIRECTION('center_axis',(1.83697019872103E-16,1.83697019872101E-16,
-1.));
#140673=DIRECTION('ref_axis',(-1.06010879087472E-14,-1.,-1.83697019872103E-16));
#140674=DIRECTION('',(-1.,5.12095491063264E-15,1.88140831196526E-30));
#140675=DIRECTION('center_axis',(0.,3.67394039744206E-16,-1.));
#140676=DIRECTION('ref_axis',(-1.,0.,0.));
#140677=DIRECTION('',(-7.6655407036011E-15,-1.,-3.67394039744206E-16));
#140678=DIRECTION('center_axis',(0.,-3.67394039744206E-16,1.));
#140679=DIRECTION('ref_axis',(1.,0.,0.));
#140680=DIRECTION('',(-0.707106781186551,-0.707106781186544,-2.59786816870647E-16));
#140681=DIRECTION('center_axis',(0.,3.67394039744206E-16,-1.));
#140682=DIRECTION('ref_axis',(-1.,0.,0.));
#140683=DIRECTION('',(-7.80891617653129E-15,-1.,-3.67394039744206E-16));
#140684=DIRECTION('',(-0.707106781186547,-0.707106781186547,-2.59786816870648E-16));
#140685=DIRECTION('',(-1.,-5.01365166467286E-16,-1.84198573895442E-31));
#140686=DIRECTION('center_axis',(0.,3.67394039744206E-16,-1.));
#140687=DIRECTION('ref_axis',(1.,0.,0.));
#140688=DIRECTION('',(-0.707106781186549,-0.707106781186546,-2.59786816870648E-16));
#140689=DIRECTION('center_axis',(0.,-3.67394039744206E-16,1.));
#140690=DIRECTION('ref_axis',(-1.,0.,0.));
#140691=DIRECTION('',(-1.,0.,0.));
#140692=DIRECTION('center_axis',(0.,3.67394039744206E-16,-1.));
#140693=DIRECTION('ref_axis',(1.,0.,0.));
#140694=DIRECTION('',(-8.61243624947577E-15,-1.,-1.83697019872102E-16));
#140695=DIRECTION('center_axis',(-1.83697019872103E-16,1.83697019872104E-16,
-1.));
#140696=DIRECTION('ref_axis',(-2.56996070515082E-15,-1.,-1.83697019872103E-16));
#140697=DIRECTION('',(1.,-1.11570220424442E-14,-1.83697019872105E-16));
#140698=DIRECTION('center_axis',(1.83697019872103E-16,-1.83697019872104E-16,
1.));
#140699=DIRECTION('ref_axis',(2.56996070515083E-15,1.,1.83697019872103E-16));
#140700=DIRECTION('',(0.707106781186541,-0.707106781186554,-2.59786816870648E-16));
#140701=DIRECTION('center_axis',(-1.83697019872103E-16,1.83697019872104E-16,
-1.));
#140702=DIRECTION('ref_axis',(-2.56996070515083E-15,-1.,-1.83697019872103E-16));
#140703=DIRECTION('',(1.,-1.13003975153744E-14,-1.83697019872105E-16));
#140704=DIRECTION('',(0.707106781186545,-0.70710678118655,-2.59786816870648E-16));
#140705=DIRECTION('',(-2.99011617237585E-15,-1.,-1.83697019872103E-16));
#140706=DIRECTION('center_axis',(-1.83697019872103E-16,1.83697019872104E-16,
-1.));
#140707=DIRECTION('ref_axis',(3.21245088143854E-15,1.,1.83697019872103E-16));
#140708=DIRECTION('',(0.707106781186544,-0.707106781186551,-2.59786816870649E-16));
#140709=DIRECTION('center_axis',(1.83697019872103E-16,-1.83697019872104E-16,
1.));
#140710=DIRECTION('ref_axis',(-3.21245088143853E-15,-1.,-1.83697019872103E-16));
#140711=DIRECTION('',(-3.49148133884313E-15,-1.,-1.83697019872103E-16));
#140712=DIRECTION('center_axis',(-1.83697019872103E-16,1.83697019872104E-16,
-1.));
#140713=DIRECTION('ref_axis',(3.53369596958238E-15,1.,1.83697019872103E-16));
#140714=DIRECTION('',(1.,-5.12095491063264E-15,0.));
#140715=DIRECTION('center_axis',(0.,0.,-1.));
#140716=DIRECTION('ref_axis',(1.,0.,0.));
#140717=DIRECTION('',(7.6655407036011E-15,1.,0.));
#140718=DIRECTION('center_axis',(0.,0.,1.));
#140719=DIRECTION('ref_axis',(-1.,0.,0.));
#140720=DIRECTION('',(0.707106781186551,0.707106781186544,0.));
#140721=DIRECTION('center_axis',(0.,0.,-1.));
#140722=DIRECTION('ref_axis',(1.,0.,0.));
#140723=DIRECTION('',(7.80891617653129E-15,1.,0.));
#140724=DIRECTION('',(0.707106781186547,0.707106781186547,0.));
#140725=DIRECTION('',(1.,5.01365166467286E-16,0.));
#140726=DIRECTION('center_axis',(0.,0.,-1.));
#140727=DIRECTION('ref_axis',(-1.,0.,0.));
#140728=DIRECTION('',(0.707106781186549,0.707106781186546,0.));
#140729=DIRECTION('center_axis',(0.,0.,1.));
#140730=DIRECTION('ref_axis',(1.,0.,0.));
#140731=DIRECTION('',(1.,0.,0.));
#140732=DIRECTION('center_axis',(1.83697019872103E-16,1.83697019872101E-16,
-1.));
#140733=DIRECTION('ref_axis',(-1.,3.37445951098915E-32,-1.83697019872103E-16));
#140734=DIRECTION('',(1.83697019872103E-16,1.83697019872101E-16,-1.));
#140735=DIRECTION('',(1.83697019872103E-16,1.83697019872101E-16,-1.));
#140736=DIRECTION('center_axis',(-1.81399847201305E-14,-1.,-1.83697019872104E-16));
#140737=DIRECTION('ref_axis',(1.,-1.81399847201305E-14,0.));
#140738=DIRECTION('',(1.83697019872103E-16,1.83697019872101E-16,-1.));
#140739=DIRECTION('center_axis',(1.83697019872103E-16,1.83697019872101E-16,
-1.));
#140740=DIRECTION('ref_axis',(-1.,3.37445951098915E-32,-1.83697019872103E-16));
#140741=DIRECTION('',(1.83697019872103E-16,1.83697019872101E-16,-1.));
#140742=DIRECTION('center_axis',(-0.707106781186559,-0.707106781186536,
-2.59786816870647E-16));
#140743=DIRECTION('ref_axis',(0.707106781186536,-0.707106781186559,-8.51191961352541E-33));
#140744=DIRECTION('',(1.83697019872103E-16,1.83697019872101E-16,-1.));
#140745=DIRECTION('center_axis',(1.83697019872103E-16,1.83697019872101E-16,
-1.));
#140746=DIRECTION('ref_axis',(-1.,3.37445951098915E-32,-1.83697019872103E-16));
#140747=DIRECTION('',(1.83697019872103E-16,1.83697019872101E-16,-1.));
#140748=DIRECTION('center_axis',(-1.82833601930607E-14,-1.,-1.83697019872104E-16));
#140749=DIRECTION('ref_axis',(1.,-1.82833601930607E-14,0.));
#140750=DIRECTION('',(1.83697019872103E-16,1.83697019872101E-16,-1.));
#140751=DIRECTION('center_axis',(-0.707106781186555,-0.70710678118654,-2.59786816870647E-16));
#140752=DIRECTION('ref_axis',(0.70710678118654,-0.707106781186555,3.77583739123461E-33));
#140753=DIRECTION('',(1.83697019872103E-16,1.83697019872101E-16,-1.));
#140754=DIRECTION('center_axis',(-1.,9.97307885006211E-15,-1.83697019872101E-16));
#140755=DIRECTION('ref_axis',(-9.97307885006211E-15,-1.,7.95933057668596E-47));
#140756=DIRECTION('',(1.83697019872103E-16,1.83697019872101E-16,-1.));
#140757=DIRECTION('center_axis',(1.83697019872103E-16,1.83697019872101E-16,
-1.));
#140758=DIRECTION('ref_axis',(-1.,3.37445951098915E-32,-1.83697019872103E-16));
#140759=DIRECTION('',(1.83697019872103E-16,1.83697019872101E-16,-1.));
#140760=DIRECTION('center_axis',(-0.707106781186556,-0.707106781186539,
-2.59786816870647E-16));
#140761=DIRECTION('ref_axis',(0.707106781186539,-0.707106781186556,1.19724503022165E-32));
#140762=DIRECTION('',(1.83697019872103E-16,1.83697019872101E-16,-1.));
#140763=DIRECTION('center_axis',(1.83697019872103E-16,1.83697019872101E-16,
-1.));
#140764=DIRECTION('ref_axis',(-1.,3.37445951098914E-32,-1.83697019872103E-16));
#140765=DIRECTION('',(1.83697019872103E-16,1.83697019872101E-16,-1.));
#140766=DIRECTION('center_axis',(-1.,1.04744440165294E-14,-1.83697019872101E-16));
#140767=DIRECTION('ref_axis',(-1.04744440165294E-14,-1.,-1.01856090860782E-46));
#140768=DIRECTION('',(1.83697019872103E-16,1.83697019872101E-16,-1.));
#140769=DIRECTION('center_axis',(1.83697019872103E-16,1.83697019872101E-16,
-1.));
#140770=DIRECTION('ref_axis',(-1.,3.37445951098915E-32,-1.83697019872103E-16));
#140771=DIRECTION('',(1.83697019872103E-16,1.83697019872101E-16,-1.));
#140772=DIRECTION('center_axis',(-5.12095491063264E-15,-1.,-3.67394039744206E-16));
#140773=DIRECTION('ref_axis',(1.,-5.12095491063264E-15,0.));
#140774=DIRECTION('',(0.,3.67394039744206E-16,-1.));
#140775=DIRECTION('center_axis',(0.,3.67394039744206E-16,-1.));
#140776=DIRECTION('ref_axis',(0.,1.,3.67394039744206E-16));
#140777=DIRECTION('',(0.,3.67394039744206E-16,-1.));
#140778=DIRECTION('center_axis',(1.,-7.66554070360109E-15,-2.81627396591965E-30));
#140779=DIRECTION('ref_axis',(7.66554070360109E-15,1.,1.20244003954024E-60));
#140780=DIRECTION('',(0.,3.67394039744206E-16,-1.));
#140781=DIRECTION('center_axis',(0.,3.67394039744206E-16,-1.));
#140782=DIRECTION('ref_axis',(0.,1.,3.67394039744206E-16));
#140783=DIRECTION('',(0.,3.67394039744206E-16,-1.));
#140784=DIRECTION('center_axis',(0.707106781186544,-0.707106781186552,-2.59786816870649E-16));
#140785=DIRECTION('ref_axis',(0.707106781186552,0.707106781186544,1.54452889108689E-32));
#140786=DIRECTION('',(0.,3.67394039744206E-16,-1.));
#140787=DIRECTION('center_axis',(0.,3.67394039744206E-16,-1.));
#140788=DIRECTION('ref_axis',(0.,1.,3.67394039744206E-16));
#140789=DIRECTION('',(0.,3.67394039744206E-16,-1.));
#140790=DIRECTION('center_axis',(1.,-7.80891617653129E-15,-2.86894926011971E-30));
#140791=DIRECTION('ref_axis',(7.80891617653129E-15,1.,1.38445973011545E-61));
#140792=DIRECTION('',(0.,3.67394039744206E-16,-1.));
#140793=DIRECTION('center_axis',(0.707106781186548,-0.707106781186548,-2.59786816870648E-16));
#140794=DIRECTION('ref_axis',(0.707106781186548,0.707106781186548,-1.22182752772918E-34));
#140795=DIRECTION('',(0.,3.67394039744206E-16,-1.));
#140796=DIRECTION('center_axis',(5.01365166467286E-16,-1.,-3.67394039744206E-16));
#140797=DIRECTION('ref_axis',(1.,5.01365166467286E-16,0.));
#140798=DIRECTION('',(0.,3.67394039744206E-16,-1.));
#140799=DIRECTION('center_axis',(0.,3.67394039744206E-16,-1.));
#140800=DIRECTION('ref_axis',(0.,1.,3.67394039744206E-16));
#140801=DIRECTION('',(0.,3.67394039744206E-16,-1.));
#140802=DIRECTION('center_axis',(0.707106781186546,-0.707106781186549,-2.59786816870648E-16));
#140803=DIRECTION('ref_axis',(0.707106781186549,0.707106781186546,3.35953521571076E-33));
#140804=DIRECTION('',(0.,3.67394039744206E-16,-1.));
#140805=DIRECTION('center_axis',(0.,3.67394039744206E-16,-1.));
#140806=DIRECTION('ref_axis',(0.,1.,3.67394039744206E-16));
#140807=DIRECTION('',(0.,3.67394039744206E-16,-1.));
#140808=DIRECTION('center_axis',(0.,-1.,-3.67394039744206E-16));
#140809=DIRECTION('ref_axis',(0.,3.67394039744206E-16,-1.));
#140810=DIRECTION('',(0.,3.67394039744206E-16,-1.));
#140811=DIRECTION('center_axis',(0.,3.67394039744206E-16,-1.));
#140812=DIRECTION('ref_axis',(0.,1.,3.67394039744206E-16));
#140813=DIRECTION('',(0.,3.67394039744206E-16,-1.));
#140814=DIRECTION('center_axis',(1.,-8.61243624947577E-15,-1.83697019872105E-16));
#140815=DIRECTION('ref_axis',(8.61243624947577E-15,1.,7.69347343280275E-47));
#140816=DIRECTION('',(-1.83697019872103E-16,1.83697019872104E-16,-1.));
#140817=DIRECTION('center_axis',(-1.83697019872103E-16,1.83697019872104E-16,
-1.));
#140818=DIRECTION('ref_axis',(3.37445951098919E-32,1.,1.83697019872104E-16));
#140819=DIRECTION('',(-1.83697019872103E-16,1.83697019872104E-16,-1.));
#140820=DIRECTION('center_axis',(1.11570220424442E-14,1.,1.83697019872102E-16));
#140821=DIRECTION('ref_axis',(-1.,1.11570220424442E-14,0.));
#140822=DIRECTION('',(-1.83697019872103E-16,1.83697019872104E-16,-1.));
#140823=DIRECTION('center_axis',(-1.83697019872103E-16,1.83697019872104E-16,
-1.));
#140824=DIRECTION('ref_axis',(3.37445951098919E-32,1.,1.83697019872104E-16));
#140825=DIRECTION('',(-1.83697019872103E-16,1.83697019872104E-16,-1.));
#140826=DIRECTION('center_axis',(0.707106781186554,0.707106781186541,-1.89630025293512E-30));
#140827=DIRECTION('ref_axis',(-0.707106781186541,0.707106781186554,6.79668681715311E-48));
#140828=DIRECTION('',(-1.83697019872103E-16,1.83697019872104E-16,-1.));
#140829=DIRECTION('center_axis',(-1.83697019872103E-16,1.83697019872104E-16,
-1.));
#140830=DIRECTION('ref_axis',(3.37445951098919E-32,1.,1.83697019872104E-16));
#140831=DIRECTION('',(-1.83697019872103E-16,1.83697019872104E-16,-1.));
#140832=DIRECTION('center_axis',(1.13003975153744E-14,1.,1.83697019872102E-16));
#140833=DIRECTION('ref_axis',(-1.,1.13003975153744E-14,0.));
#140834=DIRECTION('',(-1.83697019872103E-16,1.83697019872104E-16,-1.));
#140835=DIRECTION('center_axis',(0.70710678118655,0.707106781186545,-4.36149058175078E-31));
#140836=DIRECTION('ref_axis',(-0.707106781186545,0.70710678118655,-2.09609619079153E-48));
#140837=DIRECTION('',(-1.83697019872103E-16,1.83697019872104E-16,-1.));
#140838=DIRECTION('center_axis',(1.,-2.99011617237585E-15,-1.83697019872104E-16));
#140839=DIRECTION('ref_axis',(2.99011617237585E-15,1.,-2.91458608578564E-48));
#140840=DIRECTION('',(-1.83697019872103E-16,1.83697019872104E-16,-1.));
#140841=DIRECTION('center_axis',(-1.83697019872103E-16,1.83697019872104E-16,
-1.));
#140842=DIRECTION('ref_axis',(3.37445951098919E-32,1.,1.83697019872104E-16));
#140843=DIRECTION('',(-1.83697019872103E-16,1.83697019872104E-16,-1.));
#140844=DIRECTION('center_axis',(0.707106781186551,0.707106781186544,-8.34372111291455E-31));
#140845=DIRECTION('ref_axis',(-0.707106781186544,0.707106781186551,-4.97404528384751E-47));
#140846=DIRECTION('',(-1.83697019872103E-16,1.83697019872104E-16,-1.));
#140847=DIRECTION('center_axis',(-1.83697019872103E-16,1.83697019872104E-16,
-1.));
#140848=DIRECTION('ref_axis',(3.37445951098919E-32,1.,1.83697019872104E-16));
#140849=DIRECTION('',(-1.83697019872103E-16,1.83697019872104E-16,-1.));
#140850=DIRECTION('center_axis',(1.,-3.49148133884313E-15,-1.83697019872104E-16));
#140851=DIRECTION('ref_axis',(3.49148133884313E-15,1.,-1.78914547131776E-47));
#140852=DIRECTION('',(-1.83697019872103E-16,1.83697019872104E-16,-1.));
#140853=DIRECTION('center_axis',(-1.83697019872103E-16,1.83697019872104E-16,
-1.));
#140854=DIRECTION('ref_axis',(3.37445951098919E-32,1.,1.83697019872104E-16));
#140855=DIRECTION('',(-1.83697019872103E-16,1.83697019872104E-16,-1.));
#140856=DIRECTION('center_axis',(5.12095491063264E-15,1.,0.));
#140857=DIRECTION('ref_axis',(-1.,5.12095491063264E-15,0.));
#140858=DIRECTION('',(0.,0.,-1.));
#140859=DIRECTION('center_axis',(0.,0.,-1.));
#140860=DIRECTION('ref_axis',(-1.,0.,0.));
#140861=DIRECTION('',(0.,0.,-1.));
#140862=DIRECTION('center_axis',(-1.,7.66554070360109E-15,0.));
#140863=DIRECTION('ref_axis',(-7.66554070360109E-15,-1.,0.));
#140864=DIRECTION('',(0.,0.,-1.));
#140865=DIRECTION('center_axis',(0.,0.,-1.));
#140866=DIRECTION('ref_axis',(-1.,0.,0.));
#140867=DIRECTION('',(0.,0.,-1.));
#140868=DIRECTION('center_axis',(-0.707106781186544,0.707106781186552,0.));
#140869=DIRECTION('ref_axis',(-0.707106781186552,-0.707106781186544,0.));
#140870=DIRECTION('',(0.,0.,-1.));
#140871=DIRECTION('center_axis',(0.,0.,-1.));
#140872=DIRECTION('ref_axis',(-1.,0.,0.));
#140873=DIRECTION('',(0.,0.,-1.));
#140874=DIRECTION('center_axis',(-1.,7.80891617653129E-15,0.));
#140875=DIRECTION('ref_axis',(-7.80891617653129E-15,-1.,0.));
#140876=DIRECTION('',(0.,0.,-1.));
#140877=DIRECTION('center_axis',(-0.707106781186548,0.707106781186548,0.));
#140878=DIRECTION('ref_axis',(-0.707106781186548,-0.707106781186548,0.));
#140879=DIRECTION('',(0.,0.,-1.));
#140880=DIRECTION('center_axis',(-5.01365166467286E-16,1.,0.));
#140881=DIRECTION('ref_axis',(-1.,-5.01365166467286E-16,0.));
#140882=DIRECTION('',(0.,0.,-1.));
#140883=DIRECTION('center_axis',(0.,0.,-1.));
#140884=DIRECTION('ref_axis',(-1.,0.,0.));
#140885=DIRECTION('',(0.,0.,-1.));
#140886=DIRECTION('center_axis',(-0.707106781186546,0.707106781186549,0.));
#140887=DIRECTION('ref_axis',(-0.707106781186549,-0.707106781186546,0.));
#140888=DIRECTION('',(0.,0.,-1.));
#140889=DIRECTION('center_axis',(0.,0.,-1.));
#140890=DIRECTION('ref_axis',(-1.,0.,0.));
#140891=DIRECTION('',(0.,0.,-1.));
#140892=DIRECTION('center_axis',(0.,1.,0.));
#140893=DIRECTION('ref_axis',(0.,0.,1.));
#140894=DIRECTION('',(0.,0.,-1.));
#140895=DIRECTION('center_axis',(0.,0.,-1.));
#140896=DIRECTION('ref_axis',(-1.,0.,0.));
#140897=DIRECTION('',(0.,0.,-1.));
#140898=DIRECTION('center_axis',(-1.,1.28023872765816E-15,0.));
#140899=DIRECTION('ref_axis',(-1.28023872765816E-15,-1.,0.));
#140900=DIRECTION('center_axis',(0.,3.67394039744206E-16,-1.));
#140901=DIRECTION('ref_axis',(0.,1.,3.67394039744206E-16));
#140902=DIRECTION('center_axis',(0.,0.,1.));
#140903=DIRECTION('ref_axis',(1.,0.,0.));
#140904=DIRECTION('',(0.,3.67394039744206E-16,-1.));
#140905=DIRECTION('center_axis',(0.,-3.67394039744206E-16,1.));
#140906=DIRECTION('ref_axis',(1.,0.,0.));
#140907=DIRECTION('',(0.,3.67394039744206E-16,-1.));
#140908=DIRECTION('center_axis',(0.,0.,-1.));
#140909=DIRECTION('ref_axis',(-1.,0.,0.));
#140910=DIRECTION('center_axis',(0.,-3.67394039744206E-16,1.));
#140911=DIRECTION('ref_axis',(-1.,0.,0.));
#140912=DIRECTION('',(-0.64144963156915,0.767165151815307,2.81851904276403E-16));
#140913=DIRECTION('center_axis',(0.,-3.67394039744206E-16,1.));
#140914=DIRECTION('ref_axis',(1.,0.,0.));
#140915=DIRECTION('',(0.641449631569149,0.767165151815306,2.81851904276403E-16));
#140916=DIRECTION('center_axis',(0.,-3.67394039744206E-16,1.));
#140917=DIRECTION('ref_axis',(1.,0.,0.));
#140918=DIRECTION('',(-0.767165151815301,-0.641449631569157,-2.35664771434625E-16));
#140919=DIRECTION('',(-0.767165151815311,0.641449631569145,2.35664771434621E-16));
#140920=DIRECTION('center_axis',(0.,-3.67394039744206E-16,1.));
#140921=DIRECTION('ref_axis',(1.,0.,0.));
#140922=DIRECTION('',(0.641449631569162,-0.767165151815296,-2.81851904276399E-16));
#140923=DIRECTION('center_axis',(0.,-3.67394039744206E-16,1.));
#140924=DIRECTION('ref_axis',(1.,0.,0.));
#140925=DIRECTION('',(-0.641449631569162,-0.767165151815296,-2.81851904276399E-16));
#140926=DIRECTION('center_axis',(0.,-3.67394039744206E-16,1.));
#140927=DIRECTION('ref_axis',(-1.,0.,0.));
#140928=DIRECTION('',(0.767165151815311,0.641449631569145,2.35664771434621E-16));
#140929=DIRECTION('center_axis',(0.,-3.67394039744206E-16,1.));
#140930=DIRECTION('ref_axis',(-1.,0.,0.));
#140931=DIRECTION('',(0.767165151815301,-0.641449631569157,-2.35664771434625E-16));
#140932=DIRECTION('center_axis',(0.641449631569157,0.767165151815301,2.818519042764E-16));
#140933=DIRECTION('ref_axis',(-0.767165151815301,0.641449631569157,-1.55481997605168E-32));
#140934=DIRECTION('',(0.,3.67394039744206E-16,-1.));
#140935=DIRECTION('',(0.767165151815301,-0.641449631569157,0.));
#140936=DIRECTION('',(0.,3.67394039744206E-16,-1.));
#140937=DIRECTION('center_axis',(0.,3.67394039744206E-16,-1.));
#140938=DIRECTION('ref_axis',(-1.96623899133175E-14,-1.,-3.67394039744206E-16));
#140939=DIRECTION('',(0.,3.67394039744206E-16,-1.));
#140940=DIRECTION('center_axis',(0.,0.,1.));
#140941=DIRECTION('ref_axis',(1.,0.,0.));
#140942=DIRECTION('center_axis',(-0.641449631569145,0.767165151815311,2.81851904276404E-16));
#140943=DIRECTION('ref_axis',(-0.767165151815311,-0.641449631569145,-2.53982072604054E-32));
#140944=DIRECTION('',(0.,3.67394039744206E-16,-1.));
#140945=DIRECTION('',(0.767165151815311,0.641449631569145,0.));
#140946=DIRECTION('center_axis',(0.,3.67394039744206E-16,-1.));
#140947=DIRECTION('ref_axis',(0.,1.,3.67394039744206E-16));
#140948=DIRECTION('',(0.,3.67394039744206E-16,-1.));
#140949=DIRECTION('center_axis',(0.,0.,1.));
#140950=DIRECTION('ref_axis',(1.,0.,0.));
#140951=DIRECTION('center_axis',(0.767165151815296,-0.641449631569162,-2.35664771434627E-16));
#140952=DIRECTION('ref_axis',(0.641449631569162,0.767165151815296,-1.58791937441479E-33));
#140953=DIRECTION('',(0.,3.67394039744206E-16,-1.));
#140954=DIRECTION('',(-0.641449631569162,-0.767165151815296,0.));
#140955=DIRECTION('center_axis',(0.,3.67394039744206E-16,-1.));
#140956=DIRECTION('ref_axis',(0.,1.,3.67394039744206E-16));
#140957=DIRECTION('',(0.,3.67394039744206E-16,-1.));
#140958=DIRECTION('center_axis',(0.,0.,1.));
#140959=DIRECTION('ref_axis',(1.,0.,0.));
#140960=DIRECTION('center_axis',(0.767165151815296,0.641449631569162,2.35664771434627E-16));
#140961=DIRECTION('ref_axis',(-0.641449631569162,0.767165151815296,-1.58791937441479E-33));
#140962=DIRECTION('',(0.,3.67394039744206E-16,-1.));
#140963=DIRECTION('',(0.641449631569162,-0.767165151815296,0.));
#140964=DIRECTION('center_axis',(0.,3.67394039744206E-16,-1.));
#140965=DIRECTION('ref_axis',(0.,1.,3.67394039744206E-16));
#140966=DIRECTION('',(0.,3.67394039744206E-16,-1.));
#140967=DIRECTION('center_axis',(0.,0.,1.));
#140968=DIRECTION('ref_axis',(1.,0.,0.));
#140969=DIRECTION('center_axis',(-0.641449631569145,-0.767165151815311,
-2.81851904276404E-16));
#140970=DIRECTION('ref_axis',(0.767165151815311,-0.641449631569145,-2.53982072604054E-32));
#140971=DIRECTION('',(-0.767165151815311,0.641449631569145,0.));
#140972=DIRECTION('center_axis',(0.641449631569157,-0.767165151815301,-2.818519042764E-16));
#140973=DIRECTION('ref_axis',(0.767165151815301,0.641449631569157,-1.55481997605168E-32));
#140974=DIRECTION('',(0.,3.67394039744206E-16,-1.));
#140975=DIRECTION('',(-0.767165151815301,-0.641449631569157,0.));
#140976=DIRECTION('center_axis',(0.,3.67394039744206E-16,-1.));
#140977=DIRECTION('ref_axis',(0.,1.,3.67394039744206E-16));
#140978=DIRECTION('',(0.,3.67394039744206E-16,-1.));
#140979=DIRECTION('center_axis',(0.,0.,1.));
#140980=DIRECTION('ref_axis',(1.,0.,0.));
#140981=DIRECTION('center_axis',(-0.767165151815307,0.64144963156915,2.35664771434622E-16));
#140982=DIRECTION('ref_axis',(-0.64144963156915,-0.767165151815306,6.82549510605368E-34));
#140983=DIRECTION('',(0.,3.67394039744206E-16,-1.));
#140984=DIRECTION('',(0.641449631569149,0.767165151815306,0.));
#140985=DIRECTION('center_axis',(0.,3.67394039744206E-16,-1.));
#140986=DIRECTION('ref_axis',(0.,1.,3.67394039744206E-16));
#140987=DIRECTION('',(0.,3.67394039744206E-16,-1.));
#140988=DIRECTION('center_axis',(0.,0.,1.));
#140989=DIRECTION('ref_axis',(1.,0.,0.));
#140990=DIRECTION('center_axis',(-0.767165151815307,-0.64144963156915,-2.35664771434622E-16));
#140991=DIRECTION('ref_axis',(0.64144963156915,-0.767165151815306,6.82549510605368E-34));
#140992=DIRECTION('',(0.,3.67394039744206E-16,-1.));
#140993=DIRECTION('',(-0.641449631569149,0.767165151815306,0.));
#140994=DIRECTION('center_axis',(0.,3.67394039744206E-16,-1.));
#140995=DIRECTION('ref_axis',(0.,1.,3.67394039744206E-16));
#140996=DIRECTION('center_axis',(0.,0.,1.));
#140997=DIRECTION('ref_axis',(1.,0.,0.));
#140998=DIRECTION('center_axis',(0.,0.,1.));
#140999=DIRECTION('ref_axis',(1.,0.,0.));
#141000=DIRECTION('center_axis',(0.,0.,-1.));
#141001=DIRECTION('ref_axis',(-1.,0.,0.));
#141002=DIRECTION('center_axis',(0.,-3.67394039744206E-16,1.));
#141003=DIRECTION('ref_axis',(-1.,0.,0.));
#141004=DIRECTION('',(-1.,0.,0.));
#141005=DIRECTION('center_axis',(0.,-3.67394039744206E-16,1.));
#141006=DIRECTION('ref_axis',(-1.,0.,0.));
#141007=DIRECTION('',(0.,-1.,-3.67394039744206E-16));
#141008=DIRECTION('center_axis',(0.,-3.67394039744206E-16,1.));
#141009=DIRECTION('ref_axis',(-1.,0.,0.));
#141010=DIRECTION('',(1.,1.57059617562415E-15,5.77027673769358E-31));
#141011=DIRECTION('center_axis',(0.,-3.67394039744206E-16,1.));
#141012=DIRECTION('ref_axis',(-1.,0.,0.));
#141013=DIRECTION('',(0.,1.,3.67394039744206E-16));
#141014=DIRECTION('center_axis',(-1.,0.,0.));
#141015=DIRECTION('ref_axis',(0.,0.,1.));
#141016=DIRECTION('',(0.,3.67394039744206E-16,-1.));
#141017=DIRECTION('',(0.,1.,0.));
#141018=DIRECTION('',(0.,3.67394039744206E-16,-1.));
#141019=DIRECTION('center_axis',(0.,3.67394039744206E-16,-1.));
#141020=DIRECTION('ref_axis',(0.,1.,3.67394039744206E-16));
#141021=DIRECTION('',(0.,3.67394039744206E-16,-1.));
#141022=DIRECTION('center_axis',(0.,0.,1.));
#141023=DIRECTION('ref_axis',(1.,0.,0.));
#141024=DIRECTION('center_axis',(-1.57059617562415E-15,1.,3.67394039744206E-16));
#141025=DIRECTION('ref_axis',(-1.,-1.57059617562415E-15,0.));
#141026=DIRECTION('',(0.,3.67394039744206E-16,-1.));
#141027=DIRECTION('',(1.,1.57059617562415E-15,0.));
#141028=DIRECTION('center_axis',(0.,3.67394039744206E-16,-1.));
#141029=DIRECTION('ref_axis',(0.,1.,3.67394039744206E-16));
#141030=DIRECTION('',(0.,3.67394039744206E-16,-1.));
#141031=DIRECTION('center_axis',(0.,0.,1.));
#141032=DIRECTION('ref_axis',(1.,0.,0.));
#141033=DIRECTION('center_axis',(1.,0.,0.));
#141034=DIRECTION('ref_axis',(0.,0.,-1.));
#141035=DIRECTION('',(0.,3.67394039744206E-16,-1.));
#141036=DIRECTION('',(0.,-1.,0.));
#141037=DIRECTION('center_axis',(0.,3.67394039744206E-16,-1.));
#141038=DIRECTION('ref_axis',(0.,1.,3.67394039744206E-16));
#141039=DIRECTION('',(0.,3.67394039744206E-16,-1.));
#141040=DIRECTION('center_axis',(0.,0.,1.));
#141041=DIRECTION('ref_axis',(1.,0.,0.));
#141042=DIRECTION('center_axis',(0.,-1.,-3.67394039744206E-16));
#141043=DIRECTION('ref_axis',(0.,3.67394039744206E-16,-1.));
#141044=DIRECTION('',(0.,3.67394039744206E-16,-1.));
#141045=DIRECTION('',(-1.,0.,0.));
#141046=DIRECTION('center_axis',(0.,3.67394039744206E-16,-1.));
#141047=DIRECTION('ref_axis',(0.,1.,3.67394039744206E-16));
#141048=DIRECTION('center_axis',(0.,0.,1.));
#141049=DIRECTION('ref_axis',(1.,0.,0.));
#141050=DIRECTION('center_axis',(0.,0.,1.));
#141051=DIRECTION('ref_axis',(1.,0.,0.));
#141052=DIRECTION('center_axis',(-1.83697019872103E-16,1.83697019872104E-16,
-1.));
#141053=DIRECTION('ref_axis',(3.37445951098919E-32,1.,1.83697019872104E-16));
#141054=DIRECTION('center_axis',(0.,0.,1.));
#141055=DIRECTION('ref_axis',(1.,0.,0.));
#141056=DIRECTION('',(-1.83697019872103E-16,1.83697019872104E-16,-1.));
#141057=DIRECTION('center_axis',(1.83697019872103E-16,-1.83697019872104E-16,
1.));
#141058=DIRECTION('ref_axis',(3.30423519233678E-15,1.,1.83697019872103E-16));
#141059=DIRECTION('',(-1.83697019872103E-16,1.83697019872104E-16,-1.));
#141060=DIRECTION('center_axis',(0.,0.,-1.));
#141061=DIRECTION('ref_axis',(-1.,0.,0.));
#141062=DIRECTION('center_axis',(1.83697019872103E-16,-1.83697019872104E-16,
1.));
#141063=DIRECTION('ref_axis',(-3.49686235279956E-15,-1.,-1.83697019872103E-16));
#141064=DIRECTION('',(-0.767165151815309,-0.641449631569147,2.30935664208905E-17));
#141065=DIRECTION('',(-0.767165151815304,0.641449631569152,2.58758337855513E-16));
#141066=DIRECTION('center_axis',(1.83697019872103E-16,-1.83697019872104E-16,
1.));
#141067=DIRECTION('ref_axis',(3.49686235279957E-15,1.,1.83697019872103E-16));
#141068=DIRECTION('',(0.641449631569154,-0.767165151815303,-2.58758337855513E-16));
#141069=DIRECTION('center_axis',(1.83697019872103E-16,-1.83697019872104E-16,
1.));
#141070=DIRECTION('ref_axis',(3.30423519233678E-15,1.,1.83697019872103E-16));
#141071=DIRECTION('',(-0.641449631569147,-0.767165151815308,-2.30935664208913E-17));
#141072=DIRECTION('center_axis',(1.83697019872103E-16,-1.83697019872104E-16,
1.));
#141073=DIRECTION('ref_axis',(3.49686235279957E-15,1.,1.83697019872103E-16));
#141074=DIRECTION('',(0.767165151815299,0.641449631569159,-2.30935664208864E-17));
#141075=DIRECTION('center_axis',(1.83697019872103E-16,-1.83697019872104E-16,
1.));
#141076=DIRECTION('ref_axis',(3.30423519233678E-15,1.,1.83697019872103E-16));
#141077=DIRECTION('',(0.767165151815294,-0.641449631569164,-2.58758337855513E-16));
#141078=DIRECTION('center_axis',(1.83697019872103E-16,-1.83697019872104E-16,
1.));
#141079=DIRECTION('ref_axis',(-3.49686235279957E-15,-1.,-1.83697019872103E-16));
#141080=DIRECTION('',(-0.641449631569142,0.767165151815313,2.58758337855513E-16));
#141081=DIRECTION('center_axis',(1.83697019872103E-16,-1.83697019872104E-16,
1.));
#141082=DIRECTION('ref_axis',(-3.30423519233678E-15,-1.,-1.83697019872103E-16));
#141083=DIRECTION('',(0.641449631569159,0.767165151815299,2.30935664208873E-17));
#141084=DIRECTION('center_axis',(-0.767165151815299,0.641449631569159,2.58758337855513E-16));
#141085=DIRECTION('ref_axis',(-0.641449631569159,-0.767165151815298,2.46315430569441E-34));
#141086=DIRECTION('',(-1.83697019872103E-16,1.83697019872104E-16,-1.));
#141087=DIRECTION('',(0.641449631569159,0.767165151815299,0.));
#141088=DIRECTION('',(-1.83697019872103E-16,1.83697019872104E-16,-1.));
#141089=DIRECTION('center_axis',(-1.83697019872103E-16,1.83697019872104E-16,
-1.));
#141090=DIRECTION('ref_axis',(3.37445951098919E-32,1.,1.83697019872104E-16));
#141091=DIRECTION('',(-1.83697019872103E-16,1.83697019872104E-16,-1.));
#141092=DIRECTION('center_axis',(0.,0.,1.));
#141093=DIRECTION('ref_axis',(1.,0.,0.));
#141094=DIRECTION('center_axis',(-0.767165151815313,-0.641449631569142,
2.30935664208922E-17));
#141095=DIRECTION('ref_axis',(0.641449631569142,-0.767165151815313,1.8129589684176E-33));
#141096=DIRECTION('',(-1.83697019872103E-16,1.83697019872104E-16,-1.));
#141097=DIRECTION('',(-0.641449631569142,0.767165151815313,0.));
#141098=DIRECTION('center_axis',(-1.83697019872103E-16,1.83697019872104E-16,
-1.));
#141099=DIRECTION('ref_axis',(3.37445951098919E-32,1.,1.83697019872104E-16));
#141100=DIRECTION('',(-1.83697019872103E-16,1.83697019872104E-16,-1.));
#141101=DIRECTION('center_axis',(0.,0.,1.));
#141102=DIRECTION('ref_axis',(1.,0.,0.));
#141103=DIRECTION('center_axis',(0.641449631569165,0.767165151815294,2.30935664208855E-17));
#141104=DIRECTION('ref_axis',(-0.767165151815294,0.641449631569165,-3.14801159113747E-34));
#141105=DIRECTION('',(-1.83697019872103E-16,1.83697019872104E-16,-1.));
#141106=DIRECTION('',(0.767165151815294,-0.641449631569164,0.));
#141107=DIRECTION('center_axis',(-1.83697019872103E-16,1.83697019872104E-16,
-1.));
#141108=DIRECTION('ref_axis',(-2.23269251724179E-14,-1.,-1.836970198721E-16));
#141109=DIRECTION('',(-1.83697019872103E-16,1.83697019872104E-16,-1.));
#141110=DIRECTION('center_axis',(0.,0.,1.));
#141111=DIRECTION('ref_axis',(1.,0.,0.));
#141112=DIRECTION('center_axis',(-0.641449631569159,0.767165151815299,2.58758337855513E-16));
#141113=DIRECTION('ref_axis',(-0.767165151815298,-0.641449631569159,-9.84827031361874E-33));
#141114=DIRECTION('',(-1.83697019872103E-16,1.83697019872104E-16,-1.));
#141115=DIRECTION('',(0.767165151815299,0.641449631569159,0.));
#141116=DIRECTION('center_axis',(-1.83697019872103E-16,1.83697019872104E-16,
-1.));
#141117=DIRECTION('ref_axis',(3.37445951098919E-32,1.,1.83697019872104E-16));
#141118=DIRECTION('',(-1.83697019872103E-16,1.83697019872104E-16,-1.));
#141119=DIRECTION('center_axis',(0.,0.,1.));
#141120=DIRECTION('ref_axis',(1.,0.,0.));
#141121=DIRECTION('center_axis',(0.767165151815308,-0.641449631569147,-2.58758337855513E-16));
#141122=DIRECTION('ref_axis',(0.641449631569147,0.767165151815308,2.26488733284622E-32));
#141123=DIRECTION('',(-1.83697019872103E-16,1.83697019872104E-16,-1.));
#141124=DIRECTION('',(-0.641449631569147,-0.767165151815308,0.));
#141125=DIRECTION('center_axis',(-1.83697019872103E-16,1.83697019872104E-16,
-1.));
#141126=DIRECTION('ref_axis',(3.37445951098919E-32,1.,1.83697019872104E-16));
#141127=DIRECTION('',(-1.83697019872103E-16,1.83697019872104E-16,-1.));
#141128=DIRECTION('center_axis',(0.,0.,1.));
#141129=DIRECTION('ref_axis',(1.,0.,0.));
#141130=DIRECTION('center_axis',(0.767165151815303,0.641449631569154,-2.30935664208882E-17));
#141131=DIRECTION('ref_axis',(-0.641449631569154,0.767165151815303,4.78565540702031E-34));
#141132=DIRECTION('',(-1.83697019872103E-16,1.83697019872104E-16,-1.));
#141133=DIRECTION('',(0.641449631569154,-0.767165151815303,0.));
#141134=DIRECTION('center_axis',(-1.83697019872103E-16,1.83697019872104E-16,
-1.));
#141135=DIRECTION('ref_axis',(3.37445951098919E-32,1.,1.83697019872104E-16));
#141136=DIRECTION('',(-1.83697019872103E-16,1.83697019872104E-16,-1.));
#141137=DIRECTION('center_axis',(0.,0.,1.));
#141138=DIRECTION('ref_axis',(1.,0.,0.));
#141139=DIRECTION('center_axis',(-0.641449631569152,-0.767165151815304,
-2.30935664208896E-17));
#141140=DIRECTION('ref_axis',(0.767165151815304,-0.641449631569152,-1.89368129222539E-33));
#141141=DIRECTION('',(-0.767165151815304,0.641449631569152,0.));
#141142=DIRECTION('center_axis',(0.641449631569147,-0.767165151815309,-2.58758337855513E-16));
#141143=DIRECTION('ref_axis',(0.767165151815309,0.641449631569147,2.01792103840072E-32));
#141144=DIRECTION('',(-1.83697019872103E-16,1.83697019872104E-16,-1.));
#141145=DIRECTION('',(-0.767165151815309,-0.641449631569147,0.));
#141146=DIRECTION('center_axis',(-1.83697019872103E-16,1.83697019872104E-16,
-1.));
#141147=DIRECTION('ref_axis',(3.37445951098919E-32,1.,1.83697019872104E-16));
#141148=DIRECTION('center_axis',(0.,0.,1.));
#141149=DIRECTION('ref_axis',(1.,0.,0.));
#141150=DIRECTION('center_axis',(0.,0.,1.));
#141151=DIRECTION('ref_axis',(1.,0.,0.));
#141152=DIRECTION('center_axis',(0.,0.,-1.));
#141153=DIRECTION('ref_axis',(-1.,0.,0.));
#141154=DIRECTION('center_axis',(1.83697019872103E-16,-1.83697019872104E-16,
1.));
#141155=DIRECTION('ref_axis',(-3.85494105772625E-15,-1.,-1.83697019872103E-16));
#141156=DIRECTION('',(-3.49148133884313E-15,-1.,-1.83697019872103E-16));
#141157=DIRECTION('center_axis',(1.83697019872103E-16,-1.83697019872104E-16,
1.));
#141158=DIRECTION('ref_axis',(-3.85494105772625E-15,-1.,-1.83697019872103E-16));
#141159=DIRECTION('',(1.,-3.49148133884313E-15,-1.83697019872104E-16));
#141160=DIRECTION('center_axis',(1.83697019872103E-16,-1.83697019872104E-16,
1.));
#141161=DIRECTION('ref_axis',(-3.85494105772625E-15,-1.,-1.83697019872103E-16));
#141162=DIRECTION('',(1.92088516321898E-15,1.,1.83697019872103E-16));
#141163=DIRECTION('center_axis',(1.83697019872103E-16,-1.83697019872104E-16,
1.));
#141164=DIRECTION('ref_axis',(-3.85494105772623E-15,-1.,-1.83697019872103E-16));
#141165=DIRECTION('',(-1.,3.49148133884313E-15,1.83697019872104E-16));
#141166=DIRECTION('center_axis',(-3.49148133884313E-15,-1.,-1.83697019872103E-16));
#141167=DIRECTION('ref_axis',(1.,-3.49148133884313E-15,0.));
#141168=DIRECTION('',(-1.83697019872103E-16,1.83697019872104E-16,-1.));
#141169=DIRECTION('',(-1.,3.49148133884313E-15,0.));
#141170=DIRECTION('',(-1.83697019872103E-16,1.83697019872104E-16,-1.));
#141171=DIRECTION('center_axis',(-1.83697019872103E-16,1.83697019872104E-16,
-1.));
#141172=DIRECTION('ref_axis',(3.37445951098919E-32,1.,1.83697019872104E-16));
#141173=DIRECTION('',(-1.83697019872103E-16,1.83697019872104E-16,-1.));
#141174=DIRECTION('center_axis',(0.,0.,1.));
#141175=DIRECTION('ref_axis',(1.,0.,0.));
#141176=DIRECTION('center_axis',(-1.,1.92088516321898E-15,1.83697019872103E-16));
#141177=DIRECTION('ref_axis',(-1.92088516321898E-15,-1.,8.36251867343314E-49));
#141178=DIRECTION('',(-1.83697019872103E-16,1.83697019872104E-16,-1.));
#141179=DIRECTION('',(1.92088516321898E-15,1.,0.));
#141180=DIRECTION('center_axis',(-1.83697019872103E-16,1.83697019872104E-16,
-1.));
#141181=DIRECTION('ref_axis',(3.37445951098919E-32,1.,1.83697019872104E-16));
#141182=DIRECTION('',(-1.83697019872103E-16,1.83697019872104E-16,-1.));
#141183=DIRECTION('center_axis',(0.,0.,1.));
#141184=DIRECTION('ref_axis',(1.,0.,0.));
#141185=DIRECTION('center_axis',(3.49148133884313E-15,1.,1.83697019872103E-16));
#141186=DIRECTION('ref_axis',(-1.,3.49148133884313E-15,0.));
#141187=DIRECTION('',(-1.83697019872103E-16,1.83697019872104E-16,-1.));
#141188=DIRECTION('',(1.,-3.49148133884313E-15,0.));
#141189=DIRECTION('center_axis',(-1.83697019872103E-16,1.83697019872104E-16,
-1.));
#141190=DIRECTION('ref_axis',(3.37445951098919E-32,1.,1.83697019872104E-16));
#141191=DIRECTION('',(-1.83697019872103E-16,1.83697019872104E-16,-1.));
#141192=DIRECTION('center_axis',(0.,0.,1.));
#141193=DIRECTION('ref_axis',(1.,0.,0.));
#141194=DIRECTION('center_axis',(1.,-3.49148133884313E-15,-1.83697019872104E-16));
#141195=DIRECTION('ref_axis',(3.49148133884313E-15,1.,-1.78914547131776E-47));
#141196=DIRECTION('',(-1.83697019872103E-16,1.83697019872104E-16,-1.));
#141197=DIRECTION('',(-3.49148133884313E-15,-1.,0.));
#141198=DIRECTION('center_axis',(-1.83697019872103E-16,1.83697019872104E-16,
-1.));
#141199=DIRECTION('ref_axis',(3.37445951098919E-32,1.,1.83697019872104E-16));
#141200=DIRECTION('center_axis',(0.,0.,1.));
#141201=DIRECTION('ref_axis',(1.,0.,0.));
#141202=DIRECTION('center_axis',(0.,0.,1.));
#141203=DIRECTION('ref_axis',(1.,0.,0.));
#141204=DIRECTION('center_axis',(0.,0.,-1.));
#141205=DIRECTION('ref_axis',(-1.,0.,0.));
#141206=DIRECTION('center_axis',(0.,0.,1.));
#141207=DIRECTION('ref_axis',(1.,0.,0.));
#141208=DIRECTION('',(0.,0.,-1.));
#141209=DIRECTION('center_axis',(0.,0.,1.));
#141210=DIRECTION('ref_axis',(-1.,0.,0.));
#141211=DIRECTION('',(0.,0.,-1.));
#141212=DIRECTION('center_axis',(0.,0.,-1.));
#141213=DIRECTION('ref_axis',(-1.,0.,0.));
#141214=DIRECTION('center_axis',(0.,0.,1.));
#141215=DIRECTION('ref_axis',(1.,0.,0.));
#141216=DIRECTION('',(0.641449631569149,-0.767165151815306,0.));
#141217=DIRECTION('',(-0.641449631569149,-0.767165151815306,0.));
#141218=DIRECTION('center_axis',(0.,0.,1.));
#141219=DIRECTION('ref_axis',(-1.,0.,0.));
#141220=DIRECTION('',(0.767165151815301,0.641449631569157,0.));
#141221=DIRECTION('center_axis',(0.,0.,1.));
#141222=DIRECTION('ref_axis',(-1.,0.,0.));
#141223=DIRECTION('',(0.767165151815311,-0.641449631569145,0.));
#141224=DIRECTION('center_axis',(0.,0.,1.));
#141225=DIRECTION('ref_axis',(-1.,0.,0.));
#141226=DIRECTION('',(-0.641449631569162,0.767165151815296,0.));
#141227=DIRECTION('center_axis',(0.,0.,1.));
#141228=DIRECTION('ref_axis',(-1.,0.,0.));
#141229=DIRECTION('',(0.641449631569162,0.767165151815296,0.));
#141230=DIRECTION('center_axis',(0.,0.,1.));
#141231=DIRECTION('ref_axis',(1.,0.,0.));
#141232=DIRECTION('',(-0.767165151815311,-0.641449631569145,0.));
#141233=DIRECTION('center_axis',(0.,0.,1.));
#141234=DIRECTION('ref_axis',(1.,0.,0.));
#141235=DIRECTION('',(-0.767165151815301,0.641449631569157,0.));
#141236=DIRECTION('center_axis',(-0.641449631569157,-0.767165151815301,
0.));
#141237=DIRECTION('ref_axis',(0.767165151815301,-0.641449631569157,0.));
#141238=DIRECTION('',(0.,0.,-1.));
#141239=DIRECTION('',(-0.767165151815301,0.641449631569157,0.));
#141240=DIRECTION('',(0.,0.,-1.));
#141241=DIRECTION('center_axis',(0.,0.,-1.));
#141242=DIRECTION('ref_axis',(-1.,0.,0.));
#141243=DIRECTION('',(0.,0.,-1.));
#141244=DIRECTION('center_axis',(0.,0.,1.));
#141245=DIRECTION('ref_axis',(1.,0.,0.));
#141246=DIRECTION('center_axis',(0.641449631569145,-0.767165151815311,0.));
#141247=DIRECTION('ref_axis',(0.767165151815311,0.641449631569145,0.));
#141248=DIRECTION('',(0.,0.,-1.));
#141249=DIRECTION('',(-0.767165151815311,-0.641449631569145,0.));
#141250=DIRECTION('center_axis',(0.,0.,-1.));
#141251=DIRECTION('ref_axis',(-1.,0.,0.));
#141252=DIRECTION('',(0.,0.,-1.));
#141253=DIRECTION('center_axis',(0.,0.,1.));
#141254=DIRECTION('ref_axis',(1.,0.,0.));
#141255=DIRECTION('center_axis',(-0.767165151815296,0.641449631569162,0.));
#141256=DIRECTION('ref_axis',(-0.641449631569162,-0.767165151815296,0.));
#141257=DIRECTION('',(0.,0.,-1.));
#141258=DIRECTION('',(0.641449631569162,0.767165151815296,0.));
#141259=DIRECTION('center_axis',(0.,0.,-1.));
#141260=DIRECTION('ref_axis',(1.,7.6571373978539E-16,0.));
#141261=DIRECTION('',(0.,0.,-1.));
#141262=DIRECTION('center_axis',(0.,0.,1.));
#141263=DIRECTION('ref_axis',(1.,0.,0.));
#141264=DIRECTION('center_axis',(-0.767165151815296,-0.641449631569162,
0.));
#141265=DIRECTION('ref_axis',(0.641449631569162,-0.767165151815296,0.));
#141266=DIRECTION('',(0.,0.,-1.));
#141267=DIRECTION('',(-0.641449631569162,0.767165151815296,0.));
#141268=DIRECTION('center_axis',(0.,0.,-1.));
#141269=DIRECTION('ref_axis',(-1.,0.,0.));
#141270=DIRECTION('',(0.,0.,-1.));
#141271=DIRECTION('center_axis',(0.,0.,1.));
#141272=DIRECTION('ref_axis',(1.,0.,0.));
#141273=DIRECTION('center_axis',(0.641449631569145,0.767165151815311,0.));
#141274=DIRECTION('ref_axis',(-0.767165151815311,0.641449631569145,0.));
#141275=DIRECTION('',(0.,0.,-1.));
#141276=DIRECTION('',(0.767165151815311,-0.641449631569145,0.));
#141277=DIRECTION('center_axis',(0.,0.,-1.));
#141278=DIRECTION('ref_axis',(-1.,0.,0.));
#141279=DIRECTION('',(0.,0.,-1.));
#141280=DIRECTION('center_axis',(0.,0.,1.));
#141281=DIRECTION('ref_axis',(1.,0.,0.));
#141282=DIRECTION('center_axis',(-0.641449631569157,0.767165151815301,0.));
#141283=DIRECTION('ref_axis',(-0.767165151815301,-0.641449631569157,0.));
#141284=DIRECTION('',(0.,0.,-1.));
#141285=DIRECTION('',(0.767165151815301,0.641449631569157,0.));
#141286=DIRECTION('center_axis',(0.,0.,-1.));
#141287=DIRECTION('ref_axis',(-1.,0.,0.));
#141288=DIRECTION('',(0.,0.,-1.));
#141289=DIRECTION('center_axis',(0.,0.,1.));
#141290=DIRECTION('ref_axis',(1.,0.,0.));
#141291=DIRECTION('center_axis',(0.767165151815307,-0.64144963156915,0.));
#141292=DIRECTION('ref_axis',(0.64144963156915,0.767165151815306,0.));
#141293=DIRECTION('',(-0.641449631569149,-0.767165151815306,0.));
#141294=DIRECTION('center_axis',(0.767165151815307,0.64144963156915,0.));
#141295=DIRECTION('ref_axis',(-0.64144963156915,0.767165151815306,0.));
#141296=DIRECTION('',(0.,0.,-1.));
#141297=DIRECTION('',(0.641449631569149,-0.767165151815306,0.));
#141298=DIRECTION('center_axis',(0.,0.,-1.));
#141299=DIRECTION('ref_axis',(-1.,0.,0.));
#141300=DIRECTION('center_axis',(0.,0.,1.));
#141301=DIRECTION('ref_axis',(1.,0.,0.));
#141302=DIRECTION('center_axis',(0.,0.,1.));
#141303=DIRECTION('ref_axis',(1.,0.,0.));
#141304=DIRECTION('center_axis',(0.,0.,-1.));
#141305=DIRECTION('ref_axis',(-1.,0.,0.));
#141306=DIRECTION('center_axis',(0.,0.,1.));
#141307=DIRECTION('ref_axis',(1.,0.,0.));
#141308=DIRECTION('',(1.,0.,0.));
#141309=DIRECTION('center_axis',(0.,0.,1.));
#141310=DIRECTION('ref_axis',(1.,0.,0.));
#141311=DIRECTION('',(0.,1.,0.));
#141312=DIRECTION('center_axis',(0.,0.,1.));
#141313=DIRECTION('ref_axis',(1.,0.,0.));
#141314=DIRECTION('',(-1.,-1.57059617562415E-15,0.));
#141315=DIRECTION('center_axis',(0.,0.,1.));
#141316=DIRECTION('ref_axis',(1.,0.,0.));
#141317=DIRECTION('',(0.,-1.,0.));
#141318=DIRECTION('center_axis',(1.,0.,0.));
#141319=DIRECTION('ref_axis',(0.,0.,-1.));
#141320=DIRECTION('',(0.,0.,-1.));
#141321=DIRECTION('',(0.,-1.,0.));
#141322=DIRECTION('',(0.,0.,-1.));
#141323=DIRECTION('center_axis',(0.,0.,-1.));
#141324=DIRECTION('ref_axis',(-1.,0.,0.));
#141325=DIRECTION('',(0.,0.,-1.));
#141326=DIRECTION('center_axis',(0.,0.,1.));
#141327=DIRECTION('ref_axis',(1.,0.,0.));
#141328=DIRECTION('center_axis',(1.57059617562415E-15,-1.,0.));
#141329=DIRECTION('ref_axis',(1.,1.57059617562415E-15,0.));
#141330=DIRECTION('',(0.,0.,-1.));
#141331=DIRECTION('',(-1.,-1.57059617562415E-15,0.));
#141332=DIRECTION('center_axis',(0.,0.,-1.));
#141333=DIRECTION('ref_axis',(-1.,0.,0.));
#141334=DIRECTION('',(0.,0.,-1.));
#141335=DIRECTION('center_axis',(0.,0.,1.));
#141336=DIRECTION('ref_axis',(1.,0.,0.));
#141337=DIRECTION('center_axis',(-1.,0.,0.));
#141338=DIRECTION('ref_axis',(0.,0.,1.));
#141339=DIRECTION('',(0.,0.,-1.));
#141340=DIRECTION('',(0.,1.,0.));
#141341=DIRECTION('center_axis',(0.,0.,-1.));
#141342=DIRECTION('ref_axis',(-1.,0.,0.));
#141343=DIRECTION('',(0.,0.,-1.));
#141344=DIRECTION('center_axis',(0.,0.,1.));
#141345=DIRECTION('ref_axis',(1.,0.,0.));
#141346=DIRECTION('center_axis',(0.,1.,0.));
#141347=DIRECTION('ref_axis',(0.,0.,1.));
#141348=DIRECTION('',(0.,0.,-1.));
#141349=DIRECTION('',(1.,0.,0.));
#141350=DIRECTION('center_axis',(0.,0.,-1.));
#141351=DIRECTION('ref_axis',(-1.,0.,0.));
#141352=DIRECTION('center_axis',(0.,0.,1.));
#141353=DIRECTION('ref_axis',(1.,0.,0.));
#141354=DIRECTION('center_axis',(0.,0.,1.));
#141355=DIRECTION('ref_axis',(1.,0.,0.));
#141356=DIRECTION('center_axis',(-2.1350442781253E-15,1.,0.));
#141357=DIRECTION('ref_axis',(-1.,-2.1350442781253E-15,0.));
#141358=DIRECTION('',(1.,2.1350442781253E-15,0.));
#141359=DIRECTION('',(0.,0.,-1.));
#141360=DIRECTION('',(1.,2.1350442781253E-15,0.));
#141361=DIRECTION('',(0.,0.,1.));
#141362=DIRECTION('center_axis',(-1.,2.1350442781253E-15,0.));
#141363=DIRECTION('ref_axis',(-2.1350442781253E-15,-1.,0.));
#141364=DIRECTION('',(2.1350442781253E-15,1.,0.));
#141365=DIRECTION('',(0.,0.,-1.));
#141366=DIRECTION('',(2.1350442781253E-15,1.,0.));
#141367=DIRECTION('',(0.,0.,-1.));
#141368=DIRECTION('center_axis',(0.866025403784438,0.500000000000001,0.));
#141369=DIRECTION('ref_axis',(-0.500000000000001,0.866025403784438,0.));
#141370=DIRECTION('',(0.5,-0.866025403784438,0.));
#141371=DIRECTION('',(0.,0.,-1.));
#141372=DIRECTION('',(0.5,-0.866025403784438,0.));
#141373=DIRECTION('',(0.,0.,-1.));
#141374=DIRECTION('center_axis',(0.866025403784438,-0.500000000000002,0.));
#141375=DIRECTION('ref_axis',(0.500000000000002,0.866025403784437,0.));
#141376=DIRECTION('',(-0.500000000000002,-0.866025403784438,0.));
#141377=DIRECTION('',(-0.500000000000002,-0.866025403784438,0.));
#141378=DIRECTION('',(0.,0.,-1.));
#141379=DIRECTION('center_axis',(1.,0.,0.));
#141380=DIRECTION('ref_axis',(0.,0.,-1.));
#141381=DIRECTION('',(0.,-1.,0.));
#141382=DIRECTION('',(0.,-1.,0.));
#141383=DIRECTION('',(0.,0.,-1.));
#141384=DIRECTION('center_axis',(0.,0.,-1.));
#141385=DIRECTION('ref_axis',(-1.,0.,0.));
#141386=DIRECTION('center_axis',(0.,0.,-1.));
#141387=DIRECTION('ref_axis',(1.,0.,0.));
#141388=DIRECTION('center_axis',(0.,0.,-1.));
#141389=DIRECTION('ref_axis',(-1.,0.,0.));
#141390=DIRECTION('',(0.,0.,-1.));
#141391=DIRECTION('center_axis',(0.707106781186548,-0.707106781186548,0.));
#141392=DIRECTION('ref_axis',(0.707106781186548,0.707106781186548,0.));
#141393=DIRECTION('',(-0.707106781186548,-0.707106781186548,0.));
#141394=DIRECTION('',(-0.707106781186548,-0.707106781186548,0.));
#141395=DIRECTION('',(0.,0.,-1.));
#141396=DIRECTION('center_axis',(0.,0.,-1.));
#141397=DIRECTION('ref_axis',(-1.,0.,0.));
#141398=DIRECTION('center_axis',(0.,0.,-1.));
#141399=DIRECTION('ref_axis',(1.,-3.85494105772625E-15,0.));
#141400=DIRECTION('center_axis',(0.,0.,-1.));
#141401=DIRECTION('ref_axis',(-1.,0.,0.));
#141402=DIRECTION('',(0.,0.,-1.));
#141403=DIRECTION('center_axis',(1.6719208893717E-15,-1.,0.));
#141404=DIRECTION('ref_axis',(1.,1.6719208893717E-15,0.));
#141405=DIRECTION('',(-1.,-1.6719208893717E-15,0.));
#141406=DIRECTION('',(-1.,-1.6719208893717E-15,0.));
#141407=DIRECTION('',(0.,0.,-1.));
#141408=DIRECTION('center_axis',(0.,0.,-1.));
#141409=DIRECTION('ref_axis',(-1.,0.,0.));
#141410=DIRECTION('center_axis',(0.,0.,-1.));
#141411=DIRECTION('ref_axis',(1.,0.,0.));
#141412=DIRECTION('center_axis',(0.,0.,-1.));
#141413=DIRECTION('ref_axis',(-1.,0.,0.));
#141414=DIRECTION('',(0.,0.,-1.));
#141415=DIRECTION('center_axis',(-1.,-2.1350442781253E-15,0.));
#141416=DIRECTION('ref_axis',(2.1350442781253E-15,-1.,0.));
#141417=DIRECTION('',(-2.1350442781253E-15,1.,0.));
#141418=DIRECTION('',(-2.1350442781253E-15,1.,0.));
#141419=DIRECTION('',(0.,0.,-1.));
#141420=DIRECTION('center_axis',(0.,0.,-1.));
#141421=DIRECTION('ref_axis',(-1.,0.,0.));
#141422=DIRECTION('center_axis',(0.,0.,1.));
#141423=DIRECTION('ref_axis',(1.,0.,0.));
#141424=DIRECTION('center_axis',(0.,0.,1.));
#141425=DIRECTION('ref_axis',(-1.,0.,0.));
#141426=DIRECTION('',(0.,0.,-1.));
#141427=DIRECTION('center_axis',(3.01691039300315E-15,-1.,0.));
#141428=DIRECTION('ref_axis',(1.,3.01691039300315E-15,0.));
#141429=DIRECTION('',(-1.,-3.01691039300315E-15,0.));
#141430=DIRECTION('',(-1.,-3.01691039300315E-15,0.));
#141431=DIRECTION('',(0.,0.,-1.));
#141432=DIRECTION('center_axis',(1.,0.,0.));
#141433=DIRECTION('ref_axis',(0.,0.,-1.));
#141434=DIRECTION('',(0.,-1.,0.));
#141435=DIRECTION('',(0.,-1.,0.));
#141436=DIRECTION('',(0.,0.,-1.));
#141437=DIRECTION('center_axis',(0.,-1.,0.));
#141438=DIRECTION('ref_axis',(0.,0.,-1.));
#141439=DIRECTION('',(-1.,0.,0.));
#141440=DIRECTION('',(-1.,0.,0.));
#141441=DIRECTION('',(0.,0.,-1.));
#141442=DIRECTION('center_axis',(1.,0.,0.));
#141443=DIRECTION('ref_axis',(0.,0.,-1.));
#141444=DIRECTION('',(0.,-1.,0.));
#141445=DIRECTION('',(0.,-1.,0.));
#141446=DIRECTION('',(1.83697019872103E-16,1.83697019872101E-16,-1.));
#141447=DIRECTION('center_axis',(-7.30409884621813E-15,-1.,0.));
#141448=DIRECTION('ref_axis',(1.,-7.30409884621813E-15,0.));
#141449=DIRECTION('',(-1.,7.30409884621813E-15,0.));
#141450=DIRECTION('',(-1.83697019872103E-16,1.83697019872104E-16,-1.));
#141451=DIRECTION('',(-1.,7.30409884621813E-15,0.));
#141452=DIRECTION('',(0.,0.,-1.));
#141453=DIRECTION('center_axis',(1.,-1.26161707343766E-14,0.));
#141454=DIRECTION('ref_axis',(1.26161707343766E-14,1.,0.));
#141455=DIRECTION('',(-1.26161707343766E-14,-1.,0.));
#141456=DIRECTION('',(-1.26161707343766E-14,-1.,0.));
#141457=DIRECTION('',(0.,0.,-1.));
#141458=DIRECTION('center_axis',(-6.30808536718845E-15,-1.,0.));
#141459=DIRECTION('ref_axis',(1.,-6.30808536718845E-15,0.));
#141460=DIRECTION('',(-1.,6.30808536718845E-15,0.));
#141461=DIRECTION('',(-1.,6.30808536718845E-15,0.));
#141462=DIRECTION('',(0.,0.,-1.));
#141463=DIRECTION('center_axis',(1.,-9.05073117900944E-15,0.));
#141464=DIRECTION('ref_axis',(9.05073117900944E-15,1.,0.));
#141465=DIRECTION('',(-9.05073117900944E-15,-1.,0.));
#141466=DIRECTION('',(-9.05073117900944E-15,-1.,0.));
#141467=DIRECTION('',(0.,0.,-1.));
#141468=DIRECTION('center_axis',(0.,0.,-1.));
#141469=DIRECTION('ref_axis',(-1.,0.,0.));
#141470=DIRECTION('center_axis',(0.,0.,1.));
#141471=DIRECTION('ref_axis',(1.,0.,0.));
#141472=DIRECTION('center_axis',(0.,0.,1.));
#141473=DIRECTION('ref_axis',(1.,0.,0.));
#141474=DIRECTION('',(0.,0.,-1.));
#141475=DIRECTION('center_axis',(8.5401771125012E-15,1.,0.));
#141476=DIRECTION('ref_axis',(-1.,8.5401771125012E-15,0.));
#141477=DIRECTION('',(1.,-8.5401771125012E-15,0.));
#141478=DIRECTION('',(1.,-8.5401771125012E-15,0.));
#141479=DIRECTION('',(0.,0.,-1.));
#141480=DIRECTION('center_axis',(0.,0.,-1.));
#141481=DIRECTION('ref_axis',(-1.,0.,0.));
#141482=DIRECTION('center_axis',(0.,0.,-1.));
#141483=DIRECTION('ref_axis',(1.,2.31296463463574E-14,0.));
#141484=DIRECTION('center_axis',(0.,0.,-1.));
#141485=DIRECTION('ref_axis',(1.,0.,0.));
#141486=DIRECTION('',(0.,0.,-1.));
#141487=DIRECTION('center_axis',(1.,-8.3596044468585E-15,0.));
#141488=DIRECTION('ref_axis',(8.3596044468585E-15,1.,0.));
#141489=DIRECTION('',(-8.3596044468585E-15,-1.,0.));
#141490=DIRECTION('',(-8.3596044468585E-15,-1.,0.));
#141491=DIRECTION('',(0.,0.,-1.));
#141492=DIRECTION('center_axis',(0.,0.,-1.));
#141493=DIRECTION('ref_axis',(-1.,0.,0.));
#141494=DIRECTION('center_axis',(0.,0.,-1.));
#141495=DIRECTION('ref_axis',(1.,-7.70988211545251E-15,0.));
#141496=DIRECTION('center_axis',(0.,0.,-1.));
#141497=DIRECTION('ref_axis',(1.,0.,0.));
#141498=DIRECTION('',(0.,0.,-1.));
#141499=DIRECTION('center_axis',(0.707106781186542,-0.707106781186553,0.));
#141500=DIRECTION('ref_axis',(0.707106781186553,0.707106781186542,0.));
#141501=DIRECTION('',(-0.707106781186553,-0.707106781186542,0.));
#141502=DIRECTION('',(-0.707106781186553,-0.707106781186542,0.));
#141503=DIRECTION('',(0.,0.,-1.));
#141504=DIRECTION('center_axis',(0.,0.,-1.));
#141505=DIRECTION('ref_axis',(-1.,0.,0.));
#141506=DIRECTION('center_axis',(0.,0.,-1.));
#141507=DIRECTION('ref_axis',(1.,0.,0.));
#141508=DIRECTION('center_axis',(0.,0.,-1.));
#141509=DIRECTION('ref_axis',(1.,0.,0.));
#141510=DIRECTION('',(0.,0.,-1.));
#141511=DIRECTION('center_axis',(-8.7284827903955E-15,-1.,0.));
#141512=DIRECTION('ref_axis',(1.,-8.7284827903955E-15,0.));
#141513=DIRECTION('',(-1.,8.7284827903955E-15,0.));
#141514=DIRECTION('',(-1.,8.7284827903955E-15,0.));
#141515=DIRECTION('',(0.,0.,-1.));
#141516=DIRECTION('center_axis',(0.499999999999979,-0.866025403784451,0.));
#141517=DIRECTION('ref_axis',(0.866025403784451,0.499999999999979,0.));
#141518=DIRECTION('',(-0.866025403784451,-0.499999999999979,0.));
#141519=DIRECTION('',(-0.866025403784451,-0.499999999999979,0.));
#141520=DIRECTION('',(0.,0.,-1.));
#141521=DIRECTION('center_axis',(-0.500000000000004,-0.866025403784436,
0.));
#141522=DIRECTION('ref_axis',(0.866025403784436,-0.500000000000004,0.));
#141523=DIRECTION('',(-0.866025403784436,0.500000000000004,0.));
#141524=DIRECTION('',(-0.866025403784436,0.500000000000004,0.));
#141525=DIRECTION('',(0.,0.,-1.));
#141526=DIRECTION('center_axis',(0.,-1.,0.));
#141527=DIRECTION('ref_axis',(0.,0.,-1.));
#141528=DIRECTION('',(-1.,0.,0.));
#141529=DIRECTION('',(-1.,0.,0.));
#141530=DIRECTION('',(0.,0.,-1.));
#141531=DIRECTION('center_axis',(0.,0.,-1.));
#141532=DIRECTION('ref_axis',(-1.,0.,0.));
#141533=DIRECTION('center_axis',(0.,0.,-1.));
#141534=DIRECTION('ref_axis',(1.,-7.70988211545249E-15,0.));
#141535=DIRECTION('center_axis',(0.,0.,-1.));
#141536=DIRECTION('ref_axis',(1.,0.,0.));
#141537=DIRECTION('',(0.,0.,-1.));
#141538=DIRECTION('center_axis',(-0.707106781186548,-0.707106781186548,
0.));
#141539=DIRECTION('ref_axis',(0.707106781186548,-0.707106781186548,0.));
#141540=DIRECTION('',(-0.707106781186548,0.707106781186548,0.));
#141541=DIRECTION('',(-0.707106781186548,0.707106781186548,0.));
#141542=DIRECTION('',(0.,0.,-1.));
#141543=DIRECTION('center_axis',(0.,0.,-1.));
#141544=DIRECTION('ref_axis',(-1.,0.,0.));
#141545=DIRECTION('center_axis',(0.,0.,-1.));
#141546=DIRECTION('ref_axis',(1.,0.,0.));
#141547=DIRECTION('center_axis',(0.,0.,-1.));
#141548=DIRECTION('ref_axis',(1.,0.,0.));
#141549=DIRECTION('',(0.,0.,-1.));
#141550=DIRECTION('center_axis',(-1.,0.,0.));
#141551=DIRECTION('ref_axis',(0.,0.,1.));
#141552=DIRECTION('',(0.,1.,0.));
#141553=DIRECTION('',(0.,1.,0.));
#141554=DIRECTION('',(0.,0.,-1.));
#141555=DIRECTION('center_axis',(0.,0.,-1.));
#141556=DIRECTION('ref_axis',(-1.,0.,0.));
#141557=DIRECTION('center_axis',(0.,0.,-1.));
#141558=DIRECTION('ref_axis',(1.,0.,0.));
#141559=DIRECTION('center_axis',(0.,0.,-1.));
#141560=DIRECTION('ref_axis',(1.,0.,0.));
#141561=DIRECTION('center_axis',(-2.1350442781253E-15,1.,0.));
#141562=DIRECTION('ref_axis',(-1.,-2.1350442781253E-15,0.));
#141563=DIRECTION('',(1.,2.1350442781253E-15,0.));
#141564=DIRECTION('',(0.,0.,-1.));
#141565=DIRECTION('',(1.,2.1350442781253E-15,0.));
#141566=DIRECTION('',(0.,0.,-1.));
#141567=DIRECTION('center_axis',(0.,0.,-1.));
#141568=DIRECTION('ref_axis',(-1.,0.,0.));
#141569=DIRECTION('center_axis',(0.,0.,1.));
#141570=DIRECTION('ref_axis',(1.,0.,0.));
#141571=DIRECTION('center_axis',(0.,0.,1.));
#141572=DIRECTION('ref_axis',(1.,0.,0.));
#141573=DIRECTION('',(0.,0.,-1.));
#141574=DIRECTION('center_axis',(-1.,0.,0.));
#141575=DIRECTION('ref_axis',(0.,0.,1.));
#141576=DIRECTION('',(0.,1.,0.));
#141577=DIRECTION('',(0.,1.,0.));
#141578=DIRECTION('',(0.,0.,-1.));
#141579=DIRECTION('center_axis',(0.,-1.,0.));
#141580=DIRECTION('ref_axis',(0.,0.,-1.));
#141581=DIRECTION('',(-1.,0.,0.));
#141582=DIRECTION('',(-1.,0.,0.));
#141583=DIRECTION('',(0.,0.,-1.));
#141584=DIRECTION('center_axis',(-1.,0.,0.));
#141585=DIRECTION('ref_axis',(0.,0.,1.));
#141586=DIRECTION('',(0.,1.,0.));
#141587=DIRECTION('',(0.,1.,0.));
#141588=DIRECTION('',(0.,0.,-1.));
#141589=DIRECTION('center_axis',(0.,-1.,0.));
#141590=DIRECTION('ref_axis',(0.,0.,-1.));
#141591=DIRECTION('',(-1.,0.,0.));
#141592=DIRECTION('',(-1.,0.,0.));
#141593=DIRECTION('',(0.,0.,-1.));
#141594=DIRECTION('center_axis',(0.,0.,-1.));
#141595=DIRECTION('ref_axis',(-1.,0.,0.));
#141596=DIRECTION('center_axis',(0.,0.,1.));
#141597=DIRECTION('ref_axis',(1.,0.,0.));
#141598=DIRECTION('center_axis',(0.,0.,1.));
#141599=DIRECTION('ref_axis',(1.,0.,0.));
#141600=DIRECTION('',(0.,0.,-1.));
#141601=DIRECTION('center_axis',(1.,-4.12146228552343E-16,0.));
#141602=DIRECTION('ref_axis',(4.12146228552343E-16,1.,0.));
#141603=DIRECTION('',(-4.12146228552343E-16,-1.,0.));
#141604=DIRECTION('',(-4.12146228552343E-16,-1.,0.));
#141605=DIRECTION('',(0.,0.,-1.));
#141606=DIRECTION('center_axis',(0.,1.,0.));
#141607=DIRECTION('ref_axis',(0.,0.,1.));
#141608=DIRECTION('',(1.,0.,0.));
#141609=DIRECTION('',(1.,0.,0.));
#141610=DIRECTION('',(0.,0.,-1.));
#141611=DIRECTION('center_axis',(1.,0.,0.));
#141612=DIRECTION('ref_axis',(0.,0.,-1.));
#141613=DIRECTION('',(0.,-1.,0.));
#141614=DIRECTION('',(0.,-1.,0.));
#141615=DIRECTION('',(0.,0.,-1.));
#141616=DIRECTION('center_axis',(3.01691039300315E-15,1.,0.));
#141617=DIRECTION('ref_axis',(-1.,3.01691039300315E-15,0.));
#141618=DIRECTION('',(1.,-3.01691039300315E-15,0.));
#141619=DIRECTION('',(1.,-3.01691039300315E-15,0.));
#141620=DIRECTION('',(0.,0.,-1.));
#141621=DIRECTION('center_axis',(0.,0.,-1.));
#141622=DIRECTION('ref_axis',(-1.,0.,0.));
#141623=DIRECTION('center_axis',(0.,0.,1.));
#141624=DIRECTION('ref_axis',(1.,0.,0.));
#141625=DIRECTION('center_axis',(0.,0.,1.));
#141626=DIRECTION('ref_axis',(1.,0.,0.));
#141627=DIRECTION('',(0.,0.,-1.));
#141628=DIRECTION('center_axis',(-1.,2.1350442781253E-15,0.));
#141629=DIRECTION('ref_axis',(-2.1350442781253E-15,-1.,0.));
#141630=DIRECTION('',(2.1350442781253E-15,1.,0.));
#141631=DIRECTION('',(2.1350442781253E-15,1.,0.));
#141632=DIRECTION('',(0.,0.,1.));
#141633=DIRECTION('center_axis',(0.,0.,-1.));
#141634=DIRECTION('ref_axis',(-1.,0.,0.));
#141635=DIRECTION('center_axis',(0.,0.,-1.));
#141636=DIRECTION('ref_axis',(1.,0.,0.));
#141637=DIRECTION('center_axis',(0.,0.,-1.));
#141638=DIRECTION('ref_axis',(1.,0.,0.));
#141639=DIRECTION('',(0.,0.,-1.));
#141640=DIRECTION('center_axis',(1.6719208893717E-15,1.,0.));
#141641=DIRECTION('ref_axis',(-1.,1.6719208893717E-15,0.));
#141642=DIRECTION('',(1.,-1.6719208893717E-15,0.));
#141643=DIRECTION('',(1.,-1.6719208893717E-15,0.));
#141644=DIRECTION('',(0.,0.,-1.));
#141645=DIRECTION('center_axis',(0.,0.,-1.));
#141646=DIRECTION('ref_axis',(-1.,0.,0.));
#141647=DIRECTION('center_axis',(0.,0.,-1.));
#141648=DIRECTION('ref_axis',(1.,0.,0.));
#141649=DIRECTION('center_axis',(0.,0.,-1.));
#141650=DIRECTION('ref_axis',(1.,0.,0.));
#141651=DIRECTION('',(0.,0.,-1.));
#141652=DIRECTION('center_axis',(0.707106781186548,0.707106781186548,0.));
#141653=DIRECTION('ref_axis',(-0.707106781186548,0.707106781186548,0.));
#141654=DIRECTION('',(0.707106781186547,-0.707106781186547,0.));
#141655=DIRECTION('',(0.707106781186547,-0.707106781186547,0.));
#141656=DIRECTION('',(0.,0.,-1.));
#141657=DIRECTION('center_axis',(0.,0.,-1.));
#141658=DIRECTION('ref_axis',(-1.,0.,0.));
#141659=DIRECTION('center_axis',(0.,0.,-1.));
#141660=DIRECTION('ref_axis',(1.,4.6259292692715E-14,0.));
#141661=DIRECTION('center_axis',(0.,0.,-1.));
#141662=DIRECTION('ref_axis',(1.,0.,0.));
#141663=DIRECTION('',(0.,0.,-1.));
#141664=DIRECTION('center_axis',(1.,0.,0.));
#141665=DIRECTION('ref_axis',(0.,0.,-1.));
#141666=DIRECTION('',(0.,-1.,0.));
#141667=DIRECTION('',(0.,-1.,0.));
#141668=DIRECTION('center_axis',(0.499999999999997,-0.86602540378444,-2.50934795744788E-16));
#141669=DIRECTION('ref_axis',(0.86602540378444,0.499999999999997,1.16566443650333E-32));
#141670=DIRECTION('',(-0.86602540378444,-0.499999999999997,0.));
#141671=DIRECTION('',(-1.83697019872103E-16,1.83697019872104E-16,-1.));
#141672=DIRECTION('',(-0.86602540378444,-0.499999999999997,6.7237775872685E-17));
#141673=DIRECTION('',(-1.83697019872103E-16,1.83697019872104E-16,-1.));
#141674=DIRECTION('center_axis',(-0.500000000000005,-0.866025403784436,
-6.72377758726837E-17));
#141675=DIRECTION('ref_axis',(0.866025403784436,-0.500000000000005,6.17106363235252E-33));
#141676=DIRECTION('',(-0.866025403784436,0.500000000000005,0.));
#141677=DIRECTION('',(-0.866025403784436,0.500000000000005,2.50934795744788E-16));
#141678=DIRECTION('',(-1.83697019872103E-16,1.83697019872104E-16,-1.));
#141679=DIRECTION('center_axis',(-3.49148133884313E-15,-1.,-1.83697019872103E-16));
#141680=DIRECTION('ref_axis',(1.,-3.49148133884313E-15,0.));
#141681=DIRECTION('',(-1.,3.49148133884313E-15,0.));
#141682=DIRECTION('',(-1.,3.49148133884313E-15,1.83697019872104E-16));
#141683=DIRECTION('',(-1.83697019872103E-16,1.83697019872104E-16,-1.));
#141684=DIRECTION('center_axis',(-1.83697019872103E-16,1.83697019872104E-16,
-1.));
#141685=DIRECTION('ref_axis',(3.37445951098919E-32,1.,1.83697019872104E-16));
#141686=DIRECTION('center_axis',(0.,0.,-1.));
#141687=DIRECTION('ref_axis',(1.,0.,0.));
#141688=DIRECTION('center_axis',(-1.83697019872103E-16,1.83697019872104E-16,
-1.));
#141689=DIRECTION('ref_axis',(3.85494105772625E-15,1.,1.83697019872103E-16));
#141690=DIRECTION('',(-1.83697019872103E-16,1.83697019872104E-16,-1.));
#141691=DIRECTION('center_axis',(-0.70710678118655,-0.707106781186545,4.36149058175079E-31));
#141692=DIRECTION('ref_axis',(0.707106781186545,-0.70710678118655,2.77480222991945E-47));
#141693=DIRECTION('',(-0.707106781186545,0.70710678118655,0.));
#141694=DIRECTION('',(-0.707106781186545,0.70710678118655,2.59786816870648E-16));
#141695=DIRECTION('',(-1.83697019872103E-16,1.83697019872104E-16,-1.));
#141696=DIRECTION('center_axis',(-1.83697019872103E-16,1.83697019872104E-16,
-1.));
#141697=DIRECTION('ref_axis',(3.37445951098919E-32,1.,1.83697019872104E-16));
#141698=DIRECTION('center_axis',(0.,0.,-1.));
#141699=DIRECTION('ref_axis',(1.,0.,0.));
#141700=DIRECTION('center_axis',(-1.83697019872103E-16,1.83697019872104E-16,
-1.));
#141701=DIRECTION('ref_axis',(3.85494105772625E-15,1.,1.83697019872103E-16));
#141702=DIRECTION('',(-1.83697019872103E-16,1.83697019872104E-16,-1.));
#141703=DIRECTION('center_axis',(-1.,1.81956044947143E-15,1.83697019872103E-16));
#141704=DIRECTION('ref_axis',(-1.81956044947143E-15,-1.,1.5521017945049E-47));
#141705=DIRECTION('',(1.81956044947143E-15,1.,0.));
#141706=DIRECTION('',(1.81956044947143E-15,1.,1.83697019872103E-16));
#141707=DIRECTION('',(-1.83697019872103E-16,1.83697019872104E-16,-1.));
#141708=DIRECTION('center_axis',(-1.83697019872103E-16,1.83697019872104E-16,
-1.));
#141709=DIRECTION('ref_axis',(3.37445951098919E-32,1.,1.83697019872104E-16));
#141710=DIRECTION('center_axis',(0.,0.,-1.));
#141711=DIRECTION('ref_axis',(1.,0.,0.));
#141712=DIRECTION('center_axis',(-1.83697019872103E-16,1.83697019872104E-16,
-1.));
#141713=DIRECTION('ref_axis',(3.85494105772625E-15,1.,1.83697019872103E-16));
#141714=DIRECTION('',(-1.83697019872103E-16,1.83697019872104E-16,-1.));
#141715=DIRECTION('center_axis',(1.35643706071783E-15,1.,1.83697019872103E-16));
#141716=DIRECTION('ref_axis',(-1.,1.35643706071783E-15,0.));
#141717=DIRECTION('',(1.,-1.35643706071783E-15,0.));
#141718=DIRECTION('',(1.,-1.35643706071783E-15,-1.83697019872103E-16));
#141719=DIRECTION('',(-1.83697019872103E-16,1.83697019872104E-16,-1.));
#141720=DIRECTION('center_axis',(-1.83697019872103E-16,1.83697019872104E-16,
-1.));
#141721=DIRECTION('ref_axis',(3.37445951098919E-32,1.,1.83697019872104E-16));
#141722=DIRECTION('center_axis',(0.,0.,1.));
#141723=DIRECTION('ref_axis',(1.,0.,0.));
#141724=DIRECTION('center_axis',(1.83697019872103E-16,-1.83697019872104E-16,
1.));
#141725=DIRECTION('ref_axis',(3.85494105772628E-15,1.,1.83697019872103E-16));
#141726=DIRECTION('',(-1.83697019872103E-16,1.83697019872104E-16,-1.));
#141727=DIRECTION('center_axis',(-1.,4.74570945839986E-16,1.83697019872103E-16));
#141728=DIRECTION('ref_axis',(-4.74570945839986E-16,-1.,-8.94815989765196E-49));
#141729=DIRECTION('',(4.74570945839986E-16,1.,0.));
#141730=DIRECTION('',(4.74570945839986E-16,1.,1.83697019872104E-16));
#141731=DIRECTION('',(-1.83697019872103E-16,1.83697019872104E-16,-1.));
#141732=DIRECTION('center_axis',(-3.49148133884313E-15,-1.,-1.83697019872103E-16));
#141733=DIRECTION('ref_axis',(1.,-3.49148133884313E-15,0.));
#141734=DIRECTION('',(-1.,3.49148133884313E-15,0.));
#141735=DIRECTION('',(-1.,3.49148133884313E-15,1.83697019872104E-16));
#141736=DIRECTION('',(-1.83697019872103E-16,1.83697019872104E-16,-1.));
#141737=DIRECTION('center_axis',(-1.,3.49148133884313E-15,1.83697019872104E-16));
#141738=DIRECTION('ref_axis',(-3.49148133884313E-15,-1.,1.78914547131776E-47));
#141739=DIRECTION('',(3.49148133884313E-15,1.,0.));
#141740=DIRECTION('',(3.49148133884313E-15,1.,1.83697019872103E-16));
#141741=DIRECTION('center_axis',(-1.,1.07955801850613E-14,1.83697019872105E-16));
#141742=DIRECTION('ref_axis',(-1.07955801850613E-14,-1.,-1.3652856201189E-46));
#141743=DIRECTION('',(1.07955801850613E-14,1.,0.));
#141744=DIRECTION('',(0.,3.67394039744206E-16,-1.));
#141745=DIRECTION('',(1.07955801850613E-14,1.,1.83697019872102E-16));
#141746=DIRECTION('',(-1.83697019872103E-16,1.83697019872104E-16,-1.));
#141747=DIRECTION('center_axis',(-1.61076520732197E-14,-1.,-1.83697019872101E-16));
#141748=DIRECTION('ref_axis',(1.,-1.61076520732197E-14,0.));
#141749=DIRECTION('',(-1.,1.61076520732197E-14,0.));
#141750=DIRECTION('',(-1.,1.61076520732197E-14,1.83697019872106E-16));
#141751=DIRECTION('',(-1.83697019872103E-16,1.83697019872104E-16,-1.));
#141752=DIRECTION('center_axis',(-1.,9.79956670603158E-15,1.83697019872105E-16));
#141753=DIRECTION('ref_axis',(-9.79956670603158E-15,-1.,1.22009766052885E-46));
#141754=DIRECTION('',(9.79956670603158E-15,1.,0.));
#141755=DIRECTION('',(9.79956670603158E-15,1.,1.83697019872102E-16));
#141756=DIRECTION('',(-1.83697019872103E-16,1.83697019872104E-16,-1.));
#141757=DIRECTION('center_axis',(-1.25422125178526E-14,-1.,-1.83697019872101E-16));
#141758=DIRECTION('ref_axis',(1.,-1.25422125178526E-14,0.));
#141759=DIRECTION('',(-1.,1.25422125178526E-14,0.));
#141760=DIRECTION('',(-1.,1.25422125178526E-14,1.83697019872105E-16));
#141761=DIRECTION('',(-1.83697019872103E-16,1.83697019872104E-16,-1.));
#141762=DIRECTION('center_axis',(-1.83697019872103E-16,1.83697019872104E-16,
-1.));
#141763=DIRECTION('ref_axis',(3.37445951098919E-32,1.,1.83697019872104E-16));
#141764=DIRECTION('center_axis',(0.,0.,1.));
#141765=DIRECTION('ref_axis',(1.,0.,0.));
#141766=DIRECTION('center_axis',(1.83697019872103E-16,-1.83697019872104E-16,
1.));
#141767=DIRECTION('ref_axis',(-3.37445951098919E-32,-1.,-1.83697019872104E-16));
#141768=DIRECTION('',(-1.83697019872103E-16,1.83697019872104E-16,-1.));
#141769=DIRECTION('center_axis',(1.,-1.20316584513443E-14,-1.83697019872105E-16));
#141770=DIRECTION('ref_axis',(1.20316584513443E-14,1.,1.32485337866494E-46));
#141771=DIRECTION('',(-1.20316584513443E-14,-1.,0.));
#141772=DIRECTION('',(-1.20316584513443E-14,-1.,-1.83697019872101E-16));
#141773=DIRECTION('',(-1.83697019872103E-16,1.83697019872104E-16,-1.));
#141774=DIRECTION('center_axis',(-1.83697019872103E-16,1.83697019872104E-16,
-1.));
#141775=DIRECTION('ref_axis',(3.37445951098919E-32,1.,1.83697019872104E-16));
#141776=DIRECTION('center_axis',(0.,0.,-1.));
#141777=DIRECTION('ref_axis',(1.,-1.15648231731787E-14,0.));
#141778=DIRECTION('center_axis',(-1.83697019872103E-16,1.83697019872104E-16,
-1.));
#141779=DIRECTION('ref_axis',(-3.37445951098919E-32,-1.,-1.83697019872104E-16));
#141780=DIRECTION('',(-1.83697019872103E-16,1.83697019872104E-16,-1.));
#141781=DIRECTION('center_axis',(-1.18510857857016E-14,-1.,-1.83697019872101E-16));
#141782=DIRECTION('ref_axis',(1.,-1.18510857857016E-14,0.));
#141783=DIRECTION('',(-1.,1.18510857857016E-14,0.));
#141784=DIRECTION('',(-1.,1.18510857857016E-14,1.83697019872105E-16));
#141785=DIRECTION('',(-1.83697019872103E-16,1.83697019872104E-16,-1.));
#141786=DIRECTION('center_axis',(-1.83697019872103E-16,1.83697019872104E-16,
-1.));
#141787=DIRECTION('ref_axis',(3.37445951098919E-32,1.,1.83697019872104E-16));
#141788=DIRECTION('center_axis',(0.,0.,-1.));
#141789=DIRECTION('ref_axis',(1.,-1.92747052886312E-15,0.));
#141790=DIRECTION('center_axis',(-1.83697019872103E-16,1.83697019872104E-16,
-1.));
#141791=DIRECTION('ref_axis',(-3.37445951098919E-32,-1.,-1.83697019872104E-16));
#141792=DIRECTION('',(-1.83697019872103E-16,1.83697019872104E-16,-1.));
#141793=DIRECTION('center_axis',(-0.707106781186555,-0.70710678118654,2.38933831869826E-30));
#141794=DIRECTION('ref_axis',(0.70710678118654,-0.707106781186555,2.91705557987951E-47));
#141795=DIRECTION('',(-0.70710678118654,0.707106781186555,0.));
#141796=DIRECTION('',(-0.70710678118654,0.707106781186555,2.59786816870648E-16));
#141797=DIRECTION('',(-1.83697019872103E-16,1.83697019872104E-16,-1.));
#141798=DIRECTION('center_axis',(-1.83697019872103E-16,1.83697019872104E-16,
-1.));
#141799=DIRECTION('ref_axis',(3.37445951098919E-32,1.,1.83697019872104E-16));
#141800=DIRECTION('center_axis',(0.,0.,-1.));
#141801=DIRECTION('ref_axis',(1.,-1.15648231731787E-14,0.));
#141802=DIRECTION('center_axis',(-1.83697019872103E-16,1.83697019872104E-16,
-1.));
#141803=DIRECTION('ref_axis',(-3.37445951098919E-32,-1.,-1.83697019872104E-16));
#141804=DIRECTION('',(-1.83697019872103E-16,1.83697019872104E-16,-1.));
#141805=DIRECTION('center_axis',(-1.,1.22199641292386E-14,1.83697019872105E-16));
#141806=DIRECTION('ref_axis',(-1.22199641292386E-14,-1.,1.88282412675184E-47));
#141807=DIRECTION('',(1.22199641292386E-14,1.,0.));
#141808=DIRECTION('',(1.22199641292386E-14,1.,1.83697019872101E-16));
#141809=DIRECTION('',(-1.83697019872103E-16,1.83697019872104E-16,-1.));
#141810=DIRECTION('center_axis',(-0.866025403784453,-0.499999999999976,
6.72377758726913E-17));
#141811=DIRECTION('ref_axis',(0.499999999999976,-0.866025403784453,-1.39433958635012E-33));
#141812=DIRECTION('',(-0.499999999999976,0.866025403784453,0.));
#141813=DIRECTION('',(-0.499999999999976,0.866025403784453,2.50934795744786E-16));
#141814=DIRECTION('',(-1.83697019872103E-16,1.83697019872104E-16,-1.));
#141815=DIRECTION('center_axis',(-0.866025403784435,0.500000000000007,2.50934795744788E-16));
#141816=DIRECTION('ref_axis',(-0.500000000000007,-0.866025403784435,3.9034319157649E-33));
#141817=DIRECTION('',(0.500000000000007,0.866025403784435,0.));
#141818=DIRECTION('',(0.500000000000007,0.866025403784435,6.72377758726831E-17));
#141819=DIRECTION('',(-1.83697019872103E-16,1.83697019872104E-16,-1.));
#141820=DIRECTION('center_axis',(-1.,3.49148133884313E-15,1.83697019872104E-16));
#141821=DIRECTION('ref_axis',(-3.49148133884313E-15,-1.,1.78914547131776E-47));
#141822=DIRECTION('',(3.49148133884313E-15,1.,0.));
#141823=DIRECTION('',(3.49148133884313E-15,1.,1.83697019872103E-16));
#141824=DIRECTION('',(-1.83697019872103E-16,1.83697019872104E-16,-1.));
#141825=DIRECTION('center_axis',(-1.83697019872103E-16,1.83697019872104E-16,
-1.));
#141826=DIRECTION('ref_axis',(3.37445951098919E-32,1.,1.83697019872104E-16));
#141827=DIRECTION('center_axis',(0.,0.,-1.));
#141828=DIRECTION('ref_axis',(1.,-2.31296463463575E-14,0.));
#141829=DIRECTION('center_axis',(-1.83697019872103E-16,1.83697019872104E-16,
-1.));
#141830=DIRECTION('ref_axis',(-3.37445951098919E-32,-1.,-1.83697019872104E-16));
#141831=DIRECTION('',(-1.83697019872103E-16,1.83697019872104E-16,-1.));
#141832=DIRECTION('center_axis',(-0.707106781186545,0.70710678118655,2.59786816870649E-16));
#141833=DIRECTION('ref_axis',(-0.70710678118655,-0.707106781186545,-1.41173070057919E-32));
#141834=DIRECTION('',(0.70710678118655,0.707106781186545,0.));
#141835=DIRECTION('',(0.70710678118655,0.707106781186545,-4.68386162474976E-31));
#141836=DIRECTION('',(-1.83697019872103E-16,1.83697019872104E-16,-1.));
#141837=DIRECTION('center_axis',(-1.83697019872103E-16,1.83697019872104E-16,
-1.));
#141838=DIRECTION('ref_axis',(3.37445951098919E-32,1.,1.83697019872104E-16));
#141839=DIRECTION('center_axis',(0.,0.,-1.));
#141840=DIRECTION('ref_axis',(1.,0.,0.));
#141841=DIRECTION('center_axis',(-1.83697019872103E-16,1.83697019872104E-16,
-1.));
#141842=DIRECTION('ref_axis',(-3.37445951098919E-32,-1.,-1.83697019872104E-16));
#141843=DIRECTION('',(-1.83697019872103E-16,1.83697019872104E-16,-1.));
#141844=DIRECTION('center_axis',(3.49148133884313E-15,1.,1.83697019872103E-16));
#141845=DIRECTION('ref_axis',(-1.,3.49148133884313E-15,0.));
#141846=DIRECTION('',(1.,-3.49148133884313E-15,0.));
#141847=DIRECTION('',(1.,-3.49148133884313E-15,-1.83697019872104E-16));
#141848=DIRECTION('',(-1.83697019872103E-16,1.83697019872104E-16,-1.));
#141849=DIRECTION('center_axis',(-1.83697019872103E-16,1.83697019872104E-16,
-1.));
#141850=DIRECTION('ref_axis',(3.37445951098919E-32,1.,1.83697019872104E-16));
#141851=DIRECTION('center_axis',(0.,0.,-1.));
#141852=DIRECTION('ref_axis',(1.,2.31296463463577E-14,0.));
#141853=DIRECTION('center_axis',(-1.83697019872103E-16,1.83697019872104E-16,
-1.));
#141854=DIRECTION('ref_axis',(-3.37445951098919E-32,-1.,-1.83697019872104E-16));
#141855=DIRECTION('',(-1.83697019872103E-16,1.83697019872104E-16,-1.));
#141856=DIRECTION('center_axis',(1.,-1.35643706071783E-15,-1.83697019872103E-16));
#141857=DIRECTION('ref_axis',(1.35643706071783E-15,1.,8.4478697733554E-48));
#141858=DIRECTION('',(-1.35643706071783E-15,-1.,0.));
#141859=DIRECTION('',(-1.35643706071783E-15,-1.,-1.83697019872103E-16));
#141860=DIRECTION('',(-1.83697019872103E-16,1.83697019872104E-16,-1.));
#141861=DIRECTION('center_axis',(-1.83697019872103E-16,1.83697019872104E-16,
-1.));
#141862=DIRECTION('ref_axis',(3.37445951098919E-32,1.,1.83697019872104E-16));
#141863=DIRECTION('center_axis',(0.,0.,1.));
#141864=DIRECTION('ref_axis',(1.,0.,0.));
#141865=DIRECTION('center_axis',(1.83697019872103E-16,-1.83697019872104E-16,
1.));
#141866=DIRECTION('ref_axis',(-3.37445951098919E-32,-1.,-1.83697019872104E-16));
#141867=DIRECTION('',(-1.83697019872103E-16,1.83697019872104E-16,-1.));
#141868=DIRECTION('center_axis',(3.49148133884313E-15,1.,1.83697019872103E-16));
#141869=DIRECTION('ref_axis',(-1.,3.49148133884313E-15,0.));
#141870=DIRECTION('',(1.,-3.49148133884313E-15,0.));
#141871=DIRECTION('',(1.,-3.49148133884313E-15,-1.83697019872104E-16));
#141872=DIRECTION('',(-1.83697019872103E-16,1.83697019872104E-16,-1.));
#141873=DIRECTION('center_axis',(-1.,3.49148133884313E-15,1.83697019872104E-16));
#141874=DIRECTION('ref_axis',(-3.49148133884313E-15,-1.,1.78914547131776E-47));
#141875=DIRECTION('',(3.49148133884313E-15,1.,0.));
#141876=DIRECTION('',(3.49148133884313E-15,1.,1.83697019872103E-16));
#141877=DIRECTION('',(-1.83697019872103E-16,1.83697019872104E-16,-1.));
#141878=DIRECTION('center_axis',(3.49148133884313E-15,1.,1.83697019872103E-16));
#141879=DIRECTION('ref_axis',(-1.,3.49148133884313E-15,0.));
#141880=DIRECTION('',(1.,-3.49148133884313E-15,0.));
#141881=DIRECTION('',(1.,-3.49148133884313E-15,-1.83697019872104E-16));
#141882=DIRECTION('',(-1.83697019872103E-16,1.83697019872104E-16,-1.));
#141883=DIRECTION('center_axis',(-1.,3.49148133884313E-15,1.83697019872104E-16));
#141884=DIRECTION('ref_axis',(-3.49148133884313E-15,-1.,1.78914547131776E-47));
#141885=DIRECTION('',(3.49148133884313E-15,1.,0.));
#141886=DIRECTION('',(3.49148133884313E-15,1.,1.83697019872103E-16));
#141887=DIRECTION('',(-1.83697019872103E-16,1.83697019872104E-16,-1.));
#141888=DIRECTION('center_axis',(-1.83697019872103E-16,1.83697019872104E-16,
-1.));
#141889=DIRECTION('ref_axis',(3.37445951098919E-32,1.,1.83697019872104E-16));
#141890=DIRECTION('center_axis',(0.,0.,1.));
#141891=DIRECTION('ref_axis',(1.,0.,0.));
#141892=DIRECTION('center_axis',(1.83697019872103E-16,-1.83697019872104E-16,
1.));
#141893=DIRECTION('ref_axis',(-3.79423332453363E-15,-1.,-1.83697019872103E-16));
#141894=DIRECTION('',(-1.83697019872103E-16,1.83697019872104E-16,-1.));
#141895=DIRECTION('center_axis',(-3.90362756739548E-15,-1.,-1.83697019872103E-16));
#141896=DIRECTION('ref_axis',(1.,-3.90362756739548E-15,0.));
#141897=DIRECTION('',(-1.,3.90362756739548E-15,0.));
#141898=DIRECTION('',(-1.,3.90362756739548E-15,1.83697019872104E-16));
#141899=DIRECTION('',(-1.83697019872103E-16,1.83697019872104E-16,-1.));
#141900=DIRECTION('center_axis',(1.,-3.49148133884313E-15,-1.83697019872104E-16));
#141901=DIRECTION('ref_axis',(3.49148133884313E-15,1.,-1.78914547131776E-47));
#141902=DIRECTION('',(-3.49148133884313E-15,-1.,0.));
#141903=DIRECTION('',(-3.49148133884313E-15,-1.,-1.83697019872103E-16));
#141904=DIRECTION('',(-1.83697019872103E-16,1.83697019872104E-16,-1.));
#141905=DIRECTION('center_axis',(-3.49148133884313E-15,-1.,-1.83697019872103E-16));
#141906=DIRECTION('ref_axis',(1.,-3.49148133884313E-15,0.));
#141907=DIRECTION('',(-1.,3.49148133884313E-15,0.));
#141908=DIRECTION('',(-1.,3.49148133884313E-15,1.83697019872104E-16));
#141909=DIRECTION('',(-1.83697019872103E-16,1.83697019872104E-16,-1.));
#141910=DIRECTION('center_axis',(1.,-6.50839173184628E-15,-1.83697019872104E-16));
#141911=DIRECTION('ref_axis',(6.50839173184628E-15,1.,-4.21210294408139E-47));
#141912=DIRECTION('',(-6.50839173184628E-15,-1.,0.));
#141913=DIRECTION('',(-6.50839173184628E-15,-1.,-1.83697019872102E-16));
#141914=DIRECTION('',(-1.83697019872103E-16,1.83697019872104E-16,-1.));
#141915=DIRECTION('center_axis',(-1.83697019872103E-16,1.83697019872104E-16,
-1.));
#141916=DIRECTION('ref_axis',(3.37445951098919E-32,1.,1.83697019872104E-16));
#141917=DIRECTION('center_axis',(0.,0.,1.));
#141918=DIRECTION('ref_axis',(1.,0.,0.));
#141919=DIRECTION('center_axis',(1.83697019872103E-16,-1.83697019872104E-16,
1.));
#141920=DIRECTION('ref_axis',(-3.37445951098919E-32,-1.,-1.83697019872104E-16));
#141921=DIRECTION('',(-1.83697019872103E-16,1.83697019872104E-16,-1.));
#141922=DIRECTION('center_axis',(5.62652561696843E-15,1.,1.83697019872103E-16));
#141923=DIRECTION('ref_axis',(-1.,5.62652561696843E-15,0.));
#141924=DIRECTION('',(1.,-5.62652561696843E-15,0.));
#141925=DIRECTION('',(1.,-5.62652561696843E-15,-1.83697019872104E-16));
#141926=DIRECTION('',(-1.83697019872103E-16,1.83697019872104E-16,-1.));
#141927=DIRECTION('center_axis',(-1.83697019872103E-16,1.83697019872104E-16,
-1.));
#141928=DIRECTION('ref_axis',(3.37445951098919E-32,1.,1.83697019872104E-16));
#141929=DIRECTION('center_axis',(0.,0.,-1.));
#141930=DIRECTION('ref_axis',(1.,2.31296463463575E-14,0.));
#141931=DIRECTION('center_axis',(-1.83697019872103E-16,1.83697019872104E-16,
-1.));
#141932=DIRECTION('ref_axis',(-3.37445951098919E-32,-1.,-1.83697019872104E-16));
#141933=DIRECTION('',(-1.83697019872103E-16,1.83697019872104E-16,-1.));
#141934=DIRECTION('center_axis',(1.,-5.16340222821484E-15,-1.83697019872104E-16));
#141935=DIRECTION('ref_axis',(5.16340222821484E-15,1.,8.5317764086697E-47));
#141936=DIRECTION('',(-5.16340222821484E-15,-1.,0.));
#141937=DIRECTION('',(-5.16340222821484E-15,-1.,-1.83697019872103E-16));
#141938=DIRECTION('',(-1.83697019872103E-16,1.83697019872104E-16,-1.));
#141939=DIRECTION('center_axis',(-1.83697019872103E-16,1.83697019872104E-16,
-1.));
#141940=DIRECTION('ref_axis',(3.37445951098919E-32,1.,1.83697019872104E-16));
#141941=DIRECTION('center_axis',(0.,0.,-1.));
#141942=DIRECTION('ref_axis',(1.,0.,0.));
#141943=DIRECTION('center_axis',(-1.83697019872103E-16,1.83697019872104E-16,
-1.));
#141944=DIRECTION('ref_axis',(-3.37445951098919E-32,-1.,-1.83697019872104E-16));
#141945=DIRECTION('',(-1.83697019872103E-16,1.83697019872104E-16,-1.));
#141946=DIRECTION('center_axis',(0.707106781186545,-0.70710678118655,-2.59786816870649E-16));
#141947=DIRECTION('ref_axis',(0.70710678118655,0.707106781186545,1.41173070057919E-32));
#141948=DIRECTION('',(-0.70710678118655,-0.707106781186545,0.));
#141949=DIRECTION('',(-0.70710678118655,-0.707106781186545,4.68386162474976E-31));
#141950=DIRECTION('',(-1.83697019872103E-16,1.83697019872104E-16,-1.));
#141951=DIRECTION('center_axis',(-1.83697019872103E-16,1.83697019872104E-16,
-1.));
#141952=DIRECTION('ref_axis',(3.37445951098919E-32,1.,1.83697019872104E-16));
#141953=DIRECTION('center_axis',(0.,0.,-1.));
#141954=DIRECTION('ref_axis',(1.,7.70988211545249E-15,0.));
#141955=DIRECTION('center_axis',(-1.83697019872103E-16,1.83697019872104E-16,
-1.));
#141956=DIRECTION('ref_axis',(-3.37445951098919E-32,-1.,-1.83697019872104E-16));
#141957=DIRECTION('',(-1.83697019872103E-16,1.83697019872104E-16,-1.));
#141958=DIRECTION('center_axis',(-3.49148133884313E-15,-1.,-1.83697019872103E-16));
#141959=DIRECTION('ref_axis',(1.,-3.49148133884313E-15,0.));
#141960=DIRECTION('',(-1.,3.49148133884313E-15,0.));
#141961=DIRECTION('',(-1.,3.49148133884313E-15,1.83697019872104E-16));
#141962=DIRECTION('center_axis',(-0.866025403784438,-0.500000000000001,
-1.83697019872103E-16));
#141963=DIRECTION('ref_axis',(0.500000000000001,-0.866025403784438,2.0289671949304E-33));
#141964=DIRECTION('',(-0.5,0.866025403784438,0.));
#141965=DIRECTION('',(0.,3.67394039744206E-16,-1.));
#141966=DIRECTION('',(-0.5,0.866025403784438,3.18172571617472E-16));
#141967=DIRECTION('',(0.,3.67394039744206E-16,-1.));
#141968=DIRECTION('center_axis',(-0.866025403784438,0.500000000000002,1.83697019872104E-16));
#141969=DIRECTION('ref_axis',(-0.500000000000002,-0.866025403784437,9.7694722305658E-33));
#141970=DIRECTION('',(0.500000000000002,0.866025403784438,0.));
#141971=DIRECTION('',(0.500000000000002,0.866025403784438,3.18172571617472E-16));
#141972=DIRECTION('',(0.,3.67394039744206E-16,-1.));
#141973=DIRECTION('center_axis',(-1.,0.,0.));
#141974=DIRECTION('ref_axis',(0.,0.,1.));
#141975=DIRECTION('',(0.,1.,0.));
#141976=DIRECTION('',(0.,1.,3.67394039744206E-16));
#141977=DIRECTION('',(0.,3.67394039744206E-16,-1.));
#141978=DIRECTION('center_axis',(0.,3.67394039744206E-16,-1.));
#141979=DIRECTION('ref_axis',(0.,1.,3.67394039744206E-16));
#141980=DIRECTION('center_axis',(0.,0.,-1.));
#141981=DIRECTION('ref_axis',(1.,1.15648231731787E-14,0.));
#141982=DIRECTION('center_axis',(0.,3.67394039744206E-16,-1.));
#141983=DIRECTION('ref_axis',(1.,0.,0.));
#141984=DIRECTION('',(0.,3.67394039744206E-16,-1.));
#141985=DIRECTION('center_axis',(-0.707106781186548,0.707106781186548,2.59786816870648E-16));
#141986=DIRECTION('ref_axis',(-0.707106781186548,-0.707106781186548,1.22182752772918E-34));
#141987=DIRECTION('',(0.707106781186547,0.707106781186547,0.));
#141988=DIRECTION('',(0.707106781186547,0.707106781186547,2.59786816870648E-16));
#141989=DIRECTION('',(0.,3.67394039744206E-16,-1.));
#141990=DIRECTION('center_axis',(0.,3.67394039744206E-16,-1.));
#141991=DIRECTION('ref_axis',(0.,1.,3.67394039744206E-16));
#141992=DIRECTION('center_axis',(0.,0.,-1.));
#141993=DIRECTION('ref_axis',(1.,-7.70988211545249E-15,0.));
#141994=DIRECTION('center_axis',(0.,3.67394039744206E-16,-1.));
#141995=DIRECTION('ref_axis',(1.,0.,0.));
#141996=DIRECTION('',(0.,3.67394039744206E-16,-1.));
#141997=DIRECTION('center_axis',(-1.6719208893717E-15,1.,3.67394039744206E-16));
#141998=DIRECTION('ref_axis',(-1.,-1.6719208893717E-15,0.));
#141999=DIRECTION('',(1.,1.6719208893717E-15,0.));
#142000=DIRECTION('',(1.,1.6719208893717E-15,6.14253769678996E-31));
#142001=DIRECTION('',(0.,3.67394039744206E-16,-1.));
#142002=DIRECTION('center_axis',(0.,3.67394039744206E-16,-1.));
#142003=DIRECTION('ref_axis',(0.,1.,3.67394039744206E-16));
#142004=DIRECTION('center_axis',(0.,0.,-1.));
#142005=DIRECTION('ref_axis',(1.,0.,0.));
#142006=DIRECTION('center_axis',(0.,3.67394039744206E-16,-1.));
#142007=DIRECTION('ref_axis',(1.,0.,0.));
#142008=DIRECTION('',(0.,3.67394039744206E-16,-1.));
#142009=DIRECTION('center_axis',(1.,2.1350442781253E-15,7.84402542373206E-31));
#142010=DIRECTION('ref_axis',(-2.1350442781253E-15,1.,5.68845695218989E-62));
#142011=DIRECTION('',(2.1350442781253E-15,-1.,0.));
#142012=DIRECTION('',(2.1350442781253E-15,-1.,-3.67394039744206E-16));
#142013=DIRECTION('',(0.,3.67394039744206E-16,-1.));
#142014=DIRECTION('center_axis',(0.,3.67394039744206E-16,-1.));
#142015=DIRECTION('ref_axis',(0.,1.,3.67394039744206E-16));
#142016=DIRECTION('center_axis',(0.,0.,1.));
#142017=DIRECTION('ref_axis',(1.,0.,0.));
#142018=DIRECTION('center_axis',(0.,-3.67394039744206E-16,1.));
#142019=DIRECTION('ref_axis',(1.,0.,0.));
#142020=DIRECTION('',(0.,3.67394039744206E-16,-1.));
#142021=DIRECTION('center_axis',(-3.01691039300315E-15,1.,3.67394039744206E-16));
#142022=DIRECTION('ref_axis',(-1.,-3.01691039300315E-15,0.));
#142023=DIRECTION('',(1.,3.01691039300315E-15,0.));
#142024=DIRECTION('',(1.,3.01691039300315E-15,1.10839489683171E-30));
#142025=DIRECTION('',(0.,3.67394039744206E-16,-1.));
#142026=DIRECTION('center_axis',(-1.,0.,0.));
#142027=DIRECTION('ref_axis',(0.,0.,1.));
#142028=DIRECTION('',(0.,1.,0.));
#142029=DIRECTION('',(0.,1.,3.67394039744206E-16));
#142030=DIRECTION('',(0.,3.67394039744206E-16,-1.));
#142031=DIRECTION('center_axis',(0.,1.,3.67394039744206E-16));
#142032=DIRECTION('ref_axis',(0.,-3.67394039744206E-16,1.));
#142033=DIRECTION('',(1.,0.,0.));
#142034=DIRECTION('',(1.,0.,0.));
#142035=DIRECTION('center_axis',(7.30409884621813E-15,1.,3.67394039744206E-16));
#142036=DIRECTION('ref_axis',(-1.,7.30409884621813E-15,0.));
#142037=DIRECTION('',(1.,-7.30409884621813E-15,0.));
#142038=DIRECTION('',(1.83697019872103E-16,1.83697019872101E-16,-1.));
#142039=DIRECTION('',(1.,-7.30409884621813E-15,-2.68348238180307E-30));
#142040=DIRECTION('',(0.,3.67394039744206E-16,-1.));
#142041=DIRECTION('center_axis',(-1.,1.26161707343766E-14,4.63510593220524E-30));
#142042=DIRECTION('ref_axis',(-1.26161707343766E-14,-1.,-3.84512883862554E-60));
#142043=DIRECTION('',(1.26161707343766E-14,1.,0.));
#142044=DIRECTION('',(1.26161707343766E-14,1.,3.67394039744206E-16));
#142045=DIRECTION('',(0.,3.67394039744206E-16,-1.));
#142046=DIRECTION('center_axis',(6.30808536718845E-15,1.,3.67394039744206E-16));
#142047=DIRECTION('ref_axis',(-1.,6.30808536718845E-15,0.));
#142048=DIRECTION('',(1.,-6.30808536718845E-15,0.));
#142049=DIRECTION('',(1.,-6.30808536718845E-15,-2.31755296610268E-30));
#142050=DIRECTION('',(0.,3.67394039744206E-16,-1.));
#142051=DIRECTION('center_axis',(-1.,9.05073117900944E-15,3.32518469049512E-30));
#142052=DIRECTION('ref_axis',(-9.05073117900944E-15,-1.,1.73421017874153E-60));
#142053=DIRECTION('',(9.05073117900944E-15,1.,0.));
#142054=DIRECTION('',(9.05073117900944E-15,1.,3.67394039744206E-16));
#142055=DIRECTION('',(0.,3.67394039744206E-16,-1.));
#142056=DIRECTION('center_axis',(0.,3.67394039744206E-16,-1.));
#142057=DIRECTION('ref_axis',(0.,1.,3.67394039744206E-16));
#142058=DIRECTION('center_axis',(0.,0.,1.));
#142059=DIRECTION('ref_axis',(1.,0.,0.));
#142060=DIRECTION('center_axis',(0.,-3.67394039744206E-16,1.));
#142061=DIRECTION('ref_axis',(-1.,0.,0.));
#142062=DIRECTION('',(0.,3.67394039744206E-16,-1.));
#142063=DIRECTION('center_axis',(-8.5401771125012E-15,-1.,-3.67394039744206E-16));
#142064=DIRECTION('ref_axis',(1.,-8.5401771125012E-15,0.));
#142065=DIRECTION('',(-1.,8.5401771125012E-15,0.));
#142066=DIRECTION('',(-1.,8.5401771125012E-15,3.13761016949282E-30));
#142067=DIRECTION('',(0.,3.67394039744206E-16,-1.));
#142068=DIRECTION('center_axis',(0.,3.67394039744206E-16,-1.));
#142069=DIRECTION('ref_axis',(0.,1.,3.67394039744206E-16));
#142070=DIRECTION('center_axis',(0.,0.,-1.));
#142071=DIRECTION('ref_axis',(1.,0.,0.));
#142072=DIRECTION('center_axis',(0.,3.67394039744206E-16,-1.));
#142073=DIRECTION('ref_axis',(-1.,0.,0.));
#142074=DIRECTION('',(0.,3.67394039744206E-16,-1.));
#142075=DIRECTION('center_axis',(-1.,8.3596044468585E-15,3.07126884839497E-30));
#142076=DIRECTION('ref_axis',(-8.3596044468585E-15,-1.,-3.49500060354943E-61));
#142077=DIRECTION('',(8.3596044468585E-15,1.,0.));
#142078=DIRECTION('',(8.3596044468585E-15,1.,3.67394039744206E-16));
#142079=DIRECTION('',(0.,3.67394039744206E-16,-1.));
#142080=DIRECTION('center_axis',(0.,3.67394039744206E-16,-1.));
#142081=DIRECTION('ref_axis',(0.,1.,3.67394039744206E-16));
#142082=DIRECTION('center_axis',(0.,0.,-1.));
#142083=DIRECTION('ref_axis',(1.,7.70988211545251E-15,0.));
#142084=DIRECTION('center_axis',(0.,3.67394039744206E-16,-1.));
#142085=DIRECTION('ref_axis',(-1.,0.,0.));
#142086=DIRECTION('',(0.,3.67394039744206E-16,-1.));
#142087=DIRECTION('center_axis',(-0.707106781186542,0.707106781186553,2.5978681687065E-16));
#142088=DIRECTION('ref_axis',(-0.707106781186553,-0.707106781186542,-1.42399511956761E-32));
#142089=DIRECTION('',(0.707106781186553,0.707106781186542,0.));
#142090=DIRECTION('',(0.707106781186553,0.707106781186542,2.59786816870646E-16));
#142091=DIRECTION('',(0.,3.67394039744206E-16,-1.));
#142092=DIRECTION('center_axis',(0.,3.67394039744206E-16,-1.));
#142093=DIRECTION('ref_axis',(0.,1.,3.67394039744206E-16));
#142094=DIRECTION('center_axis',(0.,0.,-1.));
#142095=DIRECTION('ref_axis',(1.,-3.083952846181E-14,0.));
#142096=DIRECTION('center_axis',(0.,3.67394039744206E-16,-1.));
#142097=DIRECTION('ref_axis',(-1.,0.,0.));
#142098=DIRECTION('',(0.,3.67394039744206E-16,-1.));
#142099=DIRECTION('center_axis',(8.7284827903955E-15,1.,3.67394039744206E-16));
#142100=DIRECTION('ref_axis',(-1.,8.7284827903955E-15,0.));
#142101=DIRECTION('',(1.,-8.7284827903955E-15,0.));
#142102=DIRECTION('',(1.,-8.7284827903955E-15,-3.20679255320118E-30));
#142103=DIRECTION('',(0.,3.67394039744206E-16,-1.));
#142104=DIRECTION('center_axis',(-0.499999999999979,0.866025403784451,3.18172571617477E-16));
#142105=DIRECTION('ref_axis',(-0.866025403784451,-0.499999999999979,-4.69885821425642E-34));
#142106=DIRECTION('',(0.866025403784451,0.499999999999979,0.));
#142107=DIRECTION('',(0.866025403784451,0.499999999999979,1.83697019872095E-16));
#142108=DIRECTION('',(0.,3.67394039744206E-16,-1.));
#142109=DIRECTION('center_axis',(0.500000000000004,0.866025403784436,3.18172571617471E-16));
#142110=DIRECTION('ref_axis',(-0.866025403784436,0.500000000000004,-8.27337693045638E-33));
#142111=DIRECTION('',(0.866025403784436,-0.500000000000004,0.));
#142112=DIRECTION('',(0.866025403784436,-0.500000000000004,-1.83697019872104E-16));
#142113=DIRECTION('',(0.,3.67394039744206E-16,-1.));
#142114=DIRECTION('center_axis',(0.,1.,3.67394039744206E-16));
#142115=DIRECTION('ref_axis',(0.,-3.67394039744206E-16,1.));
#142116=DIRECTION('',(1.,0.,0.));
#142117=DIRECTION('',(1.,0.,0.));
#142118=DIRECTION('',(0.,3.67394039744206E-16,-1.));
#142119=DIRECTION('center_axis',(0.,3.67394039744206E-16,-1.));
#142120=DIRECTION('ref_axis',(0.,1.,3.67394039744206E-16));
#142121=DIRECTION('center_axis',(0.,0.,-1.));
#142122=DIRECTION('ref_axis',(1.,0.,0.));
#142123=DIRECTION('center_axis',(0.,3.67394039744206E-16,-1.));
#142124=DIRECTION('ref_axis',(-1.,0.,0.));
#142125=DIRECTION('',(0.,3.67394039744206E-16,-1.));
#142126=DIRECTION('center_axis',(0.707106781186548,0.707106781186548,2.59786816870648E-16));
#142127=DIRECTION('ref_axis',(-0.707106781186548,0.707106781186548,-1.22182752772918E-34));
#142128=DIRECTION('',(0.707106781186547,-0.707106781186547,0.));
#142129=DIRECTION('',(0.707106781186547,-0.707106781186547,-2.59786816870648E-16));
#142130=DIRECTION('',(0.,3.67394039744206E-16,-1.));
#142131=DIRECTION('center_axis',(0.,3.67394039744206E-16,-1.));
#142132=DIRECTION('ref_axis',(0.,1.,3.67394039744206E-16));
#142133=DIRECTION('center_axis',(0.,0.,-1.));
#142134=DIRECTION('ref_axis',(1.,0.,0.));
#142135=DIRECTION('center_axis',(0.,3.67394039744206E-16,-1.));
#142136=DIRECTION('ref_axis',(-1.,0.,0.));
#142137=DIRECTION('',(0.,3.67394039744206E-16,-1.));
#142138=DIRECTION('center_axis',(1.,0.,0.));
#142139=DIRECTION('ref_axis',(0.,0.,-1.));
#142140=DIRECTION('',(0.,-1.,0.));
#142141=DIRECTION('',(0.,-1.,-3.67394039744206E-16));
#142142=DIRECTION('',(0.,3.67394039744206E-16,-1.));
#142143=DIRECTION('center_axis',(0.,3.67394039744206E-16,-1.));
#142144=DIRECTION('ref_axis',(0.,1.,3.67394039744206E-16));
#142145=DIRECTION('center_axis',(0.,0.,-1.));
#142146=DIRECTION('ref_axis',(1.,0.,0.));
#142147=DIRECTION('center_axis',(0.,3.67394039744206E-16,-1.));
#142148=DIRECTION('ref_axis',(-1.,0.,0.));
#142149=DIRECTION('',(0.,3.67394039744206E-16,-1.));
#142150=DIRECTION('center_axis',(2.1350442781253E-15,-1.,-3.67394039744206E-16));
#142151=DIRECTION('ref_axis',(1.,2.1350442781253E-15,0.));
#142152=DIRECTION('',(-1.,-2.1350442781253E-15,0.));
#142153=DIRECTION('',(-1.,-2.1350442781253E-15,-7.84402542373207E-31));
#142154=DIRECTION('',(0.,3.67394039744206E-16,-1.));
#142155=DIRECTION('center_axis',(0.,3.67394039744206E-16,-1.));
#142156=DIRECTION('ref_axis',(0.,1.,3.67394039744206E-16));
#142157=DIRECTION('center_axis',(0.,0.,1.));
#142158=DIRECTION('ref_axis',(1.,0.,0.));
#142159=DIRECTION('center_axis',(0.,-3.67394039744206E-16,1.));
#142160=DIRECTION('ref_axis',(-1.,0.,0.));
#142161=DIRECTION('',(0.,3.67394039744206E-16,-1.));
#142162=DIRECTION('center_axis',(1.,0.,0.));
#142163=DIRECTION('ref_axis',(0.,0.,-1.));
#142164=DIRECTION('',(0.,-1.,0.));
#142165=DIRECTION('',(0.,-1.,-3.67394039744206E-16));
#142166=DIRECTION('',(0.,3.67394039744206E-16,-1.));
#142167=DIRECTION('center_axis',(0.,1.,3.67394039744206E-16));
#142168=DIRECTION('ref_axis',(0.,-3.67394039744206E-16,1.));
#142169=DIRECTION('',(1.,0.,0.));
#142170=DIRECTION('',(1.,0.,0.));
#142171=DIRECTION('',(0.,3.67394039744206E-16,-1.));
#142172=DIRECTION('center_axis',(1.,0.,0.));
#142173=DIRECTION('ref_axis',(0.,0.,-1.));
#142174=DIRECTION('',(0.,-1.,0.));
#142175=DIRECTION('',(0.,-1.,-3.67394039744206E-16));
#142176=DIRECTION('',(0.,3.67394039744206E-16,-1.));
#142177=DIRECTION('center_axis',(0.,1.,3.67394039744206E-16));
#142178=DIRECTION('ref_axis',(0.,-3.67394039744206E-16,1.));
#142179=DIRECTION('',(1.,0.,0.));
#142180=DIRECTION('',(1.,0.,0.));
#142181=DIRECTION('',(0.,3.67394039744206E-16,-1.));
#142182=DIRECTION('center_axis',(0.,3.67394039744206E-16,-1.));
#142183=DIRECTION('ref_axis',(0.,1.,3.67394039744206E-16));
#142184=DIRECTION('center_axis',(0.,0.,1.));
#142185=DIRECTION('ref_axis',(1.,0.,0.));
#142186=DIRECTION('center_axis',(0.,-3.67394039744206E-16,1.));
#142187=DIRECTION('ref_axis',(-1.,0.,0.));
#142188=DIRECTION('',(0.,3.67394039744206E-16,-1.));
#142189=DIRECTION('center_axis',(-1.,4.12146228552343E-16,1.51420067873184E-31));
#142190=DIRECTION('ref_axis',(-4.12146228552343E-16,-1.,5.13958017849863E-64));
#142191=DIRECTION('',(4.12146228552343E-16,1.,0.));
#142192=DIRECTION('',(4.12146228552343E-16,1.,3.67394039744206E-16));
#142193=DIRECTION('',(0.,3.67394039744206E-16,-1.));
#142194=DIRECTION('center_axis',(0.,-1.,-3.67394039744206E-16));
#142195=DIRECTION('ref_axis',(0.,3.67394039744206E-16,-1.));
#142196=DIRECTION('',(-1.,0.,0.));
#142197=DIRECTION('',(-1.,0.,0.));
#142198=DIRECTION('',(0.,3.67394039744206E-16,-1.));
#142199=DIRECTION('center_axis',(-1.,0.,0.));
#142200=DIRECTION('ref_axis',(0.,0.,1.));
#142201=DIRECTION('',(0.,1.,0.));
#142202=DIRECTION('',(0.,1.,3.67394039744206E-16));
#142203=DIRECTION('',(0.,3.67394039744206E-16,-1.));
#142204=DIRECTION('center_axis',(-3.01691039300315E-15,-1.,-3.67394039744206E-16));
#142205=DIRECTION('ref_axis',(1.,-3.01691039300315E-15,0.));
#142206=DIRECTION('',(-1.,3.01691039300315E-15,0.));
#142207=DIRECTION('',(-1.,3.01691039300315E-15,1.10839489683171E-30));
#142208=DIRECTION('',(0.,3.67394039744206E-16,-1.));
#142209=DIRECTION('center_axis',(0.,3.67394039744206E-16,-1.));
#142210=DIRECTION('ref_axis',(0.,1.,3.67394039744206E-16));
#142211=DIRECTION('center_axis',(0.,0.,1.));
#142212=DIRECTION('ref_axis',(1.,0.,0.));
#142213=DIRECTION('center_axis',(0.,-3.67394039744206E-16,1.));
#142214=DIRECTION('ref_axis',(-1.,0.,0.));
#142215=DIRECTION('',(0.,3.67394039744206E-16,-1.));
#142216=DIRECTION('center_axis',(1.,-2.1350442781253E-15,-7.84402542373206E-31));
#142217=DIRECTION('ref_axis',(2.1350442781253E-15,1.,5.68845695218989E-62));
#142218=DIRECTION('',(-2.1350442781253E-15,-1.,0.));
#142219=DIRECTION('',(-2.1350442781253E-15,-1.,-3.67394039744206E-16));
#142220=DIRECTION('',(0.,3.67394039744206E-16,-1.));
#142221=DIRECTION('center_axis',(0.,3.67394039744206E-16,-1.));
#142222=DIRECTION('ref_axis',(0.,1.,3.67394039744206E-16));
#142223=DIRECTION('center_axis',(0.,0.,-1.));
#142224=DIRECTION('ref_axis',(1.,0.,0.));
#142225=DIRECTION('center_axis',(0.,3.67394039744206E-16,-1.));
#142226=DIRECTION('ref_axis',(-1.,0.,0.));
#142227=DIRECTION('',(0.,3.67394039744206E-16,-1.));
#142228=DIRECTION('center_axis',(-1.6719208893717E-15,-1.,-3.67394039744206E-16));
#142229=DIRECTION('ref_axis',(1.,-1.6719208893717E-15,0.));
#142230=DIRECTION('',(-1.,1.6719208893717E-15,0.));
#142231=DIRECTION('',(-1.,1.6719208893717E-15,6.14253769678996E-31));
#142232=DIRECTION('',(0.,3.67394039744206E-16,-1.));
#142233=DIRECTION('center_axis',(0.,3.67394039744206E-16,-1.));
#142234=DIRECTION('ref_axis',(0.,1.,3.67394039744206E-16));
#142235=DIRECTION('center_axis',(0.,0.,-1.));
#142236=DIRECTION('ref_axis',(1.,0.,0.));
#142237=DIRECTION('center_axis',(0.,3.67394039744206E-16,-1.));
#142238=DIRECTION('ref_axis',(-1.,0.,0.));
#142239=DIRECTION('',(0.,3.67394039744206E-16,-1.));
#142240=DIRECTION('center_axis',(-0.707106781186548,-0.707106781186548,
-2.59786816870648E-16));
#142241=DIRECTION('ref_axis',(0.707106781186548,-0.707106781186548,1.22182752772918E-34));
#142242=DIRECTION('',(-0.707106781186547,0.707106781186547,0.));
#142243=DIRECTION('',(-0.707106781186547,0.707106781186547,2.59786816870648E-16));
#142244=DIRECTION('',(0.,3.67394039744206E-16,-1.));
#142245=DIRECTION('center_axis',(0.,3.67394039744206E-16,-1.));
#142246=DIRECTION('ref_axis',(0.,1.,3.67394039744206E-16));
#142247=DIRECTION('center_axis',(0.,0.,-1.));
#142248=DIRECTION('ref_axis',(1.,2.31296463463575E-14,0.));
#142249=DIRECTION('center_axis',(0.,3.67394039744206E-16,-1.));
#142250=DIRECTION('ref_axis',(-1.,0.,0.));
#142251=DIRECTION('',(0.,3.67394039744206E-16,-1.));
#142252=DIRECTION('center_axis',(-1.,0.,0.));
#142253=DIRECTION('ref_axis',(0.,0.,1.));
#142254=DIRECTION('',(0.,1.,0.));
#142255=DIRECTION('',(0.,1.,3.67394039744206E-16));
#142256=DIRECTION('center_axis',(-0.499999999999991,0.866025403784444,6.72377758726854E-17));
#142257=DIRECTION('ref_axis',(-0.866025403784444,-0.499999999999991,1.27198190524785E-33));
#142258=DIRECTION('',(0.866025403784444,0.499999999999991,0.));
#142259=DIRECTION('',(1.83697019872103E-16,1.83697019872101E-16,-1.));
#142260=DIRECTION('',(0.866025403784444,0.499999999999991,2.50934795744786E-16));
#142261=DIRECTION('',(1.83697019872103E-16,1.83697019872101E-16,-1.));
#142262=DIRECTION('center_axis',(0.500000000000011,0.866025403784432,2.50934795744787E-16));
#142263=DIRECTION('ref_axis',(-0.866025403784432,0.500000000000011,-2.44665721671821E-33));
#142264=DIRECTION('',(0.866025403784432,-0.500000000000011,0.));
#142265=DIRECTION('',(0.866025403784432,-0.500000000000011,6.72377758726823E-17));
#142266=DIRECTION('',(1.83697019872103E-16,1.83697019872101E-16,-1.));
#142267=DIRECTION('center_axis',(1.04744440165294E-14,1.,1.83697019872103E-16));
#142268=DIRECTION('ref_axis',(-1.,1.04744440165294E-14,0.));
#142269=DIRECTION('',(1.,-1.04744440165294E-14,0.));
#142270=DIRECTION('',(1.,-1.04744440165294E-14,1.83697019872101E-16));
#142271=DIRECTION('',(1.83697019872103E-16,1.83697019872101E-16,-1.));
#142272=DIRECTION('center_axis',(1.83697019872103E-16,1.83697019872101E-16,
-1.));
#142273=DIRECTION('ref_axis',(-1.,3.37445951098915E-32,-1.83697019872103E-16));
#142274=DIRECTION('center_axis',(0.,0.,-1.));
#142275=DIRECTION('ref_axis',(1.,-1.5419764230905E-14,0.));
#142276=DIRECTION('center_axis',(1.83697019872103E-16,1.83697019872101E-16,
-1.));
#142277=DIRECTION('ref_axis',(-1.15648231731787E-14,-1.,-1.83697019872103E-16));
#142278=DIRECTION('',(1.83697019872103E-16,1.83697019872101E-16,-1.));
#142279=DIRECTION('center_axis',(0.707106781186555,0.70710678118654,2.59786816870647E-16));
#142280=DIRECTION('ref_axis',(-0.70710678118654,0.707106781186555,3.44453791271169E-33));
#142281=DIRECTION('',(0.70710678118654,-0.707106781186555,0.));
#142282=DIRECTION('',(0.70710678118654,-0.707106781186555,-1.35585468084861E-30));
#142283=DIRECTION('',(1.83697019872103E-16,1.83697019872101E-16,-1.));
#142284=DIRECTION('center_axis',(1.83697019872103E-16,1.83697019872101E-16,
-1.));
#142285=DIRECTION('ref_axis',(-1.,3.37445951098915E-32,-1.83697019872103E-16));
#142286=DIRECTION('center_axis',(0.,0.,-1.));
#142287=DIRECTION('ref_axis',(1.,8.48087032699776E-14,0.));
#142288=DIRECTION('center_axis',(1.83697019872103E-16,1.83697019872101E-16,
-1.));
#142289=DIRECTION('ref_axis',(-9.63735264431562E-15,-1.,-1.83697019872103E-16));
#142290=DIRECTION('',(1.83697019872103E-16,1.83697019872101E-16,-1.));
#142291=DIRECTION('center_axis',(1.,-8.8025231271577E-15,1.83697019872101E-16));
#142292=DIRECTION('ref_axis',(8.8025231271577E-15,1.,8.2224033292669E-47));
#142293=DIRECTION('',(-8.8025231271577E-15,-1.,0.));
#142294=DIRECTION('',(-8.8025231271577E-15,-1.,-1.83697019872103E-16));
#142295=DIRECTION('',(1.83697019872103E-16,1.83697019872101E-16,-1.));
#142296=DIRECTION('center_axis',(1.83697019872103E-16,1.83697019872101E-16,
-1.));
#142297=DIRECTION('ref_axis',(-1.,3.37445951098915E-32,-1.83697019872103E-16));
#142298=DIRECTION('center_axis',(0.,0.,-1.));
#142299=DIRECTION('ref_axis',(1.,-7.70988211545246E-15,0.));
#142300=DIRECTION('center_axis',(1.83697019872103E-16,1.83697019872101E-16,
-1.));
#142301=DIRECTION('ref_axis',(-9.63735264431562E-15,-1.,-1.83697019872103E-16));
#142302=DIRECTION('',(1.83697019872103E-16,1.83697019872101E-16,-1.));
#142303=DIRECTION('center_axis',(-8.3393997384041E-15,-1.,-1.83697019872103E-16));
#142304=DIRECTION('ref_axis',(1.,-8.3393997384041E-15,0.));
#142305=DIRECTION('',(-1.,8.3393997384041E-15,0.));
#142306=DIRECTION('',(-1.,8.3393997384041E-15,-1.83697019872101E-16));
#142307=DIRECTION('',(1.83697019872103E-16,1.83697019872101E-16,-1.));
#142308=DIRECTION('center_axis',(1.83697019872103E-16,1.83697019872101E-16,
-1.));
#142309=DIRECTION('ref_axis',(-1.,3.37445951098914E-32,-1.83697019872103E-16));
#142310=DIRECTION('center_axis',(0.,0.,1.));
#142311=DIRECTION('ref_axis',(1.,0.,0.));
#142312=DIRECTION('center_axis',(-1.83697019872103E-16,-1.83697019872101E-16,
1.));
#142313=DIRECTION('ref_axis',(-1.15648231731788E-14,-1.,-1.83697019872103E-16));
#142314=DIRECTION('',(1.83697019872103E-16,1.83697019872101E-16,-1.));
#142315=DIRECTION('center_axis',(1.,-7.45753362352625E-15,1.83697019872102E-16));
#142316=DIRECTION('ref_axis',(7.45753362352625E-15,1.,-6.66549012489188E-47));
#142317=DIRECTION('',(-7.45753362352626E-15,-1.,0.));
#142318=DIRECTION('',(-7.45753362352626E-15,-1.,-1.83697019872102E-16));
#142319=DIRECTION('',(1.83697019872103E-16,1.83697019872101E-16,-1.));
#142320=DIRECTION('center_axis',(1.04744440165294E-14,1.,1.83697019872103E-16));
#142321=DIRECTION('ref_axis',(-1.,1.04744440165294E-14,0.));
#142322=DIRECTION('',(1.,-1.04744440165294E-14,0.));
#142323=DIRECTION('',(1.,-1.04744440165294E-14,1.83697019872101E-16));
#142324=DIRECTION('',(1.83697019872103E-16,1.83697019872101E-16,-1.));
#142325=DIRECTION('center_axis',(1.,-1.04744440165294E-14,1.83697019872101E-16));
#142326=DIRECTION('ref_axis',(1.04744440165294E-14,1.,1.01856090860782E-46));
#142327=DIRECTION('',(-1.04744440165294E-14,-1.,0.));
#142328=DIRECTION('',(-1.04744440165294E-14,-1.,-1.83697019872103E-16));
#142329=DIRECTION('center_axis',(2.3090614750906E-14,1.,1.83697019872105E-16));
#142330=DIRECTION('ref_axis',(-1.,2.3090614750906E-14,0.));
#142331=DIRECTION('',(1.,-2.3090614750906E-14,0.));
#142332=DIRECTION('',(1.,-2.3090614750906E-14,1.83697019872099E-16));
#142333=DIRECTION('',(1.83697019872103E-16,1.83697019872101E-16,-1.));
#142334=DIRECTION('center_axis',(1.,-1.67825293837178E-14,1.836970198721E-16));
#142335=DIRECTION('ref_axis',(1.67825293837178E-14,1.,-3.45098319227062E-48));
#142336=DIRECTION('',(-1.67825293837178E-14,-1.,0.));
#142337=DIRECTION('',(-1.67825293837178E-14,-1.,-1.83697019872104E-16));
#142338=DIRECTION('',(1.83697019872103E-16,1.83697019872101E-16,-1.));
#142339=DIRECTION('center_axis',(1.95251751955388E-14,1.,1.83697019872105E-16));
#142340=DIRECTION('ref_axis',(-1.,1.95251751955388E-14,0.));
#142341=DIRECTION('',(1.,-1.95251751955388E-14,0.));
#142342=DIRECTION('',(1.,-1.95251751955388E-14,1.83697019872099E-16));
#142343=DIRECTION('',(1.83697019872103E-16,1.83697019872101E-16,-1.));
#142344=DIRECTION('center_axis',(1.83697019872103E-16,1.83697019872101E-16,
-1.));
#142345=DIRECTION('ref_axis',(-1.,3.37445951098914E-32,-1.83697019872103E-16));
#142346=DIRECTION('center_axis',(0.,0.,1.));
#142347=DIRECTION('ref_axis',(1.,0.,0.));
#142348=DIRECTION('center_axis',(-1.83697019872103E-16,-1.83697019872101E-16,
1.));
#142349=DIRECTION('ref_axis',(7.70988211545252E-15,1.,1.83697019872102E-16));
#142350=DIRECTION('',(1.83697019872103E-16,1.83697019872101E-16,-1.));
#142351=DIRECTION('center_axis',(-1.,1.90146211290306E-14,-1.836970198721E-16));
#142352=DIRECTION('ref_axis',(-1.90146211290306E-14,-1.,-5.41562530658295E-47));
#142353=DIRECTION('',(1.90146211290306E-14,1.,0.));
#142354=DIRECTION('',(1.90146211290306E-14,1.,1.83697019872105E-16));
#142355=DIRECTION('',(1.83697019872103E-16,1.83697019872101E-16,-1.));
#142356=DIRECTION('center_axis',(1.83697019872103E-16,1.83697019872101E-16,
-1.));
#142357=DIRECTION('ref_axis',(-1.,3.37445951098915E-32,-1.83697019872103E-16));
#142358=DIRECTION('center_axis',(0.,0.,-1.));
#142359=DIRECTION('ref_axis',(1.,0.,0.));
#142360=DIRECTION('center_axis',(1.83697019872103E-16,1.83697019872101E-16,
-1.));
#142361=DIRECTION('ref_axis',(7.70988211545246E-15,1.,1.83697019872102E-16));
#142362=DIRECTION('',(1.83697019872103E-16,1.83697019872101E-16,-1.));
#142363=DIRECTION('center_axis',(1.88340484633879E-14,1.,1.83697019872105E-16));
#142364=DIRECTION('ref_axis',(-1.,1.88340484633879E-14,0.));
#142365=DIRECTION('',(1.,-1.88340484633879E-14,0.));
#142366=DIRECTION('',(1.,-1.88340484633879E-14,1.836970198721E-16));
#142367=DIRECTION('',(1.83697019872103E-16,1.83697019872101E-16,-1.));
#142368=DIRECTION('center_axis',(1.83697019872103E-16,1.83697019872101E-16,
-1.));
#142369=DIRECTION('ref_axis',(-1.,3.37445951098915E-32,-1.83697019872103E-16));
#142370=DIRECTION('center_axis',(0.,0.,-1.));
#142371=DIRECTION('ref_axis',(1.,2.31296463463575E-14,0.));
#142372=DIRECTION('center_axis',(1.83697019872103E-16,1.83697019872101E-16,
-1.));
#142373=DIRECTION('ref_axis',(7.70988211545251E-15,1.,1.83697019872102E-16));
#142374=DIRECTION('',(1.83697019872103E-16,1.83697019872101E-16,-1.));
#142375=DIRECTION('center_axis',(0.70710678118656,0.707106781186535,2.59786816870647E-16));
#142376=DIRECTION('ref_axis',(-0.707106781186535,0.70710678118656,-1.00703162523782E-33));
#142377=DIRECTION('',(0.707106781186535,-0.70710678118656,0.));
#142378=DIRECTION('',(0.707106781186535,-0.70710678118656,-3.27870313732483E-30));
#142379=DIRECTION('',(1.83697019872103E-16,1.83697019872101E-16,-1.));
#142380=DIRECTION('center_axis',(1.83697019872103E-16,1.83697019872101E-16,
-1.));
#142381=DIRECTION('ref_axis',(-1.,3.37445951098915E-32,-1.83697019872103E-16));
#142382=DIRECTION('center_axis',(0.,0.,-1.));
#142383=DIRECTION('ref_axis',(1.,1.11793290674061E-13,0.));
#142384=DIRECTION('center_axis',(1.83697019872103E-16,1.83697019872101E-16,
-1.));
#142385=DIRECTION('ref_axis',(7.70988211545249E-15,1.,1.83697019872103E-16));
#142386=DIRECTION('',(1.83697019872103E-16,1.83697019872101E-16,-1.));
#142387=DIRECTION('center_axis',(1.,-1.92029268069249E-14,1.83697019872099E-16));
#142388=DIRECTION('ref_axis',(1.92029268069249E-14,1.,-2.4224977382315E-46));
#142389=DIRECTION('',(-1.92029268069249E-14,-1.,0.));
#142390=DIRECTION('',(-1.92029268069249E-14,-1.,-1.83697019872105E-16));
#142391=DIRECTION('',(1.83697019872103E-16,1.83697019872101E-16,-1.));
#142392=DIRECTION('center_axis',(0.866025403784456,0.49999999999997,2.50934795744784E-16));
#142393=DIRECTION('ref_axis',(-0.49999999999997,0.866025403784456,3.80143372866314E-33));
#142394=DIRECTION('',(0.49999999999997,-0.866025403784456,0.));
#142395=DIRECTION('',(0.49999999999997,-0.866025403784456,-6.72377758726917E-17));
#142396=DIRECTION('',(1.83697019872103E-16,1.83697019872101E-16,-1.));
#142397=DIRECTION('center_axis',(0.866025403784431,-0.500000000000013,6.72377758726818E-17));
#142398=DIRECTION('ref_axis',(0.500000000000013,0.866025403784431,-1.6659815170822E-33));
#142399=DIRECTION('',(-0.500000000000013,-0.866025403784431,0.));
#142400=DIRECTION('',(-0.500000000000013,-0.866025403784431,-2.50934795744787E-16));
#142401=DIRECTION('',(1.83697019872103E-16,1.83697019872101E-16,-1.));
#142402=DIRECTION('center_axis',(1.,-1.04744440165294E-14,1.83697019872101E-16));
#142403=DIRECTION('ref_axis',(1.04744440165294E-14,1.,1.01856090860782E-46));
#142404=DIRECTION('',(-1.04744440165294E-14,-1.,0.));
#142405=DIRECTION('',(-1.04744440165294E-14,-1.,-1.83697019872103E-16));
#142406=DIRECTION('',(1.83697019872103E-16,1.83697019872101E-16,-1.));
#142407=DIRECTION('center_axis',(1.83697019872103E-16,1.83697019872101E-16,
-1.));
#142408=DIRECTION('ref_axis',(-1.,3.37445951098915E-32,-1.83697019872103E-16));
#142409=DIRECTION('center_axis',(0.,0.,-1.));
#142410=DIRECTION('ref_axis',(1.,-7.70988211545249E-15,0.));
#142411=DIRECTION('center_axis',(1.83697019872103E-16,1.83697019872101E-16,
-1.));
#142412=DIRECTION('ref_axis',(7.70988211545249E-15,1.,1.83697019872103E-16));
#142413=DIRECTION('',(1.83697019872103E-16,1.83697019872101E-16,-1.));
#142414=DIRECTION('center_axis',(0.70710678118654,-0.707106781186555,-1.36533618211329E-30));
#142415=DIRECTION('ref_axis',(0.707106781186555,0.70710678118654,3.7321785051642E-47));
#142416=DIRECTION('',(-0.707106781186555,-0.70710678118654,0.));
#142417=DIRECTION('',(-0.707106781186555,-0.70710678118654,-2.59786816870647E-16));
#142418=DIRECTION('',(1.83697019872103E-16,1.83697019872101E-16,-1.));
#142419=DIRECTION('center_axis',(1.83697019872103E-16,1.83697019872101E-16,
-1.));
#142420=DIRECTION('ref_axis',(-1.,3.37445951098915E-32,-1.83697019872103E-16));
#142421=DIRECTION('center_axis',(0.,0.,-1.));
#142422=DIRECTION('ref_axis',(1.,0.,0.));
#142423=DIRECTION('center_axis',(1.83697019872103E-16,1.83697019872101E-16,
-1.));
#142424=DIRECTION('ref_axis',(7.70988211545249E-15,1.,1.83697019872103E-16));
#142425=DIRECTION('',(1.83697019872103E-16,1.83697019872101E-16,-1.));
#142426=DIRECTION('center_axis',(-1.04744440165294E-14,-1.,-1.83697019872103E-16));
#142427=DIRECTION('ref_axis',(1.,-1.04744440165294E-14,0.));
#142428=DIRECTION('',(-1.,1.04744440165294E-14,0.));
#142429=DIRECTION('',(-1.,1.04744440165294E-14,-1.83697019872101E-16));
#142430=DIRECTION('',(1.83697019872103E-16,1.83697019872101E-16,-1.));
#142431=DIRECTION('center_axis',(1.83697019872103E-16,1.83697019872101E-16,
-1.));
#142432=DIRECTION('ref_axis',(-1.,3.37445951098914E-32,-1.83697019872103E-16));
#142433=DIRECTION('center_axis',(0.,0.,-1.));
#142434=DIRECTION('ref_axis',(1.,0.,0.));
#142435=DIRECTION('center_axis',(1.83697019872103E-16,1.83697019872101E-16,
-1.));
#142436=DIRECTION('ref_axis',(7.70988211545255E-15,1.,1.83697019872102E-16));
#142437=DIRECTION('',(1.83697019872103E-16,1.83697019872101E-16,-1.));
#142438=DIRECTION('center_axis',(-1.,8.3393997384041E-15,-1.83697019872101E-16));
#142439=DIRECTION('ref_axis',(-8.3393997384041E-15,-1.,-6.10222580802198E-47));
#142440=DIRECTION('',(8.3393997384041E-15,1.,0.));
#142441=DIRECTION('',(8.3393997384041E-15,1.,1.83697019872103E-16));
#142442=DIRECTION('',(1.83697019872103E-16,1.83697019872101E-16,-1.));
#142443=DIRECTION('center_axis',(1.83697019872103E-16,1.83697019872101E-16,
-1.));
#142444=DIRECTION('ref_axis',(-1.,3.37445951098915E-32,-1.83697019872103E-16));
#142445=DIRECTION('center_axis',(0.,0.,1.));
#142446=DIRECTION('ref_axis',(1.,0.,0.));
#142447=DIRECTION('center_axis',(-1.83697019872103E-16,-1.83697019872101E-16,
1.));
#142448=DIRECTION('ref_axis',(7.70988211545249E-15,1.,1.83697019872103E-16));
#142449=DIRECTION('',(1.83697019872103E-16,1.83697019872101E-16,-1.));
#142450=DIRECTION('center_axis',(-1.04744440165294E-14,-1.,-1.83697019872103E-16));
#142451=DIRECTION('ref_axis',(1.,-1.04744440165294E-14,0.));
#142452=DIRECTION('',(-1.,1.04744440165294E-14,0.));
#142453=DIRECTION('',(-1.,1.04744440165294E-14,-1.83697019872101E-16));
#142454=DIRECTION('',(1.83697019872103E-16,1.83697019872101E-16,-1.));
#142455=DIRECTION('center_axis',(1.,-1.04744440165294E-14,1.83697019872101E-16));
#142456=DIRECTION('ref_axis',(1.04744440165294E-14,1.,1.01856090860782E-46));
#142457=DIRECTION('',(-1.04744440165294E-14,-1.,0.));
#142458=DIRECTION('',(-1.04744440165294E-14,-1.,-1.83697019872103E-16));
#142459=DIRECTION('',(1.83697019872103E-16,1.83697019872101E-16,-1.));
#142460=DIRECTION('center_axis',(-1.04744440165294E-14,-1.,-1.83697019872103E-16));
#142461=DIRECTION('ref_axis',(1.,-1.04744440165294E-14,0.));
#142462=DIRECTION('',(-1.,1.04744440165294E-14,0.));
#142463=DIRECTION('',(-1.,1.04744440165294E-14,-1.83697019872101E-16));
#142464=DIRECTION('',(1.83697019872103E-16,1.83697019872101E-16,-1.));
#142465=DIRECTION('center_axis',(1.,-1.04744440165294E-14,1.83697019872101E-16));
#142466=DIRECTION('ref_axis',(1.04744440165294E-14,1.,1.01856090860782E-46));
#142467=DIRECTION('',(-1.04744440165294E-14,-1.,0.));
#142468=DIRECTION('',(-1.04744440165294E-14,-1.,-1.83697019872103E-16));
#142469=DIRECTION('',(1.83697019872103E-16,1.83697019872101E-16,-1.));
#142470=DIRECTION('center_axis',(1.83697019872103E-16,1.83697019872101E-16,
-1.));
#142471=DIRECTION('ref_axis',(-1.,3.37445951098915E-32,-1.83697019872103E-16));
#142472=DIRECTION('center_axis',(0.,0.,1.));
#142473=DIRECTION('ref_axis',(1.,0.,0.));
#142474=DIRECTION('center_axis',(-1.83697019872103E-16,-1.83697019872101E-16,
1.));
#142475=DIRECTION('ref_axis',(1.13826999736009E-14,1.,1.83697019872103E-16));
#142476=DIRECTION('',(1.83697019872103E-16,1.83697019872101E-16,-1.));
#142477=DIRECTION('center_axis',(1.08865902450817E-14,1.,1.83697019872103E-16));
#142478=DIRECTION('ref_axis',(-1.,1.08865902450817E-14,0.));
#142479=DIRECTION('',(1.,-1.08865902450817E-14,0.));
#142480=DIRECTION('',(1.,-1.08865902450817E-14,1.83697019872101E-16));
#142481=DIRECTION('',(1.83697019872103E-16,1.83697019872101E-16,-1.));
#142482=DIRECTION('center_axis',(-1.,1.04744440165294E-14,-1.83697019872101E-16));
#142483=DIRECTION('ref_axis',(-1.04744440165294E-14,-1.,-1.01856090860782E-46));
#142484=DIRECTION('',(1.04744440165294E-14,1.,0.));
#142485=DIRECTION('',(1.04744440165294E-14,1.,1.83697019872103E-16));
#142486=DIRECTION('',(1.83697019872103E-16,1.83697019872101E-16,-1.));
#142487=DIRECTION('center_axis',(1.04744440165294E-14,1.,1.83697019872103E-16));
#142488=DIRECTION('ref_axis',(-1.,1.04744440165294E-14,0.));
#142489=DIRECTION('',(1.,-1.04744440165294E-14,0.));
#142490=DIRECTION('',(1.,-1.04744440165294E-14,1.83697019872101E-16));
#142491=DIRECTION('',(1.83697019872103E-16,1.83697019872101E-16,-1.));
#142492=DIRECTION('center_axis',(-1.,1.34913544095325E-14,-1.83697019872101E-16));
#142493=DIRECTION('ref_axis',(-1.34913544095325E-14,-1.,-1.3549484701482E-46));
#142494=DIRECTION('',(1.34913544095325E-14,1.,0.));
#142495=DIRECTION('',(1.34913544095325E-14,1.,1.83697019872104E-16));
#142496=DIRECTION('',(1.83697019872103E-16,1.83697019872101E-16,-1.));
#142497=DIRECTION('center_axis',(1.83697019872103E-16,1.83697019872101E-16,
-1.));
#142498=DIRECTION('ref_axis',(-1.,3.37445951098914E-32,-1.83697019872103E-16));
#142499=DIRECTION('center_axis',(0.,0.,1.));
#142500=DIRECTION('ref_axis',(1.,0.,0.));
#142501=DIRECTION('center_axis',(-1.83697019872103E-16,-1.83697019872101E-16,
1.));
#142502=DIRECTION('ref_axis',(7.70988211545255E-15,1.,1.83697019872102E-16));
#142503=DIRECTION('',(1.83697019872103E-16,1.83697019872101E-16,-1.));
#142504=DIRECTION('center_axis',(-1.26094882946547E-14,-1.,-1.83697019872103E-16));
#142505=DIRECTION('ref_axis',(1.,-1.26094882946547E-14,0.));
#142506=DIRECTION('',(-1.,1.26094882946547E-14,0.));
#142507=DIRECTION('',(-1.,1.26094882946547E-14,-1.83697019872101E-16));
#142508=DIRECTION('',(1.83697019872103E-16,1.83697019872101E-16,-1.));
#142509=DIRECTION('center_axis',(1.83697019872103E-16,1.83697019872101E-16,
-1.));
#142510=DIRECTION('ref_axis',(-1.,3.37445951098915E-32,-1.83697019872103E-16));
#142511=DIRECTION('center_axis',(0.,0.,-1.));
#142512=DIRECTION('ref_axis',(1.,0.,0.));
#142513=DIRECTION('center_axis',(1.83697019872103E-16,1.83697019872101E-16,
-1.));
#142514=DIRECTION('ref_axis',(7.70988211545249E-15,1.,1.83697019872103E-16));
#142515=DIRECTION('',(1.83697019872103E-16,1.83697019872101E-16,-1.));
#142516=DIRECTION('center_axis',(-1.,1.21463649059011E-14,-1.83697019872101E-16));
#142517=DIRECTION('ref_axis',(-1.21463649059011E-14,-1.,-1.73669008789231E-46));
#142518=DIRECTION('',(1.21463649059011E-14,1.,0.));
#142519=DIRECTION('',(1.21463649059011E-14,1.,1.83697019872103E-16));
#142520=DIRECTION('',(1.83697019872103E-16,1.83697019872101E-16,-1.));
#142521=DIRECTION('center_axis',(1.83697019872103E-16,1.83697019872101E-16,
-1.));
#142522=DIRECTION('ref_axis',(-1.,3.37445951098915E-32,-1.83697019872103E-16));
#142523=DIRECTION('center_axis',(0.,0.,-1.));
#142524=DIRECTION('ref_axis',(1.,0.,0.));
#142525=DIRECTION('center_axis',(1.83697019872103E-16,1.83697019872101E-16,
-1.));
#142526=DIRECTION('ref_axis',(7.70988211545249E-15,1.,1.83697019872103E-16));
#142527=DIRECTION('',(1.83697019872103E-16,1.83697019872101E-16,-1.));
#142528=DIRECTION('center_axis',(-0.70710678118654,0.707106781186555,1.36533618211329E-30));
#142529=DIRECTION('ref_axis',(-0.707106781186555,-0.70710678118654,-3.7321785051642E-47));
#142530=DIRECTION('',(0.707106781186555,0.70710678118654,0.));
#142531=DIRECTION('',(0.707106781186555,0.70710678118654,2.59786816870647E-16));
#142532=DIRECTION('',(1.83697019872103E-16,1.83697019872101E-16,-1.));
#142533=DIRECTION('center_axis',(1.83697019872103E-16,1.83697019872101E-16,
-1.));
#142534=DIRECTION('ref_axis',(-1.,3.37445951098915E-32,-1.83697019872103E-16));
#142535=DIRECTION('center_axis',(0.,0.,-1.));
#142536=DIRECTION('ref_axis',(1.,3.083952846181E-14,0.));
#142537=DIRECTION('center_axis',(1.83697019872103E-16,1.83697019872101E-16,
-1.));
#142538=DIRECTION('ref_axis',(7.70988211545249E-15,1.,1.83697019872103E-16));
#142539=DIRECTION('',(1.83697019872103E-16,1.83697019872101E-16,-1.));
#142540=DIRECTION('center_axis',(1.04744440165294E-14,1.,1.83697019872103E-16));
#142541=DIRECTION('ref_axis',(-1.,1.04744440165294E-14,0.));
#142542=DIRECTION('',(1.,-1.04744440165294E-14,0.));
#142543=DIRECTION('',(1.,-1.04744440165294E-14,1.83697019872101E-16));
#142544=DIRECTION('center_axis',(-0.707106781186542,0.707106781186553,0.));
#142545=DIRECTION('ref_axis',(-0.707106781186553,-0.707106781186542,0.));
#142546=DIRECTION('',(0.707106781186553,0.707106781186542,0.));
#142547=DIRECTION('',(0.,0.,1.));
#142548=DIRECTION('',(0.707106781186553,0.707106781186542,0.));
#142549=DIRECTION('center_axis',(-0.70710678118655,-0.707106781186545,0.));
#142550=DIRECTION('ref_axis',(0.707106781186545,-0.70710678118655,0.));
#142551=DIRECTION('',(-0.707106781186545,0.70710678118655,0.));
#142552=DIRECTION('',(-0.707106781186545,0.70710678118655,0.));
#142553=DIRECTION('center_axis',(-0.70710678118655,0.707106781186545,0.));
#142554=DIRECTION('ref_axis',(-0.707106781186545,-0.70710678118655,0.));
#142555=DIRECTION('',(0.707106781186545,0.70710678118655,0.));
#142556=DIRECTION('',(0.707106781186545,0.70710678118655,0.));
#142557=DIRECTION('',(0.,0.,1.));
#142558=DIRECTION('center_axis',(0.70710678118655,0.707106781186545,0.));
#142559=DIRECTION('ref_axis',(-0.707106781186545,0.70710678118655,0.));
#142560=DIRECTION('',(0.707106781186545,-0.70710678118655,0.));
#142561=DIRECTION('',(0.707106781186545,-0.70710678118655,0.));
#142562=DIRECTION('center_axis',(0.,0.,-1.));
#142563=DIRECTION('ref_axis',(-1.,0.,0.));
#142564=DIRECTION('',(0.,1.,0.));
#142565=DIRECTION('',(1.,-1.21430643318376E-16,0.));
#142566=DIRECTION('',(-3.25988935000123E-16,-1.,0.));
#142567=DIRECTION('',(1.,0.,0.));
#142568=DIRECTION('',(0.,1.,0.));
#142569=DIRECTION('',(1.,-1.21430643318376E-16,0.));
#142570=DIRECTION('',(0.,1.,0.));
#142571=DIRECTION('',(-1.,0.,0.));
#142572=DIRECTION('center_axis',(0.,1.,0.));
#142573=DIRECTION('ref_axis',(0.,0.,1.));
#142574=DIRECTION('',(-1.,0.,0.));
#142575=DIRECTION('',(0.,0.,1.));
#142576=DIRECTION('',(0.,0.,1.));
#142577=DIRECTION('center_axis',(1.,0.,0.));
#142578=DIRECTION('ref_axis',(0.,0.,-1.));
#142579=DIRECTION('',(0.,1.,0.));
#142580=DIRECTION('',(0.,0.,1.));
#142581=DIRECTION('center_axis',(-1.21430643318376E-16,-1.,0.));
#142582=DIRECTION('ref_axis',(1.,-1.21430643318376E-16,0.));
#142583=DIRECTION('',(1.,-1.21430643318376E-16,0.));
#142584=DIRECTION('',(0.,0.,1.));
#142585=DIRECTION('center_axis',(1.,0.,0.));
#142586=DIRECTION('ref_axis',(0.,0.,-1.));
#142587=DIRECTION('',(0.,1.,0.));
#142588=DIRECTION('',(0.,0.,1.));
#142589=DIRECTION('center_axis',(0.,-1.,0.));
#142590=DIRECTION('ref_axis',(0.,0.,-1.));
#142591=DIRECTION('',(1.,0.,0.));
#142592=DIRECTION('',(0.,0.,1.));
#142593=DIRECTION('center_axis',(-1.,3.25988935000123E-16,0.));
#142594=DIRECTION('ref_axis',(-3.25988935000123E-16,-1.,0.));
#142595=DIRECTION('',(-3.25988935000123E-16,-1.,0.));
#142596=DIRECTION('',(0.,0.,1.));
#142597=DIRECTION('center_axis',(-1.21430643318376E-16,-1.,0.));
#142598=DIRECTION('ref_axis',(1.,-1.21430643318376E-16,0.));
#142599=DIRECTION('',(1.,-1.21430643318376E-16,0.));
#142600=DIRECTION('',(0.,0.,1.));
#142601=DIRECTION('center_axis',(1.,0.,0.));
#142602=DIRECTION('ref_axis',(0.,0.,-1.));
#142603=DIRECTION('',(0.,1.,0.));
#142604=DIRECTION('center_axis',(0.,0.,-1.));
#142605=DIRECTION('ref_axis',(-1.,0.,0.));
#142606=DIRECTION('center_axis',(-1.60944926250024E-16,1.,0.));
#142607=DIRECTION('ref_axis',(-1.,-1.60944926250024E-16,0.));
#142608=DIRECTION('',(-1.,-1.60944926250024E-16,0.));
#142609=DIRECTION('',(0.,0.,1.));
#142610=DIRECTION('',(-1.,-1.60944926250024E-16,0.));
#142611=DIRECTION('',(0.,0.,1.));
#142612=DIRECTION('center_axis',(-1.,0.,0.));
#142613=DIRECTION('ref_axis',(0.,0.,1.));
#142614=DIRECTION('',(0.,-1.,0.));
#142615=DIRECTION('',(0.,-1.,0.));
#142616=DIRECTION('',(0.,0.,1.));
#142617=DIRECTION('center_axis',(0.,-1.,0.));
#142618=DIRECTION('ref_axis',(0.,0.,-1.));
#142619=DIRECTION('',(1.,0.,0.));
#142620=DIRECTION('',(1.,0.,0.));
#142621=DIRECTION('',(0.,0.,1.));
#142622=DIRECTION('center_axis',(1.,0.,0.));
#142623=DIRECTION('ref_axis',(0.,0.,-1.));
#142624=DIRECTION('',(0.,1.,0.));
#142625=DIRECTION('',(0.,1.,0.));
#142626=DIRECTION('center_axis',(0.,0.,1.));
#142627=DIRECTION('ref_axis',(1.,0.,0.));
#142628=DIRECTION('center_axis',(0.,0.,-1.));
#142629=DIRECTION('ref_axis',(-1.,0.,0.));
#142630=DIRECTION('',(0.,0.,1.));
#142631=DIRECTION('',(1.,0.,0.));
#142632=DIRECTION('',(-1.42498634743018E-16,1.,5.98572430163289E-17));
#142633=DIRECTION('',(0.471567925465437,1.19981682658555E-16,-0.881829740750573));
#142634=DIRECTION('',(-6.83218119858761E-32,-1.,0.));
#142635=DIRECTION('',(1.,-6.83218119858761E-32,1.22464679914748E-16));
#142636=DIRECTION('',(3.49433275961834E-17,-1.,-1.17373598748286E-16));
#142637=DIRECTION('',(-0.214157326328102,-1.22133804713983E-16,0.976799180783849));
#142638=DIRECTION('',(0.,0.,-1.));
#142639=DIRECTION('',(-1.,0.,0.));
#142640=DIRECTION('',(2.22168432305414E-35,1.,-5.20417042793042E-18));
#142641=DIRECTION('',(-1.,1.14162099830241E-33,2.15097520454769E-16));
#142642=CARTESIAN_POINT('',(0.,0.,0.));
#142643=CARTESIAN_POINT('',(0.,0.,0.));
#142644=CARTESIAN_POINT('Origin',(90.,-529.112518717956,90.));
#142645=CARTESIAN_POINT('',(90.,-553.,98.4455));
#142646=CARTESIAN_POINT('Origin',(90.,-553.,90.));
#142647=CARTESIAN_POINT('',(90.,-573.,98.4455));
#142648=CARTESIAN_POINT('',(90.,-529.112518717956,98.4455));
#142649=CARTESIAN_POINT('Origin',(90.,-573.,90.));
#142650=CARTESIAN_POINT('Origin',(-90.,-529.112518717956,90.));
#142651=CARTESIAN_POINT('',(-90.,-553.,98.4455));
#142652=CARTESIAN_POINT('Origin',(-90.,-553.,90.));
#142653=CARTESIAN_POINT('',(-90.,-573.,98.4455));
#142654=CARTESIAN_POINT('',(-90.,-529.112518717956,98.4455));
#142655=CARTESIAN_POINT('Origin',(-90.,-573.,90.));
#142656=CARTESIAN_POINT('Origin',(-90.,-529.112518717956,-90.0000000000001));
#142657=CARTESIAN_POINT('',(-90.,-553.,-81.5545));
#142658=CARTESIAN_POINT('Origin',(-90.,-553.,-90.0000000000001));
#142659=CARTESIAN_POINT('',(-90.,-573.,-81.5545));
#142660=CARTESIAN_POINT('',(-90.,-529.112518717956,-81.5545));
#142661=CARTESIAN_POINT('Origin',(-90.,-573.,-90.0000000000001));
#142662=CARTESIAN_POINT('Origin',(90.,-529.112518717956,-90.));
#142663=CARTESIAN_POINT('',(90.,-553.,-81.5545));
#142664=CARTESIAN_POINT('Origin',(90.,-553.,-90.));
#142665=CARTESIAN_POINT('',(90.,-573.,-81.5545));
#142666=CARTESIAN_POINT('',(90.,-529.112518717956,-81.5545));
#142667=CARTESIAN_POINT('Origin',(90.,-573.,-90.));
#142668=CARTESIAN_POINT('Origin',(258.,-180.,-255.));
#142669=CARTESIAN_POINT('',(258.,0.,258.));
#142670=CARTESIAN_POINT('',(258.,0.,-258.));
#142671=CARTESIAN_POINT('',(258.,0.,-5.61642235986844E-14));
#142672=CARTESIAN_POINT('',(258.,-180.725252950448,258.));
#142673=CARTESIAN_POINT('',(258.,-180.,258.));
#142674=CARTESIAN_POINT('',(258.,-180.725252950448,-258.));
#142675=CARTESIAN_POINT('',(258.,-180.725252950448,-255.));
#142676=CARTESIAN_POINT('',(258.,-180.,-258.));
#142677=CARTESIAN_POINT('Origin',(-255.,-180.,258.));
#142678=CARTESIAN_POINT('',(-258.,0.,258.));
#142679=CARTESIAN_POINT('',(0.,0.,258.));
#142680=CARTESIAN_POINT('',(-258.,-180.725252950448,258.));
#142681=CARTESIAN_POINT('',(-258.,-180.,258.));
#142682=CARTESIAN_POINT('',(-255.,-180.725252950448,258.));
#142683=CARTESIAN_POINT('Origin',(-258.,-180.,-255.));
#142684=CARTESIAN_POINT('',(-258.,0.,-258.));
#142685=CARTESIAN_POINT('',(-258.,0.,2.80821117993422E-14));
#142686=CARTESIAN_POINT('',(-258.,-180.725252950448,-258.));
#142687=CARTESIAN_POINT('',(-258.,-180.,-258.));
#142688=CARTESIAN_POINT('',(-258.,-180.725252950448,-255.));
#142689=CARTESIAN_POINT('Origin',(-255.,-180.,-258.));
#142690=CARTESIAN_POINT('',(0.,0.,-258.));
#142691=CARTESIAN_POINT('',(-255.,-180.725252950448,-258.));
#142692=CARTESIAN_POINT('Origin',(0.,0.,0.));
#142693=CARTESIAN_POINT('',(255.,0.,255.));
#142694=CARTESIAN_POINT('',(255.,0.,-255.));
#142695=CARTESIAN_POINT('',(255.,0.,-255.));
#142696=CARTESIAN_POINT('',(-255.,0.,255.));
#142697=CARTESIAN_POINT('',(-255.,0.,255.));
#142698=CARTESIAN_POINT('',(-255.,0.,-255.));
#142699=CARTESIAN_POINT('',(-255.,0.,-255.));
#142700=CARTESIAN_POINT('',(-255.,0.,-255.));
#142701=CARTESIAN_POINT('Origin',(0.,-142.552494979833,-277.602227065991));
#142702=CARTESIAN_POINT('',(-66.83188665023,-553.,-66.8318866502301));
#142703=CARTESIAN_POINT('',(-229.675682842738,-235.88313373038,-229.675682842738));
#142704=CARTESIAN_POINT('',(66.8318866502301,-553.,-66.8318866502301));
#142705=CARTESIAN_POINT('',(229.675682842738,-235.883133730379,-229.675682842738));
#142706=CARTESIAN_POINT('',(0.,-553.,-66.8318866502301));
#142707=CARTESIAN_POINT('Origin',(277.602227065991,-142.552494979833,-6.04314478776244E-14));
#142708=CARTESIAN_POINT('',(66.8318866502301,-553.,66.8318866502301));
#142709=CARTESIAN_POINT('',(229.675682842738,-235.88313373038,229.675682842738));
#142710=CARTESIAN_POINT('',(66.8318866502301,-553.,-1.45486861447498E-14));
#142711=CARTESIAN_POINT('Origin',(-277.602227065991,-142.552494979833,3.02157239388122E-14));
#142712=CARTESIAN_POINT('',(-66.83188665023,-553.,66.8318866502301));
#142713=CARTESIAN_POINT('',(-229.675682842738,-235.883133730379,229.675682842738));
#142714=CARTESIAN_POINT('',(-66.83188665023,-553.,7.2743430723749E-15));
#142715=CARTESIAN_POINT('Origin',(0.,-142.552494979833,277.602227065991));
#142716=CARTESIAN_POINT('',(0.,-553.,66.8318866502301));
#142717=CARTESIAN_POINT('Origin',(255.,-180.,-255.));
#142718=CARTESIAN_POINT('',(255.,-180.,-255.));
#142719=CARTESIAN_POINT('',(255.,-180.,-255.));
#142720=CARTESIAN_POINT('',(255.,-180.,255.));
#142721=CARTESIAN_POINT('',(255.,-180.,-255.));
#142722=CARTESIAN_POINT('',(255.,-180.,255.));
#142723=CARTESIAN_POINT('Origin',(-255.,-180.,255.));
#142724=CARTESIAN_POINT('',(-255.,-180.,255.));
#142725=CARTESIAN_POINT('',(-255.,-180.,255.));
#142726=CARTESIAN_POINT('',(-255.,-180.,255.));
#142727=CARTESIAN_POINT('Origin',(-255.,-180.,-255.));
#142728=CARTESIAN_POINT('',(-255.,-180.,-255.));
#142729=CARTESIAN_POINT('',(-255.,-180.,-255.));
#142730=CARTESIAN_POINT('',(-255.,-180.,-255.));
#142731=CARTESIAN_POINT('Origin',(-255.,-180.,-255.));
#142732=CARTESIAN_POINT('',(-255.,-180.,-255.));
#142733=CARTESIAN_POINT('Origin',(0.,-141.182080924855,-274.933526011561));
#142734=CARTESIAN_POINT('',(-65.,-550.,-65.));
#142735=CARTESIAN_POINT('',(-65.,-550.,-65.));
#142736=CARTESIAN_POINT('',(65.,-550.,-65.));
#142737=CARTESIAN_POINT('',(65.,-550.,-65.));
#142738=CARTESIAN_POINT('',(65.,-550.,-65.));
#142739=CARTESIAN_POINT('Origin',(274.933526011561,-141.182080924855,-5.98504962391008E-14));
#142740=CARTESIAN_POINT('',(65.,-550.,65.));
#142741=CARTESIAN_POINT('',(65.,-550.,-65.));
#142742=CARTESIAN_POINT('',(65.,-550.,65.));
#142743=CARTESIAN_POINT('Origin',(-274.933526011561,-141.182080924855,2.99252481195504E-14));
#142744=CARTESIAN_POINT('',(-65.,-550.,65.));
#142745=CARTESIAN_POINT('',(-65.,-550.,65.));
#142746=CARTESIAN_POINT('',(-65.,-550.,-65.));
#142747=CARTESIAN_POINT('Origin',(0.,-141.182080924856,274.933526011561));
#142748=CARTESIAN_POINT('',(65.,-550.,65.));
#142749=CARTESIAN_POINT('Origin',(65.,-580.,-65.));
#142750=CARTESIAN_POINT('',(-64.9999999999999,-573.,-65.));
#142751=CARTESIAN_POINT('',(-65.,-580.,-65.));
#142752=CARTESIAN_POINT('',(65.,-573.,-65.));
#142753=CARTESIAN_POINT('',(-64.9999999999999,-573.,-65.));
#142754=CARTESIAN_POINT('',(65.,-580.,-65.));
#142755=CARTESIAN_POINT('Origin',(65.,-580.,65.));
#142756=CARTESIAN_POINT('',(65.,-573.,65.));
#142757=CARTESIAN_POINT('',(65.,-573.,65.));
#142758=CARTESIAN_POINT('',(65.,-580.,65.));
#142759=CARTESIAN_POINT('Origin',(-65.,-580.,65.));
#142760=CARTESIAN_POINT('',(-64.9999999999999,-573.,65.));
#142761=CARTESIAN_POINT('',(-64.9999999999999,-573.,65.));
#142762=CARTESIAN_POINT('',(-65.,-580.,65.));
#142763=CARTESIAN_POINT('Origin',(-65.,-580.,-65.));
#142764=CARTESIAN_POINT('',(-64.9999999999999,-573.,65.));
#142765=CARTESIAN_POINT('Origin',(0.,-553.,0.));
#142766=CARTESIAN_POINT('',(113.,-553.,90.));
#142767=CARTESIAN_POINT('',(113.,-553.,-90.));
#142768=CARTESIAN_POINT('',(113.,-553.,0.));
#142769=CARTESIAN_POINT('',(90.,-553.,-113.));
#142770=CARTESIAN_POINT('Origin',(90.,-553.,-90.));
#142771=CARTESIAN_POINT('',(-90.0000000000001,-553.,-113.));
#142772=CARTESIAN_POINT('',(0.,-553.,-113.));
#142773=CARTESIAN_POINT('',(-113.,-553.,-90.));
#142774=CARTESIAN_POINT('Origin',(-90.0000000000001,-553.,-90.));
#142775=CARTESIAN_POINT('',(-113.,-553.,90.));
#142776=CARTESIAN_POINT('',(-113.,-553.,0.));
#142777=CARTESIAN_POINT('',(-90.0000000000001,-553.,113.));
#142778=CARTESIAN_POINT('Origin',(-90.0000000000001,-553.,90.));
#142779=CARTESIAN_POINT('',(90.,-553.,113.));
#142780=CARTESIAN_POINT('',(0.,-553.,113.));
#142781=CARTESIAN_POINT('Origin',(90.,-553.,90.));
#142782=CARTESIAN_POINT('Origin',(0.,-573.,0.));
#142783=CARTESIAN_POINT('',(115.,-573.,-90.));
#142784=CARTESIAN_POINT('',(115.,-573.,90.));
#142785=CARTESIAN_POINT('',(115.,-573.,115.));
#142786=CARTESIAN_POINT('',(90.,-573.,115.));
#142787=CARTESIAN_POINT('Origin',(90.,-573.,90.));
#142788=CARTESIAN_POINT('',(-90.0000000000001,-573.,115.));
#142789=CARTESIAN_POINT('',(-115.,-573.,115.));
#142790=CARTESIAN_POINT('',(-115.,-573.,90.));
#142791=CARTESIAN_POINT('Origin',(-90.0000000000001,-573.,90.));
#142792=CARTESIAN_POINT('',(-115.,-573.,-90.));
#142793=CARTESIAN_POINT('',(-115.,-573.,115.));
#142794=CARTESIAN_POINT('',(-90.0000000000001,-573.,-115.));
#142795=CARTESIAN_POINT('Origin',(-90.0000000000001,-573.,-90.));
#142796=CARTESIAN_POINT('',(90.,-573.,-115.));
#142797=CARTESIAN_POINT('',(-115.,-573.,-115.));
#142798=CARTESIAN_POINT('Origin',(90.,-573.,-90.));
#142799=CARTESIAN_POINT('Origin',(115.,-573.,115.));
#142800=CARTESIAN_POINT('',(115.,-555.,-90.));
#142801=CARTESIAN_POINT('',(115.,-573.,-90.));
#142802=CARTESIAN_POINT('',(115.,-555.,90.));
#142803=CARTESIAN_POINT('',(115.,-555.,115.));
#142804=CARTESIAN_POINT('',(115.,-573.,90.));
#142805=CARTESIAN_POINT('Origin',(-115.,-573.,115.));
#142806=CARTESIAN_POINT('',(90.,-555.,115.));
#142807=CARTESIAN_POINT('',(90.,-573.,115.));
#142808=CARTESIAN_POINT('',(-90.0000000000001,-555.,115.));
#142809=CARTESIAN_POINT('',(-115.,-555.,115.));
#142810=CARTESIAN_POINT('',(-90.0000000000001,-573.,115.));
#142811=CARTESIAN_POINT('Origin',(-115.,-573.,115.));
#142812=CARTESIAN_POINT('',(-115.,-555.,90.));
#142813=CARTESIAN_POINT('',(-115.,-573.,90.));
#142814=CARTESIAN_POINT('',(-115.,-555.,-90.));
#142815=CARTESIAN_POINT('',(-115.,-555.,115.));
#142816=CARTESIAN_POINT('',(-115.,-573.,-90.));
#142817=CARTESIAN_POINT('Origin',(-115.,-573.,-115.));
#142818=CARTESIAN_POINT('',(-90.0000000000001,-555.,-115.));
#142819=CARTESIAN_POINT('',(-90.0000000000001,-573.,-115.));
#142820=CARTESIAN_POINT('',(90.,-555.,-115.));
#142821=CARTESIAN_POINT('',(-115.,-555.,-115.));
#142822=CARTESIAN_POINT('',(90.,-573.,-115.));
#142823=CARTESIAN_POINT('Origin',(90.,-573.,90.));
#142824=CARTESIAN_POINT('Origin',(90.,-555.,90.));
#142825=CARTESIAN_POINT('Origin',(90.,-573.,-90.));
#142826=CARTESIAN_POINT('Origin',(90.,-555.,-90.));
#142827=CARTESIAN_POINT('Origin',(-90.0000000000001,-573.,-90.));
#142828=CARTESIAN_POINT('Origin',(-90.0000000000001,-555.,-90.));
#142829=CARTESIAN_POINT('Origin',(-90.0000000000001,-573.,90.));
#142830=CARTESIAN_POINT('Origin',(-90.0000000000001,-555.,90.));
#142831=CARTESIAN_POINT('Origin',(-90.0000000000001,-555.,90.));
#142832=CARTESIAN_POINT('Origin',(-113.,-555.,90.));
#142833=CARTESIAN_POINT('Origin',(-90.0000000000001,-555.,113.));
#142834=CARTESIAN_POINT('Origin',(-115.,-555.,113.));
#142835=CARTESIAN_POINT('Origin',(90.,-555.,113.));
#142836=CARTESIAN_POINT('Origin',(-113.,-555.,115.));
#142837=CARTESIAN_POINT('Origin',(-113.,-555.,-90.));
#142838=CARTESIAN_POINT('Origin',(90.,-555.,90.));
#142839=CARTESIAN_POINT('Origin',(113.,-555.,90.));
#142840=CARTESIAN_POINT('Origin',(-90.0000000000001,-555.,-90.));
#142841=CARTESIAN_POINT('Origin',(-90.0000000000001,-555.,-113.));
#142842=CARTESIAN_POINT('Origin',(113.,-555.,115.));
#142843=CARTESIAN_POINT('Origin',(113.,-555.,-90.));
#142844=CARTESIAN_POINT('Origin',(-115.,-555.,-113.));
#142845=CARTESIAN_POINT('Origin',(90.,-555.,-113.));
#142846=CARTESIAN_POINT('Origin',(90.,-555.,-90.));
#142847=CARTESIAN_POINT('',(0.,0.,0.));
#142848=CARTESIAN_POINT('Origin',(0.,-1.83525269067091E-13,1504.696));
#142849=CARTESIAN_POINT('',(1.10218211923264E-15,-9.00000000000036,1504.696));
#142850=CARTESIAN_POINT('',(-1.10218211923264E-15,8.99999999999999,1504.696));
#142851=CARTESIAN_POINT('Origin',(0.,-1.83525269067091E-13,1504.696));
#142852=CARTESIAN_POINT('Origin',(0.,-1.83525269067091E-13,1504.696));
#142853=CARTESIAN_POINT('',(-1.13328814793098E-15,9.254,1504.95));
#142854=CARTESIAN_POINT('Origin',(-1.13328814793098E-15,9.254,1504.696));
#142855=CARTESIAN_POINT('Origin',(0.,-1.83556249024732E-13,1504.95));
#142856=CARTESIAN_POINT('Origin',(0.,-1.83525269067091E-13,1504.696));
#142857=CARTESIAN_POINT('',(-1.35482675389674E-15,11.063,1504.95));
#142858=CARTESIAN_POINT('Origin',(0.,-1.83556249024732E-13,1504.95));
#142859=CARTESIAN_POINT('',(-1.38593278259508E-15,11.317,1504.696));
#142860=CARTESIAN_POINT('Origin',(-1.35482675389674E-15,11.063,1504.696));
#142861=CARTESIAN_POINT('',(1.38593278259508E-15,-11.3170000000004,1504.696));
#142862=CARTESIAN_POINT('Origin',(0.,-1.83525269067091E-13,1504.696));
#142863=CARTESIAN_POINT('Origin',(0.,-1.83525269067091E-13,1504.696));
#142864=CARTESIAN_POINT('Origin',(-51.0189817055138,1.6136547197417E-13,
1492.25));
#142865=CARTESIAN_POINT('',(-10.0725040883277,5.15937499999993,1492.25));
#142866=CARTESIAN_POINT('',(-10.0725040883278,-5.15937500000011,1492.25));
#142867=CARTESIAN_POINT('Ctrl Pts',(-10.0725040883277,5.15937499999994,
1492.25));
#142868=CARTESIAN_POINT('Ctrl Pts',(-10.0725040883277,5.15937499999994,
1491.5908449252));
#142869=CARTESIAN_POINT('Ctrl Pts',(-10.1440843535216,5.02564501462724,
1490.8958794792));
#142870=CARTESIAN_POINT('Ctrl Pts',(-10.3894819155763,4.4964667402695,1489.62844582463));
#142871=CARTESIAN_POINT('Ctrl Pts',(-10.5585230349077,4.10136924643432,
1489.05491114807));
#142872=CARTESIAN_POINT('Ctrl Pts',(-10.866877089651,3.19590327436256,1488.14944517599));
#142873=CARTESIAN_POINT('Ctrl Pts',(-11.0278903257137,2.62207755819461,
1487.75374024113));
#142874=CARTESIAN_POINT('Ctrl Pts',(-11.254236928579,1.35344266229487,1487.22408350872));
#142875=CARTESIAN_POINT('Ctrl Pts',(-11.3170000000002,0.657970384764705,
1487.090625));
#142876=CARTESIAN_POINT('Ctrl Pts',(-11.3170000000002,-0.657970384764866,
1487.090625));
#142877=CARTESIAN_POINT('Ctrl Pts',(-11.254236928579,-1.35344266229482,
1487.22408350872));
#142878=CARTESIAN_POINT('Ctrl Pts',(-11.0278903257138,-2.62207755819449,
1487.75374024113));
#142879=CARTESIAN_POINT('Ctrl Pts',(-10.866877089651,-3.19590327436272,
1488.14944517599));
#142880=CARTESIAN_POINT('Ctrl Pts',(-10.5585230349078,-4.10136924643449,
1489.05491114807));
#142881=CARTESIAN_POINT('Ctrl Pts',(-10.3894819155764,-4.49646674026967,
1489.62844582463));
#142882=CARTESIAN_POINT('Ctrl Pts',(-10.1440843535217,-5.02564501462741,
1490.8958794792));
#142883=CARTESIAN_POINT('Ctrl Pts',(-10.0725040883278,-5.15937500000011,
1491.5908449252));
#142884=CARTESIAN_POINT('Ctrl Pts',(-10.0725040883278,-5.15937500000011,
1492.25));
#142885=CARTESIAN_POINT('',(-7.37433723187231,-5.15937500000013,1492.25));
#142886=CARTESIAN_POINT('',(-51.0189817055139,-5.15937499999986,1492.25));
#142887=CARTESIAN_POINT('',(-7.37433723187225,5.15937499999992,1492.25));
#142888=CARTESIAN_POINT('Ctrl Pts',(-7.37433723187237,-5.1593750000001,
1492.25));
#142889=CARTESIAN_POINT('Ctrl Pts',(-7.37433723187237,-5.15937500000011,
1491.5821328984));
#142890=CARTESIAN_POINT('Ctrl Pts',(-7.47468272092302,-5.0226214370987,
1490.88541735607));
#142891=CARTESIAN_POINT('Ctrl Pts',(-7.80496687696187,-4.49222528611439,
1489.62155204094));
#142892=CARTESIAN_POINT('Ctrl Pts',(-8.02760290754501,-4.09885081991491,
1489.05239272155));
#142893=CARTESIAN_POINT('Ctrl Pts',(-8.42620218982163,-3.19993704609044,
1488.15347894772));
#142894=CARTESIAN_POINT('Ctrl Pts',(-8.63162196667481,-2.63009169102994,
1487.75845526816));
#142895=CARTESIAN_POINT('Ctrl Pts',(-8.91992322022013,-1.36280970424654,
1487.22664378595));
#142896=CARTESIAN_POINT('Ctrl Pts',(-9.00000000000018,-0.664414150007918,
1487.090625));
#142897=CARTESIAN_POINT('Ctrl Pts',(-9.00000000000017,0.664414150007731,
1487.090625));
#142898=CARTESIAN_POINT('Ctrl Pts',(-8.9199232202201,1.36280970424636,1487.22664378595));
#142899=CARTESIAN_POINT('Ctrl Pts',(-8.63162196667476,2.63009169102975,
1487.75845526816));
#142900=CARTESIAN_POINT('Ctrl Pts',(-8.42620218982157,3.19993704609025,
1488.15347894772));
#142901=CARTESIAN_POINT('Ctrl Pts',(-8.02760290754492,4.09885081991471,
1489.05239272155));
#142902=CARTESIAN_POINT('Ctrl Pts',(-7.80496687696178,4.49222528611418,
1489.62155204094));
#142903=CARTESIAN_POINT('Ctrl Pts',(-7.47468272092292,5.02262143709849,
1490.88541735607));
#142904=CARTESIAN_POINT('Ctrl Pts',(-7.37433723187224,5.15937499999992,
1491.5821328984));
#142905=CARTESIAN_POINT('Ctrl Pts',(-7.37433723187224,5.15937499999992,
1492.25));
#142906=CARTESIAN_POINT('Ctrl Pts',(-7.37433723187225,5.15937499999991,
1492.25));
#142907=CARTESIAN_POINT('Ctrl Pts',(-7.37433723187225,5.15937499999991,
1492.9178671016));
#142908=CARTESIAN_POINT('Ctrl Pts',(-7.47468272092287,5.02262143709855,
1493.61458264393));
#142909=CARTESIAN_POINT('Ctrl Pts',(-7.80496687696175,4.49222528611424,
1494.87844795906));
#142910=CARTESIAN_POINT('Ctrl Pts',(-8.02760290754492,4.09885081991471,
1495.44760727845));
#142911=CARTESIAN_POINT('Ctrl Pts',(-8.42620218982157,3.19993704609025,
1496.34652105228));
#142912=CARTESIAN_POINT('Ctrl Pts',(-8.63162196667476,2.63009169102975,
1496.74154473184));
#142913=CARTESIAN_POINT('Ctrl Pts',(-8.9199232202201,1.36280970424635,1497.27335621405));
#142914=CARTESIAN_POINT('Ctrl Pts',(-9.00000000000017,0.664414150007731,
1497.409375));
#142915=CARTESIAN_POINT('Ctrl Pts',(-9.00000000000018,-0.664414150007918,
1497.409375));
#142916=CARTESIAN_POINT('Ctrl Pts',(-8.9199232202201,-1.36280970424675,
1497.27335621405));
#142917=CARTESIAN_POINT('Ctrl Pts',(-8.63162196667478,-2.63009169103002,
1496.74154473184));
#142918=CARTESIAN_POINT('Ctrl Pts',(-8.42620218982163,-3.19993704609044,
1496.34652105228));
#142919=CARTESIAN_POINT('Ctrl Pts',(-8.02760290754501,-4.09885081991491,
1495.44760727845));
#142920=CARTESIAN_POINT('Ctrl Pts',(-7.80496687696187,-4.49222528611439,
1494.87844795906));
#142921=CARTESIAN_POINT('Ctrl Pts',(-7.47468272092302,-5.0226214370987,
1493.61458264393));
#142922=CARTESIAN_POINT('Ctrl Pts',(-7.37433723187236,-5.15937500000012,
1492.9178671016));
#142923=CARTESIAN_POINT('Ctrl Pts',(-7.37433723187236,-5.15937500000012,
1492.25));
#142924=CARTESIAN_POINT('Ctrl Pts',(-10.0725040883278,-5.1593750000001,
1492.25));
#142925=CARTESIAN_POINT('Ctrl Pts',(-10.0725040883278,-5.1593750000001,
1492.9091550748));
#142926=CARTESIAN_POINT('Ctrl Pts',(-10.1440843535217,-5.02564501462741,
1493.6041205208));
#142927=CARTESIAN_POINT('Ctrl Pts',(-10.3894819155764,-4.49646674026967,
1494.87155417537));
#142928=CARTESIAN_POINT('Ctrl Pts',(-10.5585230349078,-4.10136924643449,
1495.44508885193));
#142929=CARTESIAN_POINT('Ctrl Pts',(-10.866877089651,-3.19590327436273,
1496.35055482401));
#142930=CARTESIAN_POINT('Ctrl Pts',(-11.0278903257138,-2.62207755819477,
1496.74625975887));
#142931=CARTESIAN_POINT('Ctrl Pts',(-11.254236928579,-1.35344266229503,
1497.27591649128));
#142932=CARTESIAN_POINT('Ctrl Pts',(-11.3170000000002,-0.657970384764865,
1497.409375));
#142933=CARTESIAN_POINT('Ctrl Pts',(-11.3170000000002,0.657970384764708,
1497.409375));
#142934=CARTESIAN_POINT('Ctrl Pts',(-11.254236928579,1.35344266229487,1497.27591649128));
#142935=CARTESIAN_POINT('Ctrl Pts',(-11.0278903257137,2.62207755819461,
1496.74625975887));
#142936=CARTESIAN_POINT('Ctrl Pts',(-10.866877089651,3.19590327436256,1496.35055482401));
#142937=CARTESIAN_POINT('Ctrl Pts',(-10.5585230349077,4.10136924643432,
1495.44508885193));
#142938=CARTESIAN_POINT('Ctrl Pts',(-10.3894819155763,4.4964667402695,1494.87155417537));
#142939=CARTESIAN_POINT('Ctrl Pts',(-10.1440843535216,5.02564501462724,
1493.6041205208));
#142940=CARTESIAN_POINT('Ctrl Pts',(-10.0725040883277,5.15937499999996,
1492.9091550748));
#142941=CARTESIAN_POINT('Ctrl Pts',(-10.0725040883277,5.15937499999996,
1492.25));
#142942=CARTESIAN_POINT('Origin',(-51.0189817055138,1.6136547197417E-13,
1492.25));
#142943=CARTESIAN_POINT('',(7.37433723187231,5.15937499999983,1492.25));
#142944=CARTESIAN_POINT('',(7.37433723187222,-5.15937500000021,1492.25));
#142945=CARTESIAN_POINT('Ctrl Pts',(7.37433723187231,5.15937499999983,1492.25));
#142946=CARTESIAN_POINT('Ctrl Pts',(7.3743372318723,5.15937499999983,1491.5821328984));
#142947=CARTESIAN_POINT('Ctrl Pts',(7.47468272092298,5.0226214370984,1490.88541735607));
#142948=CARTESIAN_POINT('Ctrl Pts',(7.80496687696183,4.49222528611409,1489.62155204094));
#142949=CARTESIAN_POINT('Ctrl Pts',(8.02760290754497,4.09885081991462,1489.05239272155));
#142950=CARTESIAN_POINT('Ctrl Pts',(8.42620218982161,3.19993704609015,1488.15347894772));
#142951=CARTESIAN_POINT('Ctrl Pts',(8.63162196667479,2.63009169102964,1487.75845526816));
#142952=CARTESIAN_POINT('Ctrl Pts',(8.91992322022012,1.36280970424625,1487.22664378595));
#142953=CARTESIAN_POINT('Ctrl Pts',(9.00000000000018,0.664414150007621,
1487.090625));
#142954=CARTESIAN_POINT('Ctrl Pts',(9.00000000000018,-0.664414150008029,
1487.090625));
#142955=CARTESIAN_POINT('Ctrl Pts',(8.91992322022011,-1.36280970424665,
1487.22664378595));
#142956=CARTESIAN_POINT('Ctrl Pts',(8.63162196667478,-2.63009169103005,
1487.75845526816));
#142957=CARTESIAN_POINT('Ctrl Pts',(8.4262021898216,-3.19993704609055,1488.15347894772));
#142958=CARTESIAN_POINT('Ctrl Pts',(8.02760290754496,-4.09885081991501,
1489.05239272155));
#142959=CARTESIAN_POINT('Ctrl Pts',(7.80496687696182,-4.49222528611448,
1489.62155204094));
#142960=CARTESIAN_POINT('Ctrl Pts',(7.47468272092296,-5.02262143709879,
1490.88541735607));
#142961=CARTESIAN_POINT('Ctrl Pts',(7.3743372318723,-5.1593750000002,1491.5821328984));
#142962=CARTESIAN_POINT('Ctrl Pts',(7.3743372318723,-5.15937500000019,1492.25));
#142963=CARTESIAN_POINT('',(10.0725040883277,-5.15937500000024,1492.25));
#142964=CARTESIAN_POINT('',(-51.0189817055139,-5.15937499999986,1492.25));
#142965=CARTESIAN_POINT('',(10.0725040883277,5.15937499999981,1492.25));
#142966=CARTESIAN_POINT('Ctrl Pts',(10.0725040883277,-5.15937500000025,
1492.25));
#142967=CARTESIAN_POINT('Ctrl Pts',(10.0725040883277,-5.15937500000025,
1491.5908449252));
#142968=CARTESIAN_POINT('Ctrl Pts',(10.1440843535216,-5.02564501462754,
1490.8958794792));
#142969=CARTESIAN_POINT('Ctrl Pts',(10.3894819155763,-4.4964667402698,1489.62844582463));
#142970=CARTESIAN_POINT('Ctrl Pts',(10.5585230349078,-4.10136924643461,
1489.05491114807));
#142971=CARTESIAN_POINT('Ctrl Pts',(10.866877089651,-3.19590327436286,1488.14944517599));
#142972=CARTESIAN_POINT('Ctrl Pts',(11.0278903257137,-2.62207755819491,
1487.75374024113));
#142973=CARTESIAN_POINT('Ctrl Pts',(11.254236928579,-1.35344266229517,1487.22408350872));
#142974=CARTESIAN_POINT('Ctrl Pts',(11.3170000000002,-0.657970384765003,
1487.090625));
#142975=CARTESIAN_POINT('Ctrl Pts',(11.3170000000002,0.657970384764568,
1487.090625));
#142976=CARTESIAN_POINT('Ctrl Pts',(11.254236928579,1.35344266229473,1487.22408350872));
#142977=CARTESIAN_POINT('Ctrl Pts',(11.0278903257137,2.62207755819447,1487.75374024113));
#142978=CARTESIAN_POINT('Ctrl Pts',(10.866877089651,3.19590327436243,1488.14944517599));
#142979=CARTESIAN_POINT('Ctrl Pts',(10.5585230349078,4.10136924643419,1489.05491114807));
#142980=CARTESIAN_POINT('Ctrl Pts',(10.3894819155764,4.49646674026938,1489.62844582463));
#142981=CARTESIAN_POINT('Ctrl Pts',(10.1440843535216,5.02564501462711,1490.8958794792));
#142982=CARTESIAN_POINT('Ctrl Pts',(10.0725040883277,5.15937499999981,1491.5908449252));
#142983=CARTESIAN_POINT('Ctrl Pts',(10.0725040883277,5.15937499999981,1492.25));
#142984=CARTESIAN_POINT('Ctrl Pts',(10.0725040883277,5.15937499999983,1492.25));
#142985=CARTESIAN_POINT('Ctrl Pts',(10.0725040883277,5.15937499999983,1492.9091550748));
#142986=CARTESIAN_POINT('Ctrl Pts',(10.1440843535216,5.02564501462711,1493.6041205208));
#142987=CARTESIAN_POINT('Ctrl Pts',(10.3894819155764,4.49646674026938,1494.87155417537));
#142988=CARTESIAN_POINT('Ctrl Pts',(10.5585230349078,4.10136924643419,1495.44508885193));
#142989=CARTESIAN_POINT('Ctrl Pts',(10.866877089651,3.19590327436243,1496.35055482401));
#142990=CARTESIAN_POINT('Ctrl Pts',(11.0278903257137,2.62207755819446,1496.74625975887));
#142991=CARTESIAN_POINT('Ctrl Pts',(11.254236928579,1.35344266229473,1497.27591649128));
#142992=CARTESIAN_POINT('Ctrl Pts',(11.3170000000002,0.657970384764568,
1497.409375));
#142993=CARTESIAN_POINT('Ctrl Pts',(11.3170000000002,-0.657970384765003,
1497.409375));
#142994=CARTESIAN_POINT('Ctrl Pts',(11.254236928579,-1.35344266229517,1497.27591649128));
#142995=CARTESIAN_POINT('Ctrl Pts',(11.0278903257137,-2.62207755819491,
1496.74625975887));
#142996=CARTESIAN_POINT('Ctrl Pts',(10.866877089651,-3.19590327436286,1496.35055482401));
#142997=CARTESIAN_POINT('Ctrl Pts',(10.5585230349078,-4.10136924643461,
1495.44508885193));
#142998=CARTESIAN_POINT('Ctrl Pts',(10.3894819155763,-4.4964667402698,1494.87155417537));
#142999=CARTESIAN_POINT('Ctrl Pts',(10.1440843535216,-5.02564501462754,
1493.6041205208));
#143000=CARTESIAN_POINT('Ctrl Pts',(10.0725040883277,-5.15937500000024,
1492.9091550748));
#143001=CARTESIAN_POINT('Ctrl Pts',(10.0725040883277,-5.15937500000024,
1492.25));
#143002=CARTESIAN_POINT('Ctrl Pts',(7.37433723187228,-5.15937500000022,
1492.25));
#143003=CARTESIAN_POINT('Ctrl Pts',(7.37433723187228,-5.15937500000023,
1492.9178671016));
#143004=CARTESIAN_POINT('Ctrl Pts',(7.47468272092296,-5.02262143709879,
1493.61458264393));
#143005=CARTESIAN_POINT('Ctrl Pts',(7.80496687696182,-4.49222528611448,
1494.87844795906));
#143006=CARTESIAN_POINT('Ctrl Pts',(8.02760290754496,-4.09885081991501,
1495.44760727845));
#143007=CARTESIAN_POINT('Ctrl Pts',(8.4262021898216,-3.19993704609055,1496.34652105228));
#143008=CARTESIAN_POINT('Ctrl Pts',(8.63162196667478,-2.63009169103005,
1496.74154473184));
#143009=CARTESIAN_POINT('Ctrl Pts',(8.91992322022011,-1.36280970424665,
1497.27335621405));
#143010=CARTESIAN_POINT('Ctrl Pts',(9.00000000000018,-0.664414150008027,
1497.409375));
#143011=CARTESIAN_POINT('Ctrl Pts',(9.00000000000018,0.664414150007622,
1497.409375));
#143012=CARTESIAN_POINT('Ctrl Pts',(8.91992322022012,1.36280970424625,1497.27335621405));
#143013=CARTESIAN_POINT('Ctrl Pts',(8.63162196667479,2.63009169102964,1496.74154473184));
#143014=CARTESIAN_POINT('Ctrl Pts',(8.42620218982161,3.19993704609015,1496.34652105228));
#143015=CARTESIAN_POINT('Ctrl Pts',(8.02760290754497,4.09885081991462,1495.44760727845));
#143016=CARTESIAN_POINT('Ctrl Pts',(7.80496687696183,4.49222528611409,1494.87844795906));
#143017=CARTESIAN_POINT('Ctrl Pts',(7.47468272092298,5.0226214370984,1493.61458264393));
#143018=CARTESIAN_POINT('Ctrl Pts',(7.37433723187231,5.15937499999982,1492.9178671016));
#143019=CARTESIAN_POINT('Ctrl Pts',(7.37433723187231,5.15937499999982,1492.25));
#143020=CARTESIAN_POINT('Origin',(0.,50.8013494805973,1441.45));
#143021=CARTESIAN_POINT('',(1.84349851574185E-21,11.317,1436.290625));
#143022=CARTESIAN_POINT('',(-6.31841207935097E-16,11.317,1446.609375));
#143023=CARTESIAN_POINT('Ctrl Pts',(-2.24820162486594E-14,11.317,1436.290625));
#143024=CARTESIAN_POINT('Ctrl Pts',(-0.657970384764816,11.317,1436.290625));
#143025=CARTESIAN_POINT('Ctrl Pts',(-1.35344266229499,11.2542369285788,
1436.42408350872));
#143026=CARTESIAN_POINT('Ctrl Pts',(-2.62207755819474,11.0278903257136,
1436.95374024113));
#143027=CARTESIAN_POINT('Ctrl Pts',(-3.19590327436269,10.8668770896508,
1437.34944517599));
#143028=CARTESIAN_POINT('Ctrl Pts',(-4.10136924643445,10.5585230349076,
1438.25491114807));
#143029=CARTESIAN_POINT('Ctrl Pts',(-4.49646674026965,10.3894819155762,
1438.82844582463));
#143030=CARTESIAN_POINT('Ctrl Pts',(-5.02564501462738,10.1440843535214,
1440.0958794792));
#143031=CARTESIAN_POINT('Ctrl Pts',(-5.15937500000008,10.0725040883275,
1440.7908449252));
#143032=CARTESIAN_POINT('Ctrl Pts',(-5.15937500000008,10.0725040883275,
1441.45));
#143033=CARTESIAN_POINT('Ctrl Pts',(-5.15937500000008,10.0725040883275,
1442.1091550748));
#143034=CARTESIAN_POINT('Ctrl Pts',(-5.02564501462738,10.1440843535214,
1442.8041205208));
#143035=CARTESIAN_POINT('Ctrl Pts',(-4.49646674026965,10.3894819155762,
1444.07155417537));
#143036=CARTESIAN_POINT('Ctrl Pts',(-4.10136924643444,10.5585230349076,
1444.64508885193));
#143037=CARTESIAN_POINT('Ctrl Pts',(-3.19590327436268,10.8668770896508,
1445.55055482401));
#143038=CARTESIAN_POINT('Ctrl Pts',(-2.62207755819474,11.0278903257136,
1445.94625975887));
#143039=CARTESIAN_POINT('Ctrl Pts',(-1.35344266229499,11.2542369285788,
1446.47591649128));
#143040=CARTESIAN_POINT('Ctrl Pts',(-0.657970384764796,11.317,1446.609375));
#143041=CARTESIAN_POINT('Ctrl Pts',(-3.7470027081099E-15,11.317,1446.609375));
#143042=CARTESIAN_POINT('',(-4.2017011901556E-15,9.,1446.609375));
#143043=CARTESIAN_POINT('',(-6.31841207935097E-16,50.8013494805973,1446.609375));
#143044=CARTESIAN_POINT('',(-1.55306990715387E-27,9.,1436.290625));
#143045=CARTESIAN_POINT('Ctrl Pts',(-1.11022302462516E-15,9.,1446.609375));
#143046=CARTESIAN_POINT('Ctrl Pts',(-0.664414150007834,9.,1446.609375));
#143047=CARTESIAN_POINT('Ctrl Pts',(-1.36280970424649,8.91992322021993,
1446.47335621405));
#143048=CARTESIAN_POINT('Ctrl Pts',(-2.6300916910299,8.6316219666746,1445.94154473184));
#143049=CARTESIAN_POINT('Ctrl Pts',(-3.19993704609039,8.42620218982141,
1445.54652105228));
#143050=CARTESIAN_POINT('Ctrl Pts',(-4.09885081991486,8.02760290754477,
1444.64760727845));
#143051=CARTESIAN_POINT('Ctrl Pts',(-4.49222528611435,7.80496687696161,
1444.07844795906));
#143052=CARTESIAN_POINT('Ctrl Pts',(-5.02262143709865,7.47468272092276,
1442.81458264393));
#143053=CARTESIAN_POINT('Ctrl Pts',(-5.15937500000008,7.37433723187208,
1442.1178671016));
#143054=CARTESIAN_POINT('Ctrl Pts',(-5.15937500000008,7.37433723187208,
1441.45));
#143055=CARTESIAN_POINT('Ctrl Pts',(-5.15937500000008,7.37433723187208,
1440.7821328984));
#143056=CARTESIAN_POINT('Ctrl Pts',(-5.02262143709865,7.47468272092276,
1440.08541735607));
#143057=CARTESIAN_POINT('Ctrl Pts',(-4.49222528611435,7.80496687696161,
1438.82155204094));
#143058=CARTESIAN_POINT('Ctrl Pts',(-4.09885081991486,8.02760290754477,
1438.25239272155));
#143059=CARTESIAN_POINT('Ctrl Pts',(-3.19993704609039,8.42620218982141,
1437.35347894772));
#143060=CARTESIAN_POINT('Ctrl Pts',(-2.63009169102989,8.6316219666746,1436.95845526816));
#143061=CARTESIAN_POINT('Ctrl Pts',(-1.36280970424649,8.91992322021993,
1436.42664378595));
#143062=CARTESIAN_POINT('Ctrl Pts',(-0.664414150007838,9.,1436.290625));
#143063=CARTESIAN_POINT('Ctrl Pts',(-5.48172618408671E-15,9.,1436.290625));
#143064=CARTESIAN_POINT('Ctrl Pts',(-2.91433543964104E-15,9.00000000000001,
1436.290625));
#143065=CARTESIAN_POINT('Ctrl Pts',(0.66441415000783,9.00000000000001,1436.290625));
#143066=CARTESIAN_POINT('Ctrl Pts',(1.36280970424649,8.91992322021993,1436.42664378595));
#143067=CARTESIAN_POINT('Ctrl Pts',(2.6300916910299,8.6316219666746,1436.95845526816));
#143068=CARTESIAN_POINT('Ctrl Pts',(3.19993704609039,8.42620218982141,1437.35347894772));
#143069=CARTESIAN_POINT('Ctrl Pts',(4.09885081991486,8.02760290754477,1438.25239272155));
#143070=CARTESIAN_POINT('Ctrl Pts',(4.49222528611408,7.80496687696178,1438.82155204094));
#143071=CARTESIAN_POINT('Ctrl Pts',(5.02262143709853,7.47468272092284,1440.08541735607));
#143072=CARTESIAN_POINT('Ctrl Pts',(5.15937500000008,7.37433723187208,1440.7821328984));
#143073=CARTESIAN_POINT('Ctrl Pts',(5.15937500000008,7.37433723187208,1442.1178671016));
#143074=CARTESIAN_POINT('Ctrl Pts',(5.02262143709865,7.47468272092276,1442.81458264393));
#143075=CARTESIAN_POINT('Ctrl Pts',(4.49222528611435,7.80496687696161,1444.07844795906));
#143076=CARTESIAN_POINT('Ctrl Pts',(4.09885081991486,8.02760290754477,1444.64760727845));
#143077=CARTESIAN_POINT('Ctrl Pts',(3.19993704609039,8.42620218982141,1445.54652105228));
#143078=CARTESIAN_POINT('Ctrl Pts',(2.63009169102989,8.6316219666746,1445.94154473184));
#143079=CARTESIAN_POINT('Ctrl Pts',(1.36280970424649,8.91992322021993,1446.47335621405));
#143080=CARTESIAN_POINT('Ctrl Pts',(0.664414150007821,9.,1446.609375));
#143081=CARTESIAN_POINT('Ctrl Pts',(-1.15879528195251E-14,9.,1446.609375));
#143082=CARTESIAN_POINT('Ctrl Pts',(6.10622663543836E-15,11.317,1446.609375));
#143083=CARTESIAN_POINT('Ctrl Pts',(0.6579703847648,11.317,1446.609375));
#143084=CARTESIAN_POINT('Ctrl Pts',(1.35344266229499,11.2542369285788,1446.47591649128));
#143085=CARTESIAN_POINT('Ctrl Pts',(2.62207755819474,11.0278903257136,1445.94625975887));
#143086=CARTESIAN_POINT('Ctrl Pts',(3.19590327436269,10.8668770896508,1445.55055482401));
#143087=CARTESIAN_POINT('Ctrl Pts',(4.10136924643444,10.5585230349076,1444.64508885193));
#143088=CARTESIAN_POINT('Ctrl Pts',(4.49646674026965,10.3894819155762,1444.07155417537));
#143089=CARTESIAN_POINT('Ctrl Pts',(5.02564501462738,10.1440843535214,1442.8041205208));
#143090=CARTESIAN_POINT('Ctrl Pts',(5.15937500000008,10.0725040883275,1442.1091550748));
#143091=CARTESIAN_POINT('Ctrl Pts',(5.15937500000008,10.0725040883275,1440.7908449252));
#143092=CARTESIAN_POINT('Ctrl Pts',(5.02564501462738,10.1440843535214,1440.0958794792));
#143093=CARTESIAN_POINT('Ctrl Pts',(4.49646674026965,10.3894819155762,1438.82844582463));
#143094=CARTESIAN_POINT('Ctrl Pts',(4.10136924643445,10.5585230349076,1438.25491114807));
#143095=CARTESIAN_POINT('Ctrl Pts',(3.19590327436269,10.8668770896508,1437.34944517599));
#143096=CARTESIAN_POINT('Ctrl Pts',(2.62207755819474,11.0278903257136,1436.95374024113));
#143097=CARTESIAN_POINT('Ctrl Pts',(1.35344266229499,11.2542369285788,1436.42408350872));
#143098=CARTESIAN_POINT('Ctrl Pts',(0.657970384764793,11.317,1436.290625));
#143099=CARTESIAN_POINT('Ctrl Pts',(1.38777878078145E-16,11.317,1436.290625));
#143100=CARTESIAN_POINT('Origin',(0.,50.8013494805973,1441.45));
#143101=CARTESIAN_POINT('',(-5.72393189099081E-15,-9.00000000000036,1436.290625));
#143102=CARTESIAN_POINT('',(-3.68128414736255E-15,-9.00000000000036,1446.609375));
#143103=CARTESIAN_POINT('Ctrl Pts',(4.30211422042248E-15,-9.00000000000036,
1436.290625));
#143104=CARTESIAN_POINT('Ctrl Pts',(-0.664414150007829,-9.00000000000036,
1436.290625));
#143105=CARTESIAN_POINT('Ctrl Pts',(-1.36280970424649,-8.91992322022029,
1436.42664378595));
#143106=CARTESIAN_POINT('Ctrl Pts',(-2.6300916910299,-8.63162196667495,
1436.95845526816));
#143107=CARTESIAN_POINT('Ctrl Pts',(-3.19993704609039,-8.42620218982176,
1437.35347894772));
#143108=CARTESIAN_POINT('Ctrl Pts',(-4.09885081991486,-8.02760290754512,
1438.25239272155));
#143109=CARTESIAN_POINT('Ctrl Pts',(-4.49222528611435,-7.80496687696196,
1438.82155204094));
#143110=CARTESIAN_POINT('Ctrl Pts',(-5.02262143709865,-7.47468272092311,
1440.08541735607));
#143111=CARTESIAN_POINT('Ctrl Pts',(-5.15937500000008,-7.37433723187243,
1440.7821328984));
#143112=CARTESIAN_POINT('Ctrl Pts',(-5.15937500000008,-7.37433723187243,
1441.45));
#143113=CARTESIAN_POINT('Ctrl Pts',(-5.15937500000008,-7.37433723187243,
1442.1178671016));
#143114=CARTESIAN_POINT('Ctrl Pts',(-5.02262143709865,-7.47468272092311,
1442.81458264393));
#143115=CARTESIAN_POINT('Ctrl Pts',(-4.49222528611435,-7.80496687696197,
1444.07844795906));
#143116=CARTESIAN_POINT('Ctrl Pts',(-4.09885081991486,-8.02760290754512,
1444.64760727845));
#143117=CARTESIAN_POINT('Ctrl Pts',(-3.19993704609039,-8.42620218982176,
1445.54652105228));
#143118=CARTESIAN_POINT('Ctrl Pts',(-2.63009169102989,-8.63162196667495,
1445.94154473184));
#143119=CARTESIAN_POINT('Ctrl Pts',(-1.36280970424649,-8.91992322022029,
1446.47335621405));
#143120=CARTESIAN_POINT('Ctrl Pts',(-0.664414150007844,-9.00000000000035,
1446.609375));
#143121=CARTESIAN_POINT('Ctrl Pts',(-1.09634523681734E-14,-9.00000000000035,
1446.609375));
#143122=CARTESIAN_POINT('',(-6.31841207935097E-16,-11.3170000000004,1446.609375));
#143123=CARTESIAN_POINT('',(-6.31841207935097E-16,50.8013494805973,1446.609375));
#143124=CARTESIAN_POINT('',(2.00906028488723E-14,-11.3170000000004,1436.290625));
#143125=CARTESIAN_POINT('Ctrl Pts',(-1.04083408558608E-14,-11.3170000000004,
1446.609375));
#143126=CARTESIAN_POINT('Ctrl Pts',(-0.657970384764804,-11.3170000000004,
1446.609375));
#143127=CARTESIAN_POINT('Ctrl Pts',(-1.35344266229499,-11.2542369285791,
1446.47591649128));
#143128=CARTESIAN_POINT('Ctrl Pts',(-2.62207755819474,-11.0278903257139,
1445.94625975887));
#143129=CARTESIAN_POINT('Ctrl Pts',(-3.19590327436269,-10.8668770896512,
1445.55055482401));
#143130=CARTESIAN_POINT('Ctrl Pts',(-4.10136924643444,-10.5585230349079,
1444.64508885193));
#143131=CARTESIAN_POINT('Ctrl Pts',(-4.49646674026965,-10.3894819155765,
1444.07155417537));
#143132=CARTESIAN_POINT('Ctrl Pts',(-5.02564501462738,-10.1440843535218,
1442.8041205208));
#143133=CARTESIAN_POINT('Ctrl Pts',(-5.15937500000008,-10.0725040883279,
1442.1091550748));
#143134=CARTESIAN_POINT('Ctrl Pts',(-5.15937500000008,-10.0725040883279,
1441.45));
#143135=CARTESIAN_POINT('Ctrl Pts',(-5.15937500000008,-10.0725040883279,
1440.7908449252));
#143136=CARTESIAN_POINT('Ctrl Pts',(-5.02564501462738,-10.1440843535218,
1440.0958794792));
#143137=CARTESIAN_POINT('Ctrl Pts',(-4.49646674026965,-10.3894819155765,
1438.82844582463));
#143138=CARTESIAN_POINT('Ctrl Pts',(-4.10136924643445,-10.5585230349079,
1438.25491114807));
#143139=CARTESIAN_POINT('Ctrl Pts',(-3.19590327436269,-10.8668770896512,
1437.34944517599));
#143140=CARTESIAN_POINT('Ctrl Pts',(-2.62207755819474,-11.0278903257139,
1436.95374024113));
#143141=CARTESIAN_POINT('Ctrl Pts',(-1.35344266229499,-11.2542369285791,
1436.42408350872));
#143142=CARTESIAN_POINT('Ctrl Pts',(-0.657970384764801,-11.3170000000004,
1436.290625));
#143143=CARTESIAN_POINT('Ctrl Pts',(-6.66133814775094E-15,-11.3170000000004,
1436.290625));
#143144=CARTESIAN_POINT('Ctrl Pts',(2.23432383705813E-14,-11.3170000000004,
1436.290625));
#143145=CARTESIAN_POINT('Ctrl Pts',(0.657970384764816,-11.3170000000004,
1436.290625));
#143146=CARTESIAN_POINT('Ctrl Pts',(1.35344266229499,-11.2542369285791,
1436.42408350872));
#143147=CARTESIAN_POINT('Ctrl Pts',(2.62207755819474,-11.0278903257139,
1436.95374024113));
#143148=CARTESIAN_POINT('Ctrl Pts',(3.19590327436269,-10.8668770896512,
1437.34944517599));
#143149=CARTESIAN_POINT('Ctrl Pts',(4.10136924643445,-10.5585230349079,
1438.25491114807));
#143150=CARTESIAN_POINT('Ctrl Pts',(4.49646674026965,-10.3894819155765,
1438.82844582463));
#143151=CARTESIAN_POINT('Ctrl Pts',(5.02564501462738,-10.1440843535218,
1440.0958794792));
#143152=CARTESIAN_POINT('Ctrl Pts',(5.15937500000008,-10.0725040883279,
1440.7908449252));
#143153=CARTESIAN_POINT('Ctrl Pts',(5.15937500000008,-10.0725040883279,
1442.1091550748));
#143154=CARTESIAN_POINT('Ctrl Pts',(5.02564501462738,-10.1440843535218,
1442.8041205208));
#143155=CARTESIAN_POINT('Ctrl Pts',(4.49646674026965,-10.3894819155765,
1444.07155417537));
#143156=CARTESIAN_POINT('Ctrl Pts',(4.10136924643444,-10.5585230349079,
1444.64508885193));
#143157=CARTESIAN_POINT('Ctrl Pts',(3.19590327436268,-10.8668770896512,
1445.55055482401));
#143158=CARTESIAN_POINT('Ctrl Pts',(2.62207755819474,-11.0278903257139,
1445.94625975887));
#143159=CARTESIAN_POINT('Ctrl Pts',(1.35344266229499,-11.2542369285791,
1446.47591649128));
#143160=CARTESIAN_POINT('Ctrl Pts',(0.657970384764803,-11.3170000000004,
1446.609375));
#143161=CARTESIAN_POINT('Ctrl Pts',(9.36750677027476E-15,-11.3170000000004,
1446.609375));
#143162=CARTESIAN_POINT('Ctrl Pts',(-5.55111512312578E-16,-9.00000000000036,
1446.609375));
#143163=CARTESIAN_POINT('Ctrl Pts',(0.664414150007831,-9.00000000000036,
1446.609375));
#143164=CARTESIAN_POINT('Ctrl Pts',(1.36280970424649,-8.91992322022029,
1446.47335621405));
#143165=CARTESIAN_POINT('Ctrl Pts',(2.63009169102989,-8.63162196667495,
1445.94154473184));
#143166=CARTESIAN_POINT('Ctrl Pts',(3.19993704609039,-8.42620218982176,
1445.54652105228));
#143167=CARTESIAN_POINT('Ctrl Pts',(4.09885081991486,-8.02760290754512,
1444.64760727845));
#143168=CARTESIAN_POINT('Ctrl Pts',(4.49222528611435,-7.80496687696197,
1444.07844795906));
#143169=CARTESIAN_POINT('Ctrl Pts',(5.02262143709865,-7.47468272092311,
1442.81458264393));
#143170=CARTESIAN_POINT('Ctrl Pts',(5.15937500000008,-7.37433723187243,
1442.1178671016));
#143171=CARTESIAN_POINT('Ctrl Pts',(5.15937500000008,-7.37433723187243,
1440.7821328984));
#143172=CARTESIAN_POINT('Ctrl Pts',(5.02262143709865,-7.47468272092311,
1440.08541735607));
#143173=CARTESIAN_POINT('Ctrl Pts',(4.49222528611435,-7.80496687696196,
1438.82155204094));
#143174=CARTESIAN_POINT('Ctrl Pts',(4.09885081991486,-8.02760290754512,
1438.25239272155));
#143175=CARTESIAN_POINT('Ctrl Pts',(3.19993704609039,-8.42620218982176,
1437.35347894772));
#143176=CARTESIAN_POINT('Ctrl Pts',(2.6300916910299,-8.63162196667495,1436.95845526816));
#143177=CARTESIAN_POINT('Ctrl Pts',(1.36280970424649,-8.91992322022029,
1436.42664378595));
#143178=CARTESIAN_POINT('Ctrl Pts',(0.664414150007828,-9.00000000000036,
1436.290625));
#143179=CARTESIAN_POINT('Ctrl Pts',(-4.71844785465692E-15,-9.00000000000036,
1436.290625));
#143180=CARTESIAN_POINT('Origin',(0.,0.,0.));
#143181=CARTESIAN_POINT('',(-1.38593278259508E-15,-11.3170000000004,1428.75));
#143182=CARTESIAN_POINT('Origin',(0.,-1.74262261732341E-13,1428.75));
#143183=CARTESIAN_POINT('',(-1.38593278259508E-15,-11.3170000000002,-1.38031567175848E-15));
#143184=CARTESIAN_POINT('',(-1.38593278259508E-15,-11.3170000000002,-1.38031567175848E-15));
#143185=CARTESIAN_POINT('Origin',(0.,0.,0.));
#143186=CARTESIAN_POINT('',(-1.10218211923264E-15,-9.00000000000018,-1.09771503453445E-15));
#143187=CARTESIAN_POINT('',(-1.10218211923264E-15,-9.00000000000035,1428.75));
#143188=CARTESIAN_POINT('',(-1.10218211923264E-15,-9.00000000000018,-1.09771503453445E-15));
#143189=CARTESIAN_POINT('Origin',(0.,-1.74262261732341E-13,1428.75));
#143190=CARTESIAN_POINT('Origin',(0.,11.317,1504.95));
#143191=CARTESIAN_POINT('Origin',(0.,11.317,1428.75));
#143192=CARTESIAN_POINT('Origin',(5.37704275891775E-14,4.44089209850063E-14,
1504.8993152933));
#143193=CARTESIAN_POINT('',(5.15601850460762E-14,18.048,1454.04863058659));
#143194=CARTESIAN_POINT('',(5.15601850460762E-14,18.048,1454.15));
#143195=CARTESIAN_POINT('',(1.05330612635254E-13,18.0480000000001,1504.8993152933));
#143196=CARTESIAN_POINT('',(0.,-18.048,1504.84863058659));
#143197=CARTESIAN_POINT('Ctrl Pts',(0.,-18.048,1504.84863058659));
#143198=CARTESIAN_POINT('Ctrl Pts',(-1.6723934873761,-18.048,1503.35451293953));
#143199=CARTESIAN_POINT('Ctrl Pts',(-3.31631129755346,-17.7406985030951,
1501.86039529247));
#143200=CARTESIAN_POINT('Ctrl Pts',(-4.96022910773077,-17.4333970061901,
1500.36627764542));
#143201=CARTESIAN_POINT('Ctrl Pts',(-6.51968959134574,-16.8292587962898,
1498.87215999836));
#143202=CARTESIAN_POINT('Ctrl Pts',(-8.07915007496071,-16.2251205863895,
1497.3780423513));
#143203=CARTESIAN_POINT('Ctrl Pts',(-9.50104767561052,-15.3447188656481,
1495.88392470424));
#143204=CARTESIAN_POINT('Ctrl Pts',(-10.9229452762603,-14.4643171449067,
1494.38980705718));
#143205=CARTESIAN_POINT('Ctrl Pts',(-12.1588589765331,-13.3376329379985,
1492.89568941012));
#143206=CARTESIAN_POINT('Ctrl Pts',(-13.3947726768058,-12.2109487310903,
1491.40157176306));
#143207=CARTESIAN_POINT('Ctrl Pts',(-14.4026149179538,-10.8763499173728,
1489.907454116));
#143208=CARTESIAN_POINT('Ctrl Pts',(-15.4104571591017,-9.54175110365538,
1488.41333646895));
#143209=CARTESIAN_POINT('Ctrl Pts',(-16.1559070823762,-8.04468584505497,
1486.91921882189));
#143210=CARTESIAN_POINT('Ctrl Pts',(-16.9013570056506,-6.54762058645456,
1485.42510117483));
#143211=CARTESIAN_POINT('Ctrl Pts',(-17.3590292079831,-4.93906964482095,
1483.93098352777));
#143212=CARTESIAN_POINT('Ctrl Pts',(-17.8167014103155,-3.33051870318735,
1482.43686588071));
#143213=CARTESIAN_POINT('Ctrl Pts',(-17.9710104137728,-1.66525935159368,
1480.94274823365));
#143214=CARTESIAN_POINT('Ctrl Pts',(-18.1253194172301,-1.10985572039171E-15,
1479.44863058659));
#143215=CARTESIAN_POINT('Ctrl Pts',(-17.9710104137728,1.66525935159367,
1477.95451293953));
#143216=CARTESIAN_POINT('Ctrl Pts',(-17.8167014103155,3.33051870318735,
1476.46039529247));
#143217=CARTESIAN_POINT('Ctrl Pts',(-17.3590292079831,4.93906964482096,
1474.96627764542));
#143218=CARTESIAN_POINT('Ctrl Pts',(-16.9013570056506,6.54762058645456,
1473.47215999836));
#143219=CARTESIAN_POINT('Ctrl Pts',(-16.1559070823762,8.04468584505497,
1471.9780423513));
#143220=CARTESIAN_POINT('Ctrl Pts',(-15.4104571591017,9.54175110365538,
1470.48392470424));
#143221=CARTESIAN_POINT('Ctrl Pts',(-14.4026149179538,10.8763499173728,
1468.98980705718));
#143222=CARTESIAN_POINT('Ctrl Pts',(-13.3947726768058,12.2109487310903,
1467.49568941012));
#143223=CARTESIAN_POINT('Ctrl Pts',(-12.1588589765331,13.3376329379985,
1466.00157176306));
#143224=CARTESIAN_POINT('Ctrl Pts',(-10.9229452762603,14.4643171449067,
1464.507454116));
#143225=CARTESIAN_POINT('Ctrl Pts',(-9.50104767561052,15.3447188656481,
1463.01333646895));
#143226=CARTESIAN_POINT('Ctrl Pts',(-8.07915007496071,16.2251205863895,
1461.51921882189));
#143227=CARTESIAN_POINT('Ctrl Pts',(-6.51968959134574,16.8292587962898,
1460.02510117483));
#143228=CARTESIAN_POINT('Ctrl Pts',(-4.96022910773078,17.4333970061901,
1458.53098352777));
#143229=CARTESIAN_POINT('Ctrl Pts',(-3.31631129755346,17.7406985030951,
1457.03686588071));
#143230=CARTESIAN_POINT('Ctrl Pts',(-1.67239348737615,18.048,1455.54274823365));
#143231=CARTESIAN_POINT('Ctrl Pts',(-2.21024254310115E-15,18.048,1454.04863058659));
#143232=CARTESIAN_POINT('',(0.,-18.048,1504.95));
#143233=CARTESIAN_POINT('',(0.,-18.048,1504.95));
#143234=CARTESIAN_POINT('Ctrl Pts',(0.,-18.048,1504.95));
#143235=CARTESIAN_POINT('Ctrl Pts',(-1.67239348737621,-18.048,1503.45588235294));
#143236=CARTESIAN_POINT('Ctrl Pts',(-3.31631129755346,-17.7406985030951,
1501.96176470588));
#143237=CARTESIAN_POINT('Ctrl Pts',(-4.96022910773077,-17.4333970061901,
1500.46764705882));
#143238=CARTESIAN_POINT('Ctrl Pts',(-6.51968959134574,-16.8292587962898,
1498.97352941176));
#143239=CARTESIAN_POINT('Ctrl Pts',(-8.07915007496071,-16.2251205863895,
1497.47941176471));
#143240=CARTESIAN_POINT('Ctrl Pts',(-9.50104767561052,-15.3447188656481,
1495.98529411765));
#143241=CARTESIAN_POINT('Ctrl Pts',(-10.9229452762603,-14.4643171449067,
1494.49117647059));
#143242=CARTESIAN_POINT('Ctrl Pts',(-12.1588589765331,-13.3376329379985,
1492.99705882353));
#143243=CARTESIAN_POINT('Ctrl Pts',(-13.3947726768058,-12.2109487310903,
1491.50294117647));
#143244=CARTESIAN_POINT('Ctrl Pts',(-14.4026149179538,-10.8763499173728,
1490.00882352941));
#143245=CARTESIAN_POINT('Ctrl Pts',(-15.4104571591017,-9.54175110365538,
1488.51470588235));
#143246=CARTESIAN_POINT('Ctrl Pts',(-16.1559070823762,-8.04468584505497,
1487.02058823529));
#143247=CARTESIAN_POINT('Ctrl Pts',(-16.9013570056506,-6.54762058645456,
1485.52647058824));
#143248=CARTESIAN_POINT('Ctrl Pts',(-17.3590292079831,-4.93906964482095,
1484.03235294118));
#143249=CARTESIAN_POINT('Ctrl Pts',(-17.8167014103155,-3.33051870318735,
1482.53823529412));
#143250=CARTESIAN_POINT('Ctrl Pts',(-17.9710104137728,-1.66525935159368,
1481.04411764706));
#143251=CARTESIAN_POINT('Ctrl Pts',(-18.1253194172301,-1.10985572039171E-15,
1479.55));
#143252=CARTESIAN_POINT('Ctrl Pts',(-17.9710104137728,1.66525935159367,
1478.05588235294));
#143253=CARTESIAN_POINT('Ctrl Pts',(-17.8167014103155,3.33051870318735,
1476.56176470588));
#143254=CARTESIAN_POINT('Ctrl Pts',(-17.3590292079831,4.93906964482096,
1475.06764705882));
#143255=CARTESIAN_POINT('Ctrl Pts',(-16.9013570056506,6.54762058645456,
1473.57352941176));
#143256=CARTESIAN_POINT('Ctrl Pts',(-16.1559070823762,8.04468584505497,
1472.07941176471));
#143257=CARTESIAN_POINT('Ctrl Pts',(-15.4104571591017,9.54175110365538,
1470.58529411765));
#143258=CARTESIAN_POINT('Ctrl Pts',(-14.4026149179538,10.8763499173728,
1469.09117647059));
#143259=CARTESIAN_POINT('Ctrl Pts',(-13.3947726768058,12.2109487310903,
1467.59705882353));
#143260=CARTESIAN_POINT('Ctrl Pts',(-12.1588589765331,13.3376329379985,
1466.10294117647));
#143261=CARTESIAN_POINT('Ctrl Pts',(-10.9229452762603,14.4643171449067,
1464.60882352941));
#143262=CARTESIAN_POINT('Ctrl Pts',(-9.50104767561052,15.3447188656481,
1463.11470588235));
#143263=CARTESIAN_POINT('Ctrl Pts',(-8.07915007496071,16.2251205863895,
1461.62058823529));
#143264=CARTESIAN_POINT('Ctrl Pts',(-6.51968959134574,16.8292587962898,
1460.12647058824));
#143265=CARTESIAN_POINT('Ctrl Pts',(-4.96022910773078,17.4333970061901,
1458.63235294118));
#143266=CARTESIAN_POINT('Ctrl Pts',(-3.31631129755346,17.7406985030951,
1457.13823529412));
#143267=CARTESIAN_POINT('Ctrl Pts',(-1.67239348737615,18.048,1455.64411764706));
#143268=CARTESIAN_POINT('Ctrl Pts',(-2.21024254310115E-15,18.048,1454.15));
#143269=CARTESIAN_POINT('Origin',(5.37704275891775E-14,4.44089209850063E-14,
1504.8993152933));
#143270=CARTESIAN_POINT('',(5.15601850460762E-14,18.048,1352.44863058659));
#143271=CARTESIAN_POINT('',(5.15601850460762E-14,18.048,1352.55));
#143272=CARTESIAN_POINT('',(1.05330612635254E-13,18.0480000000001,1504.8993152933));
#143273=CARTESIAN_POINT('Ctrl Pts',(-2.21024254310115E-15,18.048,1454.04863058659));
#143274=CARTESIAN_POINT('Ctrl Pts',(1.67239348737616,18.048,1452.55451293953));
#143275=CARTESIAN_POINT('Ctrl Pts',(3.31631129755346,17.7406985030951,1451.06039529247));
#143276=CARTESIAN_POINT('Ctrl Pts',(4.96022910773077,17.4333970061901,1449.56627764542));
#143277=CARTESIAN_POINT('Ctrl Pts',(6.51968959134575,16.8292587962898,1448.07215999836));
#143278=CARTESIAN_POINT('Ctrl Pts',(8.07915007496071,16.2251205863895,1446.5780423513));
#143279=CARTESIAN_POINT('Ctrl Pts',(9.50104767561053,15.3447188656481,1445.08392470424));
#143280=CARTESIAN_POINT('Ctrl Pts',(10.9229452762603,14.4643171449067,1443.58980705718));
#143281=CARTESIAN_POINT('Ctrl Pts',(12.1588589765331,13.3376329379985,1442.09568941012));
#143282=CARTESIAN_POINT('Ctrl Pts',(13.3947726768058,12.2109487310903,1440.60157176306));
#143283=CARTESIAN_POINT('Ctrl Pts',(14.4026149179538,10.8763499173728,1439.107454116));
#143284=CARTESIAN_POINT('Ctrl Pts',(15.4104571591017,9.54175110365539,1437.61333646895));
#143285=CARTESIAN_POINT('Ctrl Pts',(16.1559070823762,8.04468584505496,1436.11921882189));
#143286=CARTESIAN_POINT('Ctrl Pts',(16.9013570056506,6.54762058645456,1434.62510117483));
#143287=CARTESIAN_POINT('Ctrl Pts',(17.3590292079831,4.93906964482096,1433.13098352777));
#143288=CARTESIAN_POINT('Ctrl Pts',(17.8167014103155,3.33051870318735,1431.63686588071));
#143289=CARTESIAN_POINT('Ctrl Pts',(17.9710104137728,1.66525935159367,1430.14274823365));
#143290=CARTESIAN_POINT('Ctrl Pts',(18.1253194172301,3.32956716117513E-15,
1428.64863058659));
#143291=CARTESIAN_POINT('Ctrl Pts',(17.9710104137728,-1.66525935159367,
1427.15451293953));
#143292=CARTESIAN_POINT('Ctrl Pts',(17.8167014103155,-3.33051870318736,
1425.66039529247));
#143293=CARTESIAN_POINT('Ctrl Pts',(17.3590292079831,-4.93906964482095,
1424.16627764542));
#143294=CARTESIAN_POINT('Ctrl Pts',(16.9013570056506,-6.54762058645456,
1422.67215999836));
#143295=CARTESIAN_POINT('Ctrl Pts',(16.1559070823762,-8.04468584505497,
1421.1780423513));
#143296=CARTESIAN_POINT('Ctrl Pts',(15.4104571591017,-9.54175110365538,
1419.68392470424));
#143297=CARTESIAN_POINT('Ctrl Pts',(14.4026149179538,-10.8763499173728,
1418.18980705718));
#143298=CARTESIAN_POINT('Ctrl Pts',(13.3947726768058,-12.2109487310903,
1416.69568941012));
#143299=CARTESIAN_POINT('Ctrl Pts',(12.1588589765331,-13.3376329379985,
1415.20157176306));
#143300=CARTESIAN_POINT('Ctrl Pts',(10.9229452762603,-14.4643171449067,
1413.707454116));
#143301=CARTESIAN_POINT('Ctrl Pts',(9.50104767561053,-15.3447188656481,
1412.21333646895));
#143302=CARTESIAN_POINT('Ctrl Pts',(8.07915007496071,-16.2251205863895,
1410.71921882189));
#143303=CARTESIAN_POINT('Ctrl Pts',(6.51968959134574,-16.8292587962898,
1409.22510117483));
#143304=CARTESIAN_POINT('Ctrl Pts',(4.96022910773078,-17.4333970061901,
1407.73098352777));
#143305=CARTESIAN_POINT('Ctrl Pts',(3.31631129755346,-17.7406985030951,
1406.23686588071));
#143306=CARTESIAN_POINT('Ctrl Pts',(1.67239348737615,-18.048,1404.74274823365));
#143307=CARTESIAN_POINT('Ctrl Pts',(0.,-18.048,1403.24863058659));
#143308=CARTESIAN_POINT('Ctrl Pts',(-1.67239348737615,-18.048,1401.75451293953));
#143309=CARTESIAN_POINT('Ctrl Pts',(-3.31631129755346,-17.7406985030951,
1400.26039529247));
#143310=CARTESIAN_POINT('Ctrl Pts',(-4.96022910773077,-17.4333970061901,
1398.76627764542));
#143311=CARTESIAN_POINT('Ctrl Pts',(-6.51968959134574,-16.8292587962898,
1397.27215999836));
#143312=CARTESIAN_POINT('Ctrl Pts',(-8.07915007496071,-16.2251205863895,
1395.7780423513));
#143313=CARTESIAN_POINT('Ctrl Pts',(-9.50104767561052,-15.3447188656481,
1394.28392470424));
#143314=CARTESIAN_POINT('Ctrl Pts',(-10.9229452762603,-14.4643171449067,
1392.78980705718));
#143315=CARTESIAN_POINT('Ctrl Pts',(-12.1588589765331,-13.3376329379985,
1391.29568941012));
#143316=CARTESIAN_POINT('Ctrl Pts',(-13.3947726768058,-12.2109487310903,
1389.80157176306));
#143317=CARTESIAN_POINT('Ctrl Pts',(-14.4026149179538,-10.8763499173728,
1388.307454116));
#143318=CARTESIAN_POINT('Ctrl Pts',(-15.4104571591017,-9.54175110365538,
1386.81333646895));
#143319=CARTESIAN_POINT('Ctrl Pts',(-16.1559070823762,-8.04468584505497,
1385.31921882189));
#143320=CARTESIAN_POINT('Ctrl Pts',(-16.9013570056506,-6.54762058645456,
1383.82510117483));
#143321=CARTESIAN_POINT('Ctrl Pts',(-17.3590292079831,-4.93906964482095,
1382.33098352777));
#143322=CARTESIAN_POINT('Ctrl Pts',(-17.8167014103155,-3.33051870318735,
1380.83686588071));
#143323=CARTESIAN_POINT('Ctrl Pts',(-17.9710104137728,-1.66525935159368,
1379.34274823365));
#143324=CARTESIAN_POINT('Ctrl Pts',(-18.1253194172301,-1.10985572039171E-15,
1377.84863058659));
#143325=CARTESIAN_POINT('Ctrl Pts',(-17.9710104137728,1.66525935159367,
1376.35451293953));
#143326=CARTESIAN_POINT('Ctrl Pts',(-17.8167014103155,3.33051870318735,
1374.86039529247));
#143327=CARTESIAN_POINT('Ctrl Pts',(-17.3590292079831,4.93906964482096,
1373.36627764542));
#143328=CARTESIAN_POINT('Ctrl Pts',(-16.9013570056506,6.54762058645456,
1371.87215999836));
#143329=CARTESIAN_POINT('Ctrl Pts',(-16.1559070823762,8.04468584505497,
1370.3780423513));
#143330=CARTESIAN_POINT('Ctrl Pts',(-15.4104571591017,9.54175110365538,
1368.88392470424));
#143331=CARTESIAN_POINT('Ctrl Pts',(-14.4026149179538,10.8763499173728,
1367.38980705718));
#143332=CARTESIAN_POINT('Ctrl Pts',(-13.3947726768058,12.2109487310903,
1365.89568941012));
#143333=CARTESIAN_POINT('Ctrl Pts',(-12.1588589765331,13.3376329379985,
1364.40157176306));
#143334=CARTESIAN_POINT('Ctrl Pts',(-10.9229452762603,14.4643171449067,
1362.907454116));
#143335=CARTESIAN_POINT('Ctrl Pts',(-9.50104767561052,15.3447188656481,
1361.41333646895));
#143336=CARTESIAN_POINT('Ctrl Pts',(-8.07915007496071,16.2251205863895,
1359.91921882189));
#143337=CARTESIAN_POINT('Ctrl Pts',(-6.51968959134574,16.8292587962898,
1358.42510117483));
#143338=CARTESIAN_POINT('Ctrl Pts',(-4.96022910773078,17.4333970061901,
1356.93098352777));
#143339=CARTESIAN_POINT('Ctrl Pts',(-3.31631129755346,17.7406985030951,
1355.43686588071));
#143340=CARTESIAN_POINT('Ctrl Pts',(-1.67239348737615,18.048,1353.94274823365));
#143341=CARTESIAN_POINT('Ctrl Pts',(-2.21024254310115E-15,18.048,1352.44863058659));
#143342=CARTESIAN_POINT('Ctrl Pts',(-2.21024254310115E-15,18.048,1454.15));
#143343=CARTESIAN_POINT('Ctrl Pts',(1.67239348737616,18.048,1452.65588235294));
#143344=CARTESIAN_POINT('Ctrl Pts',(3.31631129755346,17.7406985030951,1451.16176470588));
#143345=CARTESIAN_POINT('Ctrl Pts',(4.96022910773077,17.4333970061901,1449.66764705882));
#143346=CARTESIAN_POINT('Ctrl Pts',(6.51968959134575,16.8292587962898,1448.17352941177));
#143347=CARTESIAN_POINT('Ctrl Pts',(8.07915007496071,16.2251205863895,1446.67941176471));
#143348=CARTESIAN_POINT('Ctrl Pts',(9.50104767561053,15.3447188656481,1445.18529411765));
#143349=CARTESIAN_POINT('Ctrl Pts',(10.9229452762603,14.4643171449067,1443.69117647059));
#143350=CARTESIAN_POINT('Ctrl Pts',(12.1588589765331,13.3376329379985,1442.19705882353));
#143351=CARTESIAN_POINT('Ctrl Pts',(13.3947726768058,12.2109487310903,1440.70294117647));
#143352=CARTESIAN_POINT('Ctrl Pts',(14.4026149179538,10.8763499173728,1439.20882352941));
#143353=CARTESIAN_POINT('Ctrl Pts',(15.4104571591017,9.54175110365539,1437.71470588235));
#143354=CARTESIAN_POINT('Ctrl Pts',(16.1559070823762,8.04468584505496,1436.22058823529));
#143355=CARTESIAN_POINT('Ctrl Pts',(16.9013570056506,6.54762058645456,1434.72647058824));
#143356=CARTESIAN_POINT('Ctrl Pts',(17.3590292079831,4.93906964482096,1433.23235294118));
#143357=CARTESIAN_POINT('Ctrl Pts',(17.8167014103155,3.33051870318735,1431.73823529412));
#143358=CARTESIAN_POINT('Ctrl Pts',(17.9710104137728,1.66525935159367,1430.24411764706));
#143359=CARTESIAN_POINT('Ctrl Pts',(18.1253194172301,3.32956716117513E-15,
1428.75));
#143360=CARTESIAN_POINT('Ctrl Pts',(17.9710104137728,-1.66525935159367,
1427.25588235294));
#143361=CARTESIAN_POINT('Ctrl Pts',(17.8167014103155,-3.33051870318736,
1425.76176470588));
#143362=CARTESIAN_POINT('Ctrl Pts',(17.3590292079831,-4.93906964482095,
1424.26764705882));
#143363=CARTESIAN_POINT('Ctrl Pts',(16.9013570056506,-6.54762058645456,
1422.77352941176));
#143364=CARTESIAN_POINT('Ctrl Pts',(16.1559070823762,-8.04468584505497,
1421.27941176471));
#143365=CARTESIAN_POINT('Ctrl Pts',(15.4104571591017,-9.54175110365538,
1419.78529411765));
#143366=CARTESIAN_POINT('Ctrl Pts',(14.4026149179538,-10.8763499173728,
1418.29117647059));
#143367=CARTESIAN_POINT('Ctrl Pts',(13.3947726768058,-12.2109487310903,
1416.79705882353));
#143368=CARTESIAN_POINT('Ctrl Pts',(12.1588589765331,-13.3376329379985,
1415.30294117647));
#143369=CARTESIAN_POINT('Ctrl Pts',(10.9229452762603,-14.4643171449067,
1413.80882352941));
#143370=CARTESIAN_POINT('Ctrl Pts',(9.50104767561053,-15.3447188656481,
1412.31470588235));
#143371=CARTESIAN_POINT('Ctrl Pts',(8.07915007496071,-16.2251205863895,
1410.82058823529));
#143372=CARTESIAN_POINT('Ctrl Pts',(6.51968959134574,-16.8292587962898,
1409.32647058824));
#143373=CARTESIAN_POINT('Ctrl Pts',(4.96022910773078,-17.4333970061901,
1407.83235294118));
#143374=CARTESIAN_POINT('Ctrl Pts',(3.31631129755346,-17.7406985030951,
1406.33823529412));
#143375=CARTESIAN_POINT('Ctrl Pts',(1.67239348737615,-18.048,1404.84411764706));
#143376=CARTESIAN_POINT('Ctrl Pts',(0.,-18.048,1403.35));
#143377=CARTESIAN_POINT('Ctrl Pts',(-1.67239348737615,-18.048,1401.85588235294));
#143378=CARTESIAN_POINT('Ctrl Pts',(-3.31631129755346,-17.7406985030951,
1400.36176470588));
#143379=CARTESIAN_POINT('Ctrl Pts',(-4.96022910773077,-17.4333970061901,
1398.86764705882));
#143380=CARTESIAN_POINT('Ctrl Pts',(-6.51968959134574,-16.8292587962898,
1397.37352941176));
#143381=CARTESIAN_POINT('Ctrl Pts',(-8.07915007496071,-16.2251205863895,
1395.87941176471));
#143382=CARTESIAN_POINT('Ctrl Pts',(-9.50104767561052,-15.3447188656481,
1394.38529411765));
#143383=CARTESIAN_POINT('Ctrl Pts',(-10.9229452762603,-14.4643171449067,
1392.89117647059));
#143384=CARTESIAN_POINT('Ctrl Pts',(-12.1588589765331,-13.3376329379985,
1391.39705882353));
#143385=CARTESIAN_POINT('Ctrl Pts',(-13.3947726768058,-12.2109487310903,
1389.90294117647));
#143386=CARTESIAN_POINT('Ctrl Pts',(-14.4026149179538,-10.8763499173728,
1388.40882352941));
#143387=CARTESIAN_POINT('Ctrl Pts',(-15.4104571591017,-9.54175110365538,
1386.91470588235));
#143388=CARTESIAN_POINT('Ctrl Pts',(-16.1559070823762,-8.04468584505497,
1385.42058823529));
#143389=CARTESIAN_POINT('Ctrl Pts',(-16.9013570056506,-6.54762058645456,
1383.92647058824));
#143390=CARTESIAN_POINT('Ctrl Pts',(-17.3590292079831,-4.93906964482095,
1382.43235294118));
#143391=CARTESIAN_POINT('Ctrl Pts',(-17.8167014103155,-3.33051870318735,
1380.93823529412));
#143392=CARTESIAN_POINT('Ctrl Pts',(-17.9710104137728,-1.66525935159368,
1379.44411764706));
#143393=CARTESIAN_POINT('Ctrl Pts',(-18.1253194172301,-1.10985572039171E-15,
1377.95));
#143394=CARTESIAN_POINT('Ctrl Pts',(-17.9710104137728,1.66525935159367,
1376.45588235294));
#143395=CARTESIAN_POINT('Ctrl Pts',(-17.8167014103155,3.33051870318735,
1374.96176470588));
#143396=CARTESIAN_POINT('Ctrl Pts',(-17.3590292079831,4.93906964482096,
1373.46764705882));
#143397=CARTESIAN_POINT('Ctrl Pts',(-16.9013570056506,6.54762058645456,
1371.97352941176));
#143398=CARTESIAN_POINT('Ctrl Pts',(-16.1559070823762,8.04468584505497,
1370.47941176471));
#143399=CARTESIAN_POINT('Ctrl Pts',(-15.4104571591017,9.54175110365538,
1368.98529411765));
#143400=CARTESIAN_POINT('Ctrl Pts',(-14.4026149179538,10.8763499173728,
1367.49117647059));
#143401=CARTESIAN_POINT('Ctrl Pts',(-13.3947726768058,12.2109487310903,
1365.99705882353));
#143402=CARTESIAN_POINT('Ctrl Pts',(-12.1588589765331,13.3376329379985,
1364.50294117647));
#143403=CARTESIAN_POINT('Ctrl Pts',(-10.9229452762603,14.4643171449067,
1363.00882352941));
#143404=CARTESIAN_POINT('Ctrl Pts',(-9.50104767561052,15.3447188656481,
1361.51470588235));
#143405=CARTESIAN_POINT('Ctrl Pts',(-8.07915007496071,16.2251205863895,
1360.02058823529));
#143406=CARTESIAN_POINT('Ctrl Pts',(-6.51968959134574,16.8292587962898,
1358.52647058824));
#143407=CARTESIAN_POINT('Ctrl Pts',(-4.96022910773078,17.4333970061901,
1357.03235294118));
#143408=CARTESIAN_POINT('Ctrl Pts',(-3.31631129755346,17.7406985030951,
1355.53823529412));
#143409=CARTESIAN_POINT('Ctrl Pts',(-1.67239348737615,18.048,1354.04411764706));
#143410=CARTESIAN_POINT('Ctrl Pts',(-2.21024254310115E-15,18.048,1352.55));
#143411=CARTESIAN_POINT('Origin',(5.37704275891775E-14,4.44089209850063E-14,
1504.8993152933));
#143412=CARTESIAN_POINT('',(5.15601850460762E-14,18.048,1250.84863058659));
#143413=CARTESIAN_POINT('',(5.15601850460762E-14,18.048,1250.95));
#143414=CARTESIAN_POINT('',(1.05330612635254E-13,18.0480000000001,1504.8993152933));
#143415=CARTESIAN_POINT('Ctrl Pts',(-2.21024254310115E-15,18.048,1352.44863058659));
#143416=CARTESIAN_POINT('Ctrl Pts',(1.67239348737616,18.048,1350.95451293953));
#143417=CARTESIAN_POINT('Ctrl Pts',(3.31631129755346,17.7406985030951,1349.46039529247));
#143418=CARTESIAN_POINT('Ctrl Pts',(4.96022910773077,17.4333970061901,1347.96627764542));
#143419=CARTESIAN_POINT('Ctrl Pts',(6.51968959134575,16.8292587962898,1346.47215999836));
#143420=CARTESIAN_POINT('Ctrl Pts',(8.07915007496071,16.2251205863895,1344.9780423513));
#143421=CARTESIAN_POINT('Ctrl Pts',(9.50104767561053,15.3447188656481,1343.48392470424));
#143422=CARTESIAN_POINT('Ctrl Pts',(10.9229452762603,14.4643171449067,1341.98980705718));
#143423=CARTESIAN_POINT('Ctrl Pts',(12.1588589765331,13.3376329379985,1340.49568941012));
#143424=CARTESIAN_POINT('Ctrl Pts',(13.3947726768058,12.2109487310903,1339.00157176306));
#143425=CARTESIAN_POINT('Ctrl Pts',(14.4026149179538,10.8763499173728,1337.507454116));
#143426=CARTESIAN_POINT('Ctrl Pts',(15.4104571591017,9.54175110365539,1336.01333646895));
#143427=CARTESIAN_POINT('Ctrl Pts',(16.1559070823762,8.04468584505496,1334.51921882189));
#143428=CARTESIAN_POINT('Ctrl Pts',(16.9013570056506,6.54762058645456,1333.02510117483));
#143429=CARTESIAN_POINT('Ctrl Pts',(17.3590292079831,4.93906964482096,1331.53098352777));
#143430=CARTESIAN_POINT('Ctrl Pts',(17.8167014103155,3.33051870318735,1330.03686588071));
#143431=CARTESIAN_POINT('Ctrl Pts',(17.9710104137728,1.66525935159367,1328.54274823365));
#143432=CARTESIAN_POINT('Ctrl Pts',(18.1253194172301,3.32956716117513E-15,
1327.04863058659));
#143433=CARTESIAN_POINT('Ctrl Pts',(17.9710104137728,-1.66525935159367,
1325.55451293953));
#143434=CARTESIAN_POINT('Ctrl Pts',(17.8167014103155,-3.33051870318736,
1324.06039529247));
#143435=CARTESIAN_POINT('Ctrl Pts',(17.3590292079831,-4.93906964482095,
1322.56627764542));
#143436=CARTESIAN_POINT('Ctrl Pts',(16.9013570056506,-6.54762058645456,
1321.07215999836));
#143437=CARTESIAN_POINT('Ctrl Pts',(16.1559070823762,-8.04468584505497,
1319.5780423513));
#143438=CARTESIAN_POINT('Ctrl Pts',(15.4104571591017,-9.54175110365538,
1318.08392470424));
#143439=CARTESIAN_POINT('Ctrl Pts',(14.4026149179538,-10.8763499173728,
1316.58980705718));
#143440=CARTESIAN_POINT('Ctrl Pts',(13.3947726768058,-12.2109487310903,
1315.09568941012));
#143441=CARTESIAN_POINT('Ctrl Pts',(12.1588589765331,-13.3376329379985,
1313.60157176306));
#143442=CARTESIAN_POINT('Ctrl Pts',(10.9229452762603,-14.4643171449067,
1312.107454116));
#143443=CARTESIAN_POINT('Ctrl Pts',(9.50104767561053,-15.3447188656481,
1310.61333646895));
#143444=CARTESIAN_POINT('Ctrl Pts',(8.07915007496071,-16.2251205863895,
1309.11921882189));
#143445=CARTESIAN_POINT('Ctrl Pts',(6.51968959134574,-16.8292587962898,
1307.62510117483));
#143446=CARTESIAN_POINT('Ctrl Pts',(4.96022910773078,-17.4333970061901,
1306.13098352777));
#143447=CARTESIAN_POINT('Ctrl Pts',(3.31631129755346,-17.7406985030951,
1304.63686588071));
#143448=CARTESIAN_POINT('Ctrl Pts',(1.67239348737615,-18.048,1303.14274823365));
#143449=CARTESIAN_POINT('Ctrl Pts',(0.,-18.048,1301.64863058659));
#143450=CARTESIAN_POINT('Ctrl Pts',(-1.67239348737615,-18.048,1300.15451293953));
#143451=CARTESIAN_POINT('Ctrl Pts',(-3.31631129755346,-17.7406985030951,
1298.66039529247));
#143452=CARTESIAN_POINT('Ctrl Pts',(-4.96022910773077,-17.4333970061901,
1297.16627764542));
#143453=CARTESIAN_POINT('Ctrl Pts',(-6.51968959134574,-16.8292587962898,
1295.67215999836));
#143454=CARTESIAN_POINT('Ctrl Pts',(-8.07915007496071,-16.2251205863895,
1294.1780423513));
#143455=CARTESIAN_POINT('Ctrl Pts',(-9.50104767561052,-15.3447188656481,
1292.68392470424));
#143456=CARTESIAN_POINT('Ctrl Pts',(-10.9229452762603,-14.4643171449067,
1291.18980705718));
#143457=CARTESIAN_POINT('Ctrl Pts',(-12.1588589765331,-13.3376329379985,
1289.69568941012));
#143458=CARTESIAN_POINT('Ctrl Pts',(-13.3947726768058,-12.2109487310903,
1288.20157176306));
#143459=CARTESIAN_POINT('Ctrl Pts',(-14.4026149179538,-10.8763499173728,
1286.707454116));
#143460=CARTESIAN_POINT('Ctrl Pts',(-15.4104571591017,-9.54175110365538,
1285.21333646895));
#143461=CARTESIAN_POINT('Ctrl Pts',(-16.1559070823762,-8.04468584505497,
1283.71921882189));
#143462=CARTESIAN_POINT('Ctrl Pts',(-16.9013570056506,-6.54762058645456,
1282.22510117483));
#143463=CARTESIAN_POINT('Ctrl Pts',(-17.3590292079831,-4.93906964482095,
1280.73098352777));
#143464=CARTESIAN_POINT('Ctrl Pts',(-17.8167014103155,-3.33051870318735,
1279.23686588071));
#143465=CARTESIAN_POINT('Ctrl Pts',(-17.9710104137728,-1.66525935159368,
1277.74274823365));
#143466=CARTESIAN_POINT('Ctrl Pts',(-18.1253194172301,-1.10985572039171E-15,
1276.24863058659));
#143467=CARTESIAN_POINT('Ctrl Pts',(-17.9710104137728,1.66525935159367,
1274.75451293953));
#143468=CARTESIAN_POINT('Ctrl Pts',(-17.8167014103155,3.33051870318735,
1273.26039529247));
#143469=CARTESIAN_POINT('Ctrl Pts',(-17.3590292079831,4.93906964482096,
1271.76627764542));
#143470=CARTESIAN_POINT('Ctrl Pts',(-16.9013570056506,6.54762058645456,
1270.27215999836));
#143471=CARTESIAN_POINT('Ctrl Pts',(-16.1559070823762,8.04468584505497,
1268.7780423513));
#143472=CARTESIAN_POINT('Ctrl Pts',(-15.4104571591017,9.54175110365538,
1267.28392470424));
#143473=CARTESIAN_POINT('Ctrl Pts',(-14.4026149179538,10.8763499173728,
1265.78980705718));
#143474=CARTESIAN_POINT('Ctrl Pts',(-13.3947726768058,12.2109487310903,
1264.29568941012));
#143475=CARTESIAN_POINT('Ctrl Pts',(-12.1588589765331,13.3376329379985,
1262.80157176306));
#143476=CARTESIAN_POINT('Ctrl Pts',(-10.9229452762603,14.4643171449067,
1261.307454116));
#143477=CARTESIAN_POINT('Ctrl Pts',(-9.50104767561052,15.3447188656481,
1259.81333646895));
#143478=CARTESIAN_POINT('Ctrl Pts',(-8.07915007496071,16.2251205863895,
1258.31921882189));
#143479=CARTESIAN_POINT('Ctrl Pts',(-6.51968959134574,16.8292587962898,
1256.82510117483));
#143480=CARTESIAN_POINT('Ctrl Pts',(-4.96022910773078,17.4333970061901,
1255.33098352777));
#143481=CARTESIAN_POINT('Ctrl Pts',(-3.31631129755346,17.7406985030951,
1253.83686588071));
#143482=CARTESIAN_POINT('Ctrl Pts',(-1.67239348737615,18.048,1252.34274823365));
#143483=CARTESIAN_POINT('Ctrl Pts',(-2.21024254310115E-15,18.048,1250.84863058659));
#143484=CARTESIAN_POINT('Ctrl Pts',(-2.21024254310115E-15,18.048,1352.55));
#143485=CARTESIAN_POINT('Ctrl Pts',(1.67239348737616,18.048,1351.05588235294));
#143486=CARTESIAN_POINT('Ctrl Pts',(3.31631129755346,17.7406985030951,1349.56176470588));
#143487=CARTESIAN_POINT('Ctrl Pts',(4.96022910773077,17.4333970061901,1348.06764705882));
#143488=CARTESIAN_POINT('Ctrl Pts',(6.51968959134575,16.8292587962898,1346.57352941176));
#143489=CARTESIAN_POINT('Ctrl Pts',(8.07915007496071,16.2251205863895,1345.07941176471));
#143490=CARTESIAN_POINT('Ctrl Pts',(9.50104767561053,15.3447188656481,1343.58529411765));
#143491=CARTESIAN_POINT('Ctrl Pts',(10.9229452762603,14.4643171449067,1342.09117647059));
#143492=CARTESIAN_POINT('Ctrl Pts',(12.1588589765331,13.3376329379985,1340.59705882353));
#143493=CARTESIAN_POINT('Ctrl Pts',(13.3947726768058,12.2109487310903,1339.10294117647));
#143494=CARTESIAN_POINT('Ctrl Pts',(14.4026149179538,10.8763499173728,1337.60882352941));
#143495=CARTESIAN_POINT('Ctrl Pts',(15.4104571591017,9.54175110365539,1336.11470588235));
#143496=CARTESIAN_POINT('Ctrl Pts',(16.1559070823762,8.04468584505496,1334.62058823529));
#143497=CARTESIAN_POINT('Ctrl Pts',(16.9013570056506,6.54762058645456,1333.12647058824));
#143498=CARTESIAN_POINT('Ctrl Pts',(17.3590292079831,4.93906964482096,1331.63235294118));
#143499=CARTESIAN_POINT('Ctrl Pts',(17.8167014103155,3.33051870318735,1330.13823529412));
#143500=CARTESIAN_POINT('Ctrl Pts',(17.9710104137728,1.66525935159367,1328.64411764706));
#143501=CARTESIAN_POINT('Ctrl Pts',(18.1253194172301,3.32956716117513E-15,
1327.15));
#143502=CARTESIAN_POINT('Ctrl Pts',(17.9710104137728,-1.66525935159367,
1325.65588235294));
#143503=CARTESIAN_POINT('Ctrl Pts',(17.8167014103155,-3.33051870318736,
1324.16176470588));
#143504=CARTESIAN_POINT('Ctrl Pts',(17.3590292079831,-4.93906964482095,
1322.66764705882));
#143505=CARTESIAN_POINT('Ctrl Pts',(16.9013570056506,-6.54762058645456,
1321.17352941176));
#143506=CARTESIAN_POINT('Ctrl Pts',(16.1559070823762,-8.04468584505497,
1319.67941176471));
#143507=CARTESIAN_POINT('Ctrl Pts',(15.4104571591017,-9.54175110365538,
1318.18529411765));
#143508=CARTESIAN_POINT('Ctrl Pts',(14.4026149179538,-10.8763499173728,
1316.69117647059));
#143509=CARTESIAN_POINT('Ctrl Pts',(13.3947726768058,-12.2109487310903,
1315.19705882353));
#143510=CARTESIAN_POINT('Ctrl Pts',(12.1588589765331,-13.3376329379985,
1313.70294117647));
#143511=CARTESIAN_POINT('Ctrl Pts',(10.9229452762603,-14.4643171449067,
1312.20882352941));
#143512=CARTESIAN_POINT('Ctrl Pts',(9.50104767561053,-15.3447188656481,
1310.71470588235));
#143513=CARTESIAN_POINT('Ctrl Pts',(8.07915007496071,-16.2251205863895,
1309.22058823529));
#143514=CARTESIAN_POINT('Ctrl Pts',(6.51968959134574,-16.8292587962898,
1307.72647058824));
#143515=CARTESIAN_POINT('Ctrl Pts',(4.96022910773078,-17.4333970061901,
1306.23235294118));
#143516=CARTESIAN_POINT('Ctrl Pts',(3.31631129755346,-17.7406985030951,
1304.73823529412));
#143517=CARTESIAN_POINT('Ctrl Pts',(1.67239348737615,-18.048,1303.24411764706));
#143518=CARTESIAN_POINT('Ctrl Pts',(0.,-18.048,1301.75));
#143519=CARTESIAN_POINT('Ctrl Pts',(-1.67239348737615,-18.048,1300.25588235294));
#143520=CARTESIAN_POINT('Ctrl Pts',(-3.31631129755346,-17.7406985030951,
1298.76176470588));
#143521=CARTESIAN_POINT('Ctrl Pts',(-4.96022910773077,-17.4333970061901,
1297.26764705882));
#143522=CARTESIAN_POINT('Ctrl Pts',(-6.51968959134574,-16.8292587962898,
1295.77352941176));
#143523=CARTESIAN_POINT('Ctrl Pts',(-8.07915007496071,-16.2251205863895,
1294.27941176471));
#143524=CARTESIAN_POINT('Ctrl Pts',(-9.50104767561052,-15.3447188656481,
1292.78529411765));
#143525=CARTESIAN_POINT('Ctrl Pts',(-10.9229452762603,-14.4643171449067,
1291.29117647059));
#143526=CARTESIAN_POINT('Ctrl Pts',(-12.1588589765331,-13.3376329379985,
1289.79705882353));
#143527=CARTESIAN_POINT('Ctrl Pts',(-13.3947726768058,-12.2109487310903,
1288.30294117647));
#143528=CARTESIAN_POINT('Ctrl Pts',(-14.4026149179538,-10.8763499173728,
1286.80882352941));
#143529=CARTESIAN_POINT('Ctrl Pts',(-15.4104571591017,-9.54175110365538,
1285.31470588235));
#143530=CARTESIAN_POINT('Ctrl Pts',(-16.1559070823762,-8.04468584505497,
1283.82058823529));
#143531=CARTESIAN_POINT('Ctrl Pts',(-16.9013570056506,-6.54762058645456,
1282.32647058824));
#143532=CARTESIAN_POINT('Ctrl Pts',(-17.3590292079831,-4.93906964482095,
1280.83235294118));
#143533=CARTESIAN_POINT('Ctrl Pts',(-17.8167014103155,-3.33051870318735,
1279.33823529412));
#143534=CARTESIAN_POINT('Ctrl Pts',(-17.9710104137728,-1.66525935159368,
1277.84411764706));
#143535=CARTESIAN_POINT('Ctrl Pts',(-18.1253194172301,-1.10985572039171E-15,
1276.35));
#143536=CARTESIAN_POINT('Ctrl Pts',(-17.9710104137728,1.66525935159367,
1274.85588235294));
#143537=CARTESIAN_POINT('Ctrl Pts',(-17.8167014103155,3.33051870318735,
1273.36176470588));
#143538=CARTESIAN_POINT('Ctrl Pts',(-17.3590292079831,4.93906964482096,
1271.86764705882));
#143539=CARTESIAN_POINT('Ctrl Pts',(-16.9013570056506,6.54762058645456,
1270.37352941176));
#143540=CARTESIAN_POINT('Ctrl Pts',(-16.1559070823762,8.04468584505497,
1268.87941176471));
#143541=CARTESIAN_POINT('Ctrl Pts',(-15.4104571591017,9.54175110365538,
1267.38529411765));
#143542=CARTESIAN_POINT('Ctrl Pts',(-14.4026149179538,10.8763499173728,
1265.89117647059));
#143543=CARTESIAN_POINT('Ctrl Pts',(-13.3947726768058,12.2109487310903,
1264.39705882353));
#143544=CARTESIAN_POINT('Ctrl Pts',(-12.1588589765331,13.3376329379985,
1262.90294117647));
#143545=CARTESIAN_POINT('Ctrl Pts',(-10.9229452762603,14.4643171449067,
1261.40882352941));
#143546=CARTESIAN_POINT('Ctrl Pts',(-9.50104767561052,15.3447188656481,
1259.91470588235));
#143547=CARTESIAN_POINT('Ctrl Pts',(-8.07915007496071,16.2251205863895,
1258.42058823529));
#143548=CARTESIAN_POINT('Ctrl Pts',(-6.51968959134574,16.8292587962898,
1256.92647058824));
#143549=CARTESIAN_POINT('Ctrl Pts',(-4.96022910773078,17.4333970061901,
1255.43235294118));
#143550=CARTESIAN_POINT('Ctrl Pts',(-3.31631129755346,17.7406985030951,
1253.93823529412));
#143551=CARTESIAN_POINT('Ctrl Pts',(-1.67239348737615,18.048,1252.44411764706));
#143552=CARTESIAN_POINT('Ctrl Pts',(-2.21024254310115E-15,18.048,1250.95));
#143553=CARTESIAN_POINT('Origin',(5.37704275891775E-14,4.44089209850063E-14,
1504.8993152933));
#143554=CARTESIAN_POINT('',(5.15601850460762E-14,18.048,1149.24863058659));
#143555=CARTESIAN_POINT('',(5.15601850460762E-14,18.048,1149.35));
#143556=CARTESIAN_POINT('',(1.05330612635254E-13,18.0480000000001,1504.8993152933));
#143557=CARTESIAN_POINT('Ctrl Pts',(-2.21024254310115E-15,18.048,1250.84863058659));
#143558=CARTESIAN_POINT('Ctrl Pts',(1.67239348737616,18.048,1249.35451293953));
#143559=CARTESIAN_POINT('Ctrl Pts',(3.31631129755346,17.7406985030951,1247.86039529247));
#143560=CARTESIAN_POINT('Ctrl Pts',(4.96022910773077,17.4333970061901,1246.36627764542));
#143561=CARTESIAN_POINT('Ctrl Pts',(6.51968959134575,16.8292587962898,1244.87215999836));
#143562=CARTESIAN_POINT('Ctrl Pts',(8.07915007496071,16.2251205863895,1243.3780423513));
#143563=CARTESIAN_POINT('Ctrl Pts',(9.50104767561053,15.3447188656481,1241.88392470424));
#143564=CARTESIAN_POINT('Ctrl Pts',(10.9229452762603,14.4643171449067,1240.38980705718));
#143565=CARTESIAN_POINT('Ctrl Pts',(12.1588589765331,13.3376329379985,1238.89568941012));
#143566=CARTESIAN_POINT('Ctrl Pts',(13.3947726768058,12.2109487310903,1237.40157176306));
#143567=CARTESIAN_POINT('Ctrl Pts',(14.4026149179538,10.8763499173728,1235.907454116));
#143568=CARTESIAN_POINT('Ctrl Pts',(15.4104571591017,9.54175110365539,1234.41333646895));
#143569=CARTESIAN_POINT('Ctrl Pts',(16.1559070823762,8.04468584505496,1232.91921882189));
#143570=CARTESIAN_POINT('Ctrl Pts',(16.9013570056506,6.54762058645456,1231.42510117483));
#143571=CARTESIAN_POINT('Ctrl Pts',(17.3590292079831,4.93906964482096,1229.93098352777));
#143572=CARTESIAN_POINT('Ctrl Pts',(17.8167014103155,3.33051870318735,1228.43686588071));
#143573=CARTESIAN_POINT('Ctrl Pts',(17.9710104137728,1.66525935159367,1226.94274823365));
#143574=CARTESIAN_POINT('Ctrl Pts',(18.1253194172301,3.32956716117513E-15,
1225.44863058659));
#143575=CARTESIAN_POINT('Ctrl Pts',(17.9710104137728,-1.66525935159367,
1223.95451293953));
#143576=CARTESIAN_POINT('Ctrl Pts',(17.8167014103155,-3.33051870318736,
1222.46039529247));
#143577=CARTESIAN_POINT('Ctrl Pts',(17.3590292079831,-4.93906964482095,
1220.96627764542));
#143578=CARTESIAN_POINT('Ctrl Pts',(16.9013570056506,-6.54762058645456,
1219.47215999836));
#143579=CARTESIAN_POINT('Ctrl Pts',(16.1559070823762,-8.04468584505497,
1217.9780423513));
#143580=CARTESIAN_POINT('Ctrl Pts',(15.4104571591017,-9.54175110365538,
1216.48392470424));
#143581=CARTESIAN_POINT('Ctrl Pts',(14.4026149179538,-10.8763499173728,
1214.98980705718));
#143582=CARTESIAN_POINT('Ctrl Pts',(13.3947726768058,-12.2109487310903,
1213.49568941012));
#143583=CARTESIAN_POINT('Ctrl Pts',(12.1588589765331,-13.3376329379985,
1212.00157176306));
#143584=CARTESIAN_POINT('Ctrl Pts',(10.9229452762603,-14.4643171449067,
1210.507454116));
#143585=CARTESIAN_POINT('Ctrl Pts',(9.50104767561053,-15.3447188656481,
1209.01333646895));
#143586=CARTESIAN_POINT('Ctrl Pts',(8.07915007496071,-16.2251205863895,
1207.51921882189));
#143587=CARTESIAN_POINT('Ctrl Pts',(6.51968959134574,-16.8292587962898,
1206.02510117483));
#143588=CARTESIAN_POINT('Ctrl Pts',(4.96022910773078,-17.4333970061901,
1204.53098352777));
#143589=CARTESIAN_POINT('Ctrl Pts',(3.31631129755346,-17.7406985030951,
1203.03686588071));
#143590=CARTESIAN_POINT('Ctrl Pts',(1.67239348737615,-18.048,1201.54274823365));
#143591=CARTESIAN_POINT('Ctrl Pts',(0.,-18.048,1200.04863058659));
#143592=CARTESIAN_POINT('Ctrl Pts',(-1.67239348737615,-18.048,1198.55451293953));
#143593=CARTESIAN_POINT('Ctrl Pts',(-3.31631129755346,-17.7406985030951,
1197.06039529247));
#143594=CARTESIAN_POINT('Ctrl Pts',(-4.96022910773077,-17.4333970061901,
1195.56627764542));
#143595=CARTESIAN_POINT('Ctrl Pts',(-6.51968959134574,-16.8292587962898,
1194.07215999836));
#143596=CARTESIAN_POINT('Ctrl Pts',(-8.07915007496071,-16.2251205863895,
1192.5780423513));
#143597=CARTESIAN_POINT('Ctrl Pts',(-9.50104767561052,-15.3447188656481,
1191.08392470424));
#143598=CARTESIAN_POINT('Ctrl Pts',(-10.9229452762603,-14.4643171449067,
1189.58980705718));
#143599=CARTESIAN_POINT('Ctrl Pts',(-12.1588589765331,-13.3376329379985,
1188.09568941012));
#143600=CARTESIAN_POINT('Ctrl Pts',(-13.3947726768058,-12.2109487310903,
1186.60157176306));
#143601=CARTESIAN_POINT('Ctrl Pts',(-14.4026149179538,-10.8763499173728,
1185.107454116));
#143602=CARTESIAN_POINT('Ctrl Pts',(-15.4104571591017,-9.54175110365538,
1183.61333646895));
#143603=CARTESIAN_POINT('Ctrl Pts',(-16.1559070823762,-8.04468584505497,
1182.11921882189));
#143604=CARTESIAN_POINT('Ctrl Pts',(-16.9013570056506,-6.54762058645456,
1180.62510117483));
#143605=CARTESIAN_POINT('Ctrl Pts',(-17.3590292079831,-4.93906964482095,
1179.13098352777));
#143606=CARTESIAN_POINT('Ctrl Pts',(-17.8167014103155,-3.33051870318735,
1177.63686588071));
#143607=CARTESIAN_POINT('Ctrl Pts',(-17.9710104137728,-1.66525935159368,
1176.14274823365));
#143608=CARTESIAN_POINT('Ctrl Pts',(-18.1253194172301,-1.10985572039171E-15,
1174.64863058659));
#143609=CARTESIAN_POINT('Ctrl Pts',(-17.9710104137728,1.66525935159367,
1173.15451293953));
#143610=CARTESIAN_POINT('Ctrl Pts',(-17.8167014103155,3.33051870318735,
1171.66039529247));
#143611=CARTESIAN_POINT('Ctrl Pts',(-17.3590292079831,4.93906964482096,
1170.16627764542));
#143612=CARTESIAN_POINT('Ctrl Pts',(-16.9013570056506,6.54762058645456,
1168.67215999836));
#143613=CARTESIAN_POINT('Ctrl Pts',(-16.1559070823762,8.04468584505497,
1167.1780423513));
#143614=CARTESIAN_POINT('Ctrl Pts',(-15.4104571591017,9.54175110365538,
1165.68392470424));
#143615=CARTESIAN_POINT('Ctrl Pts',(-14.4026149179538,10.8763499173728,
1164.18980705718));
#143616=CARTESIAN_POINT('Ctrl Pts',(-13.3947726768058,12.2109487310903,
1162.69568941012));
#143617=CARTESIAN_POINT('Ctrl Pts',(-12.1588589765331,13.3376329379985,
1161.20157176306));
#143618=CARTESIAN_POINT('Ctrl Pts',(-10.9229452762603,14.4643171449067,
1159.707454116));
#143619=CARTESIAN_POINT('Ctrl Pts',(-9.50104767561052,15.3447188656481,
1158.21333646895));
#143620=CARTESIAN_POINT('Ctrl Pts',(-8.07915007496071,16.2251205863895,
1156.71921882189));
#143621=CARTESIAN_POINT('Ctrl Pts',(-6.51968959134574,16.8292587962898,
1155.22510117483));
#143622=CARTESIAN_POINT('Ctrl Pts',(-4.96022910773078,17.4333970061901,
1153.73098352777));
#143623=CARTESIAN_POINT('Ctrl Pts',(-3.31631129755346,17.7406985030951,
1152.23686588071));
#143624=CARTESIAN_POINT('Ctrl Pts',(-1.67239348737615,18.048,1150.74274823365));
#143625=CARTESIAN_POINT('Ctrl Pts',(-2.21024254310115E-15,18.048,1149.24863058659));
#143626=CARTESIAN_POINT('Ctrl Pts',(-2.21024254310115E-15,18.048,1250.95));
#143627=CARTESIAN_POINT('Ctrl Pts',(1.67239348737616,18.048,1249.45588235294));
#143628=CARTESIAN_POINT('Ctrl Pts',(3.31631129755346,17.7406985030951,1247.96176470588));
#143629=CARTESIAN_POINT('Ctrl Pts',(4.96022910773077,17.4333970061901,1246.46764705882));
#143630=CARTESIAN_POINT('Ctrl Pts',(6.51968959134575,16.8292587962898,1244.97352941176));
#143631=CARTESIAN_POINT('Ctrl Pts',(8.07915007496071,16.2251205863895,1243.47941176471));
#143632=CARTESIAN_POINT('Ctrl Pts',(9.50104767561053,15.3447188656481,1241.98529411765));
#143633=CARTESIAN_POINT('Ctrl Pts',(10.9229452762603,14.4643171449067,1240.49117647059));
#143634=CARTESIAN_POINT('Ctrl Pts',(12.1588589765331,13.3376329379985,1238.99705882353));
#143635=CARTESIAN_POINT('Ctrl Pts',(13.3947726768058,12.2109487310903,1237.50294117647));
#143636=CARTESIAN_POINT('Ctrl Pts',(14.4026149179538,10.8763499173728,1236.00882352941));
#143637=CARTESIAN_POINT('Ctrl Pts',(15.4104571591017,9.54175110365539,1234.51470588235));
#143638=CARTESIAN_POINT('Ctrl Pts',(16.1559070823762,8.04468584505496,1233.02058823529));
#143639=CARTESIAN_POINT('Ctrl Pts',(16.9013570056506,6.54762058645456,1231.52647058824));
#143640=CARTESIAN_POINT('Ctrl Pts',(17.3590292079831,4.93906964482096,1230.03235294118));
#143641=CARTESIAN_POINT('Ctrl Pts',(17.8167014103155,3.33051870318735,1228.53823529412));
#143642=CARTESIAN_POINT('Ctrl Pts',(17.9710104137728,1.66525935159367,1227.04411764706));
#143643=CARTESIAN_POINT('Ctrl Pts',(18.1253194172301,3.32956716117513E-15,
1225.55));
#143644=CARTESIAN_POINT('Ctrl Pts',(17.9710104137728,-1.66525935159367,
1224.05588235294));
#143645=CARTESIAN_POINT('Ctrl Pts',(17.8167014103155,-3.33051870318736,
1222.56176470588));
#143646=CARTESIAN_POINT('Ctrl Pts',(17.3590292079831,-4.93906964482095,
1221.06764705882));
#143647=CARTESIAN_POINT('Ctrl Pts',(16.9013570056506,-6.54762058645456,
1219.57352941176));
#143648=CARTESIAN_POINT('Ctrl Pts',(16.1559070823762,-8.04468584505497,
1218.07941176471));
#143649=CARTESIAN_POINT('Ctrl Pts',(15.4104571591017,-9.54175110365538,
1216.58529411765));
#143650=CARTESIAN_POINT('Ctrl Pts',(14.4026149179538,-10.8763499173728,
1215.09117647059));
#143651=CARTESIAN_POINT('Ctrl Pts',(13.3947726768058,-12.2109487310903,
1213.59705882353));
#143652=CARTESIAN_POINT('Ctrl Pts',(12.1588589765331,-13.3376329379985,
1212.10294117647));
#143653=CARTESIAN_POINT('Ctrl Pts',(10.9229452762603,-14.4643171449067,
1210.60882352941));
#143654=CARTESIAN_POINT('Ctrl Pts',(9.50104767561053,-15.3447188656481,
1209.11470588235));
#143655=CARTESIAN_POINT('Ctrl Pts',(8.07915007496071,-16.2251205863895,
1207.62058823529));
#143656=CARTESIAN_POINT('Ctrl Pts',(6.51968959134574,-16.8292587962898,
1206.12647058824));
#143657=CARTESIAN_POINT('Ctrl Pts',(4.96022910773078,-17.4333970061901,
1204.63235294118));
#143658=CARTESIAN_POINT('Ctrl Pts',(3.31631129755346,-17.7406985030951,
1203.13823529412));
#143659=CARTESIAN_POINT('Ctrl Pts',(1.67239348737615,-18.048,1201.64411764706));
#143660=CARTESIAN_POINT('Ctrl Pts',(0.,-18.048,1200.15));
#143661=CARTESIAN_POINT('Ctrl Pts',(-1.67239348737615,-18.048,1198.65588235294));
#143662=CARTESIAN_POINT('Ctrl Pts',(-3.31631129755346,-17.7406985030951,
1197.16176470588));
#143663=CARTESIAN_POINT('Ctrl Pts',(-4.96022910773077,-17.4333970061901,
1195.66764705882));
#143664=CARTESIAN_POINT('Ctrl Pts',(-6.51968959134574,-16.8292587962898,
1194.17352941176));
#143665=CARTESIAN_POINT('Ctrl Pts',(-8.07915007496071,-16.2251205863895,
1192.67941176471));
#143666=CARTESIAN_POINT('Ctrl Pts',(-9.50104767561052,-15.3447188656481,
1191.18529411765));
#143667=CARTESIAN_POINT('Ctrl Pts',(-10.9229452762603,-14.4643171449067,
1189.69117647059));
#143668=CARTESIAN_POINT('Ctrl Pts',(-12.1588589765331,-13.3376329379985,
1188.19705882353));
#143669=CARTESIAN_POINT('Ctrl Pts',(-13.3947726768058,-12.2109487310903,
1186.70294117647));
#143670=CARTESIAN_POINT('Ctrl Pts',(-14.4026149179538,-10.8763499173728,
1185.20882352941));
#143671=CARTESIAN_POINT('Ctrl Pts',(-15.4104571591017,-9.54175110365538,
1183.71470588235));
#143672=CARTESIAN_POINT('Ctrl Pts',(-16.1559070823762,-8.04468584505497,
1182.22058823529));
#143673=CARTESIAN_POINT('Ctrl Pts',(-16.9013570056506,-6.54762058645456,
1180.72647058824));
#143674=CARTESIAN_POINT('Ctrl Pts',(-17.3590292079831,-4.93906964482095,
1179.23235294118));
#143675=CARTESIAN_POINT('Ctrl Pts',(-17.8167014103155,-3.33051870318735,
1177.73823529412));
#143676=CARTESIAN_POINT('Ctrl Pts',(-17.9710104137728,-1.66525935159368,
1176.24411764706));
#143677=CARTESIAN_POINT('Ctrl Pts',(-18.1253194172301,-1.10985572039171E-15,
1174.75));
#143678=CARTESIAN_POINT('Ctrl Pts',(-17.9710104137728,1.66525935159367,
1173.25588235294));
#143679=CARTESIAN_POINT('Ctrl Pts',(-17.8167014103155,3.33051870318735,
1171.76176470588));
#143680=CARTESIAN_POINT('Ctrl Pts',(-17.3590292079831,4.93906964482096,
1170.26764705882));
#143681=CARTESIAN_POINT('Ctrl Pts',(-16.9013570056506,6.54762058645456,
1168.77352941176));
#143682=CARTESIAN_POINT('Ctrl Pts',(-16.1559070823762,8.04468584505497,
1167.27941176471));
#143683=CARTESIAN_POINT('Ctrl Pts',(-15.4104571591017,9.54175110365538,
1165.78529411765));
#143684=CARTESIAN_POINT('Ctrl Pts',(-14.4026149179538,10.8763499173728,
1164.29117647059));
#143685=CARTESIAN_POINT('Ctrl Pts',(-13.3947726768058,12.2109487310903,
1162.79705882353));
#143686=CARTESIAN_POINT('Ctrl Pts',(-12.1588589765331,13.3376329379985,
1161.30294117647));
#143687=CARTESIAN_POINT('Ctrl Pts',(-10.9229452762603,14.4643171449067,
1159.80882352941));
#143688=CARTESIAN_POINT('Ctrl Pts',(-9.50104767561052,15.3447188656481,
1158.31470588235));
#143689=CARTESIAN_POINT('Ctrl Pts',(-8.07915007496071,16.2251205863895,
1156.82058823529));
#143690=CARTESIAN_POINT('Ctrl Pts',(-6.51968959134574,16.8292587962898,
1155.32647058824));
#143691=CARTESIAN_POINT('Ctrl Pts',(-4.96022910773078,17.4333970061901,
1153.83235294118));
#143692=CARTESIAN_POINT('Ctrl Pts',(-3.31631129755346,17.7406985030951,
1152.33823529412));
#143693=CARTESIAN_POINT('Ctrl Pts',(-1.67239348737615,18.048,1150.84411764706));
#143694=CARTESIAN_POINT('Ctrl Pts',(-2.21024254310115E-15,18.048,1149.35));
#143695=CARTESIAN_POINT('Origin',(5.37704275891775E-14,4.44089209850063E-14,
1504.8993152933));
#143696=CARTESIAN_POINT('',(5.15601850460762E-14,18.048,1047.64863058659));
#143697=CARTESIAN_POINT('',(5.15601850460762E-14,18.048,1047.75));
#143698=CARTESIAN_POINT('',(1.05330612635254E-13,18.0480000000001,1504.8993152933));
#143699=CARTESIAN_POINT('Ctrl Pts',(-2.21024254310115E-15,18.048,1149.24863058659));
#143700=CARTESIAN_POINT('Ctrl Pts',(1.67239348737616,18.048,1147.75451293953));
#143701=CARTESIAN_POINT('Ctrl Pts',(3.31631129755346,17.7406985030951,1146.26039529247));
#143702=CARTESIAN_POINT('Ctrl Pts',(4.96022910773077,17.4333970061901,1144.76627764542));
#143703=CARTESIAN_POINT('Ctrl Pts',(6.51968959134575,16.8292587962898,1143.27215999836));
#143704=CARTESIAN_POINT('Ctrl Pts',(8.07915007496071,16.2251205863895,1141.7780423513));
#143705=CARTESIAN_POINT('Ctrl Pts',(9.50104767561053,15.3447188656481,1140.28392470424));
#143706=CARTESIAN_POINT('Ctrl Pts',(10.9229452762603,14.4643171449067,1138.78980705718));
#143707=CARTESIAN_POINT('Ctrl Pts',(12.1588589765331,13.3376329379985,1137.29568941012));
#143708=CARTESIAN_POINT('Ctrl Pts',(13.3947726768058,12.2109487310903,1135.80157176306));
#143709=CARTESIAN_POINT('Ctrl Pts',(14.4026149179538,10.8763499173728,1134.307454116));
#143710=CARTESIAN_POINT('Ctrl Pts',(15.4104571591017,9.54175110365539,1132.81333646895));
#143711=CARTESIAN_POINT('Ctrl Pts',(16.1559070823762,8.04468584505496,1131.31921882189));
#143712=CARTESIAN_POINT('Ctrl Pts',(16.9013570056506,6.54762058645456,1129.82510117483));
#143713=CARTESIAN_POINT('Ctrl Pts',(17.3590292079831,4.93906964482096,1128.33098352777));
#143714=CARTESIAN_POINT('Ctrl Pts',(17.8167014103155,3.33051870318735,1126.83686588071));
#143715=CARTESIAN_POINT('Ctrl Pts',(17.9710104137728,1.66525935159367,1125.34274823365));
#143716=CARTESIAN_POINT('Ctrl Pts',(18.1253194172301,3.32956716117513E-15,
1123.84863058659));
#143717=CARTESIAN_POINT('Ctrl Pts',(17.9710104137728,-1.66525935159367,
1122.35451293953));
#143718=CARTESIAN_POINT('Ctrl Pts',(17.8167014103155,-3.33051870318736,
1120.86039529247));
#143719=CARTESIAN_POINT('Ctrl Pts',(17.3590292079831,-4.93906964482095,
1119.36627764542));
#143720=CARTESIAN_POINT('Ctrl Pts',(16.9013570056506,-6.54762058645456,
1117.87215999836));
#143721=CARTESIAN_POINT('Ctrl Pts',(16.1559070823762,-8.04468584505497,
1116.3780423513));
#143722=CARTESIAN_POINT('Ctrl Pts',(15.4104571591017,-9.54175110365538,
1114.88392470424));
#143723=CARTESIAN_POINT('Ctrl Pts',(14.4026149179538,-10.8763499173728,
1113.38980705718));
#143724=CARTESIAN_POINT('Ctrl Pts',(13.3947726768058,-12.2109487310903,
1111.89568941012));
#143725=CARTESIAN_POINT('Ctrl Pts',(12.1588589765331,-13.3376329379985,
1110.40157176306));
#143726=CARTESIAN_POINT('Ctrl Pts',(10.9229452762603,-14.4643171449067,
1108.907454116));
#143727=CARTESIAN_POINT('Ctrl Pts',(9.50104767561053,-15.3447188656481,
1107.41333646895));
#143728=CARTESIAN_POINT('Ctrl Pts',(8.07915007496071,-16.2251205863895,
1105.91921882189));
#143729=CARTESIAN_POINT('Ctrl Pts',(6.51968959134574,-16.8292587962898,
1104.42510117483));
#143730=CARTESIAN_POINT('Ctrl Pts',(4.96022910773078,-17.4333970061901,
1102.93098352777));
#143731=CARTESIAN_POINT('Ctrl Pts',(3.31631129755346,-17.7406985030951,
1101.43686588071));
#143732=CARTESIAN_POINT('Ctrl Pts',(1.67239348737615,-18.048,1099.94274823365));
#143733=CARTESIAN_POINT('Ctrl Pts',(0.,-18.048,1098.44863058659));
#143734=CARTESIAN_POINT('Ctrl Pts',(-1.67239348737615,-18.048,1096.95451293953));
#143735=CARTESIAN_POINT('Ctrl Pts',(-3.31631129755346,-17.7406985030951,
1095.46039529247));
#143736=CARTESIAN_POINT('Ctrl Pts',(-4.96022910773077,-17.4333970061901,
1093.96627764542));
#143737=CARTESIAN_POINT('Ctrl Pts',(-6.51968959134574,-16.8292587962898,
1092.47215999836));
#143738=CARTESIAN_POINT('Ctrl Pts',(-8.07915007496071,-16.2251205863895,
1090.9780423513));
#143739=CARTESIAN_POINT('Ctrl Pts',(-9.50104767561052,-15.3447188656481,
1089.48392470424));
#143740=CARTESIAN_POINT('Ctrl Pts',(-10.9229452762603,-14.4643171449067,
1087.98980705718));
#143741=CARTESIAN_POINT('Ctrl Pts',(-12.1588589765331,-13.3376329379985,
1086.49568941012));
#143742=CARTESIAN_POINT('Ctrl Pts',(-13.3947726768058,-12.2109487310903,
1085.00157176306));
#143743=CARTESIAN_POINT('Ctrl Pts',(-14.4026149179538,-10.8763499173728,
1083.507454116));
#143744=CARTESIAN_POINT('Ctrl Pts',(-15.4104571591017,-9.54175110365538,
1082.01333646895));
#143745=CARTESIAN_POINT('Ctrl Pts',(-16.1559070823762,-8.04468584505497,
1080.51921882189));
#143746=CARTESIAN_POINT('Ctrl Pts',(-16.9013570056506,-6.54762058645456,
1079.02510117483));
#143747=CARTESIAN_POINT('Ctrl Pts',(-17.3590292079831,-4.93906964482095,
1077.53098352777));
#143748=CARTESIAN_POINT('Ctrl Pts',(-17.8167014103155,-3.33051870318735,
1076.03686588071));
#143749=CARTESIAN_POINT('Ctrl Pts',(-17.9710104137728,-1.66525935159368,
1074.54274823365));
#143750=CARTESIAN_POINT('Ctrl Pts',(-18.1253194172301,-1.10985572039171E-15,
1073.04863058659));
#143751=CARTESIAN_POINT('Ctrl Pts',(-17.9710104137728,1.66525935159367,
1071.55451293953));
#143752=CARTESIAN_POINT('Ctrl Pts',(-17.8167014103155,3.33051870318735,
1070.06039529247));
#143753=CARTESIAN_POINT('Ctrl Pts',(-17.3590292079831,4.93906964482096,
1068.56627764542));
#143754=CARTESIAN_POINT('Ctrl Pts',(-16.9013570056506,6.54762058645456,
1067.07215999836));
#143755=CARTESIAN_POINT('Ctrl Pts',(-16.1559070823762,8.04468584505497,
1065.5780423513));
#143756=CARTESIAN_POINT('Ctrl Pts',(-15.4104571591017,9.54175110365538,
1064.08392470424));
#143757=CARTESIAN_POINT('Ctrl Pts',(-14.4026149179538,10.8763499173728,
1062.58980705718));
#143758=CARTESIAN_POINT('Ctrl Pts',(-13.3947726768058,12.2109487310903,
1061.09568941012));
#143759=CARTESIAN_POINT('Ctrl Pts',(-12.1588589765331,13.3376329379985,
1059.60157176306));
#143760=CARTESIAN_POINT('Ctrl Pts',(-10.9229452762603,14.4643171449067,
1058.107454116));
#143761=CARTESIAN_POINT('Ctrl Pts',(-9.50104767561052,15.3447188656481,
1056.61333646895));
#143762=CARTESIAN_POINT('Ctrl Pts',(-8.07915007496071,16.2251205863895,
1055.11921882189));
#143763=CARTESIAN_POINT('Ctrl Pts',(-6.51968959134574,16.8292587962898,
1053.62510117483));
#143764=CARTESIAN_POINT('Ctrl Pts',(-4.96022910773078,17.4333970061901,
1052.13098352777));
#143765=CARTESIAN_POINT('Ctrl Pts',(-3.31631129755346,17.7406985030951,
1050.63686588071));
#143766=CARTESIAN_POINT('Ctrl Pts',(-1.67239348737615,18.048,1049.14274823365));
#143767=CARTESIAN_POINT('Ctrl Pts',(-2.21024254310115E-15,18.048,1047.64863058659));
#143768=CARTESIAN_POINT('Ctrl Pts',(-2.21024254310115E-15,18.048,1149.35));
#143769=CARTESIAN_POINT('Ctrl Pts',(1.67239348737616,18.048,1147.85588235294));
#143770=CARTESIAN_POINT('Ctrl Pts',(3.31631129755346,17.7406985030951,1146.36176470588));
#143771=CARTESIAN_POINT('Ctrl Pts',(4.96022910773077,17.4333970061901,1144.86764705882));
#143772=CARTESIAN_POINT('Ctrl Pts',(6.51968959134575,16.8292587962898,1143.37352941176));
#143773=CARTESIAN_POINT('Ctrl Pts',(8.07915007496071,16.2251205863895,1141.87941176471));
#143774=CARTESIAN_POINT('Ctrl Pts',(9.50104767561053,15.3447188656481,1140.38529411765));
#143775=CARTESIAN_POINT('Ctrl Pts',(10.9229452762603,14.4643171449067,1138.89117647059));
#143776=CARTESIAN_POINT('Ctrl Pts',(12.1588589765331,13.3376329379985,1137.39705882353));
#143777=CARTESIAN_POINT('Ctrl Pts',(13.3947726768058,12.2109487310903,1135.90294117647));
#143778=CARTESIAN_POINT('Ctrl Pts',(14.4026149179538,10.8763499173728,1134.40882352941));
#143779=CARTESIAN_POINT('Ctrl Pts',(15.4104571591017,9.54175110365539,1132.91470588235));
#143780=CARTESIAN_POINT('Ctrl Pts',(16.1559070823762,8.04468584505496,1131.42058823529));
#143781=CARTESIAN_POINT('Ctrl Pts',(16.9013570056506,6.54762058645456,1129.92647058824));
#143782=CARTESIAN_POINT('Ctrl Pts',(17.3590292079831,4.93906964482096,1128.43235294118));
#143783=CARTESIAN_POINT('Ctrl Pts',(17.8167014103155,3.33051870318735,1126.93823529412));
#143784=CARTESIAN_POINT('Ctrl Pts',(17.9710104137728,1.66525935159367,1125.44411764706));
#143785=CARTESIAN_POINT('Ctrl Pts',(18.1253194172301,3.32956716117513E-15,
1123.95));
#143786=CARTESIAN_POINT('Ctrl Pts',(17.9710104137728,-1.66525935159367,
1122.45588235294));
#143787=CARTESIAN_POINT('Ctrl Pts',(17.8167014103155,-3.33051870318736,
1120.96176470588));
#143788=CARTESIAN_POINT('Ctrl Pts',(17.3590292079831,-4.93906964482095,
1119.46764705882));
#143789=CARTESIAN_POINT('Ctrl Pts',(16.9013570056506,-6.54762058645456,
1117.97352941176));
#143790=CARTESIAN_POINT('Ctrl Pts',(16.1559070823762,-8.04468584505497,
1116.47941176471));
#143791=CARTESIAN_POINT('Ctrl Pts',(15.4104571591017,-9.54175110365538,
1114.98529411765));
#143792=CARTESIAN_POINT('Ctrl Pts',(14.4026149179538,-10.8763499173728,
1113.49117647059));
#143793=CARTESIAN_POINT('Ctrl Pts',(13.3947726768058,-12.2109487310903,
1111.99705882353));
#143794=CARTESIAN_POINT('Ctrl Pts',(12.1588589765331,-13.3376329379985,
1110.50294117647));
#143795=CARTESIAN_POINT('Ctrl Pts',(10.9229452762603,-14.4643171449067,
1109.00882352941));
#143796=CARTESIAN_POINT('Ctrl Pts',(9.50104767561053,-15.3447188656481,
1107.51470588235));
#143797=CARTESIAN_POINT('Ctrl Pts',(8.07915007496071,-16.2251205863895,
1106.02058823529));
#143798=CARTESIAN_POINT('Ctrl Pts',(6.51968959134574,-16.8292587962898,
1104.52647058824));
#143799=CARTESIAN_POINT('Ctrl Pts',(4.96022910773078,-17.4333970061901,
1103.03235294118));
#143800=CARTESIAN_POINT('Ctrl Pts',(3.31631129755346,-17.7406985030951,
1101.53823529412));
#143801=CARTESIAN_POINT('Ctrl Pts',(1.67239348737615,-18.048,1100.04411764706));
#143802=CARTESIAN_POINT('Ctrl Pts',(0.,-18.048,1098.55));
#143803=CARTESIAN_POINT('Ctrl Pts',(-1.67239348737615,-18.048,1097.05588235294));
#143804=CARTESIAN_POINT('Ctrl Pts',(-3.31631129755346,-17.7406985030951,
1095.56176470588));
#143805=CARTESIAN_POINT('Ctrl Pts',(-4.96022910773077,-17.4333970061901,
1094.06764705882));
#143806=CARTESIAN_POINT('Ctrl Pts',(-6.51968959134574,-16.8292587962898,
1092.57352941176));
#143807=CARTESIAN_POINT('Ctrl Pts',(-8.07915007496071,-16.2251205863895,
1091.07941176471));
#143808=CARTESIAN_POINT('Ctrl Pts',(-9.50104767561052,-15.3447188656481,
1089.58529411765));
#143809=CARTESIAN_POINT('Ctrl Pts',(-10.9229452762603,-14.4643171449067,
1088.09117647059));
#143810=CARTESIAN_POINT('Ctrl Pts',(-12.1588589765331,-13.3376329379985,
1086.59705882353));
#143811=CARTESIAN_POINT('Ctrl Pts',(-13.3947726768058,-12.2109487310903,
1085.10294117647));
#143812=CARTESIAN_POINT('Ctrl Pts',(-14.4026149179538,-10.8763499173728,
1083.60882352941));
#143813=CARTESIAN_POINT('Ctrl Pts',(-15.4104571591017,-9.54175110365538,
1082.11470588235));
#143814=CARTESIAN_POINT('Ctrl Pts',(-16.1559070823762,-8.04468584505497,
1080.62058823529));
#143815=CARTESIAN_POINT('Ctrl Pts',(-16.9013570056506,-6.54762058645456,
1079.12647058824));
#143816=CARTESIAN_POINT('Ctrl Pts',(-17.3590292079831,-4.93906964482095,
1077.63235294118));
#143817=CARTESIAN_POINT('Ctrl Pts',(-17.8167014103155,-3.33051870318735,
1076.13823529412));
#143818=CARTESIAN_POINT('Ctrl Pts',(-17.9710104137728,-1.66525935159368,
1074.64411764706));
#143819=CARTESIAN_POINT('Ctrl Pts',(-18.1253194172301,-1.10985572039171E-15,
1073.15));
#143820=CARTESIAN_POINT('Ctrl Pts',(-17.9710104137728,1.66525935159367,
1071.65588235294));
#143821=CARTESIAN_POINT('Ctrl Pts',(-17.8167014103155,3.33051870318735,
1070.16176470588));
#143822=CARTESIAN_POINT('Ctrl Pts',(-17.3590292079831,4.93906964482096,
1068.66764705882));
#143823=CARTESIAN_POINT('Ctrl Pts',(-16.9013570056506,6.54762058645456,
1067.17352941176));
#143824=CARTESIAN_POINT('Ctrl Pts',(-16.1559070823762,8.04468584505497,
1065.67941176471));
#143825=CARTESIAN_POINT('Ctrl Pts',(-15.4104571591017,9.54175110365538,
1064.18529411765));
#143826=CARTESIAN_POINT('Ctrl Pts',(-14.4026149179538,10.8763499173728,
1062.69117647059));
#143827=CARTESIAN_POINT('Ctrl Pts',(-13.3947726768058,12.2109487310903,
1061.19705882353));
#143828=CARTESIAN_POINT('Ctrl Pts',(-12.1588589765331,13.3376329379985,
1059.70294117647));
#143829=CARTESIAN_POINT('Ctrl Pts',(-10.9229452762603,14.4643171449067,
1058.20882352941));
#143830=CARTESIAN_POINT('Ctrl Pts',(-9.50104767561052,15.3447188656481,
1056.71470588235));
#143831=CARTESIAN_POINT('Ctrl Pts',(-8.07915007496071,16.2251205863895,
1055.22058823529));
#143832=CARTESIAN_POINT('Ctrl Pts',(-6.51968959134574,16.8292587962898,
1053.72647058824));
#143833=CARTESIAN_POINT('Ctrl Pts',(-4.96022910773078,17.4333970061901,
1052.23235294118));
#143834=CARTESIAN_POINT('Ctrl Pts',(-3.31631129755346,17.7406985030951,
1050.73823529412));
#143835=CARTESIAN_POINT('Ctrl Pts',(-1.67239348737615,18.048,1049.24411764706));
#143836=CARTESIAN_POINT('Ctrl Pts',(-2.21024254310115E-15,18.048,1047.75));
#143837=CARTESIAN_POINT('Origin',(5.37704275891775E-14,4.44089209850063E-14,
1504.8993152933));
#143838=CARTESIAN_POINT('',(5.15601850460762E-14,18.048,946.048630586592));
#143839=CARTESIAN_POINT('',(5.15601850460762E-14,18.048,946.15));
#143840=CARTESIAN_POINT('',(1.05330612635254E-13,18.0480000000001,1504.8993152933));
#143841=CARTESIAN_POINT('Ctrl Pts',(-2.21024254310115E-15,18.048,1047.64863058659));
#143842=CARTESIAN_POINT('Ctrl Pts',(1.67239348737616,18.048,1046.15451293953));
#143843=CARTESIAN_POINT('Ctrl Pts',(3.31631129755346,17.7406985030951,1044.66039529247));
#143844=CARTESIAN_POINT('Ctrl Pts',(4.96022910773077,17.4333970061901,1043.16627764542));
#143845=CARTESIAN_POINT('Ctrl Pts',(6.51968959134575,16.8292587962898,1041.67215999836));
#143846=CARTESIAN_POINT('Ctrl Pts',(8.07915007496071,16.2251205863895,1040.1780423513));
#143847=CARTESIAN_POINT('Ctrl Pts',(9.50104767561053,15.3447188656481,1038.68392470424));
#143848=CARTESIAN_POINT('Ctrl Pts',(10.9229452762603,14.4643171449067,1037.18980705718));
#143849=CARTESIAN_POINT('Ctrl Pts',(12.1588589765331,13.3376329379985,1035.69568941012));
#143850=CARTESIAN_POINT('Ctrl Pts',(13.3947726768058,12.2109487310903,1034.20157176306));
#143851=CARTESIAN_POINT('Ctrl Pts',(14.4026149179538,10.8763499173728,1032.707454116));
#143852=CARTESIAN_POINT('Ctrl Pts',(15.4104571591017,9.54175110365539,1031.21333646895));
#143853=CARTESIAN_POINT('Ctrl Pts',(16.1559070823762,8.04468584505496,1029.71921882189));
#143854=CARTESIAN_POINT('Ctrl Pts',(16.9013570056506,6.54762058645456,1028.22510117483));
#143855=CARTESIAN_POINT('Ctrl Pts',(17.3590292079831,4.93906964482096,1026.73098352777));
#143856=CARTESIAN_POINT('Ctrl Pts',(17.8167014103155,3.33051870318735,1025.23686588071));
#143857=CARTESIAN_POINT('Ctrl Pts',(17.9710104137728,1.66525935159367,1023.74274823365));
#143858=CARTESIAN_POINT('Ctrl Pts',(18.1253194172301,3.32956716117513E-15,
1022.24863058659));
#143859=CARTESIAN_POINT('Ctrl Pts',(17.9710104137728,-1.66525935159367,
1020.75451293953));
#143860=CARTESIAN_POINT('Ctrl Pts',(17.8167014103155,-3.33051870318736,
1019.26039529247));
#143861=CARTESIAN_POINT('Ctrl Pts',(17.3590292079831,-4.93906964482095,
1017.76627764542));
#143862=CARTESIAN_POINT('Ctrl Pts',(16.9013570056506,-6.54762058645456,
1016.27215999836));
#143863=CARTESIAN_POINT('Ctrl Pts',(16.1559070823762,-8.04468584505497,
1014.7780423513));
#143864=CARTESIAN_POINT('Ctrl Pts',(15.4104571591017,-9.54175110365538,
1013.28392470424));
#143865=CARTESIAN_POINT('Ctrl Pts',(14.4026149179538,-10.8763499173728,
1011.78980705718));
#143866=CARTESIAN_POINT('Ctrl Pts',(13.3947726768058,-12.2109487310903,
1010.29568941012));
#143867=CARTESIAN_POINT('Ctrl Pts',(12.1588589765331,-13.3376329379985,
1008.80157176306));
#143868=CARTESIAN_POINT('Ctrl Pts',(10.9229452762603,-14.4643171449067,
1007.307454116));
#143869=CARTESIAN_POINT('Ctrl Pts',(9.50104767561053,-15.3447188656481,
1005.81333646895));
#143870=CARTESIAN_POINT('Ctrl Pts',(8.07915007496071,-16.2251205863895,
1004.31921882189));
#143871=CARTESIAN_POINT('Ctrl Pts',(6.51968959134574,-16.8292587962898,
1002.82510117483));
#143872=CARTESIAN_POINT('Ctrl Pts',(4.96022910773078,-17.4333970061901,
1001.33098352777));
#143873=CARTESIAN_POINT('Ctrl Pts',(3.31631129755346,-17.7406985030951,
999.83686588071));
#143874=CARTESIAN_POINT('Ctrl Pts',(1.67239348737615,-18.048,998.342748233651));
#143875=CARTESIAN_POINT('Ctrl Pts',(0.,-18.048,996.848630586592));
#143876=CARTESIAN_POINT('Ctrl Pts',(-1.67239348737615,-18.048,995.354512939534));
#143877=CARTESIAN_POINT('Ctrl Pts',(-3.31631129755346,-17.7406985030951,
993.860395292475));
#143878=CARTESIAN_POINT('Ctrl Pts',(-4.96022910773077,-17.4333970061901,
992.366277645416));
#143879=CARTESIAN_POINT('Ctrl Pts',(-6.51968959134574,-16.8292587962898,
990.872159998357));
#143880=CARTESIAN_POINT('Ctrl Pts',(-8.07915007496071,-16.2251205863895,
989.378042351298));
#143881=CARTESIAN_POINT('Ctrl Pts',(-9.50104767561052,-15.3447188656481,
987.883924704239));
#143882=CARTESIAN_POINT('Ctrl Pts',(-10.9229452762603,-14.4643171449067,
986.389807057181));
#143883=CARTESIAN_POINT('Ctrl Pts',(-12.1588589765331,-13.3376329379985,
984.895689410122));
#143884=CARTESIAN_POINT('Ctrl Pts',(-13.3947726768058,-12.2109487310903,
983.401571763063));
#143885=CARTESIAN_POINT('Ctrl Pts',(-14.4026149179538,-10.8763499173728,
981.907454116004));
#143886=CARTESIAN_POINT('Ctrl Pts',(-15.4104571591017,-9.54175110365538,
980.413336468945));
#143887=CARTESIAN_POINT('Ctrl Pts',(-16.1559070823762,-8.04468584505497,
978.919218821886));
#143888=CARTESIAN_POINT('Ctrl Pts',(-16.9013570056506,-6.54762058645456,
977.425101174828));
#143889=CARTESIAN_POINT('Ctrl Pts',(-17.3590292079831,-4.93906964482095,
975.930983527769));
#143890=CARTESIAN_POINT('Ctrl Pts',(-17.8167014103155,-3.33051870318735,
974.43686588071));
#143891=CARTESIAN_POINT('Ctrl Pts',(-17.9710104137728,-1.66525935159368,
972.942748233651));
#143892=CARTESIAN_POINT('Ctrl Pts',(-18.1253194172301,-1.10985572039171E-15,
971.448630586592));
#143893=CARTESIAN_POINT('Ctrl Pts',(-17.9710104137728,1.66525935159367,
969.954512939534));
#143894=CARTESIAN_POINT('Ctrl Pts',(-17.8167014103155,3.33051870318735,
968.460395292475));
#143895=CARTESIAN_POINT('Ctrl Pts',(-17.3590292079831,4.93906964482096,
966.966277645416));
#143896=CARTESIAN_POINT('Ctrl Pts',(-16.9013570056506,6.54762058645456,
965.472159998357));
#143897=CARTESIAN_POINT('Ctrl Pts',(-16.1559070823762,8.04468584505497,
963.978042351298));
#143898=CARTESIAN_POINT('Ctrl Pts',(-15.4104571591017,9.54175110365538,
962.483924704239));
#143899=CARTESIAN_POINT('Ctrl Pts',(-14.4026149179538,10.8763499173728,
960.989807057181));
#143900=CARTESIAN_POINT('Ctrl Pts',(-13.3947726768058,12.2109487310903,
959.495689410122));
#143901=CARTESIAN_POINT('Ctrl Pts',(-12.1588589765331,13.3376329379985,
958.001571763063));
#143902=CARTESIAN_POINT('Ctrl Pts',(-10.9229452762603,14.4643171449067,
956.507454116004));
#143903=CARTESIAN_POINT('Ctrl Pts',(-9.50104767561052,15.3447188656481,
955.013336468945));
#143904=CARTESIAN_POINT('Ctrl Pts',(-8.07915007496071,16.2251205863895,
953.519218821887));
#143905=CARTESIAN_POINT('Ctrl Pts',(-6.51968959134574,16.8292587962898,
952.025101174828));
#143906=CARTESIAN_POINT('Ctrl Pts',(-4.96022910773078,17.4333970061901,
950.530983527769));
#143907=CARTESIAN_POINT('Ctrl Pts',(-3.31631129755346,17.7406985030951,
949.03686588071));
#143908=CARTESIAN_POINT('Ctrl Pts',(-1.67239348737615,18.048,947.542748233651));
#143909=CARTESIAN_POINT('Ctrl Pts',(-2.21024254310115E-15,18.048,946.048630586592));
#143910=CARTESIAN_POINT('Ctrl Pts',(-2.21024254310115E-15,18.048,1047.75));
#143911=CARTESIAN_POINT('Ctrl Pts',(1.67239348737616,18.048,1046.25588235294));
#143912=CARTESIAN_POINT('Ctrl Pts',(3.31631129755346,17.7406985030951,1044.76176470588));
#143913=CARTESIAN_POINT('Ctrl Pts',(4.96022910773077,17.4333970061901,1043.26764705882));
#143914=CARTESIAN_POINT('Ctrl Pts',(6.51968959134575,16.8292587962898,1041.77352941176));
#143915=CARTESIAN_POINT('Ctrl Pts',(8.07915007496071,16.2251205863895,1040.27941176471));
#143916=CARTESIAN_POINT('Ctrl Pts',(9.50104767561053,15.3447188656481,1038.78529411765));
#143917=CARTESIAN_POINT('Ctrl Pts',(10.9229452762603,14.4643171449067,1037.29117647059));
#143918=CARTESIAN_POINT('Ctrl Pts',(12.1588589765331,13.3376329379985,1035.79705882353));
#143919=CARTESIAN_POINT('Ctrl Pts',(13.3947726768058,12.2109487310903,1034.30294117647));
#143920=CARTESIAN_POINT('Ctrl Pts',(14.4026149179538,10.8763499173728,1032.80882352941));
#143921=CARTESIAN_POINT('Ctrl Pts',(15.4104571591017,9.54175110365539,1031.31470588235));
#143922=CARTESIAN_POINT('Ctrl Pts',(16.1559070823762,8.04468584505496,1029.82058823529));
#143923=CARTESIAN_POINT('Ctrl Pts',(16.9013570056506,6.54762058645456,1028.32647058824));
#143924=CARTESIAN_POINT('Ctrl Pts',(17.3590292079831,4.93906964482096,1026.83235294118));
#143925=CARTESIAN_POINT('Ctrl Pts',(17.8167014103155,3.33051870318735,1025.33823529412));
#143926=CARTESIAN_POINT('Ctrl Pts',(17.9710104137728,1.66525935159367,1023.84411764706));
#143927=CARTESIAN_POINT('Ctrl Pts',(18.1253194172301,3.32956716117513E-15,
1022.35));
#143928=CARTESIAN_POINT('Ctrl Pts',(17.9710104137728,-1.66525935159367,
1020.85588235294));
#143929=CARTESIAN_POINT('Ctrl Pts',(17.8167014103155,-3.33051870318736,
1019.36176470588));
#143930=CARTESIAN_POINT('Ctrl Pts',(17.3590292079831,-4.93906964482095,
1017.86764705882));
#143931=CARTESIAN_POINT('Ctrl Pts',(16.9013570056506,-6.54762058645456,
1016.37352941176));
#143932=CARTESIAN_POINT('Ctrl Pts',(16.1559070823762,-8.04468584505497,
1014.87941176471));
#143933=CARTESIAN_POINT('Ctrl Pts',(15.4104571591017,-9.54175110365538,
1013.38529411765));
#143934=CARTESIAN_POINT('Ctrl Pts',(14.4026149179538,-10.8763499173728,
1011.89117647059));
#143935=CARTESIAN_POINT('Ctrl Pts',(13.3947726768058,-12.2109487310903,
1010.39705882353));
#143936=CARTESIAN_POINT('Ctrl Pts',(12.1588589765331,-13.3376329379985,
1008.90294117647));
#143937=CARTESIAN_POINT('Ctrl Pts',(10.9229452762603,-14.4643171449067,
1007.40882352941));
#143938=CARTESIAN_POINT('Ctrl Pts',(9.50104767561053,-15.3447188656481,
1005.91470588235));
#143939=CARTESIAN_POINT('Ctrl Pts',(8.07915007496071,-16.2251205863895,
1004.42058823529));
#143940=CARTESIAN_POINT('Ctrl Pts',(6.51968959134574,-16.8292587962898,
1002.92647058824));
#143941=CARTESIAN_POINT('Ctrl Pts',(4.96022910773078,-17.4333970061901,
1001.43235294118));
#143942=CARTESIAN_POINT('Ctrl Pts',(3.31631129755346,-17.7406985030951,
999.938235294118));
#143943=CARTESIAN_POINT('Ctrl Pts',(1.67239348737615,-18.048,998.444117647059));
#143944=CARTESIAN_POINT('Ctrl Pts',(0.,-18.048,996.95));
#143945=CARTESIAN_POINT('Ctrl Pts',(-1.67239348737615,-18.048,995.455882352941));
#143946=CARTESIAN_POINT('Ctrl Pts',(-3.31631129755346,-17.7406985030951,
993.961764705882));
#143947=CARTESIAN_POINT('Ctrl Pts',(-4.96022910773077,-17.4333970061901,
992.467647058824));
#143948=CARTESIAN_POINT('Ctrl Pts',(-6.51968959134574,-16.8292587962898,
990.973529411765));
#143949=CARTESIAN_POINT('Ctrl Pts',(-8.07915007496071,-16.2251205863895,
989.479411764706));
#143950=CARTESIAN_POINT('Ctrl Pts',(-9.50104767561052,-15.3447188656481,
987.985294117647));
#143951=CARTESIAN_POINT('Ctrl Pts',(-10.9229452762603,-14.4643171449067,
986.491176470588));
#143952=CARTESIAN_POINT('Ctrl Pts',(-12.1588589765331,-13.3376329379985,
984.997058823529));
#143953=CARTESIAN_POINT('Ctrl Pts',(-13.3947726768058,-12.2109487310903,
983.502941176471));
#143954=CARTESIAN_POINT('Ctrl Pts',(-14.4026149179538,-10.8763499173728,
982.008823529412));
#143955=CARTESIAN_POINT('Ctrl Pts',(-15.4104571591017,-9.54175110365538,
980.514705882353));
#143956=CARTESIAN_POINT('Ctrl Pts',(-16.1559070823762,-8.04468584505497,
979.020588235294));
#143957=CARTESIAN_POINT('Ctrl Pts',(-16.9013570056506,-6.54762058645456,
977.526470588235));
#143958=CARTESIAN_POINT('Ctrl Pts',(-17.3590292079831,-4.93906964482095,
976.032352941177));
#143959=CARTESIAN_POINT('Ctrl Pts',(-17.8167014103155,-3.33051870318735,
974.538235294118));
#143960=CARTESIAN_POINT('Ctrl Pts',(-17.9710104137728,-1.66525935159368,
973.044117647059));
#143961=CARTESIAN_POINT('Ctrl Pts',(-18.1253194172301,-1.10985572039171E-15,
971.55));
#143962=CARTESIAN_POINT('Ctrl Pts',(-17.9710104137728,1.66525935159367,
970.055882352941));
#143963=CARTESIAN_POINT('Ctrl Pts',(-17.8167014103155,3.33051870318735,
968.561764705883));
#143964=CARTESIAN_POINT('Ctrl Pts',(-17.3590292079831,4.93906964482096,
967.067647058824));
#143965=CARTESIAN_POINT('Ctrl Pts',(-16.9013570056506,6.54762058645456,
965.573529411765));
#143966=CARTESIAN_POINT('Ctrl Pts',(-16.1559070823762,8.04468584505497,
964.079411764706));
#143967=CARTESIAN_POINT('Ctrl Pts',(-15.4104571591017,9.54175110365538,
962.585294117647));
#143968=CARTESIAN_POINT('Ctrl Pts',(-14.4026149179538,10.8763499173728,
961.091176470588));
#143969=CARTESIAN_POINT('Ctrl Pts',(-13.3947726768058,12.2109487310903,
959.59705882353));
#143970=CARTESIAN_POINT('Ctrl Pts',(-12.1588589765331,13.3376329379985,
958.102941176471));
#143971=CARTESIAN_POINT('Ctrl Pts',(-10.9229452762603,14.4643171449067,
956.608823529412));
#143972=CARTESIAN_POINT('Ctrl Pts',(-9.50104767561052,15.3447188656481,
955.114705882353));
#143973=CARTESIAN_POINT('Ctrl Pts',(-8.07915007496071,16.2251205863895,
953.620588235294));
#143974=CARTESIAN_POINT('Ctrl Pts',(-6.51968959134574,16.8292587962898,
952.126470588235));
#143975=CARTESIAN_POINT('Ctrl Pts',(-4.96022910773078,17.4333970061901,
950.632352941177));
#143976=CARTESIAN_POINT('Ctrl Pts',(-3.31631129755346,17.7406985030951,
949.138235294118));
#143977=CARTESIAN_POINT('Ctrl Pts',(-1.67239348737615,18.048,947.644117647059));
#143978=CARTESIAN_POINT('Ctrl Pts',(-2.21024254310115E-15,18.048,946.15));
#143979=CARTESIAN_POINT('Origin',(5.37704275891775E-14,4.44089209850063E-14,
1504.8993152933));
#143980=CARTESIAN_POINT('',(5.15601850460762E-14,18.048,844.448630586592));
#143981=CARTESIAN_POINT('',(5.15601850460762E-14,18.048,844.55));
#143982=CARTESIAN_POINT('',(1.05330612635254E-13,18.0480000000001,1504.8993152933));
#143983=CARTESIAN_POINT('Ctrl Pts',(-2.21024254310115E-15,18.048,946.048630586592));
#143984=CARTESIAN_POINT('Ctrl Pts',(1.67239348737616,18.048,944.554512939534));
#143985=CARTESIAN_POINT('Ctrl Pts',(3.31631129755346,17.7406985030951,943.060395292475));
#143986=CARTESIAN_POINT('Ctrl Pts',(4.96022910773077,17.4333970061901,941.566277645416));
#143987=CARTESIAN_POINT('Ctrl Pts',(6.51968959134575,16.8292587962898,940.072159998357));
#143988=CARTESIAN_POINT('Ctrl Pts',(8.07915007496071,16.2251205863895,938.578042351298));
#143989=CARTESIAN_POINT('Ctrl Pts',(9.50104767561053,15.3447188656481,937.083924704239));
#143990=CARTESIAN_POINT('Ctrl Pts',(10.9229452762603,14.4643171449067,935.589807057181));
#143991=CARTESIAN_POINT('Ctrl Pts',(12.1588589765331,13.3376329379985,934.095689410122));
#143992=CARTESIAN_POINT('Ctrl Pts',(13.3947726768058,12.2109487310903,932.601571763063));
#143993=CARTESIAN_POINT('Ctrl Pts',(14.4026149179538,10.8763499173728,931.107454116004));
#143994=CARTESIAN_POINT('Ctrl Pts',(15.4104571591017,9.54175110365539,929.613336468945));
#143995=CARTESIAN_POINT('Ctrl Pts',(16.1559070823762,8.04468584505496,928.119218821886));
#143996=CARTESIAN_POINT('Ctrl Pts',(16.9013570056506,6.54762058645456,926.625101174828));
#143997=CARTESIAN_POINT('Ctrl Pts',(17.3590292079831,4.93906964482096,925.130983527769));
#143998=CARTESIAN_POINT('Ctrl Pts',(17.8167014103155,3.33051870318735,923.63686588071));
#143999=CARTESIAN_POINT('Ctrl Pts',(17.9710104137728,1.66525935159367,922.142748233651));
#144000=CARTESIAN_POINT('Ctrl Pts',(18.1253194172301,3.32956716117513E-15,
920.648630586592));
#144001=CARTESIAN_POINT('Ctrl Pts',(17.9710104137728,-1.66525935159367,
919.154512939534));
#144002=CARTESIAN_POINT('Ctrl Pts',(17.8167014103155,-3.33051870318736,
917.660395292475));
#144003=CARTESIAN_POINT('Ctrl Pts',(17.3590292079831,-4.93906964482095,
916.166277645416));
#144004=CARTESIAN_POINT('Ctrl Pts',(16.9013570056506,-6.54762058645456,
914.672159998357));
#144005=CARTESIAN_POINT('Ctrl Pts',(16.1559070823762,-8.04468584505497,
913.178042351298));
#144006=CARTESIAN_POINT('Ctrl Pts',(15.4104571591017,-9.54175110365538,
911.683924704239));
#144007=CARTESIAN_POINT('Ctrl Pts',(14.4026149179538,-10.8763499173728,
910.18980705718));
#144008=CARTESIAN_POINT('Ctrl Pts',(13.3947726768058,-12.2109487310903,
908.695689410122));
#144009=CARTESIAN_POINT('Ctrl Pts',(12.1588589765331,-13.3376329379985,
907.201571763063));
#144010=CARTESIAN_POINT('Ctrl Pts',(10.9229452762603,-14.4643171449067,
905.707454116004));
#144011=CARTESIAN_POINT('Ctrl Pts',(9.50104767561053,-15.3447188656481,
904.213336468945));
#144012=CARTESIAN_POINT('Ctrl Pts',(8.07915007496071,-16.2251205863895,
902.719218821886));
#144013=CARTESIAN_POINT('Ctrl Pts',(6.51968959134574,-16.8292587962898,
901.225101174828));
#144014=CARTESIAN_POINT('Ctrl Pts',(4.96022910773078,-17.4333970061901,
899.730983527769));
#144015=CARTESIAN_POINT('Ctrl Pts',(3.31631129755346,-17.7406985030951,
898.23686588071));
#144016=CARTESIAN_POINT('Ctrl Pts',(1.67239348737615,-18.048,896.742748233651));
#144017=CARTESIAN_POINT('Ctrl Pts',(0.,-18.048,895.248630586592));
#144018=CARTESIAN_POINT('Ctrl Pts',(-1.67239348737615,-18.048,893.754512939534));
#144019=CARTESIAN_POINT('Ctrl Pts',(-3.31631129755346,-17.7406985030951,
892.260395292475));
#144020=CARTESIAN_POINT('Ctrl Pts',(-4.96022910773077,-17.4333970061901,
890.766277645416));
#144021=CARTESIAN_POINT('Ctrl Pts',(-6.51968959134574,-16.8292587962898,
889.272159998357));
#144022=CARTESIAN_POINT('Ctrl Pts',(-8.07915007496071,-16.2251205863895,
887.778042351298));
#144023=CARTESIAN_POINT('Ctrl Pts',(-9.50104767561052,-15.3447188656481,
886.283924704239));
#144024=CARTESIAN_POINT('Ctrl Pts',(-10.9229452762603,-14.4643171449067,
884.789807057181));
#144025=CARTESIAN_POINT('Ctrl Pts',(-12.1588589765331,-13.3376329379985,
883.295689410122));
#144026=CARTESIAN_POINT('Ctrl Pts',(-13.3947726768058,-12.2109487310903,
881.801571763063));
#144027=CARTESIAN_POINT('Ctrl Pts',(-14.4026149179538,-10.8763499173728,
880.307454116004));
#144028=CARTESIAN_POINT('Ctrl Pts',(-15.4104571591017,-9.54175110365538,
878.813336468945));
#144029=CARTESIAN_POINT('Ctrl Pts',(-16.1559070823762,-8.04468584505497,
877.319218821886));
#144030=CARTESIAN_POINT('Ctrl Pts',(-16.9013570056506,-6.54762058645456,
875.825101174828));
#144031=CARTESIAN_POINT('Ctrl Pts',(-17.3590292079831,-4.93906964482095,
874.330983527769));
#144032=CARTESIAN_POINT('Ctrl Pts',(-17.8167014103155,-3.33051870318735,
872.83686588071));
#144033=CARTESIAN_POINT('Ctrl Pts',(-17.9710104137728,-1.66525935159368,
871.342748233651));
#144034=CARTESIAN_POINT('Ctrl Pts',(-18.1253194172301,-1.10985572039171E-15,
869.848630586592));
#144035=CARTESIAN_POINT('Ctrl Pts',(-17.9710104137728,1.66525935159367,
868.354512939534));
#144036=CARTESIAN_POINT('Ctrl Pts',(-17.8167014103155,3.33051870318735,
866.860395292475));
#144037=CARTESIAN_POINT('Ctrl Pts',(-17.3590292079831,4.93906964482096,
865.366277645416));
#144038=CARTESIAN_POINT('Ctrl Pts',(-16.9013570056506,6.54762058645456,
863.872159998357));
#144039=CARTESIAN_POINT('Ctrl Pts',(-16.1559070823762,8.04468584505497,
862.378042351298));
#144040=CARTESIAN_POINT('Ctrl Pts',(-15.4104571591017,9.54175110365538,
860.883924704239));
#144041=CARTESIAN_POINT('Ctrl Pts',(-14.4026149179538,10.8763499173728,
859.389807057181));
#144042=CARTESIAN_POINT('Ctrl Pts',(-13.3947726768058,12.2109487310903,
857.895689410122));
#144043=CARTESIAN_POINT('Ctrl Pts',(-12.1588589765331,13.3376329379985,
856.401571763063));
#144044=CARTESIAN_POINT('Ctrl Pts',(-10.9229452762603,14.4643171449067,
854.907454116004));
#144045=CARTESIAN_POINT('Ctrl Pts',(-9.50104767561052,15.3447188656481,
853.413336468945));
#144046=CARTESIAN_POINT('Ctrl Pts',(-8.07915007496071,16.2251205863895,
851.919218821886));
#144047=CARTESIAN_POINT('Ctrl Pts',(-6.51968959134574,16.8292587962898,
850.425101174828));
#144048=CARTESIAN_POINT('Ctrl Pts',(-4.96022910773078,17.4333970061901,
848.930983527769));
#144049=CARTESIAN_POINT('Ctrl Pts',(-3.31631129755346,17.7406985030951,
847.43686588071));
#144050=CARTESIAN_POINT('Ctrl Pts',(-1.67239348737615,18.048,845.942748233651));
#144051=CARTESIAN_POINT('Ctrl Pts',(-2.21024254310115E-15,18.048,844.448630586592));
#144052=CARTESIAN_POINT('Ctrl Pts',(-2.21024254310115E-15,18.048,946.15));
#144053=CARTESIAN_POINT('Ctrl Pts',(1.67239348737616,18.048,944.655882352941));
#144054=CARTESIAN_POINT('Ctrl Pts',(3.31631129755346,17.7406985030951,943.161764705882));
#144055=CARTESIAN_POINT('Ctrl Pts',(4.96022910773077,17.4333970061901,941.667647058824));
#144056=CARTESIAN_POINT('Ctrl Pts',(6.51968959134575,16.8292587962898,940.173529411765));
#144057=CARTESIAN_POINT('Ctrl Pts',(8.07915007496071,16.2251205863895,938.679411764706));
#144058=CARTESIAN_POINT('Ctrl Pts',(9.50104767561053,15.3447188656481,937.185294117647));
#144059=CARTESIAN_POINT('Ctrl Pts',(10.9229452762603,14.4643171449067,935.691176470589));
#144060=CARTESIAN_POINT('Ctrl Pts',(12.1588589765331,13.3376329379985,934.19705882353));
#144061=CARTESIAN_POINT('Ctrl Pts',(13.3947726768058,12.2109487310903,932.702941176471));
#144062=CARTESIAN_POINT('Ctrl Pts',(14.4026149179538,10.8763499173728,931.208823529412));
#144063=CARTESIAN_POINT('Ctrl Pts',(15.4104571591017,9.54175110365539,929.714705882353));
#144064=CARTESIAN_POINT('Ctrl Pts',(16.1559070823762,8.04468584505496,928.220588235294));
#144065=CARTESIAN_POINT('Ctrl Pts',(16.9013570056506,6.54762058645456,926.726470588235));
#144066=CARTESIAN_POINT('Ctrl Pts',(17.3590292079831,4.93906964482096,925.232352941176));
#144067=CARTESIAN_POINT('Ctrl Pts',(17.8167014103155,3.33051870318735,923.738235294118));
#144068=CARTESIAN_POINT('Ctrl Pts',(17.9710104137728,1.66525935159367,922.244117647059));
#144069=CARTESIAN_POINT('Ctrl Pts',(18.1253194172301,3.32956716117513E-15,
920.75));
#144070=CARTESIAN_POINT('Ctrl Pts',(17.9710104137728,-1.66525935159367,
919.255882352941));
#144071=CARTESIAN_POINT('Ctrl Pts',(17.8167014103155,-3.33051870318736,
917.761764705882));
#144072=CARTESIAN_POINT('Ctrl Pts',(17.3590292079831,-4.93906964482095,
916.267647058824));
#144073=CARTESIAN_POINT('Ctrl Pts',(16.9013570056506,-6.54762058645456,
914.773529411765));
#144074=CARTESIAN_POINT('Ctrl Pts',(16.1559070823762,-8.04468584505497,
913.279411764706));
#144075=CARTESIAN_POINT('Ctrl Pts',(15.4104571591017,-9.54175110365538,
911.785294117647));
#144076=CARTESIAN_POINT('Ctrl Pts',(14.4026149179538,-10.8763499173728,
910.291176470588));
#144077=CARTESIAN_POINT('Ctrl Pts',(13.3947726768058,-12.2109487310903,
908.79705882353));
#144078=CARTESIAN_POINT('Ctrl Pts',(12.1588589765331,-13.3376329379985,
907.302941176471));
#144079=CARTESIAN_POINT('Ctrl Pts',(10.9229452762603,-14.4643171449067,
905.808823529412));
#144080=CARTESIAN_POINT('Ctrl Pts',(9.50104767561053,-15.3447188656481,
904.314705882353));
#144081=CARTESIAN_POINT('Ctrl Pts',(8.07915007496071,-16.2251205863895,
902.820588235294));
#144082=CARTESIAN_POINT('Ctrl Pts',(6.51968959134574,-16.8292587962898,
901.326470588235));
#144083=CARTESIAN_POINT('Ctrl Pts',(4.96022910773078,-17.4333970061901,
899.832352941177));
#144084=CARTESIAN_POINT('Ctrl Pts',(3.31631129755346,-17.7406985030951,
898.338235294118));
#144085=CARTESIAN_POINT('Ctrl Pts',(1.67239348737615,-18.048,896.844117647059));
#144086=CARTESIAN_POINT('Ctrl Pts',(0.,-18.048,895.35));
#144087=CARTESIAN_POINT('Ctrl Pts',(-1.67239348737615,-18.048,893.855882352941));
#144088=CARTESIAN_POINT('Ctrl Pts',(-3.31631129755346,-17.7406985030951,
892.361764705882));
#144089=CARTESIAN_POINT('Ctrl Pts',(-4.96022910773077,-17.4333970061901,
890.867647058824));
#144090=CARTESIAN_POINT('Ctrl Pts',(-6.51968959134574,-16.8292587962898,
889.373529411765));
#144091=CARTESIAN_POINT('Ctrl Pts',(-8.07915007496071,-16.2251205863895,
887.879411764706));
#144092=CARTESIAN_POINT('Ctrl Pts',(-9.50104767561052,-15.3447188656481,
886.385294117647));
#144093=CARTESIAN_POINT('Ctrl Pts',(-10.9229452762603,-14.4643171449067,
884.891176470588));
#144094=CARTESIAN_POINT('Ctrl Pts',(-12.1588589765331,-13.3376329379985,
883.39705882353));
#144095=CARTESIAN_POINT('Ctrl Pts',(-13.3947726768058,-12.2109487310903,
881.902941176471));
#144096=CARTESIAN_POINT('Ctrl Pts',(-14.4026149179538,-10.8763499173728,
880.408823529412));
#144097=CARTESIAN_POINT('Ctrl Pts',(-15.4104571591017,-9.54175110365538,
878.914705882353));
#144098=CARTESIAN_POINT('Ctrl Pts',(-16.1559070823762,-8.04468584505497,
877.420588235294));
#144099=CARTESIAN_POINT('Ctrl Pts',(-16.9013570056506,-6.54762058645456,
875.926470588235));
#144100=CARTESIAN_POINT('Ctrl Pts',(-17.3590292079831,-4.93906964482095,
874.432352941177));
#144101=CARTESIAN_POINT('Ctrl Pts',(-17.8167014103155,-3.33051870318735,
872.938235294118));
#144102=CARTESIAN_POINT('Ctrl Pts',(-17.9710104137728,-1.66525935159368,
871.444117647059));
#144103=CARTESIAN_POINT('Ctrl Pts',(-18.1253194172301,-1.10985572039171E-15,
869.95));
#144104=CARTESIAN_POINT('Ctrl Pts',(-17.9710104137728,1.66525935159367,
868.455882352941));
#144105=CARTESIAN_POINT('Ctrl Pts',(-17.8167014103155,3.33051870318735,
866.961764705882));
#144106=CARTESIAN_POINT('Ctrl Pts',(-17.3590292079831,4.93906964482096,
865.467647058824));
#144107=CARTESIAN_POINT('Ctrl Pts',(-16.9013570056506,6.54762058645456,
863.973529411765));
#144108=CARTESIAN_POINT('Ctrl Pts',(-16.1559070823762,8.04468584505497,
862.479411764706));
#144109=CARTESIAN_POINT('Ctrl Pts',(-15.4104571591017,9.54175110365538,
860.985294117647));
#144110=CARTESIAN_POINT('Ctrl Pts',(-14.4026149179538,10.8763499173728,
859.491176470588));
#144111=CARTESIAN_POINT('Ctrl Pts',(-13.3947726768058,12.2109487310903,
857.99705882353));
#144112=CARTESIAN_POINT('Ctrl Pts',(-12.1588589765331,13.3376329379985,
856.502941176471));
#144113=CARTESIAN_POINT('Ctrl Pts',(-10.9229452762603,14.4643171449067,
855.008823529412));
#144114=CARTESIAN_POINT('Ctrl Pts',(-9.50104767561052,15.3447188656481,
853.514705882353));
#144115=CARTESIAN_POINT('Ctrl Pts',(-8.07915007496071,16.2251205863895,
852.020588235294));
#144116=CARTESIAN_POINT('Ctrl Pts',(-6.51968959134574,16.8292587962898,
850.526470588235));
#144117=CARTESIAN_POINT('Ctrl Pts',(-4.96022910773078,17.4333970061901,
849.032352941177));
#144118=CARTESIAN_POINT('Ctrl Pts',(-3.31631129755346,17.7406985030951,
847.538235294118));
#144119=CARTESIAN_POINT('Ctrl Pts',(-1.67239348737615,18.048,846.044117647059));
#144120=CARTESIAN_POINT('Ctrl Pts',(-2.21024254310115E-15,18.048,844.55));
#144121=CARTESIAN_POINT('Origin',(5.37704275891775E-14,4.44089209850063E-14,
1504.8993152933));
#144122=CARTESIAN_POINT('',(5.15601850460762E-14,18.048,742.848630586592));
#144123=CARTESIAN_POINT('',(5.15601850460762E-14,18.048,742.95));
#144124=CARTESIAN_POINT('',(1.05330612635254E-13,18.0480000000001,1504.8993152933));
#144125=CARTESIAN_POINT('Ctrl Pts',(-2.21024254310115E-15,18.048,844.448630586592));
#144126=CARTESIAN_POINT('Ctrl Pts',(1.67239348737616,18.048,842.954512939534));
#144127=CARTESIAN_POINT('Ctrl Pts',(3.31631129755346,17.7406985030951,841.460395292475));
#144128=CARTESIAN_POINT('Ctrl Pts',(4.96022910773077,17.4333970061901,839.966277645416));
#144129=CARTESIAN_POINT('Ctrl Pts',(6.51968959134575,16.8292587962898,838.472159998357));
#144130=CARTESIAN_POINT('Ctrl Pts',(8.07915007496071,16.2251205863895,836.978042351298));
#144131=CARTESIAN_POINT('Ctrl Pts',(9.50104767561053,15.3447188656481,835.483924704239));
#144132=CARTESIAN_POINT('Ctrl Pts',(10.9229452762603,14.4643171449067,833.989807057181));
#144133=CARTESIAN_POINT('Ctrl Pts',(12.1588589765331,13.3376329379985,832.495689410122));
#144134=CARTESIAN_POINT('Ctrl Pts',(13.3947726768058,12.2109487310903,831.001571763063));
#144135=CARTESIAN_POINT('Ctrl Pts',(14.4026149179538,10.8763499173728,829.507454116004));
#144136=CARTESIAN_POINT('Ctrl Pts',(15.4104571591017,9.54175110365539,828.013336468945));
#144137=CARTESIAN_POINT('Ctrl Pts',(16.1559070823762,8.04468584505496,826.519218821886));
#144138=CARTESIAN_POINT('Ctrl Pts',(16.9013570056506,6.54762058645456,825.025101174828));
#144139=CARTESIAN_POINT('Ctrl Pts',(17.3590292079831,4.93906964482096,823.530983527769));
#144140=CARTESIAN_POINT('Ctrl Pts',(17.8167014103155,3.33051870318735,822.03686588071));
#144141=CARTESIAN_POINT('Ctrl Pts',(17.9710104137728,1.66525935159367,820.542748233651));
#144142=CARTESIAN_POINT('Ctrl Pts',(18.1253194172301,3.32956716117513E-15,
819.048630586592));
#144143=CARTESIAN_POINT('Ctrl Pts',(17.9710104137728,-1.66525935159367,
817.554512939533));
#144144=CARTESIAN_POINT('Ctrl Pts',(17.8167014103155,-3.33051870318736,
816.060395292475));
#144145=CARTESIAN_POINT('Ctrl Pts',(17.3590292079831,-4.93906964482095,
814.566277645416));
#144146=CARTESIAN_POINT('Ctrl Pts',(16.9013570056506,-6.54762058645456,
813.072159998357));
#144147=CARTESIAN_POINT('Ctrl Pts',(16.1559070823762,-8.04468584505497,
811.578042351298));
#144148=CARTESIAN_POINT('Ctrl Pts',(15.4104571591017,-9.54175110365538,
810.083924704239));
#144149=CARTESIAN_POINT('Ctrl Pts',(14.4026149179538,-10.8763499173728,
808.589807057181));
#144150=CARTESIAN_POINT('Ctrl Pts',(13.3947726768058,-12.2109487310903,
807.095689410122));
#144151=CARTESIAN_POINT('Ctrl Pts',(12.1588589765331,-13.3376329379985,
805.601571763063));
#144152=CARTESIAN_POINT('Ctrl Pts',(10.9229452762603,-14.4643171449067,
804.107454116004));
#144153=CARTESIAN_POINT('Ctrl Pts',(9.50104767561053,-15.3447188656481,
802.613336468945));
#144154=CARTESIAN_POINT('Ctrl Pts',(8.07915007496071,-16.2251205863895,
801.119218821887));
#144155=CARTESIAN_POINT('Ctrl Pts',(6.51968959134574,-16.8292587962898,
799.625101174828));
#144156=CARTESIAN_POINT('Ctrl Pts',(4.96022910773078,-17.4333970061901,
798.130983527769));
#144157=CARTESIAN_POINT('Ctrl Pts',(3.31631129755346,-17.7406985030951,
796.63686588071));
#144158=CARTESIAN_POINT('Ctrl Pts',(1.67239348737615,-18.048,795.142748233651));
#144159=CARTESIAN_POINT('Ctrl Pts',(0.,-18.048,793.648630586592));
#144160=CARTESIAN_POINT('Ctrl Pts',(-1.67239348737615,-18.048,792.154512939534));
#144161=CARTESIAN_POINT('Ctrl Pts',(-3.31631129755346,-17.7406985030951,
790.660395292475));
#144162=CARTESIAN_POINT('Ctrl Pts',(-4.96022910773077,-17.4333970061901,
789.166277645416));
#144163=CARTESIAN_POINT('Ctrl Pts',(-6.51968959134574,-16.8292587962898,
787.672159998357));
#144164=CARTESIAN_POINT('Ctrl Pts',(-8.07915007496071,-16.2251205863895,
786.178042351298));
#144165=CARTESIAN_POINT('Ctrl Pts',(-9.50104767561052,-15.3447188656481,
784.683924704239));
#144166=CARTESIAN_POINT('Ctrl Pts',(-10.9229452762603,-14.4643171449067,
783.189807057181));
#144167=CARTESIAN_POINT('Ctrl Pts',(-12.1588589765331,-13.3376329379985,
781.695689410122));
#144168=CARTESIAN_POINT('Ctrl Pts',(-13.3947726768058,-12.2109487310903,
780.201571763063));
#144169=CARTESIAN_POINT('Ctrl Pts',(-14.4026149179538,-10.8763499173728,
778.707454116004));
#144170=CARTESIAN_POINT('Ctrl Pts',(-15.4104571591017,-9.54175110365538,
777.213336468945));
#144171=CARTESIAN_POINT('Ctrl Pts',(-16.1559070823762,-8.04468584505497,
775.719218821886));
#144172=CARTESIAN_POINT('Ctrl Pts',(-16.9013570056506,-6.54762058645456,
774.225101174828));
#144173=CARTESIAN_POINT('Ctrl Pts',(-17.3590292079831,-4.93906964482095,
772.730983527769));
#144174=CARTESIAN_POINT('Ctrl Pts',(-17.8167014103155,-3.33051870318735,
771.23686588071));
#144175=CARTESIAN_POINT('Ctrl Pts',(-17.9710104137728,-1.66525935159368,
769.742748233651));
#144176=CARTESIAN_POINT('Ctrl Pts',(-18.1253194172301,-1.10985572039171E-15,
768.248630586592));
#144177=CARTESIAN_POINT('Ctrl Pts',(-17.9710104137728,1.66525935159367,
766.754512939533));
#144178=CARTESIAN_POINT('Ctrl Pts',(-17.8167014103155,3.33051870318735,
765.260395292475));
#144179=CARTESIAN_POINT('Ctrl Pts',(-17.3590292079831,4.93906964482096,
763.766277645416));
#144180=CARTESIAN_POINT('Ctrl Pts',(-16.9013570056506,6.54762058645456,
762.272159998357));
#144181=CARTESIAN_POINT('Ctrl Pts',(-16.1559070823762,8.04468584505497,
760.778042351298));
#144182=CARTESIAN_POINT('Ctrl Pts',(-15.4104571591017,9.54175110365538,
759.283924704239));
#144183=CARTESIAN_POINT('Ctrl Pts',(-14.4026149179538,10.8763499173728,
757.78980705718));
#144184=CARTESIAN_POINT('Ctrl Pts',(-13.3947726768058,12.2109487310903,
756.295689410122));
#144185=CARTESIAN_POINT('Ctrl Pts',(-12.1588589765331,13.3376329379985,
754.801571763063));
#144186=CARTESIAN_POINT('Ctrl Pts',(-10.9229452762603,14.4643171449067,
753.307454116004));
#144187=CARTESIAN_POINT('Ctrl Pts',(-9.50104767561052,15.3447188656481,
751.813336468945));
#144188=CARTESIAN_POINT('Ctrl Pts',(-8.07915007496071,16.2251205863895,
750.319218821886));
#144189=CARTESIAN_POINT('Ctrl Pts',(-6.51968959134574,16.8292587962898,
748.825101174828));
#144190=CARTESIAN_POINT('Ctrl Pts',(-4.96022910773078,17.4333970061901,
747.330983527769));
#144191=CARTESIAN_POINT('Ctrl Pts',(-3.31631129755346,17.7406985030951,
745.83686588071));
#144192=CARTESIAN_POINT('Ctrl Pts',(-1.67239348737615,18.048,744.342748233651));
#144193=CARTESIAN_POINT('Ctrl Pts',(-2.21024254310115E-15,18.048,742.848630586592));
#144194=CARTESIAN_POINT('Ctrl Pts',(-2.21024254310115E-15,18.048,844.55));
#144195=CARTESIAN_POINT('Ctrl Pts',(1.67239348737616,18.048,843.055882352941));
#144196=CARTESIAN_POINT('Ctrl Pts',(3.31631129755346,17.7406985030951,841.561764705883));
#144197=CARTESIAN_POINT('Ctrl Pts',(4.96022910773077,17.4333970061901,840.067647058824));
#144198=CARTESIAN_POINT('Ctrl Pts',(6.51968959134575,16.8292587962898,838.573529411765));
#144199=CARTESIAN_POINT('Ctrl Pts',(8.07915007496071,16.2251205863895,837.079411764706));
#144200=CARTESIAN_POINT('Ctrl Pts',(9.50104767561053,15.3447188656481,835.585294117647));
#144201=CARTESIAN_POINT('Ctrl Pts',(10.9229452762603,14.4643171449067,834.091176470588));
#144202=CARTESIAN_POINT('Ctrl Pts',(12.1588589765331,13.3376329379985,832.597058823529));
#144203=CARTESIAN_POINT('Ctrl Pts',(13.3947726768058,12.2109487310903,831.102941176471));
#144204=CARTESIAN_POINT('Ctrl Pts',(14.4026149179538,10.8763499173728,829.608823529412));
#144205=CARTESIAN_POINT('Ctrl Pts',(15.4104571591017,9.54175110365539,828.114705882353));
#144206=CARTESIAN_POINT('Ctrl Pts',(16.1559070823762,8.04468584505496,826.620588235294));
#144207=CARTESIAN_POINT('Ctrl Pts',(16.9013570056506,6.54762058645456,825.126470588235));
#144208=CARTESIAN_POINT('Ctrl Pts',(17.3590292079831,4.93906964482096,823.632352941177));
#144209=CARTESIAN_POINT('Ctrl Pts',(17.8167014103155,3.33051870318735,822.138235294118));
#144210=CARTESIAN_POINT('Ctrl Pts',(17.9710104137728,1.66525935159367,820.644117647059));
#144211=CARTESIAN_POINT('Ctrl Pts',(18.1253194172301,3.32956716117513E-15,
819.15));
#144212=CARTESIAN_POINT('Ctrl Pts',(17.9710104137728,-1.66525935159367,
817.655882352941));
#144213=CARTESIAN_POINT('Ctrl Pts',(17.8167014103155,-3.33051870318736,
816.161764705882));
#144214=CARTESIAN_POINT('Ctrl Pts',(17.3590292079831,-4.93906964482095,
814.667647058824));
#144215=CARTESIAN_POINT('Ctrl Pts',(16.9013570056506,-6.54762058645456,
813.173529411765));
#144216=CARTESIAN_POINT('Ctrl Pts',(16.1559070823762,-8.04468584505497,
811.679411764706));
#144217=CARTESIAN_POINT('Ctrl Pts',(15.4104571591017,-9.54175110365538,
810.185294117647));
#144218=CARTESIAN_POINT('Ctrl Pts',(14.4026149179538,-10.8763499173728,
808.691176470588));
#144219=CARTESIAN_POINT('Ctrl Pts',(13.3947726768058,-12.2109487310903,
807.19705882353));
#144220=CARTESIAN_POINT('Ctrl Pts',(12.1588589765331,-13.3376329379985,
805.702941176471));
#144221=CARTESIAN_POINT('Ctrl Pts',(10.9229452762603,-14.4643171449067,
804.208823529412));
#144222=CARTESIAN_POINT('Ctrl Pts',(9.50104767561053,-15.3447188656481,
802.714705882353));
#144223=CARTESIAN_POINT('Ctrl Pts',(8.07915007496071,-16.2251205863895,
801.220588235294));
#144224=CARTESIAN_POINT('Ctrl Pts',(6.51968959134574,-16.8292587962898,
799.726470588235));
#144225=CARTESIAN_POINT('Ctrl Pts',(4.96022910773078,-17.4333970061901,
798.232352941177));
#144226=CARTESIAN_POINT('Ctrl Pts',(3.31631129755346,-17.7406985030951,
796.738235294118));
#144227=CARTESIAN_POINT('Ctrl Pts',(1.67239348737615,-18.048,795.244117647059));
#144228=CARTESIAN_POINT('Ctrl Pts',(0.,-18.048,793.75));
#144229=CARTESIAN_POINT('Ctrl Pts',(-1.67239348737615,-18.048,792.255882352941));
#144230=CARTESIAN_POINT('Ctrl Pts',(-3.31631129755346,-17.7406985030951,
790.761764705882));
#144231=CARTESIAN_POINT('Ctrl Pts',(-4.96022910773077,-17.4333970061901,
789.267647058824));
#144232=CARTESIAN_POINT('Ctrl Pts',(-6.51968959134574,-16.8292587962898,
787.773529411765));
#144233=CARTESIAN_POINT('Ctrl Pts',(-8.07915007496071,-16.2251205863895,
786.279411764706));
#144234=CARTESIAN_POINT('Ctrl Pts',(-9.50104767561052,-15.3447188656481,
784.785294117647));
#144235=CARTESIAN_POINT('Ctrl Pts',(-10.9229452762603,-14.4643171449067,
783.291176470588));
#144236=CARTESIAN_POINT('Ctrl Pts',(-12.1588589765331,-13.3376329379985,
781.797058823529));
#144237=CARTESIAN_POINT('Ctrl Pts',(-13.3947726768058,-12.2109487310903,
780.302941176471));
#144238=CARTESIAN_POINT('Ctrl Pts',(-14.4026149179538,-10.8763499173728,
778.808823529412));
#144239=CARTESIAN_POINT('Ctrl Pts',(-15.4104571591017,-9.54175110365538,
777.314705882353));
#144240=CARTESIAN_POINT('Ctrl Pts',(-16.1559070823762,-8.04468584505497,
775.820588235294));
#144241=CARTESIAN_POINT('Ctrl Pts',(-16.9013570056506,-6.54762058645456,
774.326470588235));
#144242=CARTESIAN_POINT('Ctrl Pts',(-17.3590292079831,-4.93906964482095,
772.832352941177));
#144243=CARTESIAN_POINT('Ctrl Pts',(-17.8167014103155,-3.33051870318735,
771.338235294118));
#144244=CARTESIAN_POINT('Ctrl Pts',(-17.9710104137728,-1.66525935159368,
769.844117647059));
#144245=CARTESIAN_POINT('Ctrl Pts',(-18.1253194172301,-1.10985572039171E-15,
768.35));
#144246=CARTESIAN_POINT('Ctrl Pts',(-17.9710104137728,1.66525935159367,
766.855882352941));
#144247=CARTESIAN_POINT('Ctrl Pts',(-17.8167014103155,3.33051870318735,
765.361764705882));
#144248=CARTESIAN_POINT('Ctrl Pts',(-17.3590292079831,4.93906964482096,
763.867647058824));
#144249=CARTESIAN_POINT('Ctrl Pts',(-16.9013570056506,6.54762058645456,
762.373529411765));
#144250=CARTESIAN_POINT('Ctrl Pts',(-16.1559070823762,8.04468584505497,
760.879411764706));
#144251=CARTESIAN_POINT('Ctrl Pts',(-15.4104571591017,9.54175110365538,
759.385294117647));
#144252=CARTESIAN_POINT('Ctrl Pts',(-14.4026149179538,10.8763499173728,
757.891176470588));
#144253=CARTESIAN_POINT('Ctrl Pts',(-13.3947726768058,12.2109487310903,
756.39705882353));
#144254=CARTESIAN_POINT('Ctrl Pts',(-12.1588589765331,13.3376329379985,
754.902941176471));
#144255=CARTESIAN_POINT('Ctrl Pts',(-10.9229452762603,14.4643171449067,
753.408823529412));
#144256=CARTESIAN_POINT('Ctrl Pts',(-9.50104767561052,15.3447188656481,
751.914705882353));
#144257=CARTESIAN_POINT('Ctrl Pts',(-8.07915007496071,16.2251205863895,
750.420588235294));
#144258=CARTESIAN_POINT('Ctrl Pts',(-6.51968959134574,16.8292587962898,
748.926470588235));
#144259=CARTESIAN_POINT('Ctrl Pts',(-4.96022910773078,17.4333970061901,
747.432352941177));
#144260=CARTESIAN_POINT('Ctrl Pts',(-3.31631129755346,17.7406985030951,
745.938235294118));
#144261=CARTESIAN_POINT('Ctrl Pts',(-1.67239348737615,18.048,744.444117647059));
#144262=CARTESIAN_POINT('Ctrl Pts',(-2.21024254310115E-15,18.048,742.95));
#144263=CARTESIAN_POINT('Origin',(0.,0.,0.));
#144264=CARTESIAN_POINT('',(2.57009189155355E-10,-15.0000000000002,1403.35000000055));
#144265=CARTESIAN_POINT('',(1.83781454274905E-15,-15.0000000000002,1436.290625));
#144266=CARTESIAN_POINT('',(-1.83697019872103E-15,-15.,-1.82952505755738E-15));
#144267=CARTESIAN_POINT('',(0.,-15.0000000000001,1504.95));
#144268=CARTESIAN_POINT('Ctrl Pts',(5.13986631034413E-10,-15.0000000000002,
1403.35000000055));
#144269=CARTESIAN_POINT('Ctrl Pts',(2.07827945901844,-14.9999999999289,
1405.58402534592));
#144270=CARTESIAN_POINT('Ctrl Pts',(4.13908692185227,-14.5684603429543,
1407.81020920318));
#144271=CARTESIAN_POINT('Ctrl Pts',(8.68689829398006,-12.5629931687572,
1413.17009322386));
#144272=CARTESIAN_POINT('Ctrl Pts',(10.9344652135011,-10.6646060820942,
1416.21094592123));
#144273=CARTESIAN_POINT('Ctrl Pts',(14.1072706803958,-5.85542612428411,
1422.42816851589));
#144274=CARTESIAN_POINT('Ctrl Pts',(14.9683604747762,-3.04195026298039,
1425.46607790158));
#144275=CARTESIAN_POINT('Ctrl Pts',(15.029933794911,2.72204213970847,1431.68856689381));
#144276=CARTESIAN_POINT('Ctrl Pts',(14.2291832910922,5.55329976428186,1434.72524170703));
#144277=CARTESIAN_POINT('Ctrl Pts',(11.1573566374657,10.4318055046907,1440.94870782112));
#144278=CARTESIAN_POINT('Ctrl Pts',(8.94969556395685,12.3777406823635,1443.98680513831));
#144279=CARTESIAN_POINT('Ctrl Pts',(3.72577049390288,14.8129297813082,1450.20684436425));
#144280=CARTESIAN_POINT('Ctrl Pts',(0.815546969962605,15.2523333509076,
1453.24820170673));
#144281=CARTESIAN_POINT('Ctrl Pts',(-4.89155833830842,14.4694790480348,
1459.46097488352));
#144282=CARTESIAN_POINT('Ctrl Pts',(-7.57588543252332,13.2625961079929,
1462.50715168045));
#144283=CARTESIAN_POINT('Ctrl Pts',(-11.9461394121487,9.51657316639935,
1468.70916033785));
#144284=CARTESIAN_POINT('Ctrl Pts',(-13.5495708516033,7.04921298326686,
1471.76148533607));
#144285=CARTESIAN_POINT('Ctrl Pts',(-15.1953740827798,1.53729692049363,
1477.95185674073));
#144286=CARTESIAN_POINT('Ctrl Pts',(-15.2079313081015,-1.40536021411593,
1481.01043271643));
#144287=CARTESIAN_POINT('Ctrl Pts',(-13.6115405479348,-6.92758911761814,
1487.19191578933));
#144288=CARTESIAN_POINT('Ctrl Pts',(-12.0318291094507,-9.40666760558364,
1490.2455169837));
#144289=CARTESIAN_POINT('Ctrl Pts',(-8.51254032736959,-12.4811631175375,
1495.2775465698));
#144290=CARTESIAN_POINT('Ctrl Pts',(-6.95318389069969,-13.4120759382215,
1497.21026935134));
#144291=CARTESIAN_POINT('Ctrl Pts',(-3.58613197332224,-14.6756940642514,
1501.07970655087));
#144292=CARTESIAN_POINT('Ctrl Pts',(-1.79915829322707,-15.0000000000001,
1503.01601310958));
#144293=CARTESIAN_POINT('Ctrl Pts',(-4.413136522885E-14,-15.0000000000002,
1504.95));
#144294=CARTESIAN_POINT('Origin',(0.,-1.83556249024732E-13,1504.95));
#144295=CARTESIAN_POINT('',(0.,-15.,1500.1875));
#144296=CARTESIAN_POINT('',(0.,-15.,1500.1875));
#144297=CARTESIAN_POINT('',(-6.31841207935097E-16,-15.0000000000002,1446.609375));
#144298=CARTESIAN_POINT('',(-1.83697019872103E-15,-15.,-1.82952505755738E-15));
#144299=CARTESIAN_POINT('Ctrl Pts',(1.31838984174237E-15,-15.0000000000002,
1436.290625));
#144300=CARTESIAN_POINT('Ctrl Pts',(0.65346443120896,-15.0000000000002,
1436.290625));
#144301=CARTESIAN_POINT('Ctrl Pts',(1.34693085135696,-14.9531257199513,
1436.42230514128));
#144302=CARTESIAN_POINT('Ctrl Pts',(2.61662608066102,-14.7838918918852,
1436.95053274143));
#144303=CARTESIAN_POINT('Ctrl Pts',(3.19325594296631,-14.6636670624435,
1437.3467978446));
#144304=CARTESIAN_POINT('Ctrl Pts',(4.10344327628912,-14.4354425556451,
1438.25698517792));
#144305=CARTESIAN_POINT('Ctrl Pts',(4.49952313800711,-14.3119470704814,
1438.8335196808));
#144306=CARTESIAN_POINT('Ctrl Pts',(5.02761209168826,-14.1350860668278,
1440.10285875835));
#144307=CARTESIAN_POINT('Ctrl Pts',(5.15937500000008,-14.0847736797358,
1440.79618925399));
#144308=CARTESIAN_POINT('Ctrl Pts',(5.15937500000008,-14.0847736797358,
1442.10381074602));
#144309=CARTESIAN_POINT('Ctrl Pts',(5.02761209168842,-14.1350860668278,
1442.79714124165));
#144310=CARTESIAN_POINT('Ctrl Pts',(4.49952313800732,-14.3119470704813,
1444.0664803192));
#144311=CARTESIAN_POINT('Ctrl Pts',(4.10344327628912,-14.4354425556451,
1444.64301482208));
#144312=CARTESIAN_POINT('Ctrl Pts',(3.19325594296631,-14.6636670624435,
1445.5532021554));
#144313=CARTESIAN_POINT('Ctrl Pts',(2.61662608066126,-14.7838918918852,
1445.94946725857));
#144314=CARTESIAN_POINT('Ctrl Pts',(1.34693085135724,-14.9531257199512,
1446.47769485872));
#144315=CARTESIAN_POINT('Ctrl Pts',(0.653464431208942,-15.0000000000002,
1446.609375));
#144316=CARTESIAN_POINT('Ctrl Pts',(-1.69309011255336E-14,-15.0000000000002,
1446.609375));
#144317=CARTESIAN_POINT('',(14.0847736797357,5.15937499999978,1492.25));
#144318=CARTESIAN_POINT('',(14.0847736797356,-5.15937500000027,1492.25));
#144319=CARTESIAN_POINT('Ctrl Pts',(14.0847736797357,5.15937499999978,1492.25));
#144320=CARTESIAN_POINT('Ctrl Pts',(14.0847736797357,5.15937499999977,1492.90381074601));
#144321=CARTESIAN_POINT('Ctrl Pts',(14.1350860668277,5.02761209168797,1493.59714124165));
#144322=CARTESIAN_POINT('Ctrl Pts',(14.3119470704813,4.49952313800681,1494.8664803192));
#144323=CARTESIAN_POINT('Ctrl Pts',(14.4354425556449,4.10344327628884,1495.44301482208));
#144324=CARTESIAN_POINT('Ctrl Pts',(14.6636670624433,3.19325594296603,1496.3532021554));
#144325=CARTESIAN_POINT('Ctrl Pts',(14.7838918918851,2.61662608066068,1496.74946725857));
#144326=CARTESIAN_POINT('Ctrl Pts',(14.9531257199511,1.34693085135664,1497.27769485872));
#144327=CARTESIAN_POINT('Ctrl Pts',(15.,0.653464431208711,1497.409375));
#144328=CARTESIAN_POINT('Ctrl Pts',(15.,-0.653464431209192,1497.409375));
#144329=CARTESIAN_POINT('Ctrl Pts',(14.9531257199511,-1.34693085135711,
1497.27769485872));
#144330=CARTESIAN_POINT('Ctrl Pts',(14.783891891885,-2.61662608066116,1496.74946725857));
#144331=CARTESIAN_POINT('Ctrl Pts',(14.6636670624433,-3.1932559429665,1496.3532021554));
#144332=CARTESIAN_POINT('Ctrl Pts',(14.4354425556449,-4.10344327628932,
1495.44301482208));
#144333=CARTESIAN_POINT('Ctrl Pts',(14.3119470704812,-4.49952313800728,
1494.8664803192));
#144334=CARTESIAN_POINT('Ctrl Pts',(14.1350860668277,-5.02761209168844,
1493.59714124165));
#144335=CARTESIAN_POINT('Ctrl Pts',(14.0847736797356,-5.15937500000027,
1492.90381074601));
#144336=CARTESIAN_POINT('Ctrl Pts',(14.0847736797356,-5.15937500000027,
1492.25));
#144337=CARTESIAN_POINT('Ctrl Pts',(14.0847736797356,-5.15937500000027,
1492.25));
#144338=CARTESIAN_POINT('Ctrl Pts',(14.0847736797356,-5.15937500000028,
1491.59618925398));
#144339=CARTESIAN_POINT('Ctrl Pts',(14.1350860668277,-5.02761209168844,
1490.90285875835));
#144340=CARTESIAN_POINT('Ctrl Pts',(14.3119470704812,-4.49952313800728,
1489.6335196808));
#144341=CARTESIAN_POINT('Ctrl Pts',(14.4354425556449,-4.10344327628932,
1489.05698517792));
#144342=CARTESIAN_POINT('Ctrl Pts',(14.6636670624433,-3.1932559429665,1488.1467978446));
#144343=CARTESIAN_POINT('Ctrl Pts',(14.783891891885,-2.61662608066116,1487.75053274143));
#144344=CARTESIAN_POINT('Ctrl Pts',(14.9531257199511,-1.34693085135711,
1487.22230514128));
#144345=CARTESIAN_POINT('Ctrl Pts',(15.,-0.653464431209191,1487.090625));
#144346=CARTESIAN_POINT('Ctrl Pts',(15.,0.65346443120871,1487.090625));
#144347=CARTESIAN_POINT('Ctrl Pts',(14.9531257199511,1.34693085135663,1487.22230514128));
#144348=CARTESIAN_POINT('Ctrl Pts',(14.7838918918851,2.61662608066068,1487.75053274143));
#144349=CARTESIAN_POINT('Ctrl Pts',(14.6636670624433,3.19325594296603,1488.1467978446));
#144350=CARTESIAN_POINT('Ctrl Pts',(14.4354425556449,4.10344327628884,1489.05698517792));
#144351=CARTESIAN_POINT('Ctrl Pts',(14.3119470704813,4.49952313800681,1489.6335196808));
#144352=CARTESIAN_POINT('Ctrl Pts',(14.1350860668277,5.02761209168797,1490.90285875835));
#144353=CARTESIAN_POINT('Ctrl Pts',(14.0847736797357,5.15937499999978,1491.59618925399));
#144354=CARTESIAN_POINT('Ctrl Pts',(14.0847736797357,5.15937499999978,1492.25));
#144355=CARTESIAN_POINT('',(-14.0847736797356,5.15937499999996,1492.25));
#144356=CARTESIAN_POINT('',(-14.0847736797357,-5.1593750000001,1492.25));
#144357=CARTESIAN_POINT('Ctrl Pts',(-14.0847736797356,5.15937499999994,
1492.25));
#144358=CARTESIAN_POINT('Ctrl Pts',(-14.0847736797356,5.15937499999995,
1491.59618925398));
#144359=CARTESIAN_POINT('Ctrl Pts',(-14.1350860668276,5.02761209168814,
1490.90285875835));
#144360=CARTESIAN_POINT('Ctrl Pts',(-14.3119470704812,4.49952313800698,
1489.6335196808));
#144361=CARTESIAN_POINT('Ctrl Pts',(-14.4354425556449,4.10344327628902,
1489.05698517792));
#144362=CARTESIAN_POINT('Ctrl Pts',(-14.6636670624433,3.1932559429662,1488.1467978446));
#144363=CARTESIAN_POINT('Ctrl Pts',(-14.783891891885,2.61662608066086,1487.75053274143));
#144364=CARTESIAN_POINT('Ctrl Pts',(-14.9531257199511,1.34693085135682,
1487.22230514128));
#144365=CARTESIAN_POINT('Ctrl Pts',(-15.,0.653464431208892,1487.090625));
#144366=CARTESIAN_POINT('Ctrl Pts',(-15.,-0.653464431209009,1487.090625));
#144367=CARTESIAN_POINT('Ctrl Pts',(-14.9531257199511,-1.34693085135693,
1487.22230514128));
#144368=CARTESIAN_POINT('Ctrl Pts',(-14.7838918918851,-2.61662608066098,
1487.75053274143));
#144369=CARTESIAN_POINT('Ctrl Pts',(-14.6636670624433,-3.19325594296632,
1488.1467978446));
#144370=CARTESIAN_POINT('Ctrl Pts',(-14.4354425556449,-4.10344327628914,
1489.05698517792));
#144371=CARTESIAN_POINT('Ctrl Pts',(-14.3119470704813,-4.49952313800711,
1489.6335196808));
#144372=CARTESIAN_POINT('Ctrl Pts',(-14.1350860668277,-5.02761209168827,
1490.90285875835));
#144373=CARTESIAN_POINT('Ctrl Pts',(-14.0847736797357,-5.15937500000011,
1491.59618925398));
#144374=CARTESIAN_POINT('Ctrl Pts',(-14.0847736797357,-5.1593750000001,
1492.25));
#144375=CARTESIAN_POINT('Ctrl Pts',(-14.0847736797357,-5.1593750000001,
1492.25));
#144376=CARTESIAN_POINT('Ctrl Pts',(-14.0847736797357,-5.15937500000009,
1492.90381074602));
#144377=CARTESIAN_POINT('Ctrl Pts',(-14.1350860668277,-5.02761209168827,
1493.59714124165));
#144378=CARTESIAN_POINT('Ctrl Pts',(-14.3119470704813,-4.49952313800711,
1494.8664803192));
#144379=CARTESIAN_POINT('Ctrl Pts',(-14.4354425556449,-4.10344327628914,
1495.44301482208));
#144380=CARTESIAN_POINT('Ctrl Pts',(-14.6636670624433,-3.19325594296633,
1496.3532021554));
#144381=CARTESIAN_POINT('Ctrl Pts',(-14.7838918918851,-2.61662608066098,
1496.74946725857));
#144382=CARTESIAN_POINT('Ctrl Pts',(-14.9531257199511,-1.34693085135693,
1497.27769485872));
#144383=CARTESIAN_POINT('Ctrl Pts',(-15.,-0.653464431209007,1497.409375));
#144384=CARTESIAN_POINT('Ctrl Pts',(-15.,0.653464431208894,1497.409375));
#144385=CARTESIAN_POINT('Ctrl Pts',(-14.9531257199511,1.34693085135682,
1497.27769485872));
#144386=CARTESIAN_POINT('Ctrl Pts',(-14.783891891885,2.61662608066086,1496.74946725857));
#144387=CARTESIAN_POINT('Ctrl Pts',(-14.6636670624433,3.1932559429662,1496.3532021554));
#144388=CARTESIAN_POINT('Ctrl Pts',(-14.4354425556449,4.10344327628902,
1495.44301482208));
#144389=CARTESIAN_POINT('Ctrl Pts',(-14.3119470704812,4.49952313800698,
1494.8664803192));
#144390=CARTESIAN_POINT('Ctrl Pts',(-14.1350860668276,5.02761209168814,
1493.59714124165));
#144391=CARTESIAN_POINT('Ctrl Pts',(-14.0847736797356,5.15937499999995,
1492.90381074601));
#144392=CARTESIAN_POINT('Ctrl Pts',(-14.0847736797356,5.15937499999995,
1492.25));
#144393=CARTESIAN_POINT('Origin',(0.,0.,0.));
#144394=CARTESIAN_POINT('',(5.36664099495454E-10,-15.0000000000002,1301.75000000115));
#144395=CARTESIAN_POINT('',(5.89150092069277E-11,-15.0000000000002,1398.58750000013));
#144396=CARTESIAN_POINT('',(-1.83697019872103E-15,-15.,-1.82952505755738E-15));
#144397=CARTESIAN_POINT('Ctrl Pts',(1.07339914734439E-9,-15.0000000000002,
1301.75000000115));
#144398=CARTESIAN_POINT('Ctrl Pts',(2.02543822040446,-14.9999999998552,
1303.92722419444));
#144399=CARTESIAN_POINT('Ctrl Pts',(4.03516631768684,-14.5900202019492,
1306.0994090624));
#144400=CARTESIAN_POINT('Ctrl Pts',(8.55354940935205,-12.6538998087048,
1311.3974852079));
#144401=CARTESIAN_POINT('Ctrl Pts',(10.8207722409004,-10.779571491316,1314.44081265877));
#144402=CARTESIAN_POINT('Ctrl Pts',(14.0433921586252,-6.00653378080796,
1320.65317208807));
#144403=CARTESIAN_POINT('Ctrl Pts',(14.9346560888454,-3.20260822987993,
1323.69264040189));
#144404=CARTESIAN_POINT('Ctrl Pts',(15.0584371310492,2.55890057198171,1329.91244823535));
#144405=CARTESIAN_POINT('Ctrl Pts',(14.2885008909213,5.39870928526927,1332.94964058359));
#144406=CARTESIAN_POINT('Ctrl Pts',(11.2699281285619,10.3101005421185,1339.17302602159));
#144407=CARTESIAN_POINT('Ctrl Pts',(9.08384366129597,12.2797340197557,1342.21000829538));
#144408=CARTESIAN_POINT('Ctrl Pts',(3.88567321836983,14.7719134699867,1348.4325824966));
#144409=CARTESIAN_POINT('Ctrl Pts',(0.980539852744524,15.2427566439719,
1351.47179820227));
#144410=CARTESIAN_POINT('Ctrl Pts',(-4.73667751952996,14.5211716925833,
1357.68933833136));
#144411=CARTESIAN_POINT('Ctrl Pts',(-7.43379822914247,13.3429445600174,
1360.73247180874));
#144412=CARTESIAN_POINT('Ctrl Pts',(-11.8458131267598,9.6417587937456,1366.94128753384));
#144413=CARTESIAN_POINT('Ctrl Pts',(-13.4750877044247,7.19090259561012,
1369.98980741048));
#144414=CARTESIAN_POINT('Ctrl Pts',(-15.1787035856865,1.69505586624364,
1376.18654827176));
#144415=CARTESIAN_POINT('Ctrl Pts',(-15.2225085183137,-1.24681598994607,
1379.24168501291));
#144416=CARTESIAN_POINT('Ctrl Pts',(-13.6819345669464,-6.78643951579951,
1385.42572949408));
#144417=CARTESIAN_POINT('Ctrl Pts',(-12.1270137088126,-9.28387784012087,
1388.48363239768));
#144418=CARTESIAN_POINT('Ctrl Pts',(-7.83615501145688,-13.1096904546586,
1394.66915124053));
#144419=CARTESIAN_POINT('Ctrl Pts',(-5.17881657278763,-14.3680357852792,
1397.72013525724));
#144420=CARTESIAN_POINT('Ctrl Pts',(-1.56277020429806,-14.9390998255564,
1401.66404994413));
#144421=CARTESIAN_POINT('Ctrl Pts',(-0.78204833489024,-15.000000000027,
1402.50934510429));
#144422=CARTESIAN_POINT('Ctrl Pts',(5.14190356959432E-10,-15.0000000000002,
1403.35000000055));
#144423=CARTESIAN_POINT('Ctrl Pts',(6.38378239159465E-15,-15.0000000000002,
1446.609375));
#144424=CARTESIAN_POINT('Ctrl Pts',(-0.653464431208952,-15.0000000000002,
1446.609375));
#144425=CARTESIAN_POINT('Ctrl Pts',(-1.34693085135696,-14.9531257199513,
1446.47769485872));
#144426=CARTESIAN_POINT('Ctrl Pts',(-2.61662608066102,-14.7838918918852,
1445.94946725857));
#144427=CARTESIAN_POINT('Ctrl Pts',(-3.19325594296631,-14.6636670624435,
1445.5532021554));
#144428=CARTESIAN_POINT('Ctrl Pts',(-4.10344327628912,-14.4354425556451,
1444.64301482208));
#144429=CARTESIAN_POINT('Ctrl Pts',(-4.49952313800711,-14.3119470704814,
1444.0664803192));
#144430=CARTESIAN_POINT('Ctrl Pts',(-5.02761209168826,-14.1350860668278,
1442.79714124165));
#144431=CARTESIAN_POINT('Ctrl Pts',(-5.15937500000008,-14.0847736797358,
1442.10381074602));
#144432=CARTESIAN_POINT('Ctrl Pts',(-5.15937500000008,-14.0847736797358,
1441.45));
#144433=CARTESIAN_POINT('Ctrl Pts',(-5.15937500000008,-14.0847736797358,
1440.79618925399));
#144434=CARTESIAN_POINT('Ctrl Pts',(-5.02761209168826,-14.1350860668278,
1440.10285875835));
#144435=CARTESIAN_POINT('Ctrl Pts',(-4.49952313800711,-14.3119470704814,
1438.8335196808));
#144436=CARTESIAN_POINT('Ctrl Pts',(-4.10344327628912,-14.4354425556451,
1438.25698517792));
#144437=CARTESIAN_POINT('Ctrl Pts',(-3.19325594296631,-14.6636670624435,
1437.3467978446));
#144438=CARTESIAN_POINT('Ctrl Pts',(-2.61662608066102,-14.7838918918852,
1436.95053274143));
#144439=CARTESIAN_POINT('Ctrl Pts',(-1.34693085135696,-14.9531257199513,
1436.42230514128));
#144440=CARTESIAN_POINT('Ctrl Pts',(-0.653464431208967,-15.0000000000002,
1436.290625));
#144441=CARTESIAN_POINT('Ctrl Pts',(-8.88178419700125E-15,-15.0000000000002,
1436.290625));
#144442=CARTESIAN_POINT('Ctrl Pts',(-3.21964677141295E-14,-15.0000000000002,
1500.1875));
#144443=CARTESIAN_POINT('Ctrl Pts',(-1.76742229229486,-15.0000000000002,
1498.28762740068));
#144444=CARTESIAN_POINT('Ctrl Pts',(-3.52305311160152,-14.6871041937304,
1496.38607439147));
#144445=CARTESIAN_POINT('Ctrl Pts',(-6.83900014078546,-13.4665430518641,
1492.58242152618));
#144446=CARTESIAN_POINT('Ctrl Pts',(-8.37850025940737,-12.5669392521719,
1490.68632496464));
#144447=CARTESIAN_POINT('Ctrl Pts',(-11.9141329007694,-9.5562284284336,
1485.68171169807));
#144448=CARTESIAN_POINT('Ctrl Pts',(-13.5248067380123,-7.09592658651337,
1482.63269613729));
#144449=CARTESIAN_POINT('Ctrl Pts',(-15.1894805082896,-1.59255519695219,
1476.44356712209));
#144450=CARTESIAN_POINT('Ctrl Pts',(-15.2127708569242,1.34762269085022,
1473.38707582416));
#144451=CARTESIAN_POINT('Ctrl Pts',(-13.6380720372901,6.87605632801695,
1467.2078061325));
#144452=CARTESIAN_POINT('Ctrl Pts',(-12.0663282125807,9.36278073914447,
1464.15025536866));
#144453=CARTESIAN_POINT('Ctrl Pts',(-7.74812761957123,13.1624797736,1457.95817034909));
#144454=CARTESIAN_POINT('Ctrl Pts',(-5.08002271936798,14.4039629815762,
1454.90758866529));
#144455=CARTESIAN_POINT('Ctrl Pts',(0.613086311585234,15.2616144348726,
1448.70241026148));
#144456=CARTESIAN_POINT('Ctrl Pts',(3.52888509754822,14.860811034796,1445.65764851361));
#144457=CARTESIAN_POINT('Ctrl Pts',(8.78291544086862,12.4964470149111,1439.44259712957));
#144458=CARTESIAN_POINT('Ctrl Pts',(11.0166930867714,10.580104205331,1436.40226353964));
#144459=CARTESIAN_POINT('Ctrl Pts',(14.1532167714079,5.74397732306138,1430.18092697203));
#144460=CARTESIAN_POINT('Ctrl Pts',(14.9921131886098,2.92336609792222,1427.14340515978));
#144461=CARTESIAN_POINT('Ctrl Pts',(15.0077755460274,-2.84165960585207,
1420.91980067256));
#144462=CARTESIAN_POINT('Ctrl Pts',(14.1844363389502,-5.66644694002087,
1417.8829764111));
#144463=CARTESIAN_POINT('Ctrl Pts',(11.0746670298407,-10.519278170437,1411.66151250116));
#144464=CARTESIAN_POINT('Ctrl Pts',(8.85220915139545,-12.4473699157053,
1408.62298180108));
#144465=CARTESIAN_POINT('Ctrl Pts',(4.26917589575086,-14.5406277074722,
1403.18681607211));
#144466=CARTESIAN_POINT('Ctrl Pts',(2.1447555437566,-14.9999999999999,1400.89298313642));
#144467=CARTESIAN_POINT('Ctrl Pts',(1.17759552109575E-10,-15.0000000000001,
1398.58750000013));
#144468=CARTESIAN_POINT('',(-8.4434420636672E-19,14.9999999999998,1436.290625));
#144469=CARTESIAN_POINT('',(-6.31841207935097E-16,14.9999999999998,1446.609375));
#144470=CARTESIAN_POINT('Ctrl Pts',(-8.46545056276682E-15,14.9999999999998,
1436.290625));
#144471=CARTESIAN_POINT('Ctrl Pts',(-0.653464431208967,14.9999999999998,
1436.290625));
#144472=CARTESIAN_POINT('Ctrl Pts',(-1.34693085135696,14.9531257199509,
1436.42230514128));
#144473=CARTESIAN_POINT('Ctrl Pts',(-2.61662608066102,14.7838918918849,
1436.95053274143));
#144474=CARTESIAN_POINT('Ctrl Pts',(-3.19325594296631,14.6636670624431,
1437.3467978446));
#144475=CARTESIAN_POINT('Ctrl Pts',(-4.10344327628912,14.4354425556447,
1438.25698517792));
#144476=CARTESIAN_POINT('Ctrl Pts',(-4.49952313800711,14.3119470704811,
1438.8335196808));
#144477=CARTESIAN_POINT('Ctrl Pts',(-5.02761209168826,14.1350860668275,
1440.10285875835));
#144478=CARTESIAN_POINT('Ctrl Pts',(-5.15937500000008,14.0847736797355,
1440.79618925399));
#144479=CARTESIAN_POINT('Ctrl Pts',(-5.15937500000008,14.0847736797355,
1441.45));
#144480=CARTESIAN_POINT('Ctrl Pts',(-5.15937500000008,14.0847736797355,
1442.10381074602));
#144481=CARTESIAN_POINT('Ctrl Pts',(-5.02761209168826,14.1350860668275,
1442.79714124165));
#144482=CARTESIAN_POINT('Ctrl Pts',(-4.49952313800711,14.3119470704811,
1444.0664803192));
#144483=CARTESIAN_POINT('Ctrl Pts',(-4.10344327628912,14.4354425556447,
1444.64301482208));
#144484=CARTESIAN_POINT('Ctrl Pts',(-3.19325594296631,14.6636670624431,
1445.5532021554));
#144485=CARTESIAN_POINT('Ctrl Pts',(-2.61662608066101,14.7838918918849,
1445.94946725857));
#144486=CARTESIAN_POINT('Ctrl Pts',(-1.34693085135696,14.9531257199509,
1446.47769485872));
#144487=CARTESIAN_POINT('Ctrl Pts',(-0.653464431208951,14.9999999999998,
1446.609375));
#144488=CARTESIAN_POINT('Ctrl Pts',(6.24500451351651E-15,14.9999999999998,
1446.609375));
#144489=CARTESIAN_POINT('Ctrl Pts',(7.63278329429795E-16,14.9999999999998,
1446.609375));
#144490=CARTESIAN_POINT('Ctrl Pts',(0.65346443120896,14.9999999999998,1446.609375));
#144491=CARTESIAN_POINT('Ctrl Pts',(1.34693085135724,14.9531257199509,1446.47769485872));
#144492=CARTESIAN_POINT('Ctrl Pts',(2.61662608066126,14.7838918918848,1445.94946725857));
#144493=CARTESIAN_POINT('Ctrl Pts',(3.19325594296631,14.6636670624431,1445.5532021554));
#144494=CARTESIAN_POINT('Ctrl Pts',(4.10344327628912,14.4354425556447,1444.64301482208));
#144495=CARTESIAN_POINT('Ctrl Pts',(4.49952313800732,14.311947070481,1444.0664803192));
#144496=CARTESIAN_POINT('Ctrl Pts',(5.02761209168842,14.1350860668274,1442.79714124165));
#144497=CARTESIAN_POINT('Ctrl Pts',(5.15937500000008,14.0847736797355,1442.10381074602));
#144498=CARTESIAN_POINT('Ctrl Pts',(5.15937500000008,14.0847736797355,1440.79618925399));
#144499=CARTESIAN_POINT('Ctrl Pts',(5.02761209168819,14.1350860668275,1440.10285875835));
#144500=CARTESIAN_POINT('Ctrl Pts',(4.49952313800696,14.3119470704811,1438.8335196808));
#144501=CARTESIAN_POINT('Ctrl Pts',(4.10344327628912,14.4354425556447,1438.25698517792));
#144502=CARTESIAN_POINT('Ctrl Pts',(3.19325594296631,14.6636670624431,1437.3467978446));
#144503=CARTESIAN_POINT('Ctrl Pts',(2.61662608066102,14.7838918918849,1436.95053274143));
#144504=CARTESIAN_POINT('Ctrl Pts',(1.34693085135696,14.9531257199509,1436.42230514128));
#144505=CARTESIAN_POINT('Ctrl Pts',(0.653464431208971,14.9999999999998,
1436.290625));
#144506=CARTESIAN_POINT('Ctrl Pts',(1.2490009027033E-14,14.9999999999998,
1436.290625));
#144507=CARTESIAN_POINT('Origin',(0.,0.,0.));
#144508=CARTESIAN_POINT('',(8.79825987290161E-10,-15.0000000000001,1200.15000000189));
#144509=CARTESIAN_POINT('',(2.06320846743069E-10,-15.0000000000002,1296.98750000044));
#144510=CARTESIAN_POINT('',(-1.83697019872103E-15,-15.,-1.82952505755738E-15));
#144511=CARTESIAN_POINT('Ctrl Pts',(1.75979453231889E-9,-15.0000000000001,
1200.15000000189));
#144512=CARTESIAN_POINT('Ctrl Pts',(1.97399358436651,-14.9999999997686,
1202.27192430669));
#144513=CARTESIAN_POINT('Ctrl Pts',(3.93352370368442,-14.6105361002977,
1204.39131264898));
#144514=CARTESIAN_POINT('Ctrl Pts',(8.42209926513274,-12.7415093717001,
1209.62829861148));
#144515=CARTESIAN_POINT('Ctrl Pts',(10.708157128334,-10.8909829112263,1212.67455397258));
#144516=CARTESIAN_POINT('Ctrl Pts',(13.9790171867833,-6.15435157868962,
1218.88091311306));
#144517=CARTESIAN_POINT('Ctrl Pts',(14.8997625697908,-3.36022939188954,
1221.92248126964));
#144518=CARTESIAN_POINT('Ctrl Pts',(15.0847894150078,2.39760634805479,1228.13832386759));
#144519=CARTESIAN_POINT('Ctrl Pts',(14.3453595870873,5.2454463407763,1231.17665534719));
#144520=CARTESIAN_POINT('Ctrl Pts',(11.3801811105094,10.1881713863212,1237.39845607226));
#144521=CARTESIAN_POINT('Ctrl Pts',(9.21562980893118,12.1811613315997,1240.43522159905));
#144522=CARTESIAN_POINT('Ctrl Pts',(4.04428599820379,14.7293316556033,1246.65881387988));
#144523=CARTESIAN_POINT('Ctrl Pts',(1.14467164290646,15.2314208312659,1249.69649554128));
#144524=CARTESIAN_POINT('Ctrl Pts',(-4.58141563311257,14.5710755535568,
1255.91747033129));
#144525=CARTESIAN_POINT('Ctrl Pts',(-7.29089458762112,13.4217383032652,
1258.95810002799));
#144526=CARTESIAN_POINT('Ctrl Pts',(-11.7438326680798,9.76617145395712,
1265.17249253716));
#144527=CARTESIAN_POINT('Ctrl Pts',(-13.398827027713,7.33236029579112,1268.2176697433));
#144528=CARTESIAN_POINT('Ctrl Pts',(-15.1608221842952,1.85167160060532,
1274.42191838725));
#144529=CARTESIAN_POINT('Ctrl Pts',(-15.2346745109395,-1.09014303455582,
1277.47301604798));
#144530=CARTESIAN_POINT('Ctrl Pts',(-13.7499080930685,-6.64897693704802,
1283.66637557301));
#144531=CARTESIAN_POINT('Ctrl Pts',(-12.2192777208826,-9.16225557399221,
1286.72502342585));
#144532=CARTESIAN_POINT('Ctrl Pts',(-7.96708294002146,-13.0303297743241,
1292.90472764945));
#144533=CARTESIAN_POINT('Ctrl Pts',(-5.32321122148986,-14.3146286300458,
1295.95959992813));
#144534=CARTESIAN_POINT('Ctrl Pts',(-1.66486260240058,-14.9308817487195,
1299.95348817526));
#144535=CARTESIAN_POINT('Ctrl Pts',(-0.833320165543613,-15.0000000000598,
1300.85423097193));
#144536=CARTESIAN_POINT('Ctrl Pts',(1.07344951901075E-9,-15.0000000000002,
1301.75000000115));
#144537=CARTESIAN_POINT('Ctrl Pts',(1.17824847101211E-10,-15.0000000000002,
1398.58750000013));
#144538=CARTESIAN_POINT('Ctrl Pts',(-0.71771403817806,-15.0000000000003,
1397.81600060157));
#144539=CARTESIAN_POINT('Ctrl Pts',(-1.43458366106872,-14.9486793604924,
1397.04029696054));
#144540=CARTESIAN_POINT('Ctrl Pts',(-4.99620392819751,-14.4331061176049,
1393.16041437585));
#144541=CARTESIAN_POINT('Ctrl Pts',(-7.66995212336838,-13.2079060285185,
1390.11373050036));
#144542=CARTESIAN_POINT('Ctrl Pts',(-12.0093941122352,-9.43548920412243,
1383.92109513407));
#144543=CARTESIAN_POINT('Ctrl Pts',(-13.5950655942685,-6.95995628694869,
1380.86842290804));
#144544=CARTESIAN_POINT('Ctrl Pts',(-15.2045078947381,-1.44150614914692,
1374.68565391779));
#144545=CARTESIAN_POINT('Ctrl Pts',(-15.1988282304223,1.50118033788765,
1371.62706038024));
#144546=CARTESIAN_POINT('Ctrl Pts',(-13.5667033566612,7.0161084865984,1365.43899111184));
#144547=CARTESIAN_POINT('Ctrl Pts',(-11.9693212941103,9.48724026705885,
1362.38571456362));
#144548=CARTESIAN_POINT('Ctrl Pts',(-7.60893334399002,13.2436188010555,
1356.185468396));
#144549=CARTESIAN_POINT('Ctrl Pts',(-4.92765696827631,14.4571536279501,
1353.1385064468));
#144550=CARTESIAN_POINT('Ctrl Pts',(0.77691088707214,15.2543139944877,1346.92703588305));
#144551=CARTESIAN_POINT('Ctrl Pts',(3.68825684256168,14.8222754834421,1343.88509349636));
#144552=CARTESIAN_POINT('Ctrl Pts',(8.91805348489406,12.4005263563624,1337.66584740671));
#144553=CARTESIAN_POINT('Ctrl Pts',(11.130730801771,10.4601942654857,1334.62739603187));
#144554=CARTESIAN_POINT('Ctrl Pts',(14.2149626350962,5.58959776446285,1328.40413944157));
#144555=CARTESIAN_POINT('Ctrl Pts',(15.0229610734552,2.7603694750373,1325.36744297579));
#144556=CARTESIAN_POINT('Ctrl Pts',(14.9760496486665,-3.00400024173918,
1319.14454665604));
#144557=CARTESIAN_POINT('Ctrl Pts',(14.1221027053062,-5.81966903139119,
1316.1069172253));
#144558=CARTESIAN_POINT('Ctrl Pts',(10.9611608397889,-10.6372410828221,
1309.88873413739));
#144559=CARTESIAN_POINT('Ctrl Pts',(8.71830137524085,-12.5412811976424,
1306.84838787216));
#144560=CARTESIAN_POINT('Ctrl Pts',(4.16368759723579,-14.5632693044744,
1301.47398043358));
#144561=CARTESIAN_POINT('Ctrl Pts',(2.09082327762966,-14.9999999999426,
1299.23500919603));
#144562=CARTESIAN_POINT('Ctrl Pts',(4.12767042767825E-10,-15.0000000000002,
1296.98750000044));
#144563=CARTESIAN_POINT('Origin',(0.,0.,0.));
#144564=CARTESIAN_POINT('',(9.52135784329144E-10,-15.0000000000001,1098.55000000205));
#144565=CARTESIAN_POINT('',(4.61706142986984E-10,-15.0000000000001,1195.38750000099));
#144566=CARTESIAN_POINT('',(-1.83697019872103E-15,-15.,-1.82952505755738E-15));
#144567=CARTESIAN_POINT('Ctrl Pts',(1.90432308810884E-9,-15.0000000000001,
1098.55000000205));
#144568=CARTESIAN_POINT('Ctrl Pts',(1.92202320191745,-14.9999999997561,
1100.61605927318));
#144569=CARTESIAN_POINT('Ctrl Pts',(3.83162991280002,-14.6307194546823,
1102.68313352437));
#144570=CARTESIAN_POINT('Ctrl Pts',(8.29048688497464,-12.8272881628003,
1107.85983619282));
#144571=CARTESIAN_POINT('Ctrl Pts',(10.5948484305959,-11.0006774132446,
1110.90947698597));
#144572=CARTESIAN_POINT('Ctrl Pts',(13.9131826583481,-6.30124214664866,
1117.10867571733));
#144573=CARTESIAN_POINT('Ctrl Pts',(14.8631643120297,-3.51733684258962,
1120.15287671185));
#144574=CARTESIAN_POINT('Ctrl Pts',(15.1094439039152,2.23563536119488,1126.36346890381));
#144575=CARTESIAN_POINT('Ctrl Pts',(14.4006802897054,5.09109066860144,1129.40354120608));
#144576=CARTESIAN_POINT('Ctrl Pts',(11.4898658308363,10.064093992546,1135.62223731496));
#144577=CARTESIAN_POINT('Ctrl Pts',(9.34710505755872,12.0804849622448,1138.65972306586));
#144578=CARTESIAN_POINT('Ctrl Pts',(4.20410894919187,14.6845033463582,1144.88279479004));
#144579=CARTESIAN_POINT('Ctrl Pts',(1.31050196415145,15.218120096428,1147.91956278325));
#144580=CARTESIAN_POINT('Ctrl Pts',(-4.42330682574351,14.6199503152763,
1154.14264456888));
#144581=CARTESIAN_POINT('Ctrl Pts',(-7.14491054562634,13.5001672047438,
1157.18131185169));
#144582=CARTESIAN_POINT('Ctrl Pts',(-11.6385345751432,9.8917585283482,1163.40007537353));
#144583=CARTESIAN_POINT('Ctrl Pts',(-13.3195217540098,7.47578682138226,
1166.44236284484));
#144584=CARTESIAN_POINT('Ctrl Pts',(-15.1407775212644,2.01164521892566,
1172.65306468181));
#144585=CARTESIAN_POINT('Ctrl Pts',(-15.2454755863158,-0.929573713222222,
1175.70048315408));
#144586=CARTESIAN_POINT('Ctrl Pts',(-13.8187694358849,-6.50478376461115,
1181.89970327795));
#144587=CARTESIAN_POINT('Ctrl Pts',(-12.315292405085,-9.03405822125963,
1184.95352856043));
#144588=CARTESIAN_POINT('Ctrl Pts',(-8.10107486955481,-12.9471147882967,
1191.14027521031));
#144589=CARTESIAN_POINT('Ctrl Pts',(-5.46767650788743,-14.2603922672436,
1194.19890607217));
#144590=CARTESIAN_POINT('Ctrl Pts',(-1.76443889312882,-14.922363100848,
1198.24560113117));
#144591=CARTESIAN_POINT('Ctrl Pts',(-0.883351399577367,-15.0000000001038,
1199.20045040626));
#144592=CARTESIAN_POINT('Ctrl Pts',(1.75977386471601E-9,-15.0000000000001,
1200.15000000189));
#144593=CARTESIAN_POINT('Ctrl Pts',(4.12697515050908E-10,-15.0000000000002,
1296.98750000044));
#144594=CARTESIAN_POINT('Ctrl Pts',(-0.769894768051591,-15.0000000000213,
1296.15990945723));
#144595=CARTESIAN_POINT('Ctrl Pts',(-1.53856172628175,-14.9409719495836,
1295.32775907935));
#144596=CARTESIAN_POINT('Ctrl Pts',(-5.14443979608549,-14.380495004843,
1291.39582925936));
#144597=CARTESIAN_POINT('Ctrl Pts',(-7.80491977416643,-13.1283632101541,
1288.34570821307));
#144598=CARTESIAN_POINT('Ctrl Pts',(-12.105104901342,-9.31246842067276,
1282.15860694432));
#144599=CARTESIAN_POINT('Ctrl Pts',(-13.6654892130908,-6.81929030932275,
1279.10135175935));
#144600=CARTESIAN_POINT('Ctrl Pts',(-15.2193804718104,-1.28406273702655,
1272.91933040514));
#144601=CARTESIAN_POINT('Ctrl Pts',(-15.1827094895822,1.65774377668617,
1269.86317053524));
#144602=CARTESIAN_POINT('Ctrl Pts',(-13.4930535609753,7.15705228474937,
1263.66838894451));
#144603=CARTESIAN_POINT('Ctrl Pts',(-11.8699457523811,9.61190395378373,
1260.61900038051));
#144604=CARTESIAN_POINT('Ctrl Pts',(-7.46783838915637,13.3238782986591,
1254.41170121311));
#144605=CARTESIAN_POINT('Ctrl Pts',(-4.77373574858607,14.5089779731568,
1251.36788828749));
#144606=CARTESIAN_POINT('Ctrl Pts',(0.941176728315708,15.2452064662291,
1245.15136717061));
#144607=CARTESIAN_POINT('Ctrl Pts',(3.84756728011627,14.7818617551212,1242.11169395613));
#144608=CARTESIAN_POINT('Ctrl Pts',(9.05198286843481,12.3032191192182,1235.88959848178));
#144609=CARTESIAN_POINT('Ctrl Pts',(11.2432367200937,10.3392060353596,1232.852409349));
#144610=CARTESIAN_POINT('Ctrl Pts',(14.2745479122127,5.43554174545849,1226.62887674805));
#144611=CARTESIAN_POINT('Ctrl Pts',(15.0518224439408,2.59773028908131,1223.59186666104));
#144612=CARTESIAN_POINT('Ctrl Pts',(14.9428235958911,-3.16448362300977,
1217.37129762939));
#144613=CARTESIAN_POINT('Ctrl Pts',(14.0587097698017,-5.97071514542203,
1214.33225324628));
#144614=CARTESIAN_POINT('Ctrl Pts',(10.8478515048654,-10.7524187323543,
1208.11862409471));
#144615=CARTESIAN_POINT('Ctrl Pts',(8.5852522919524,-12.6324748082145,1205.07593148621));
#144616=CARTESIAN_POINT('Ctrl Pts',(4.05979577078787,-14.5849641361676,
1199.76314315456));
#144617=CARTESIAN_POINT('Ctrl Pts',(2.0379397774467,-14.9999999998747,1197.57816261591));
#144618=CARTESIAN_POINT('Ctrl Pts',(9.23458105710732E-10,-15.0000000000001,
1195.38750000099));
#144619=CARTESIAN_POINT('Origin',(0.,0.,0.));
#144620=CARTESIAN_POINT('',(1.12804740017511E-11,-15.0000000000001,996.950000000024));
#144621=CARTESIAN_POINT('',(8.43148104337132E-10,-15.0000000000001,1093.78750000181));
#144622=CARTESIAN_POINT('',(-1.83697019872103E-15,-15.,-1.82952505755738E-15));
#144623=CARTESIAN_POINT('Ctrl Pts',(2.24431584427975E-11,-15.0000000000001,
996.950000000024));
#144624=CARTESIAN_POINT('Ctrl Pts',(1.8730160222366,-15.0000000000001,998.963379504291));
#144625=CARTESIAN_POINT('Ctrl Pts',(3.73260476096043,-14.6497110398557,
1000.97830003658));
#144626=CARTESIAN_POINT('Ctrl Pts',(8.16125115437788,-12.9096787385466,
1006.09530088561));
#144627=CARTESIAN_POINT('Ctrl Pts',(10.4830299559481,-11.1066322977705,
1009.14867930291));
#144628=CARTESIAN_POINT('Ctrl Pts',(13.8472105025231,-6.44441945178535,
1015.33976831645));
#144629=CARTESIAN_POINT('Ctrl Pts',(14.8256060144153,-3.67095044645471,
1018.38704391883));
#144630=CARTESIAN_POINT('Ctrl Pts',(15.1319727650807,2.07612182853235,1024.59126687234));
#144631=CARTESIAN_POINT('Ctrl Pts',(14.4534309549069,4.9386110172691,1027.633609537));
#144632=CARTESIAN_POINT('Ctrl Pts',(11.5968074887327,9.94040367199438,1033.84793273401));
#144633=CARTESIAN_POINT('Ctrl Pts',(9.47586063211703,11.9795942956902,1036.8867496228));
#144634=CARTESIAN_POINT('Ctrl Pts',(4.36222498638682,14.6382077696174,1043.10771916763));
#144635=CARTESIAN_POINT('Ctrl Pts',(1.47462240033404,15.2030775705206,1046.14464154482));
#144636=CARTESIAN_POINT('Ctrl Pts',(-4.26538892408494,14.6668340844614,
1052.3682223371));
#144637=CARTESIAN_POINT('Ctrl Pts',(-6.99866059986271,13.576672237868,1055.40554621383));
#144638=CARTESIAN_POINT('Ctrl Pts',(-11.5319057810387,10.0160832097434,
1061.62733309336));
#144639=CARTESIAN_POINT('Ctrl Pts',(-13.2386493056426,7.61838119872912,
1064.66728246334));
#144640=CARTESIAN_POINT('Ctrl Pts',(-15.1188894104588,2.17192003957943,
1070.8831888708));
#144641=CARTESIAN_POINT('Ctrl Pts',(-15.2546242876952,-0.768179479350522,
1073.92740266756));
#144642=CARTESIAN_POINT('Ctrl Pts',(-13.8859768100344,-6.36101200390849,
1080.13380626064));
#144643=CARTESIAN_POINT('Ctrl Pts',(-12.4083713615784,-8.90603998351183,
1083.18370155585));
#144644=CARTESIAN_POINT('Ctrl Pts',(-8.2334486591165,-12.8635554275619,
1089.37733866998));
#144645=CARTESIAN_POINT('Ctrl Pts',(-5.61463438468432,-14.2040034671046,
1092.4340911989));
#144646=CARTESIAN_POINT('Ctrl Pts',(-1.86492777684583,-14.9132117530754,
1096.53706165363));
#144647=CARTESIAN_POINT('Ctrl Pts',(-0.933904123582952,-15.0000000001187,
1097.54610927026));
#144648=CARTESIAN_POINT('Ctrl Pts',(1.90427969863687E-9,-15.0000000000001,
1098.55000000205));
#144649=CARTESIAN_POINT('Ctrl Pts',(9.23458105710732E-10,-15.0000000000001,
1195.38750000099));
#144650=CARTESIAN_POINT('Ctrl Pts',(-0.821178976272775,-15.0000000000507,
1194.50478201972));
#144651=CARTESIAN_POINT('Ctrl Pts',(-1.64069188092298,-14.9328745854408,
1193.6171687484));
#144652=CARTESIAN_POINT('Ctrl Pts',(-5.28911085923903,-14.327398555011,
1189.63502775005));
#144653=CARTESIAN_POINT('Ctrl Pts',(-7.93620275077505,-13.049206807507,
1186.58111164689));
#144654=CARTESIAN_POINT('Ctrl Pts',(-12.1975161535311,-9.1911476248741,
1180.4000672537));
#144655=CARTESIAN_POINT('Ctrl Pts',(-13.7339933049332,-6.68144215564515,
1177.34148343405));
#144656=CARTESIAN_POINT('Ctrl Pts',(-15.2319436817764,-1.12717518048759,
1171.1503549189));
#144657=CARTESIAN_POINT('Ctrl Pts',(-15.1651986962582,1.81470064774139,
1168.09834177543));
#144658=CARTESIAN_POINT('Ctrl Pts',(-13.4169527219817,7.29905964381786,
1161.89576029855));
#144659=CARTESIAN_POINT('Ctrl Pts',(-11.7680056471831,9.7369333162655,1158.84983893944));
#144660=CARTESIAN_POINT('Ctrl Pts',(-7.32463102653318,13.4033178858974,
1152.63664761051));
#144661=CARTESIAN_POINT('Ctrl Pts',(-4.61802494538421,14.5594801028764,
1149.59547813664));
#144662=CARTESIAN_POINT('Ctrl Pts',(1.10608557067634,15.2342487988229,1143.37519155904));
#144663=CARTESIAN_POINT('Ctrl Pts',(4.00703668296603,14.7395020205243,1140.33720438905));
#144664=CARTESIAN_POINT('Ctrl Pts',(9.18481444702779,12.2044224110096,1134.11369371611));
#144665=CARTESIAN_POINT('Ctrl Pts',(11.3544041109852,10.2169309128655,1131.07700218978));
#144666=CARTESIAN_POINT('Ctrl Pts',(14.3321826275215,5.2814322920117,1124.85467352815));
#144667=CARTESIAN_POINT('Ctrl Pts',(15.0787707297665,2.43543683555569,1121.81666357999));
#144668=CARTESIAN_POINT('Ctrl Pts',(14.9080518871194,-3.32452031727013,
1115.59853082145));
#144669=CARTESIAN_POINT('Ctrl Pts',(13.9934828338927,-6.12205439404753,
1112.55627793874));
#144670=CARTESIAN_POINT('Ctrl Pts',(10.7312074299843,-10.868816474941,1106.34549903581));
#144671=CARTESIAN_POINT('Ctrl Pts',(8.44741452093267,-12.7251674847629,
1103.29812611831));
#144672=CARTESIAN_POINT('Ctrl Pts',(3.95184186519944,-14.6068799135907,
1098.04827409019));
#144673=CARTESIAN_POINT('Ctrl Pts',(1.98322361516975,-14.9999999997772,
1095.91934603433));
#144674=CARTESIAN_POINT('Ctrl Pts',(1.68617259044268E-9,-15.0000000000001,
1093.78750000181));
#144675=CARTESIAN_POINT('Origin',(0.,0.,0.));
#144676=CARTESIAN_POINT('',(-3.39412889236257E-10,-15.0000000000001,895.34999999927));
#144677=CARTESIAN_POINT('',(1.18621812117655E-9,-15.0000000000001,992.18750000255));
#144678=CARTESIAN_POINT('',(-1.83697019872103E-15,-15.,-1.82952505755738E-15));
#144679=CARTESIAN_POINT('Ctrl Pts',(-6.78717360091952E-10,-15.0000000000001,
895.34999999927));
#144680=CARTESIAN_POINT('Ctrl Pts',(1.81530776265467,-15.0000000000822,
897.301346598161));
#144681=CARTESIAN_POINT('Ctrl Pts',(3.61819325598204,-14.6713763119832,
899.254859370096));
#144682=CARTESIAN_POINT('Ctrl Pts',(8.01267924322565,-13.0019991669338,
904.310990328089));
#144683=CARTESIAN_POINT('Ctrl Pts',(10.3575355933915,-11.2240553804396,
907.369583455908));
#144684=CARTESIAN_POINT('Ctrl Pts',(13.7748779118175,-6.59802740400891,
913.557672489966));
#144685=CARTESIAN_POINT('Ctrl Pts',(14.7841893814279,-3.83407757460096,
916.610940848539));
#144686=CARTESIAN_POINT('Ctrl Pts',(15.1540025554497,1.90932507552399,922.811202277));
#144687=CARTESIAN_POINT('Ctrl Pts',(14.5065334548264,4.78033466882151,925.858157433005));
#144688=CARTESIAN_POINT('Ctrl Pts',(11.7048007290421,9.81301866781119,932.069639374599));
#144689=CARTESIAN_POINT('Ctrl Pts',(9.60550431941437,11.8759162278827,935.111576652667));
#144690=CARTESIAN_POINT('Ctrl Pts',(4.52118877587782,14.5898454704389,941.33082980798));
#144691=CARTESIAN_POINT('Ctrl Pts',(1.63932192043573,15.1862259714449,944.369278023895));
#144692=CARTESIAN_POINT('Ctrl Pts',(-4.10612417080342,14.7121834621567,
950.592505158305));
#144693=CARTESIAN_POINT('Ctrl Pts',(-6.85077495090437,13.6519489150702,
953.629170558023));
#144694=CARTESIAN_POINT('Ctrl Pts',(-11.4229070225234,10.1403302346103,
959.85259962067));
#144695=CARTESIAN_POINT('Ctrl Pts',(-13.155411596351,7.76147412577686,962.890777822469));
#144696=CARTESIAN_POINT('Ctrl Pts',(-15.0949074247572,2.33404345680181,
969.110635615743));
#144697=CARTESIAN_POINT('Ctrl Pts',(-15.2621496783219,-0.604415026600302,
972.152129000351));
#144698=CARTESIAN_POINT('Ctrl Pts',(-13.9527222770561,-6.21403477228019,
978.364599340677));
#144699=CARTESIAN_POINT('Ctrl Pts',(-12.5018017555402,-8.77468893311663,
981.410960060362));
#144700=CARTESIAN_POINT('Ctrl Pts',(-8.36628607719189,-12.7781047944913,
987.612556095191));
#144701=CARTESIAN_POINT('Ctrl Pts',(-5.76074314579896,-14.145524343791,
990.665104924394));
#144702=CARTESIAN_POINT('Ctrl Pts',(-1.9673848809929,-14.903369644354,994.8277692865));
#144703=CARTESIAN_POINT('Ctrl Pts',(-0.984787905444944,-15.0000000000001,
995.891412266977));
#144704=CARTESIAN_POINT('Ctrl Pts',(2.24911755886126E-11,-15.0000000000001,
996.950000000024));
#144705=CARTESIAN_POINT('Ctrl Pts',(1.68611037020101E-9,-15.0000000000001,
1093.78750000181));
#144706=CARTESIAN_POINT('Ctrl Pts',(-0.876425657055577,-15.0000000000986,
1092.84539516268));
#144707=CARTESIAN_POINT('Ctrl Pts',(-1.75065812745964,-14.9235720281569,
1091.89803504357));
#144708=CARTESIAN_POINT('Ctrl Pts',(-5.44814057417547,-14.2679091189493,
1087.85815476261));
#144709=CARTESIAN_POINT('Ctrl Pts',(-8.08330603931329,-12.9581831528988,
1084.79952847719));
#144710=CARTESIAN_POINT('Ctrl Pts',(-12.3011322074853,-9.05260244348057,
1078.6161215134));
#144711=CARTESIAN_POINT('Ctrl Pts',(-13.807366164627,-6.52782291760142,
1075.56391360973));
#144712=CARTESIAN_POINT('Ctrl Pts',(-15.2432587189879,-0.959580395540722,
1069.37026490581));
#144713=CARTESIAN_POINT('Ctrl Pts',(-15.1445654985297,1.97993033575274,
1066.32396755525));
#144714=CARTESIAN_POINT('Ctrl Pts',(-13.3365580323199,7.44480340050893,
1060.1176959226));
#144715=CARTESIAN_POINT('Ctrl Pts',(-11.6620142236278,9.86363973510192,
1057.07609626137));
#144716=CARTESIAN_POINT('Ctrl Pts',(-7.17920077957322,13.4817799027032,
1050.86031498226));
#144717=CARTESIAN_POINT('Ctrl Pts',(-4.46113110936773,14.6082956535718,
1047.8219642932));
#144718=CARTESIAN_POINT('Ctrl Pts',(1.27006225544689,15.2215062214116,1041.60019575181));
#144719=CARTESIAN_POINT('Ctrl Pts',(4.16501214688111,14.6956178083694,1038.56342494792));
#144720=CARTESIAN_POINT('Ctrl Pts',(9.31529759896216,12.1051517549074,1032.33983033606));
#144721=CARTESIAN_POINT('Ctrl Pts',(11.4636677038208,10.0940979652688,1029.30216497423));
#144722=CARTESIAN_POINT('Ctrl Pts',(14.3881591190903,5.12704029501961,1023.08115335682));
#144723=CARTESIAN_POINT('Ctrl Pts',(15.1042014134289,2.27230308855386,1020.04055336436));
#144724=CARTESIAN_POINT('Ctrl Pts',(14.8713083193167,-3.48425063619731,
1013.82609475946));
#144725=CARTESIAN_POINT('Ctrl Pts',(13.9268335217246,-6.2717978451629,1010.78095898351));
#144726=CARTESIAN_POINT('Ctrl Pts',(10.6156269806208,-10.9812493468169,
1004.57661759013));
#144727=CARTESIAN_POINT('Ctrl Pts',(8.31276114991967,-12.8133439752483,
1001.52557122028));
#144728=CARTESIAN_POINT('Ctrl Pts',(3.84726626553424,-14.627690881467,996.337201344411));
#144729=CARTESIAN_POINT('Ctrl Pts',(1.92979839330253,-14.9999999996949,
994.261917136008));
#144730=CARTESIAN_POINT('Ctrl Pts',(2.37242503420276E-9,-15.0000000000001,
992.18750000255));
#144731=CARTESIAN_POINT('Origin',(0.,0.,0.));
#144732=CARTESIAN_POINT('',(-7.10644545762562E-10,-15.0000000000001,793.749999998472));
#144733=CARTESIAN_POINT('',(5.08855987370824E-11,-15.0000000000001,890.587500000109));
#144734=CARTESIAN_POINT('',(-1.83697019872103E-15,-15.,-1.82952505755738E-15));
#144735=CARTESIAN_POINT('Ctrl Pts',(-1.4212352516319E-9,-15.0000000000001,
793.749999998472));
#144736=CARTESIAN_POINT('Ctrl Pts',(1.76519122070185,-15.0000000001673,
795.647474331607));
#144737=CARTESIAN_POINT('Ctrl Pts',(3.51901863713381,-14.6893233616095,
797.546580864287));
#144738=CARTESIAN_POINT('Ctrl Pts',(7.88307933530167,-13.0810399035321,
802.553071209357));
#144739=CARTESIAN_POINT('Ctrl Pts',(10.2433978333917,-11.327723059795,805.609567012152));
#144740=CARTESIAN_POINT('Ctrl Pts',(13.7061245965917,-6.7393853876843,811.788854396085));
#144741=CARTESIAN_POINT('Ctrl Pts',(14.7433308821365,-3.98649793084226,
814.846396219982));
#144742=CARTESIAN_POINT('Ctrl Pts',(15.1731391053388,1.7493469424941,821.038498688545));
#144743=CARTESIAN_POINT('Ctrl Pts',(14.5559111691972,4.62668927378638,824.089072661046));
#144744=CARTESIAN_POINT('Ctrl Pts',(11.8093560737853,9.68668515431755,830.294264904198));
#144745=CARTESIAN_POINT('Ctrl Pts',(9.73230183022213,11.7719603645367,833.339020465625));
#144746=CARTESIAN_POINT('Ctrl Pts',(4.67917428517377,14.5398118424006,839.554081593592));
#144747=CARTESIAN_POINT('Ctrl Pts',(1.8037345722074,15.1674876194237,842.594410804555));
#144748=CARTESIAN_POINT('Ctrl Pts',(-3.94574904241249,14.7559442362928,
848.815752630463));
#144749=CARTESIAN_POINT('Ctrl Pts',(-6.70217019283721,13.7255397948671,
851.853272124192));
#144750=CARTESIAN_POINT('Ctrl Pts',(-11.3121227246376,10.263733864938,858.076876602063));
#144751=CARTESIAN_POINT('Ctrl Pts',(-13.0701273279823,7.90434178378963,
861.113701837503));
#144752=CARTESIAN_POINT('Ctrl Pts',(-15.0685969374762,2.49816738752234,
867.335160491185));
#144753=CARTESIAN_POINT('Ctrl Pts',(-15.2678536303296,-0.437331223543642,
870.373694270458));
#144754=CARTESIAN_POINT('Ctrl Pts',(-14.0198829821495,-6.06101357079894,
876.588896410459));
#144755=CARTESIAN_POINT('Ctrl Pts',(-12.5977171160585,-8.6362950379507,
879.63079255184));
#144756=CARTESIAN_POINT('Ctrl Pts',(-8.50671645746886,-12.6851234777784,
885.83624334546));
#144757=CARTESIAN_POINT('Ctrl Pts',(-5.91766454505476,-14.0804183360584,
888.882933729287));
#144758=CARTESIAN_POINT('Ctrl Pts',(-2.07890783483043,-14.8920661724229,
893.10863180637));
#144759=CARTESIAN_POINT('Ctrl Pts',(-1.04034966888609,-14.999999999953,
894.231686715025));
#144760=CARTESIAN_POINT('Ctrl Pts',(-6.7874927900391E-10,-15.0000000000001,
895.34999999927));
#144761=CARTESIAN_POINT('Ctrl Pts',(2.37243471590498E-9,-15.0000000000001,
992.18750000255));
#144762=CARTESIAN_POINT('Ctrl Pts',(-0.927957530816727,-15.0000000001469,
991.190001499619));
#144763=CARTESIAN_POINT('Ctrl Pts',(-1.85296309005188,-14.9143294957641,
990.187315211522));
#144764=CARTESIAN_POINT('Ctrl Pts',(-5.59527262211916,-14.2111492040552,
986.093806251726));
#144765=CARTESIAN_POINT('Ctrl Pts',(-8.21361976692825,-12.8756124686143,
983.03887894798));
#144766=CARTESIAN_POINT('Ctrl Pts',(-12.3917472570646,-8.92848976450734,
976.851202299565));
#144767=CARTESIAN_POINT('Ctrl Pts',(-13.873061125772,-6.38810058370437,
973.80261370812));
#144768=CARTESIAN_POINT('Ctrl Pts',(-15.2525780670412,-0.801972300954369,
967.60116828226));
#144769=CARTESIAN_POINT('Ctrl Pts',(-15.1235572878471,2.13685845381269,
964.557803828508));
#144770=CARTESIAN_POINT('Ctrl Pts',(-13.2574509380886,7.58519758337838,
958.345518804266));
#144771=CARTESIAN_POINT('Ctrl Pts',(-11.5573269768786,9.98642922314981,
955.306025368043));
#144772=CARTESIAN_POINT('Ctrl Pts',(-7.0346793751524,13.5579395357593,949.086263182288));
#144773=CARTESIAN_POINT('Ctrl Pts',(-4.30463460409252,14.6552860177948,
946.049059359286));
#144774=CARTESIAN_POINT('Ctrl Pts',(1.43374846857219,15.2070315904723,939.825684710236));
#144775=CARTESIAN_POINT('Ctrl Pts',(4.32303749816315,14.6498960878069,936.788713098054));
#144776=CARTESIAN_POINT('Ctrl Pts',(9.44483642742651,12.0042902169801,930.566113997223));
#144777=CARTESIAN_POINT('Ctrl Pts',(11.5716088123676,9.97000556149205,927.526923347156));
#144778=CARTESIAN_POINT('Ctrl Pts',(14.4419093540699,4.97311569195438,921.309327379516));
#144779=CARTESIAN_POINT('Ctrl Pts',(15.1274586611398,2.11082613967822,918.266231736795));
#144780=CARTESIAN_POINT('Ctrl Pts',(14.8335136101058,-3.64057867511896,
912.057331611732));
#144781=CARTESIAN_POINT('Ctrl Pts',(13.8599399514386,-6.41788133803346,
909.008860498642));
#144782=CARTESIAN_POINT('Ctrl Pts',(10.5014564938674,-11.0898991083664,
902.812009755185));
#144783=CARTESIAN_POINT('Ctrl Pts',(8.18043380872852,-12.8980569953977,
899.75693072865));
#144784=CARTESIAN_POINT('Ctrl Pts',(3.74578459492545,-14.6471922085484,
894.629748667918));
#144785=CARTESIAN_POINT('Ctrl Pts',(1.87950880952251,-14.9999999999999,
892.607858859883));
#144786=CARTESIAN_POINT('Ctrl Pts',(1.01686159492687E-10,-15.,890.587500000109));
#144787=CARTESIAN_POINT('Origin',(0.,0.,0.));
#144788=CARTESIAN_POINT('',(-1.80332313813543E-12,-15.0000000000001,692.149999999996));
#144789=CARTESIAN_POINT('',(-2.4458388347729E-10,-15.0000000000001,788.987499999474));
#144790=CARTESIAN_POINT('',(-1.83697019872103E-15,-15.,-1.82952505755738E-15));
#144791=CARTESIAN_POINT('Ctrl Pts',(-3.5241254359164E-12,-15.0000000000001,
692.149999999996));
#144792=CARTESIAN_POINT('Ctrl Pts',(2.27103459580004,-15.0000000000006,
694.591225517793));
#144793=CARTESIAN_POINT('Ctrl Pts',(4.51291959281525,-14.4846707381985,
697.011788622728));
#144794=CARTESIAN_POINT('Ctrl Pts',(8.64315435316608,-12.4767767750544,
701.96930729735));
#144795=CARTESIAN_POINT('Ctrl Pts',(10.4683168716844,-10.9901223189493,
704.442659371204));
#144796=CARTESIAN_POINT('Ctrl Pts',(13.6358594810391,-6.87878566199796,
710.026361856284));
#144797=CARTESIAN_POINT('Ctrl Pts',(14.70182367816,-4.13630823077973,713.084669264574));
#144798=CARTESIAN_POINT('Ctrl Pts',(15.1901873421449,1.5931409972409,719.26986734642));
#144799=CARTESIAN_POINT('Ctrl Pts',(14.602480182245,4.47613423322987,722.324420568784));
#144800=CARTESIAN_POINT('Ctrl Pts',(11.9104277463035,9.56187576526177,728.522269143782));
#144801=CARTESIAN_POINT('Ctrl Pts',(9.85546654182256,11.6686743298856,731.570297221167));
#144802=CARTESIAN_POINT('Ctrl Pts',(4.8340096828692,14.4889113802708,737.779960433601));
#144803=CARTESIAN_POINT('Ctrl Pts',(1.96533794957528,15.1472381812194,740.82271390217));
#144804=CARTESIAN_POINT('Ctrl Pts',(-3.78684542770849,14.7974126041612,
747.040810232922));
#144805=CARTESIAN_POINT('Ctrl Pts',(-6.55447001096606,13.7966352145626,
750.079776453113));
#144806=CARTESIAN_POINT('Ctrl Pts',(-11.2011708624236,10.384705053829,756.302591703863));
#144807=CARTESIAN_POINT('Ctrl Pts',(-12.9845668664545,8.04427576340637,
759.339471318412));
#144808=CARTESIAN_POINT('Ctrl Pts',(-15.0411951245362,2.65883896988886,
765.562735066766));
#144809=CARTESIAN_POINT('Ctrl Pts',(-15.2718217246421,-0.274436759551656,
768.600049449871));
#144810=CARTESIAN_POINT('Ctrl Pts',(-14.0831511308341,-5.91309660484774,
774.819382059842));
#144811=CARTESIAN_POINT('Ctrl Pts',(-12.6880307450419,-8.50343061672422,
777.859110474772));
#144812=CARTESIAN_POINT('Ctrl Pts',(-8.63749803694922,-12.5968495674121,
784.07070355884));
#144813=CARTESIAN_POINT('Ctrl Pts',(-6.06246619700213,-14.0189147492482,
787.11441114891));
#144814=CARTESIAN_POINT('Ctrl Pts',(-2.1806435024888,-14.8812351916921,
791.399796387356));
#144815=CARTESIAN_POINT('Ctrl Pts',(-1.0910039980068,-14.9999999998967,
792.577236359633));
#144816=CARTESIAN_POINT('Ctrl Pts',(-1.421166517801E-9,-15.0000000000001,
793.749999998472));
#144817=CARTESIAN_POINT('Ctrl Pts',(1.01688518716614E-10,-15.0000000000002,
890.587500000109));
#144818=CARTESIAN_POINT('Ctrl Pts',(-0.977428461994903,-15.0000000000003,
889.536823225789));
#144819=CARTESIAN_POINT('Ctrl Pts',(-1.95255362472441,-14.9048231302732,
888.481098490165));
#144820=CARTESIAN_POINT('Ctrl Pts',(-5.73749331040952,-14.1545187708565,
884.329403256852));
#144821=CARTESIAN_POINT('Ctrl Pts',(-8.34325300287303,-12.7925966847513,
881.27836923249));
#144822=CARTESIAN_POINT('Ctrl Pts',(-12.4834370889708,-8.80020283642223,
875.082171224733));
#144823=CARTESIAN_POINT('Ctrl Pts',(-13.9388522127874,-6.24418165447485,
872.036841463946));
#144824=CARTESIAN_POINT('Ctrl Pts',(-15.2604165047268,-0.640780879139956,
865.828562924129));
#144825=CARTESIAN_POINT('Ctrl Pts',(-15.1003526217916,2.29686927308867,
862.787680347582));
#144826=CARTESIAN_POINT('Ctrl Pts',(-13.1753791252392,7.72725137941694,
856.570514872512));
#144827=CARTESIAN_POINT('Ctrl Pts',(-11.449446160624,10.1101637037372,853.532588444096));
#144828=CARTESIAN_POINT('Ctrl Pts',(-6.88731259235128,13.6335360655616,
847.310126440447));
#144829=CARTESIAN_POINT('Ctrl Pts',(-4.1455159194855,14.7011388963839,844.273449042886));
#144830=CARTESIAN_POINT('Ctrl Pts',(1.59873478344331,15.1905640636383,838.049974645588));
#144831=CARTESIAN_POINT('Ctrl Pts',(4.48211981955633,14.6019231598022,835.011896556154));
#144832=CARTESIAN_POINT('Ctrl Pts',(9.57397060596606,11.9014034615129,828.791814175797));
#144833=CARTESIAN_POINT('Ctrl Pts',(11.6787211549985,9.84410097360831,825.75048940482));
#144834=CARTESIAN_POINT('Ctrl Pts',(14.4940300860886,4.81833720724832,819.537643727229));
#144835=CARTESIAN_POINT('Ctrl Pts',(15.1489947663658,1.94897957664842,816.491511094136));
#144836=CARTESIAN_POINT('Ctrl Pts',(14.7940850656901,-3.79613331868855,
810.289403379063));
#144837=CARTESIAN_POINT('Ctrl Pts',(13.79175459564,-6.56276165432192,807.237132215546));
#144838=CARTESIAN_POINT('Ctrl Pts',(10.385580112573,-11.1983334067647,801.046630210449));
#144839=CARTESIAN_POINT('Ctrl Pts',(8.04509568799686,-12.9820150209759,
797.988053372213));
#144840=CARTESIAN_POINT('Ctrl Pts',(3.64287626884949,-14.66683091111,792.919331437006));
#144841=CARTESIAN_POINT('Ctrl Pts',(1.82776494649211,-15.0000000000597,
790.952237321105));
#144842=CARTESIAN_POINT('Ctrl Pts',(-4.89162321759551E-10,-15.0000000000001,
788.987499999474));
#144843=CARTESIAN_POINT('Origin',(0.,0.,-11.4051836540916));
#144844=CARTESIAN_POINT('',(-39.,3.56961574259503E-12,767.551815642455));
#144845=CARTESIAN_POINT('',(-39.,-1.80076817690714E-11,764.385684357557));
#144846=CARTESIAN_POINT('',(-39.,-4.77612251667468E-15,-11.4051836540916));
#144847=CARTESIAN_POINT('',(1.56487907968316,-38.9685918845674,692.));
#144848=CARTESIAN_POINT('Ctrl Pts',(-39.,7.1880001950575E-12,767.551815642455));
#144849=CARTESIAN_POINT('Ctrl Pts',(-39.,0.444599787572262,767.367213541182));
#144850=CARTESIAN_POINT('Ctrl Pts',(-38.992397846984,0.889538753063548,
767.182470609977));
#144851=CARTESIAN_POINT('Ctrl Pts',(-38.7890284837619,6.82867978239275,
764.716482221239));
#144852=CARTESIAN_POINT('Ctrl Pts',(-37.4402879297879,12.2245802425215,
762.458043468178));
#144853=CARTESIAN_POINT('Ctrl Pts',(-32.6014351065545,22.0997120942476,
757.90889018916));
#144854=CARTESIAN_POINT('Ctrl Pts',(-29.1621326216746,26.4734173647096,
755.64917874153));
#144855=CARTESIAN_POINT('Ctrl Pts',(-20.7028282263121,33.5056264037719,
751.086638313621));
#144856=CARTESIAN_POINT('Ctrl Pts',(-15.7768863592026,36.0878204316542,
748.834245115048));
#144857=CARTESIAN_POINT('Ctrl Pts',(-5.18442159666645,39.0428894729064,
744.268269289717));
#144858=CARTESIAN_POINT('Ctrl Pts',(0.365808868099208,39.383788448861,742.015279419795));
#144859=CARTESIAN_POINT('Ctrl Pts',(11.2391673468008,37.748076109223,737.457150275462));
#144860=CARTESIAN_POINT('Ctrl Pts',(16.4443409752546,35.7884046024072,735.199214991829));
#144861=CARTESIAN_POINT('Ctrl Pts',(25.6986365833266,29.8467189665087,730.646129090551));
#144862=CARTESIAN_POINT('Ctrl Pts',(29.6484851419845,25.927241388788,728.3887560339));
#144863=CARTESIAN_POINT('Ctrl Pts',(35.6615894594247,16.7177367431117,723.823289708095));
#144864=CARTESIAN_POINT('Ctrl Pts',(37.6604489060644,11.5291626374632,721.572274339719));
#144865=CARTESIAN_POINT('Ctrl Pts',(39.3798653450543,0.668787227458401,
717.008539998774));
#144866=CARTESIAN_POINT('Ctrl Pts',(39.0813650471648,-4.88478403069311,
714.751600946893));
#144867=CARTESIAN_POINT('Ctrl Pts',(36.2080678936678,-15.4990648548602,
710.200272791918));
#144868=CARTESIAN_POINT('Ctrl Pts',(33.6630934166401,-20.4463943747878,
707.941434691088));
#144869=CARTESIAN_POINT('Ctrl Pts',(26.6958917991014,-28.9579870927979,
703.380807166622));
#144870=CARTESIAN_POINT('Ctrl Pts',(22.3503480195058,-32.4300148760212,
701.127610053241));
#144871=CARTESIAN_POINT('Ctrl Pts',(12.4910508591148,-37.3559251748377,
696.551440503674));
#144872=CARTESIAN_POINT('Ctrl Pts',(7.08162027719987,-38.7470536541486,
694.289319896425));
#144873=CARTESIAN_POINT('Ctrl Pts',(1.56487907968316,-38.9685918845674,
692.000000000001));
#144874=CARTESIAN_POINT('',(9.11627411387425,-37.91956679975,692.));
#144875=CARTESIAN_POINT('Origin',(0.,0.,692.));
#144876=CARTESIAN_POINT('Ctrl Pts',(9.1162741138742,-37.9195667997501,692.));
#144877=CARTESIAN_POINT('Ctrl Pts',(14.1364514273045,-36.7126618598502,
694.141991806554));
#144878=CARTESIAN_POINT('Ctrl Pts',(18.8687364296366,-34.5200872168667,
696.25895288502));
#144879=CARTESIAN_POINT('Ctrl Pts',(27.2024632672717,-28.4199203974411,
700.546668576892));
#144880=CARTESIAN_POINT('Ctrl Pts',(30.7225562439626,-24.5721582467486,
702.661883267291));
#144881=CARTESIAN_POINT('Ctrl Pts',(36.2324554963202,-15.4420798166754,
707.089320277153));
#144882=CARTESIAN_POINT('Ctrl Pts',(38.0466274529669,-10.1829991503243,
709.344111975511));
#144883=CARTESIAN_POINT('Ctrl Pts',(39.3789466567602,0.734164630120643,
713.901490499695));
#144884=CARTESIAN_POINT('Ctrl Pts',(38.8826514753387,6.27508587776081,716.159640762425));
#144885=CARTESIAN_POINT('Ctrl Pts',(35.6324146729093,16.7793046237023,720.714080390645));
#144886=CARTESIAN_POINT('Ctrl Pts',(32.9140276449878,21.6307625893325,722.969013463136));
#144887=CARTESIAN_POINT('Ctrl Pts',(25.6512770191788,29.8872448531897,727.534034394676));
#144888=CARTESIAN_POINT('Ctrl Pts',(21.1864018163163,33.2019407361348,729.785369990551));
#144889=CARTESIAN_POINT('Ctrl Pts',(11.1789157366835,37.7662650004625,734.349697976576));
#144890=CARTESIAN_POINT('Ctrl Pts',(5.74390122675569,38.9648870548074,736.609589868737));
#144891=CARTESIAN_POINT('Ctrl Pts',(-5.25341170921003,39.0335708226067,
741.158932569111));
#144892=CARTESIAN_POINT('Ctrl Pts',(-10.6985856030828,37.9048715375236,
743.417488861358));
#144893=CARTESIAN_POINT('Ctrl Pts',(-20.7607467890849,33.4695665217669,
747.978260294979));
#144894=CARTESIAN_POINT('Ctrl Pts',(-25.2673353820903,30.2124000190225,
750.23016450274));
#144895=CARTESIAN_POINT('Ctrl Pts',(-32.63599301526,22.0485276733406,754.796393500793));
#144896=CARTESIAN_POINT('Ctrl Pts',(-35.4166106518228,17.2308001327554,
757.050113502379));
#144897=CARTESIAN_POINT('Ctrl Pts',(-38.3641920260956,8.1148275827748,761.021668280858));
#144898=CARTESIAN_POINT('Ctrl Pts',(-39.0000000000038,4.06368217415025,
762.698404495439));
#144899=CARTESIAN_POINT('Ctrl Pts',(-39.,-3.61188856601302E-11,764.385684357557));
#144900=CARTESIAN_POINT('Origin',(0.,0.,-11.4051836540916));
#144901=CARTESIAN_POINT('',(-39.,-4.02744219736708E-14,869.151815642458));
#144902=CARTESIAN_POINT('',(-39.,-8.91515698045976E-11,865.985684357616));
#144903=CARTESIAN_POINT('',(-39.,-4.77612251667468E-15,-11.4051836540916));
#144904=CARTESIAN_POINT('Ctrl Pts',(-39.,5.88418203051333E-14,869.151815642458));
#144905=CARTESIAN_POINT('Ctrl Pts',(-39.,5.43573553489539,866.894846049194));
#144906=CARTESIAN_POINT('Ctrl Pts',(-37.8631212524949,10.8138469940783,
864.667660265692));
#144907=CARTESIAN_POINT('Ctrl Pts',(-33.4370296592246,20.8135523395336,
860.132186162968));
#144908=CARTESIAN_POINT('Ctrl Pts',(-30.1721615248585,25.3151904067071,
857.873657366882));
#144909=CARTESIAN_POINT('Ctrl Pts',(-21.9967696512043,32.6710375348237,
853.324209146));
#144910=CARTESIAN_POINT('Ctrl Pts',(-17.1720111301126,35.4454630157482,
851.064390556249));
#144911=CARTESIAN_POINT('Ctrl Pts',(-6.70052089744381,38.8115381378829,
846.500025433587));
#144912=CARTESIAN_POINT('Ctrl Pts',(-1.16770832885968,39.3684107232863,
844.248705172239));
#144913=CARTESIAN_POINT('Ctrl Pts',(9.76154258437761,38.1567207763231,839.683712548098));
#144914=CARTESIAN_POINT('Ctrl Pts',(15.0383962019526,36.4013826067875,837.428730640023));
#144915=CARTESIAN_POINT('Ctrl Pts',(24.51549939447,30.8257647944294,832.874370577483));
#144916=CARTESIAN_POINT('Ctrl Pts',(28.6141467064143,27.0642110841891,830.616212538848));
#144917=CARTESIAN_POINT('Ctrl Pts',(34.981969791075,18.096988705713,826.058741973881));
#144918=CARTESIAN_POINT('Ctrl Pts',(37.1828994118403,12.9877066390436,823.803998730174));
#144919=CARTESIAN_POINT('Ctrl Pts',(39.3241345362518,2.20024120607044,819.237839384974));
#144920=CARTESIAN_POINT('Ctrl Pts',(39.2420353216892,-3.35949143992115,
816.986391935878));
#144921=CARTESIAN_POINT('Ctrl Pts',(36.7838234711582,-14.0780771294997,
812.424161558999));
#144922=CARTESIAN_POINT('Ctrl Pts',(34.4343093017528,-19.1178375038457,
810.16482214988));
#144923=CARTESIAN_POINT('Ctrl Pts',(27.8063368808782,-27.893884243463,805.617939454984));
#144924=CARTESIAN_POINT('Ctrl Pts',(23.5963270574983,-31.5352943432299,
803.356306298561));
#144925=CARTESIAN_POINT('Ctrl Pts',(13.9552638353624,-36.8304721490037,
798.792907898438));
#144926=CARTESIAN_POINT('Ctrl Pts',(8.62872741855903,-38.4289357163304,
796.541140708907));
#144927=CARTESIAN_POINT('Ctrl Pts',(-2.3319679143772,-39.3164874371797,
791.975565719672));
#144928=CARTESIAN_POINT('Ctrl Pts',(-7.8460057578923,-38.5960507447532,
789.721660590033));
#144929=CARTESIAN_POINT('Ctrl Pts',(-18.2099342535552,-34.9232527989276,
785.165399093187));
#144930=CARTESIAN_POINT('Ctrl Pts',(-22.9483474087012,-32.0094593548667,
782.907430332298));
#144931=CARTESIAN_POINT('Ctrl Pts',(-30.9042815915061,-24.4165483955361,
778.352121306444));
#144932=CARTESIAN_POINT('Ctrl Pts',(-34.0365945401134,-19.8182183286086,
776.096150894115));
#144933=CARTESIAN_POINT('Ctrl Pts',(-38.021049427416,-10.0464108930014,
771.715153884756));
#144934=CARTESIAN_POINT('Ctrl Pts',(-39.,-5.04360596152766,769.645969271254));
#144935=CARTESIAN_POINT('Ctrl Pts',(-39.,7.16232628761304E-12,767.551815642455));
#144936=CARTESIAN_POINT('Ctrl Pts',(-39.,-3.61427554551597E-11,764.385684357557));
#144937=CARTESIAN_POINT('Ctrl Pts',(-38.9999999999987,-1.41200103218787,
764.971960745502));
#144938=CARTESIAN_POINT('Ctrl Pts',(-38.9233013074596,-2.82623296434554,
765.557781691743));
#144939=CARTESIAN_POINT('Ctrl Pts',(-38.1722588338924,-9.70013164892058,
768.420594268634));
#144940=CARTESIAN_POINT('Ctrl Pts',(-36.4255115393919,-14.9801180847204,
770.676769353789));
#144941=CARTESIAN_POINT('Ctrl Pts',(-30.8647629112545,-24.4662881566758,
775.241027877367));
#144942=CARTESIAN_POINT('Ctrl Pts',(-27.1116891258472,-28.5690135328132,
777.49208368091));
#144943=CARTESIAN_POINT('Ctrl Pts',(-18.1545878659332,-34.9523543053397,
782.057206704967));
#144944=CARTESIAN_POINT('Ctrl Pts',(-13.0472248932953,-37.1620661313272,
784.315434277579));
#144945=CARTESIAN_POINT('Ctrl Pts',(-2.26362020088496,-39.3204680063181,
788.867220301099));
#144946=CARTESIAN_POINT('Ctrl Pts',(3.29737917386447,-39.2474740090443,
791.125283740846));
#144947=CARTESIAN_POINT('Ctrl Pts',(14.0188203721114,-36.8061204904945,
795.68439528666));
#144948=CARTESIAN_POINT('Ctrl Pts',(19.0626052570436,-34.4651011006093,
797.936948847296));
#144949=CARTESIAN_POINT('Ctrl Pts',(27.8486672076749,-27.8512893435151,
802.503067329164));
#144950=CARTESIAN_POINT('Ctrl Pts',(31.4942080166653,-23.6505762003017,
804.755886017233));
#144951=CARTESIAN_POINT('Ctrl Pts',(36.8068355358466,-14.018608246568,809.317379629089));
#144952=CARTESIAN_POINT('Ctrl Pts',(38.4147344977359,-8.69228539662842,
811.576563989154));
#144953=CARTESIAN_POINT('Ctrl Pts',(39.3201679817139,2.26694917916401,816.126943426164));
#144954=CARTESIAN_POINT('Ctrl Pts',(38.6088754210609,7.78300555017287,818.384528116055));
#144955=CARTESIAN_POINT('Ctrl Pts',(34.9528871370198,18.1528208293289,822.947789636676));
#144956=CARTESIAN_POINT('Ctrl Pts',(32.0482572340742,22.8941072466728,825.198840226943));
#144957=CARTESIAN_POINT('Ctrl Pts',(24.4682514825065,30.8635363641544,829.764524896469));
#144958=CARTESIAN_POINT('Ctrl Pts',(19.8747124247098,34.0035355777327,832.021254263112));
#144959=CARTESIAN_POINT('Ctrl Pts',(9.69813407717675,38.1729616484813,836.575344807772));
#144960=CARTESIAN_POINT('Ctrl Pts',(4.22398187768683,39.1585705743747,838.833253131089));
#144961=CARTESIAN_POINT('Ctrl Pts',(-6.76575577782906,38.8000042504229,
843.39056952592));
#144962=CARTESIAN_POINT('Ctrl Pts',(-12.1627992121961,37.4605290148405,
845.643944977488));
#144963=CARTESIAN_POINT('Ctrl Pts',(-22.045652839921,32.6378433627528,850.209765718567));
#144964=CARTESIAN_POINT('Ctrl Pts',(-26.4229593532984,29.2072045838926,
852.461859088474));
#144965=CARTESIAN_POINT('Ctrl Pts',(-33.4707468218834,20.76022457522,857.025202485842));
#144966=CARTESIAN_POINT('Ctrl Pts',(-36.0620133214413,15.8361821387683,
859.285407332465));
#144967=CARTESIAN_POINT('Ctrl Pts',(-38.5138914172955,7.10187197100778,
863.037292523889));
#144968=CARTESIAN_POINT('Ctrl Pts',(-39.0000000000163,3.554560955032,864.50979651469));
#144969=CARTESIAN_POINT('Ctrl Pts',(-39.,-1.78223547031564E-10,865.985684357616));
#144970=CARTESIAN_POINT('Origin',(0.,0.,-11.4051836540916));
#144971=CARTESIAN_POINT('',(-39.,-1.05587355240895E-11,970.751815642467));
#144972=CARTESIAN_POINT('',(-39.,-1.22179591926513E-11,967.585684357552));
#144973=CARTESIAN_POINT('',(-39.,-4.77612251667468E-15,-11.4051836540916));
#144974=CARTESIAN_POINT('Ctrl Pts',(-39.,-2.11605732935993E-11,970.751815642467));
#144975=CARTESIAN_POINT('Ctrl Pts',(-39.0000000000027,4.92045984381282,
968.708793464306));
#144976=CARTESIAN_POINT('Ctrl Pts',(-38.0680720015819,9.80530383712027,
966.688880125693));
#144977=CARTESIAN_POINT('Ctrl Pts',(-34.2201085718197,19.4989496685401,
962.358617547347));
#144978=CARTESIAN_POINT('Ctrl Pts',(-31.1327799735451,24.1239656923328,
960.105203795389));
#144979=CARTESIAN_POINT('Ctrl Pts',(-23.2507510474625,31.7905365139141,
955.547965852891));
#144980=CARTESIAN_POINT('Ctrl Pts',(-18.5404717310421,34.7488123608543,
953.290056619791));
#144981=CARTESIAN_POINT('Ctrl Pts',(-8.20992752944213,38.5206638305759,
948.735872244936));
#144982=CARTESIAN_POINT('Ctrl Pts',(-2.69967510934749,39.2933179652049,
946.479202197762));
#144983=CARTESIAN_POINT('Ctrl Pts',(8.27075550201749,38.5074729519727,941.913498726737));
#144984=CARTESIAN_POINT('Ctrl Pts',(13.6110658153455,36.9590035688653,939.662442975147));
#144985=CARTESIAN_POINT('Ctrl Pts',(23.2975428355124,31.7560210478991,935.099228184755));
#144986=CARTESIAN_POINT('Ctrl Pts',(27.5383720174836,28.1576417514627,932.841580577787));
#144987=CARTESIAN_POINT('Ctrl Pts',(34.250086087367,19.4468375978943,928.291292528354));
#144988=CARTESIAN_POINT('Ctrl Pts',(36.6487984492457,14.4267332905264,926.032071881529));
#144989=CARTESIAN_POINT('Ctrl Pts',(39.2088126415577,3.72878507586251,921.470497515674));
#144990=CARTESIAN_POINT('Ctrl Pts',(39.3432049830526,-1.8315782015685,919.217712942267));
#144991=CARTESIAN_POINT('Ctrl Pts',(37.3029756255119,-12.637803275991,914.651603230416));
#144992=CARTESIAN_POINT('Ctrl Pts',(35.1513049600264,-17.7652326337268,
912.399018510629));
#144993=CARTESIAN_POINT('Ctrl Pts',(28.8703393170326,-26.790676818201,907.839979854173));
#144994=CARTESIAN_POINT('Ctrl Pts',(24.8088327264741,-30.5899530438165,
905.581929779443));
#144995=CARTESIAN_POINT('Ctrl Pts',(15.3839930471174,-36.2571617911556,
901.030043861947));
#144996=CARTESIAN_POINT('Ctrl Pts',(10.1204684588554,-38.0635275467779,
898.771882771897));
#144997=CARTESIAN_POINT('Ctrl Pts',(-0.799685057268203,-39.3775662049388,
894.206730309309));
#144998=CARTESIAN_POINT('Ctrl Pts',(-6.33707553182674,-38.8725380651309,
891.95568238689));
#144999=CARTESIAN_POINT('Ctrl Pts',(-16.8364085685143,-35.605577080513,
887.391460074885));
#145000=CARTESIAN_POINT('Ctrl Pts',(-21.6836447425657,-32.8790733233354,
885.135228979051));
#145001=CARTESIAN_POINT('Ctrl Pts',(-29.9284323367762,-25.6033471660073,
880.582834717982));
#145002=CARTESIAN_POINT('Ctrl Pts',(-33.2374777722068,-21.1310829147382,
878.324314875799));
#145003=CARTESIAN_POINT('Ctrl Pts',(-37.7845490861634,-11.1159588568865,
873.76472521789));
#145004=CARTESIAN_POINT('Ctrl Pts',(-38.9738384760769,-5.6820241810347,
871.5110466467));
#145005=CARTESIAN_POINT('Ctrl Pts',(-38.9998577080699,-0.121656064835777,
869.202328408837));
#145006=CARTESIAN_POINT('Ctrl Pts',(-39.,-0.0608242949889622,869.177070473831));
#145007=CARTESIAN_POINT('Ctrl Pts',(-39.,-2.5360886051307E-15,869.151815642458));
#145008=CARTESIAN_POINT('Ctrl Pts',(-39.,-1.78279613294308E-10,865.985684357616));
#145009=CARTESIAN_POINT('Ctrl Pts',(-38.9999999999912,-1.91614269570151,
866.781285205448));
#145010=CARTESIAN_POINT('Ctrl Pts',(-38.8586492523547,-3.83569992409224,
867.574718006289));
#145011=CARTESIAN_POINT('Ctrl Pts',(-37.7660819373123,-11.1780366895091,
870.654775329797));
#145012=CARTESIAN_POINT('Ctrl Pts',(-35.8156431428152,-16.3850268959936,
872.906032745858));
#145013=CARTESIAN_POINT('Ctrl Pts',(-29.8889018752433,-25.6496346055645,
877.472074254061));
#145014=CARTESIAN_POINT('Ctrl Pts',(-25.9764906847373,-29.6051152359186,
879.72747839053));
#145015=CARTESIAN_POINT('Ctrl Pts',(-16.7779944725433,-35.6333243471609,
884.283725350576));
#145016=CARTESIAN_POINT('Ctrl Pts',(-11.5901967615144,-37.641764954479,
886.54181709808));
#145017=CARTESIAN_POINT('Ctrl Pts',(-0.732831366644527,-39.3786413109767,
891.097209752753));
#145018=CARTESIAN_POINT('Ctrl Pts',(4.82065298608422,-39.089449133969,893.351573189743));
#145019=CARTESIAN_POINT('Ctrl Pts',(15.4396725026777,-36.2333177596016,
897.916911861676));
#145020=CARTESIAN_POINT('Ctrl Pts',(20.3888906201009,-33.6975651182713,
900.168458710607));
#145021=CARTESIAN_POINT('Ctrl Pts',(28.9126401245583,-26.74545823846,904.732309528255));
#145022=CARTESIAN_POINT('Ctrl Pts',(32.394104696192,-22.4026799003182,906.993115408434));
#145023=CARTESIAN_POINT('Ctrl Pts',(37.3249232093689,-12.5724135651128,
911.541156287731));
#145024=CARTESIAN_POINT('Ctrl Pts',(38.7238464068962,-7.19056169986337,
913.80009408905));
#145025=CARTESIAN_POINT('Ctrl Pts',(39.2022363161185,3.79561924881892,918.361661918849));
#145026=CARTESIAN_POINT('Ctrl Pts',(38.2771142429207,9.27849894774687,920.613301618383));
#145027=CARTESIAN_POINT('Ctrl Pts',(34.2196133974516,19.5003906151297,925.179514617699));
#145028=CARTESIAN_POINT('Ctrl Pts',(31.1308192063526,24.1269579025388,927.433762820568));
#145029=CARTESIAN_POINT('Ctrl Pts',(23.2455746018107,31.7944851846347,931.992193752191));
#145030=CARTESIAN_POINT('Ctrl Pts',(18.5339271312125,34.7524557069582,934.250471010959));
#145031=CARTESIAN_POINT('Ctrl Pts',(8.20428422704431,38.5214691152723,938.80397296253));
#145032=CARTESIAN_POINT('Ctrl Pts',(2.69680821024608,39.2931256125301,941.059490457559));
#145033=CARTESIAN_POINT('Ctrl Pts',(-8.27114295907375,38.5074321825743,
945.624163024791));
#145034=CARTESIAN_POINT('Ctrl Pts',(-13.611727879551,36.9588039026025,947.875340054341));
#145035=CARTESIAN_POINT('Ctrl Pts',(-23.3013168801336,31.7538378152413,
952.440078615087));
#145036=CARTESIAN_POINT('Ctrl Pts',(-27.5442735200595,28.1525304217482,
954.699138598242));
#145037=CARTESIAN_POINT('Ctrl Pts',(-34.2556024106436,19.4371253352674,
959.250730670246));
#145038=CARTESIAN_POINT('Ctrl Pts',(-36.6529021409899,14.4163237958122,
961.509989737668));
#145039=CARTESIAN_POINT('Ctrl Pts',(-38.6433191435739,6.08814410720707,
965.060909914876));
#145040=CARTESIAN_POINT('Ctrl Pts',(-39.0000000000019,3.04469482380837,
966.3214978286));
#145041=CARTESIAN_POINT('Ctrl Pts',(-39.,-2.44598785670291E-11,967.585684357552));
#145042=CARTESIAN_POINT('Origin',(0.,0.,-11.4051836540916));
#145043=CARTESIAN_POINT('',(-39.,-1.20381251188915E-10,1072.35181564256));
#145044=CARTESIAN_POINT('',(-39.,3.32285671526687E-12,1069.18568435754));
#145045=CARTESIAN_POINT('',(-39.,-4.77612251667468E-15,-11.4051836540916));
#145046=CARTESIAN_POINT('Ctrl Pts',(-39.,-2.40734654433084E-10,1072.35181564256));
#145047=CARTESIAN_POINT('Ctrl Pts',(-39.0000000000272,4.40669534644803,
1070.52211341727));
#145048=CARTESIAN_POINT('Ctrl Pts',(-38.2519218970919,8.79514383817135,
1068.7075610424));
#145049=CARTESIAN_POINT('Ctrl Pts',(-34.95323281987,18.1522402513944,1064.58998699583));
#145050=CARTESIAN_POINT('Ctrl Pts',(-32.0485147457729,22.8938143039188,
1062.3388216931));
#145051=CARTESIAN_POINT('Ctrl Pts',(-24.4702653485043,30.86144123232,1057.77418130979));
#145052=CARTESIAN_POINT('Ctrl Pts',(-19.8794677561395,34.0003032109931,
1055.51861143013));
#145053=CARTESIAN_POINT('Ctrl Pts',(-9.70545079215384,38.1712465858339,
1050.96519208669));
#145054=CARTESIAN_POINT('Ctrl Pts',(-4.23045115476902,39.1580106813823,
1048.70690006653));
#145055=CARTESIAN_POINT('Ctrl Pts',(6.76233223196223,38.8008860452023,1044.14837968156));
#145056=CARTESIAN_POINT('Ctrl Pts',(12.1614862664044,37.4612506269753,1041.89417657098));
#145057=CARTESIAN_POINT('Ctrl Pts',(22.0451309758311,32.6380171285112,1037.32796040776));
#145058=CARTESIAN_POINT('Ctrl Pts',(26.4216655732491,29.2081754381505,1035.07630071444));
#145059=CARTESIAN_POINT('Ctrl Pts',(33.4671612900492,20.7651016180944,1030.51479696608));
#145060=CARTESIAN_POINT('Ctrl Pts',(36.0577483833216,15.8446981587664,1028.25589378643));
#145061=CARTESIAN_POINT('Ctrl Pts',(39.0335483194285,5.25736747886637,1023.7077446547));
#145062=CARTESIAN_POINT('Ctrl Pts',(39.3849169238395,-0.297496027210565,
1021.44701543651));
#145063=CARTESIAN_POINT('Ctrl Pts',(37.7664474293011,-11.1771274820797,
1016.88312363906));
#145064=CARTESIAN_POINT('Ctrl Pts',(35.8158523018511,-16.3847920769605,
1014.63159586748));
#145065=CARTESIAN_POINT('Ctrl Pts',(29.8899703813292,-25.6478722084131,
1010.06628145815));
#145066=CARTESIAN_POINT('Ctrl Pts',(25.9796475946162,-29.6018969664766,
1007.81187290831));
#145067=CARTESIAN_POINT('Ctrl Pts',(16.784203177988,-35.630403856542,1003.25656263356));
#145068=CARTESIAN_POINT('Ctrl Pts',(11.5967237879651,-37.639755608264,1000.99845840472));
#145069=CARTESIAN_POINT('Ctrl Pts',(0.737286909422714,-39.3788926554812,
996.442122710503));
#145070=CARTESIAN_POINT('Ctrl Pts',(-4.81870463978068,-39.0900264694501,
994.186770501551));
#145071=CARTESIAN_POINT('Ctrl Pts',(-15.4393561983312,-36.2333495478132,
989.620718069404));
#145072=CARTESIAN_POINT('Ctrl Pts',(-20.3879904968142,-33.6979990799886,
987.369448125984));
#145073=CARTESIAN_POINT('Ctrl Pts',(-28.9085862874412,-26.7490646841177,
982.807436091745));
#145074=CARTESIAN_POINT('Ctrl Pts',(-32.3884041854296,-22.4099933719744,
980.548212396911));
#145075=CARTESIAN_POINT('Ctrl Pts',(-37.3223319393225,-12.5816239153753,
976.000161533641));
#145076=CARTESIAN_POINT('Ctrl Pts',(-38.7232174803287,-7.19658426606107,
973.73990653827));
#145077=CARTESIAN_POINT('Ctrl Pts',(-38.9876796771853,-1.13252041238029,
971.222048993232));
#145078=CARTESIAN_POINT('Ctrl Pts',(-38.9999999999997,-0.566005030289253,
970.986826366361));
#145079=CARTESIAN_POINT('Ctrl Pts',(-39.,-2.11239359337867E-11,970.751815642467));
#145080=CARTESIAN_POINT('Ctrl Pts',(-39.,-2.45281572830436E-11,967.585684357552));
#145081=CARTESIAN_POINT('Ctrl Pts',(-38.9999999999985,-2.42407756834171,
968.592184642248));
#145082=CARTESIAN_POINT('Ctrl Pts',(-38.7738086935458,-4.85115479483614,
969.595638499149));
#145083=CARTESIAN_POINT('Ctrl Pts',(-37.2993818336415,-12.6484040123052,
972.890497539515));
#145084=CARTESIAN_POINT('Ctrl Pts',(-35.1462500049703,-17.7752282487208,
975.143115035084));
#145085=CARTESIAN_POINT('Ctrl Pts',(-28.8627288744489,-26.7988743877845,
979.70207752624));
#145086=CARTESIAN_POINT('Ctrl Pts',(-24.8001245103406,-30.5970173517883,
981.960114319475));
#145087=CARTESIAN_POINT('Ctrl Pts',(-15.3736672565857,-36.2615382735034,
986.51210400875));
#145088=CARTESIAN_POINT('Ctrl Pts',(-10.1096591876265,-38.0663982542976,
988.770196174658));
#145089=CARTESIAN_POINT('Ctrl Pts',(0.810854819229557,-39.3773377218996,
993.335378945768));
#145090=CARTESIAN_POINT('Ctrl Pts',(6.34808589841638,-38.8707401479934,
995.586418997613));
#145091=CARTESIAN_POINT('Ctrl Pts',(16.8464795008,-35.6008123867018,1000.15060324527));
#145092=CARTESIAN_POINT('Ctrl Pts',(21.6929555690272,-32.8729312097374,
1002.40689298906));
#145093=CARTESIAN_POINT('Ctrl Pts',(29.935698723851,-25.5948553290272,1006.9591977836));
#145094=CARTESIAN_POINT('Ctrl Pts',(33.2434856325897,-21.121642604465,1009.21774126761));
#145095=CARTESIAN_POINT('Ctrl Pts',(37.7877155770828,-11.1051856131721,
1013.77742081939));
#145096=CARTESIAN_POINT('Ctrl Pts',(38.9754514576547,-5.67093770419533,
1016.03105656495));
#145097=CARTESIAN_POINT('Ctrl Pts',(39.0237879021348,5.32646418474255,1020.59728343689));
#145098=CARTESIAN_POINT('Ctrl Pts',(37.8846828359875,10.7689854040637,1022.84923656495));
#145099=CARTESIAN_POINT('Ctrl Pts',(33.4311239339301,20.8230342782236,1027.40987077843));
#145100=CARTESIAN_POINT('Ctrl Pts',(30.1649685930785,25.3237652473569,1029.66837156485));
#145101=CARTESIAN_POINT('Ctrl Pts',(21.9874860148398,32.6772820623094,1034.21792943879));
#145102=CARTESIAN_POINT('Ctrl Pts',(17.1619696342435,35.4503243055008,1036.47767198415));
#145103=CARTESIAN_POINT('Ctrl Pts',(6.68953916182195,38.8134322237963,1041.04207544429));
#145104=CARTESIAN_POINT('Ctrl Pts',(1.1565875492231,39.3687375276673,1043.2933800649));
#145105=CARTESIAN_POINT('Ctrl Pts',(-9.77230555535638,38.1539649824231,
1047.85834285374));
#145106=CARTESIAN_POINT('Ctrl Pts',(-15.0486747245861,36.3971342631628,
1050.11337594687));
#145107=CARTESIAN_POINT('Ctrl Pts',(-24.5242177640814,30.8188324763402,
1054.66765286728));
#145108=CARTESIAN_POINT('Ctrl Pts',(-28.6218089207113,27.0561169484875,
1056.92581964375));
#145109=CARTESIAN_POINT('Ctrl Pts',(-34.9871035270197,18.0870581421282,
1061.48338582739));
#145110=CARTESIAN_POINT('Ctrl Pts',(-37.186573660034,12.9771776024501,1063.73807891462));
#145111=CARTESIAN_POINT('Ctrl Pts',(-38.752066982733,5.07858103950625,1067.08124972354));
#145112=CARTESIAN_POINT('Ctrl Pts',(-39.,2.53802064523472,1068.13187381312));
#145113=CARTESIAN_POINT('Ctrl Pts',(-39.,6.6818772737065E-12,1069.18568435754));
#145114=CARTESIAN_POINT('Origin',(0.,0.,-11.4051836540916));
#145115=CARTESIAN_POINT('',(-39.,-1.9327470101175E-12,1173.95181564246));
#145116=CARTESIAN_POINT('',(-39.,7.6522481211573E-11,1170.78568435748));
#145117=CARTESIAN_POINT('',(-39.,-4.77612251667468E-15,-11.4051836540916));
#145118=CARTESIAN_POINT('Ctrl Pts',(-39.,-3.89355214736042E-12,1173.95181564246));
#145119=CARTESIAN_POINT('Ctrl Pts',(-39.0000000000004,3.89628960201103,
1172.33403878377));
#145120=CARTESIAN_POINT('Ctrl Pts',(-38.4156384927199,7.78182406127406,
1170.72444552087));
#145121=CARTESIAN_POINT('Ctrl Pts',(-35.6349007362537,16.7748741585694,
1166.825507846));
#145122=CARTESIAN_POINT('Ctrl Pts',(-32.9156592349078,21.6289390011343,
1164.56950248956));
#145123=CARTESIAN_POINT('Ctrl Pts',(-25.6514842461451,29.8869780371979,
1160.00360544265));
#145124=CARTESIAN_POINT('Ctrl Pts',(-21.1870597913509,33.2014408747266,
1157.75246707764));
#145125=CARTESIAN_POINT('Ctrl Pts',(-11.183414353962,37.7644129148115,1153.18981684574));
#145126=CARTESIAN_POINT('Ctrl Pts',(-5.75222980330756,38.9631534505373,
1150.93141990017));
#145127=CARTESIAN_POINT('Ctrl Pts',(5.24445745961987,39.0351938236361,1146.38220728312));
#145128=CARTESIAN_POINT('Ctrl Pts',(10.6928461412629,37.9069188122571,1144.12252328313));
#145129=CARTESIAN_POINT('Ctrl Pts',(20.7591961881651,33.4707320654403,1139.5600317458));
#145130=CARTESIAN_POINT('Ctrl Pts',(25.2669350996321,30.2129607232191,1137.30761951472));
#145131=CARTESIAN_POINT('Ctrl Pts',(32.635081188955,22.0494206969798,1132.74163557832));
#145132=CARTESIAN_POINT('Ctrl Pts',(35.4150168873858,17.2334918475209,1130.488667703));
#145133=CARTESIAN_POINT('Ctrl Pts',(38.7992588732006,6.77153421948918,1125.93049079934));
#145134=CARTESIAN_POINT('Ctrl Pts',(39.3661250868372,1.23866868789697,1123.6725517893));
#145135=CARTESIAN_POINT('Ctrl Pts',(38.1742261404252,-9.69407731506407,
1119.1195268412));
#145136=CARTESIAN_POINT('Ctrl Pts',(36.4271546111516,-14.9772160932738,
1116.86211424447));
#145137=CARTESIAN_POINT('Ctrl Pts',(30.8650369918341,-24.4659196034356,
1112.29666213713));
#145138=CARTESIAN_POINT('Ctrl Pts',(27.1120874699223,-28.5686160683228,
1110.04564776162));
#145139=CARTESIAN_POINT('Ctrl Pts',(18.1577692119097,-34.950200646368,1105.48188630413));
#145140=CARTESIAN_POINT('Ctrl Pts',(13.0537483440062,-37.1593035688508,
1103.22498482583));
#145141=CARTESIAN_POINT('Ctrl Pts',(2.27187987206591,-39.3202697017892,
1098.67360080778));
#145142=CARTESIAN_POINT('Ctrl Pts',(-3.29118271115233,-39.2482698618276,
1096.41478130458));
#145143=CARTESIAN_POINT('Ctrl Pts',(-14.0163937440488,-36.807287473383,
1091.85420641104));
#145144=CARTESIAN_POINT('Ctrl Pts',(-19.0618186421746,-34.4657956797521,
1089.60098559052));
#145145=CARTESIAN_POINT('Ctrl Pts',(-27.8479269337317,-27.851744166451,
1085.03479176213));
#145146=CARTESIAN_POINT('Ctrl Pts',(-31.4926544757299,-23.6523090805093,
1082.78256529372));
#145147=CARTESIAN_POINT('Ctrl Pts',(-36.8043276295087,-14.0242385086279,
1078.22265613395));
#145148=CARTESIAN_POINT('Ctrl Pts',(-38.4124932907264,-8.70063483893357,
1075.96440277947));
#145149=CARTESIAN_POINT('Ctrl Pts',(-38.955687170905,-2.14833127284238,
1073.24382341729));
#145150=CARTESIAN_POINT('Ctrl Pts',(-38.9999999999934,-1.07354426693828,
1072.7975615313));
#145151=CARTESIAN_POINT('Ctrl Pts',(-39.,-2.40743813773037E-10,1072.35181564256));
#145152=CARTESIAN_POINT('Ctrl Pts',(-39.,6.7390537594747E-12,1069.18568435754));
#145153=CARTESIAN_POINT('Ctrl Pts',(-39.,-2.92908286305145,1070.40186769016));
#145154=CARTESIAN_POINT('Ctrl Pts',(-38.6698735170771,-5.85801370569777,
1071.61450745359));
#145155=CARTESIAN_POINT('Ctrl Pts',(-36.7798486915294,-14.0884527735446,
1075.1178764091));
#145156=CARTESIAN_POINT('Ctrl Pts',(-34.42890930272,-19.1275658806115,1077.37717345445));
#145157=CARTESIAN_POINT('Ctrl Pts',(-27.7984595898942,-27.9017290234602,
1081.92417113998));
#145158=CARTESIAN_POINT('Ctrl Pts',(-23.5874503239633,-31.5419326682777,
1084.18572159625));
#145159=CARTESIAN_POINT('Ctrl Pts',(-13.9449101522654,-36.8343930863333,
1088.74916602945));
#145160=CARTESIAN_POINT('Ctrl Pts',(-8.61794438291774,-38.4313537265566,
1091.0009100477));
#145161=CARTESIAN_POINT('Ctrl Pts',(2.3429835031869,-39.3158318656711,1095.56646343224));
#145162=CARTESIAN_POINT('Ctrl Pts',(7.85682919037316,-38.5938481919951,
1097.82041211834));
#145163=CARTESIAN_POINT('Ctrl Pts',(18.2197211130999,-34.9181476162326,
1102.37658946879));
#145164=CARTESIAN_POINT('Ctrl Pts',(22.9573494361813,-32.0030078391976,
1104.63456736523));
#145165=CARTESIAN_POINT('Ctrl Pts',(30.9111507093045,-24.4078483224121,
1109.1899697186));
#145166=CARTESIAN_POINT('Ctrl Pts',(34.0421550841879,-19.8086620493969,
1111.44588305573));
#145167=CARTESIAN_POINT('Ctrl Pts',(38.1919195816138,-9.6232672276592,1116.01180423757));
#145168=CARTESIAN_POINT('Ctrl Pts',(39.166468806553,-4.14905254858988,1118.26295789616));
#145169=CARTESIAN_POINT('Ctrl Pts',(38.7871156041852,6.83953168245799,1122.82552359188));
#145170=CARTESIAN_POINT('Ctrl Pts',(37.4368627370235,12.2350688954627,1125.08403118664));
#145171=CARTESIAN_POINT('Ctrl Pts',(32.595228404851,22.1088711917865,1129.63308690113));
#145172=CARTESIAN_POINT('Ctrl Pts',(29.1546851162566,26.4816299228362,1131.89284389154));
#145173=CARTESIAN_POINT('Ctrl Pts',(20.6933554732093,33.5114768607126,1136.45546432974));
#145174=CARTESIAN_POINT('Ctrl Pts',(15.7667043480505,36.0922683185844,1138.7078265675));
#145175=CARTESIAN_POINT('Ctrl Pts',(5.17342299714505,39.0443477133479,1143.27378879888));
#145176=CARTESIAN_POINT('Ctrl Pts',(-0.37691182012992,39.3836826504988,
1145.52681502005));
#145177=CARTESIAN_POINT('Ctrl Pts',(-11.2497965798242,37.7449090321416,
1150.08486559052));
#145178=CARTESIAN_POINT('Ctrl Pts',(-16.4544474528643,35.7837625096039,
1152.34279527611));
#145179=CARTESIAN_POINT('Ctrl Pts',(-25.7070652977076,29.8394562917062,
1156.89598098112));
#145180=CARTESIAN_POINT('Ctrl Pts',(-29.6557870721231,25.9188866020372,
1159.1532894125));
#145181=CARTESIAN_POINT('Ctrl Pts',(-35.6662892255865,16.7077054790432,
1163.71877878532));
#145182=CARTESIAN_POINT('Ctrl Pts',(-37.6636877096582,11.5185699648607,
1165.96979605541));
#145183=CARTESIAN_POINT('Ctrl Pts',(-38.8408829296079,4.06949041451221,
1169.09987601447));
#145184=CARTESIAN_POINT('Ctrl Pts',(-38.9999999999999,2.032982257003,1169.94157060178));
#145185=CARTESIAN_POINT('Ctrl Pts',(-39.,1.53110857326055E-10,1170.78568435748));
#145186=CARTESIAN_POINT('Origin',(0.,0.,-11.4051836540916));
#145187=CARTESIAN_POINT('',(-39.,-6.92868819070596E-11,1275.55181564252));
#145188=CARTESIAN_POINT('',(-39.,7.90570704135022E-14,1272.38568435754));
#145189=CARTESIAN_POINT('',(-39.,-4.77612251667468E-15,-11.4051836540916));
#145190=CARTESIAN_POINT('Ctrl Pts',(-39.,-1.38611622180207E-10,1275.55181564252));
#145191=CARTESIAN_POINT('Ctrl Pts',(-39.0000000000121,3.39009799570675,
1274.14421439965));
#145192=CARTESIAN_POINT('Ctrl Pts',(-38.5578414158399,6.77504194114251,
1272.74016932084));
#145193=CARTESIAN_POINT('Ctrl Pts',(-36.2593020322943,15.3782008352702,
1269.0535111035));
#145194=CARTESIAN_POINT('Ctrl Pts',(-33.7316775642524,20.3324889403378,
1266.79557053843));
#145195=CARTESIAN_POINT('Ctrl Pts',(-26.7960837422303,28.8649715059958,
1262.23737458539));
#145196=CARTESIAN_POINT('Ctrl Pts',(-22.463919094978,32.3511642572694,1259.98441546151));
#145197=CARTESIAN_POINT('Ctrl Pts',(-12.6439735093029,37.3010853753511,
1255.4184283221));
#145198=CARTESIAN_POINT('Ctrl Pts',(-7.2636870838922,38.7101148932136,1253.16600845434));
#145199=CARTESIAN_POINT('Ctrl Pts',(3.72546313492805,39.2095936708073,1248.6035364724));
#145200=CARTESIAN_POINT('Ctrl Pts',(9.21344617495873,38.2931199921262,1246.34386337045));
#145201=CARTESIAN_POINT('Ctrl Pts',(19.441245138911,34.2527873764992,1241.79462707815));
#145202=CARTESIAN_POINT('Ctrl Pts',(24.0724262610235,31.1727116195146,1239.53624680028));
#145203=CARTESIAN_POINT('Ctrl Pts',(31.7520139165969,23.3032636376238,1234.97338516403));
#145204=CARTESIAN_POINT('Ctrl Pts',(34.7175002768481,18.5992083269852,1232.72205531739));
#145205=CARTESIAN_POINT('Ctrl Pts',(38.5061843592954,8.27628254398474,1228.15704489311));
#145206=CARTESIAN_POINT('Ctrl Pts',(39.2879009775359,2.77035504833265,1225.90209366215));
#145207=CARTESIAN_POINT('Ctrl Pts',(38.5229871029467,-8.198586862572,1221.34768364638));
#145208=CARTESIAN_POINT('Ctrl Pts',(36.983616651298,-13.5444717146089,1219.08953055696));
#145209=CARTESIAN_POINT('Ctrl Pts',(31.7965405177819,-23.242618137828,1214.5321177159));
#145210=CARTESIAN_POINT('Ctrl Pts',(28.2046521619375,-27.4908386398366,
1212.27734410354));
#145211=CARTESIAN_POINT('Ctrl Pts',(19.5036771475858,-34.2174696969444,
1207.71118909283));
#145212=CARTESIAN_POINT('Ctrl Pts',(14.4906255946235,-36.6230170530299,
1205.45975193439));
#145213=CARTESIAN_POINT('Ctrl Pts',(3.8025676904283,-39.2015111663801,1200.89838937249));
#145214=CARTESIAN_POINT('Ctrl Pts',(-1.75779254886071,-39.3462572065711,
1198.63834207664));
#145215=CARTESIAN_POINT('Ctrl Pts',(-12.5684694905614,-37.3268034371924,
1194.09142647996));
#145216=CARTESIAN_POINT('Ctrl Pts',(-17.7036431989977,-35.183323529683,
1191.83054903452));
#145217=CARTESIAN_POINT('Ctrl Pts',(-26.7439367605968,-28.9135770053946,
1187.2662842232));
#145218=CARTESIAN_POINT('Ctrl Pts',(-30.5497675463814,-24.8585963968017,
1185.01450274688));
#145219=CARTESIAN_POINT('Ctrl Pts',(-36.2314872565174,-15.4435624601413,
1180.44891476071));
#145220=CARTESIAN_POINT('Ctrl Pts',(-38.0452931856009,-10.1867875622354,
1178.19503602378));
#145221=CARTESIAN_POINT('Ctrl Pts',(-38.904245474371,-3.15764135812629,
1175.26062781204));
#145222=CARTESIAN_POINT('Ctrl Pts',(-38.9999999999998,-1.57742956945571,
1174.6067795477));
#145223=CARTESIAN_POINT('Ctrl Pts',(-39.,-3.85858012208473E-12,1173.95181564246));
#145224=CARTESIAN_POINT('Ctrl Pts',(-39.,1.53028145710721E-10,1170.78568435748));
#145225=CARTESIAN_POINT('Ctrl Pts',(-39.0000000000002,-3.43671147175983,
1172.21263996323));
#145226=CARTESIAN_POINT('Ctrl Pts',(-38.5455980291902,-6.86767714357309,
1173.63607290253));
#145227=CARTESIAN_POINT('Ctrl Pts',(-36.2037036727293,-15.5092640042679,
1177.34172285394));
#145228=CARTESIAN_POINT('Ctrl Pts',(-33.6573303360208,-20.4558930289092,
1179.60059198728));
#145229=CARTESIAN_POINT('Ctrl Pts',(-26.6876907218572,-28.9655440023475,
1184.16130566822));
#145230=CARTESIAN_POINT('Ctrl Pts',(-22.3411840840882,-32.4363266018347,
1186.41446414357));
#145231=CARTESIAN_POINT('Ctrl Pts',(-12.5020145840668,-37.3487112574047,
1190.98064938005));
#145232=CARTESIAN_POINT('Ctrl Pts',(-7.11759788381116,-38.7370446357954,
1193.23292212716));
#145233=CARTESIAN_POINT('Ctrl Pts',(3.86889336978166,-39.1952716515687,
1197.79271440655));
#145234=CARTESIAN_POINT('Ctrl Pts',(9.35082466511408,-38.2594188534342,
1200.05093475405));
#145235=CARTESIAN_POINT('Ctrl Pts',(19.5648565769327,-34.1828573801283,
1204.60175915323));
#145236=CARTESIAN_POINT('Ctrl Pts',(24.1875101948081,-31.0841055881524,
1206.86063323524));
#145237=CARTESIAN_POINT('Ctrl Pts',(31.8397140269745,-23.1832893296027,
1211.42546008912));
#145238=CARTESIAN_POINT('Ctrl Pts',(34.7873038977391,-18.4682792629896,
1213.67660659029));
#145239=CARTESIAN_POINT('Ctrl Pts',(38.5370384484279,-8.13136021947425,
1218.24119272561));
#145240=CARTESIAN_POINT('Ctrl Pts',(39.2980535938245,-2.62237187735175,
1220.49685037152));
#145241=CARTESIAN_POINT('Ctrl Pts',(38.4918215306549,8.34385191811939,1225.05013179966));
#145242=CARTESIAN_POINT('Ctrl Pts',(36.9323013274488,13.6840218885835,1227.30844969847));
#145243=CARTESIAN_POINT('Ctrl Pts',(31.7082793287542,23.3628496115169,1231.86711830015));
#145244=CARTESIAN_POINT('Ctrl Pts',(28.1005812757189,27.5971767593091,1234.12124709457));
#145245=CARTESIAN_POINT('Ctrl Pts',(19.3744690646522,34.2907832826383,1238.68746778651));
#145246=CARTESIAN_POINT('Ctrl Pts',(14.3523225347968,36.6774118726178,1240.93916141839));
#145247=CARTESIAN_POINT('Ctrl Pts',(3.65283329393246,39.2160289927788,1245.50055806714));
#145248=CARTESIAN_POINT('Ctrl Pts',(-1.90654130622282,39.3393075310152,
1247.75940496865));
#145249=CARTESIAN_POINT('Ctrl Pts',(-12.709415220828,37.2790572970399,1252.30773360844));
#145250=CARTESIAN_POINT('Ctrl Pts',(-17.8375195708604,35.1152800961424,
1254.56833596046));
#145251=CARTESIAN_POINT('Ctrl Pts',(-26.8522956797519,28.8129642019199,
1259.1322952039));
#145252=CARTESIAN_POINT('Ctrl Pts',(-30.6426963934833,24.7439215570187,
1261.38379193086));
#145253=CARTESIAN_POINT('Ctrl Pts',(-36.2890196037476,15.3078623613554,
1265.94906526269));
#145254=CARTESIAN_POINT('Ctrl Pts',(-38.0831767765695,10.0442011135505,
1268.20354950298));
#145255=CARTESIAN_POINT('Ctrl Pts',(-38.9100499980652,3.06047839876306,
1271.11697111921));
#145256=CARTESIAN_POINT('Ctrl Pts',(-39.,1.52893054872031,1271.75085771145));
#145257=CARTESIAN_POINT('Ctrl Pts',(-39.,2.20101714631937E-13,1272.38568435754));
#145258=CARTESIAN_POINT('Origin',(0.,0.,-11.4051836540916));
#145259=CARTESIAN_POINT('',(-39.,-1.43281722098234E-12,1377.15181564246));
#145260=CARTESIAN_POINT('',(-39.,1.04944080121118E-10,1373.98568435745));
#145261=CARTESIAN_POINT('',(-39.,-4.77612251667468E-15,-11.4051836540916));
#145262=CARTESIAN_POINT('Ctrl Pts',(-39.,-2.82135426132868E-12,1377.15181564246));
#145263=CARTESIAN_POINT('Ctrl Pts',(-39.0000000000002,2.88041777647212,
1375.95583852112));
#145264=CARTESIAN_POINT('Ctrl Pts',(-38.6807435490783,5.76111009139163,
1374.76337209935));
#145265=CARTESIAN_POINT('Ctrl Pts',(-36.8318578925542,13.9525788639201,
1371.27904717011));
#145266=CARTESIAN_POINT('Ctrl Pts',(-34.4972202638612,19.0052537775258,
1369.01829870079));
#145267=CARTESIAN_POINT('Ctrl Pts',(-27.8971802064615,27.8022114893361,
1364.47017676853));
#145268=CARTESIAN_POINT('Ctrl Pts',(-23.7038291806506,31.4542341225288,
1362.21126493798));
#145269=CARTESIAN_POINT('Ctrl Pts',(-14.0837403213775,36.7813840979505,
1357.64974505296));
#145270=CARTESIAN_POINT('Ctrl Pts',(-8.76363186995282,38.3982647036319,
1355.3980904166));
#145271=CARTESIAN_POINT('Ctrl Pts',(2.19501292647189,39.3246614391287,1350.83187501784));
#145272=CARTESIAN_POINT('Ctrl Pts',(7.71346452394935,38.6230551216481,1348.57766059682));
#145273=CARTESIAN_POINT('Ctrl Pts',(18.0926794494128,34.9843013980631,1344.01916268284));
#145274=CARTESIAN_POINT('Ctrl Pts',(22.8413040626638,32.0860501965724,1341.76087443117));
#145275=CARTESIAN_POINT('Ctrl Pts',(30.8210535135947,24.5209404045838,1337.20743429205));
#145276=CARTESIAN_POINT('Ctrl Pts',(33.967642327505,19.9354390322161,1334.9518776128));
#145277=CARTESIAN_POINT('Ctrl Pts',(38.1552177008476,9.76797933073579,1330.38722910559));
#145278=CARTESIAN_POINT('Ctrl Pts',(39.150558748526,4.29721574010371,1328.13606088376));
#145279=CARTESIAN_POINT('Ctrl Pts',(38.8125265088509,-6.69666200815592,
1323.57129726886));
#145280=CARTESIAN_POINT('Ctrl Pts',(37.4811251675765,-12.1002914500509,
1321.31228975546));
#145281=CARTESIAN_POINT('Ctrl Pts',(32.6740393585401,-21.9915389253384,
1316.76166173402));
#145282=CARTESIAN_POINT('Ctrl Pts',(29.2510655423101,-26.3744760051109,
1314.50340324433));
#145283=CARTESIAN_POINT('Ctrl Pts',(20.8195296146921,-33.4330110139997,
1309.94347646719));
#145284=CARTESIAN_POINT('Ctrl Pts',(15.9037342957803,-36.0319016450438,
1307.69125692304));
#145285=CARTESIAN_POINT('Ctrl Pts',(5.32145177615644,-39.0246868645341,
1303.12506187543));
#145286=CARTESIAN_POINT('Ctrl Pts',(-0.229142101628406,-39.3850633927897,
1300.87183155197));
#145287=CARTESIAN_POINT('Ctrl Pts',(-11.1117677761475,-37.7860696001166,
1296.31127770666));
#145288=CARTESIAN_POINT('Ctrl Pts',(-16.3250416871503,-35.8432420952935,
1294.05246556515));
#145289=CARTESIAN_POINT('Ctrl Pts',(-25.5977941436226,-29.9327097697844,
1289.50105926183));
#145290=CARTESIAN_POINT('Ctrl Pts',(-29.5588628263736,-26.0287293417693,
1287.2441727584));
#145291=CARTESIAN_POINT('Ctrl Pts',(-35.6025966941331,-16.8429885383189,
1282.68040050665));
#145292=CARTESIAN_POINT('Ctrl Pts',(-37.6196980955947,-11.6614777857802,
1280.42938649254));
#145293=CARTESIAN_POINT('Ctrl Pts',(-38.8330920305166,-4.16786431624148,
1277.27836870029));
#145294=CARTESIAN_POINT('Ctrl Pts',(-38.9999999999926,-2.08216040212245,
1276.41634863633));
#145295=CARTESIAN_POINT('Ctrl Pts',(-39.,-1.38562772367123E-10,1275.55181564252));
#145296=CARTESIAN_POINT('Ctrl Pts',(-39.,2.647881913731E-13,1272.38568435754));
#145297=CARTESIAN_POINT('Ctrl Pts',(-39.,-3.94534185592291,1274.0238281831));
#145298=CARTESIAN_POINT('Ctrl Pts',(-38.4007569452698,-7.87952769446106,
1275.65311463225));
#145299=CARTESIAN_POINT('Ctrl Pts',(-35.5715404036943,-16.9087570846571,
1279.57333127736));
#145300=CARTESIAN_POINT('Ctrl Pts',(-32.8342767055597,-21.7522446139334,
1281.82859776841));
#145301=CARTESIAN_POINT('Ctrl Pts',(-25.5393666793081,-29.98282822353,1286.39466764876));
#145302=CARTESIAN_POINT('Ctrl Pts',(-21.0625296728186,-33.2805482709015,
1288.64595911512));
#145303=CARTESIAN_POINT('Ctrl Pts',(-11.0421380925384,-37.8059505035515,
1293.20788033371));
#145304=CARTESIAN_POINT('Ctrl Pts',(-5.60631950711533,-38.9844311981042,
1295.46722018366));
#145305=CARTESIAN_POINT('Ctrl Pts',(5.39098520885725,-39.0152716393876,
1300.01510968091));
#145306=CARTESIAN_POINT('Ctrl Pts',(10.8354276405026,-37.8665138835699,
1302.27544940074));
#145307=CARTESIAN_POINT('Ctrl Pts',(20.8855354501616,-33.3920330986026,
1306.83899128012));
#145308=CARTESIAN_POINT('Ctrl Pts',(25.3806943553124,-30.1174311355258,
1309.09101442429));
#145309=CARTESIAN_POINT('Ctrl Pts',(32.7178846802067,-21.926349624505,1313.65679019088));
#145310=CARTESIAN_POINT('Ctrl Pts',(35.4797105811817,-17.0998751609009,
1315.91026833225));
#145311=CARTESIAN_POINT('Ctrl Pts',(38.8244745123745,-6.62538734318276,
1320.46737521405));
#145312=CARTESIAN_POINT('Ctrl Pts',(39.3705647181445,-1.08999955230238,
1322.7252872927));
#145313=CARTESIAN_POINT('Ctrl Pts',(38.1372954002353,9.83823489768537,1327.27962723063));
#145314=CARTESIAN_POINT('Ctrl Pts',(36.3704386297287,15.1143662728797,1329.53619924304));
#145315=CARTESIAN_POINT('Ctrl Pts',(30.7727670954361,24.5818543154064,1334.10193326534));
#145316=CARTESIAN_POINT('Ctrl Pts',(27.0044017377237,28.6703866293253,1336.35299830247));
#145317=CARTESIAN_POINT('Ctrl Pts',(18.0264084499264,35.0181220236859,1340.91613461669));
#145318=CARTESIAN_POINT('Ctrl Pts',(12.913961529755,37.2081229471099,1343.17388755452));
#145319=CARTESIAN_POINT('Ctrl Pts',(2.12369724136763,39.3285926079057,1347.72402300653));
#145320=CARTESIAN_POINT('Ctrl Pts',(-3.43930503697113,39.2356616772837,
1349.9833053519));
#145321=CARTESIAN_POINT('Ctrl Pts',(-14.155752083824,36.7539032180833,1354.54501354965));
#145322=CARTESIAN_POINT('Ctrl Pts',(-19.1919795822001,34.3934611066868,
1356.79774204446));
#145323=CARTESIAN_POINT('Ctrl Pts',(-27.9528668502543,27.746409001408,1361.36383642538));
#145324=CARTESIAN_POINT('Ctrl Pts',(-31.5817648869465,23.5331615977101,
1363.61647367641));
#145325=CARTESIAN_POINT('Ctrl Pts',(-36.8569517582067,13.88531067212,1368.17539050311));
#145326=CARTESIAN_POINT('Ctrl Pts',(-38.4451521731786,8.55535292592722,
1370.43341966595));
#145327=CARTESIAN_POINT('Ctrl Pts',(-38.9596487804728,2.05002493395998,
1373.13449431865));
#145328=CARTESIAN_POINT('Ctrl Pts',(-38.9999999999999,1.02442168325448,
1373.56033463717));
#145329=CARTESIAN_POINT('Ctrl Pts',(-39.,2.09992717659091E-10,1373.98568435745));
#145330=CARTESIAN_POINT('Origin',(0.,0.,-11.4051836540916));
#145331=CARTESIAN_POINT('',(-39.,1.80311138088147E-11,1478.75181564244));
#145332=CARTESIAN_POINT('',(-39.,7.02754413066815E-12,1475.58568435754));
#145333=CARTESIAN_POINT('',(-39.,-4.77612251667468E-15,-11.4051836540916));
#145334=CARTESIAN_POINT('Ctrl Pts',(-39.,3.61144447680317E-11,1478.75181564244));
#145335=CARTESIAN_POINT('Ctrl Pts',(-39.,2.37441675948014,1477.76593500248));
#145336=CARTESIAN_POINT('Ctrl Pts',(-38.7829742622338,4.75198370846709,
1476.78303645826));
#145337=CARTESIAN_POINT('Ctrl Pts',(-37.347229177159,12.5070764604314,1473.50833436143));
#145338=CARTESIAN_POINT('Ctrl Pts',(-35.2129213102348,17.6432711332436,
1471.25554123724));
#145339=CARTESIAN_POINT('Ctrl Pts',(-28.9606169290237,26.6935870925475,
1466.69398715833));
#145340=CARTESIAN_POINT('Ctrl Pts',(-24.9101561368435,30.5078998124061,
1464.43477569376));
#145341=CARTESIAN_POINT('Ctrl Pts',(-15.5045799938302,36.2052856351559,
1459.88446463748));
#145342=CARTESIAN_POINT('Ctrl Pts',(-10.2501188711739,38.0283506563109,
1457.6268328815));
#145343=CARTESIAN_POINT('Ctrl Pts',(0.661883501075245,39.3800839171634,
1453.06360630778));
#145344=CARTESIAN_POINT('Ctrl Pts',(6.20091300299922,38.894467021419,1450.8125518839));
#145345=CARTESIAN_POINT('Ctrl Pts',(16.7141980976748,35.6635485592597,1446.24685311034));
#145346=CARTESIAN_POINT('Ctrl Pts',(21.5730610713052,32.9522007088133,1443.99016817262));
#145347=CARTESIAN_POINT('Ctrl Pts',(29.8429570127381,25.7026634234135,1439.43600737227));
#145348=CARTESIAN_POINT('Ctrl Pts',(33.1661994321955,21.2423835839676,1437.17809842454));
#145349=CARTESIAN_POINT('Ctrl Pts',(37.7458046507818,11.2458863025301,1432.620840729));
#145350=CARTESIAN_POINT('Ctrl Pts',(38.953532270286,5.81783508378545,1430.36743663771));
#145351=CARTESIAN_POINT('Ctrl Pts',(39.0438479909382,-5.1785588031054,1425.80162829789));
#145352=CARTESIAN_POINT('Ctrl Pts',(37.9251153602865,-10.6263433292262,
1423.54955488541));
#145353=CARTESIAN_POINT('Ctrl Pts',(33.5072026416274,-20.7013434890943,
1418.98615553982));
#145354=CARTESIAN_POINT('Ctrl Pts',(30.2553113772127,-25.216458746652,1416.72591321134));
#145355=CARTESIAN_POINT('Ctrl Pts',(22.1036478741556,-32.5982400550239,
1412.17783801107));
#145356=CARTESIAN_POINT('Ctrl Pts',(17.2911749160037,-35.386920041304,1409.91863180754));
#145357=CARTESIAN_POINT('Ctrl Pts',(6.83547549740724,-38.7879054736836,
1405.35660612111));
#145358=CARTESIAN_POINT('Ctrl Pts',(1.30509855894386,-39.3640200220915,
1403.10533935717));
#145359=CARTESIAN_POINT('Ctrl Pts',(-9.63023925437765,-38.1904256013885,
1398.53928964146));
#145360=CARTESIAN_POINT('Ctrl Pts',(-14.9152855697462,-36.4523671333016,
1396.28392440178));
#145361=CARTESIAN_POINT('Ctrl Pts',(-24.4127757610747,-30.9071429022493,
1391.72761197885));
#145362=CARTESIAN_POINT('Ctrl Pts',(-28.5238375105124,-27.1592675983071,
1389.46950898569));
#145363=CARTESIAN_POINT('Ctrl Pts',(-34.9199771510344,-18.2156415998711,
1384.91417895116));
#145364=CARTESIAN_POINT('Ctrl Pts',(-37.1375385041311,-13.1159035068419,
1382.65978177388));
#145365=CARTESIAN_POINT('Ctrl Pts',(-38.7423587002407,-5.17687524663117,
1379.2971087506));
#145366=CARTESIAN_POINT('Ctrl Pts',(-38.9999999999998,-2.58728858011592,
1378.22608270656));
#145367=CARTESIAN_POINT('Ctrl Pts',(-39.,-2.84605672362659E-12,1377.15181564246));
#145368=CARTESIAN_POINT('Ctrl Pts',(-39.0000000000001,2.09855327559794E-10,
1373.98568435745));
#145369=CARTESIAN_POINT('Ctrl Pts',(-39.0000000000004,-4.45618022580496,
1375.83593317984));
#145370=CARTESIAN_POINT('Ctrl Pts',(-38.2350734620249,-8.8927699197193,
1377.6702641004));
#145371=CARTESIAN_POINT('Ctrl Pts',(-34.8846175646687,-18.2837541637938,
1381.80872310428));
#145372=CARTESIAN_POINT('Ctrl Pts',(-31.9621762762703,-23.0141664573471,
1384.05975861463));
#145373=CARTESIAN_POINT('Ctrl Pts',(-24.3541829842684,-30.9531169708647,
1388.62391993159));
#145374=CARTESIAN_POINT('Ctrl Pts',(-19.7514891007839,-34.0748091144117,
1390.8802448956));
#145375=CARTESIAN_POINT('Ctrl Pts',(-9.56160343469945,-38.2075719539005,
1395.43249606781));
#145376=CARTESIAN_POINT('Ctrl Pts',(-4.08276794280321,-39.1737724321858,
1397.69105399931));
#145377=CARTESIAN_POINT('Ctrl Pts',(6.90909010052654,-38.7750050144413,
1402.25078717627));
#145378=CARTESIAN_POINT('Ctrl Pts',(12.3028022100999,-37.4150548403148,
1404.50439747286));
#145379=CARTESIAN_POINT('Ctrl Pts',(22.1679831917244,-32.554688309711,1409.07062342063));
#145380=CARTESIAN_POINT('Ctrl Pts',(26.5316025562092,-29.1083189220235,
1411.32259173001));
#145381=CARTESIAN_POINT('Ctrl Pts',(33.5450503237739,-20.6390004187557,
1415.883183882));
#145382=CARTESIAN_POINT('Ctrl Pts',(36.1172600369038,-15.708662448361,1418.14166822648));
#145383=CARTESIAN_POINT('Ctrl Pts',(39.0530359196965,-5.11023800956806,
1422.69129154581));
#145384=CARTESIAN_POINT('Ctrl Pts',(39.383501308142,0.445475200229383,1424.95098876778));
#145385=CARTESIAN_POINT('Ctrl Pts',(37.7242291732344,11.3187887239687,1429.51541498531));
#145386=CARTESIAN_POINT('Ctrl Pts',(35.7541933445629,16.5188612851454,1431.7667104148));
#145387=CARTESIAN_POINT('Ctrl Pts',(29.793792131418,25.7595209126659,1436.33165519177));
#145388=CARTESIAN_POINT('Ctrl Pts',(25.8685919165449,29.6989887557016,1438.58671904772));
#145389=CARTESIAN_POINT('Ctrl Pts',(16.6504672755713,35.6931331713202,1443.14094612052));
#145390=CARTESIAN_POINT('Ctrl Pts',(11.4554285550858,37.6830845947796,1445.39911843335));
#145391=CARTESIAN_POINT('Ctrl Pts',(0.589091599192387,39.3813659275958,
1449.95674167307));
#145392=CARTESIAN_POINT('Ctrl Pts',(-4.96540523733698,39.0716402290369,
1452.21140492066));
#145393=CARTESIAN_POINT('Ctrl Pts',(-15.5750437562469,36.1752198940577,
1456.77757513838));
#145394=CARTESIAN_POINT('Ctrl Pts',(-20.5141684009702,33.6213054232799,
1459.02905048086));
#145395=CARTESIAN_POINT('Ctrl Pts',(-29.0101491441578,26.639311686823,1463.59117855446));
#145396=CARTESIAN_POINT('Ctrl Pts',(-32.4723478199063,22.2881206444973,
1465.85045056518));
#145397=CARTESIAN_POINT('Ctrl Pts',(-37.3695418329642,12.4409805236918,
1470.39751689979));
#145398=CARTESIAN_POINT('Ctrl Pts',(-38.7501977411297,7.0486479464448,1472.65901804226));
#145399=CARTESIAN_POINT('Ctrl Pts',(-38.9897218108706,1.0343759573043,1475.15620152699));
#145400=CARTESIAN_POINT('Ctrl Pts',(-39.,0.516968414109846,1475.37103410757));
#145401=CARTESIAN_POINT('Ctrl Pts',(-39.,1.41471556691641E-11,1475.58568435754));
#145402=CARTESIAN_POINT('Origin',(-51.0189817055138,1.6136547197417E-13,
1492.25));
#145403=CARTESIAN_POINT('',(-10.2149882823905,-5.15937500000011,1492.25));
#145404=CARTESIAN_POINT('',(-51.0189817055139,-5.15937499999986,1492.25));
#145405=CARTESIAN_POINT('',(-10.2149882823904,5.15937499999993,1492.25));
#145406=CARTESIAN_POINT('Ctrl Pts',(-10.2149882823905,-5.15937500000011,
1492.25));
#145407=CARTESIAN_POINT('Ctrl Pts',(-10.2149882823905,-5.15937500000011,
1491.59113903279));
#145408=CARTESIAN_POINT('Ctrl Pts',(-10.2855048387883,-5.02575113964846,
1490.89625255689));
#145409=CARTESIAN_POINT('Ctrl Pts',(-10.5275891593601,-4.49662578128932,
1489.62870790392));
#145410=CARTESIAN_POINT('Ctrl Pts',(-10.6944718935536,-4.10147232415352,
1489.05501422578));
#145411=CARTESIAN_POINT('Ctrl Pts',(-10.9990970108091,-3.1957609090983,
1488.14930281073));
#145412=CARTESIAN_POINT('Ctrl Pts',(-11.1582376083003,-2.62178859469202,
1487.7535702398));
#145413=CARTESIAN_POINT('Ctrl Pts',(-11.3819664861004,-1.35310050851121,
1487.22399004237));
#145414=CARTESIAN_POINT('Ctrl Pts',(-11.444,-0.657734185748201,1487.090625));
#145415=CARTESIAN_POINT('Ctrl Pts',(-11.444,0.657734185748043,1487.090625));
#145416=CARTESIAN_POINT('Ctrl Pts',(-11.3819664861004,1.35310050851105,
1487.22399004237));
#145417=CARTESIAN_POINT('Ctrl Pts',(-11.1582376083003,2.62178859469186,
1487.7535702398));
#145418=CARTESIAN_POINT('Ctrl Pts',(-10.999097010809,3.19576090909814,1488.14930281073));
#145419=CARTESIAN_POINT('Ctrl Pts',(-10.6944718935536,4.10147232415335,
1489.05501422578));
#145420=CARTESIAN_POINT('Ctrl Pts',(-10.52758915936,4.49662578128915,1489.62870790392));
#145421=CARTESIAN_POINT('Ctrl Pts',(-10.2855048387882,5.02575113964829,
1490.89625255689));
#145422=CARTESIAN_POINT('Ctrl Pts',(-10.2149882823904,5.15937499999993,
1491.59113903279));
#145423=CARTESIAN_POINT('Ctrl Pts',(-10.2149882823904,5.15937499999993,
1492.25));
#145424=CARTESIAN_POINT('Ctrl Pts',(-10.2149882823904,5.15937499999994,
1492.25));
#145425=CARTESIAN_POINT('Ctrl Pts',(-10.2149882823904,5.15937499999994,
1492.90886096721));
#145426=CARTESIAN_POINT('Ctrl Pts',(-10.2855048387882,5.02575113964829,
1493.60374744311));
#145427=CARTESIAN_POINT('Ctrl Pts',(-10.52758915936,4.49662578128915,1494.87129209608));
#145428=CARTESIAN_POINT('Ctrl Pts',(-10.6944718935536,4.10147232415335,
1495.44498577422));
#145429=CARTESIAN_POINT('Ctrl Pts',(-10.999097010809,3.19576090909814,1496.35069718927));
#145430=CARTESIAN_POINT('Ctrl Pts',(-11.1582376083003,2.62178859469186,
1496.7464297602));
#145431=CARTESIAN_POINT('Ctrl Pts',(-11.3819664861004,1.35310050851105,
1497.27600995763));
#145432=CARTESIAN_POINT('Ctrl Pts',(-11.444,0.657734185748043,1497.409375));
#145433=CARTESIAN_POINT('Ctrl Pts',(-11.444,-0.657734185748201,1497.409375));
#145434=CARTESIAN_POINT('Ctrl Pts',(-11.3819664861004,-1.35310050851147,
1497.27600995763));
#145435=CARTESIAN_POINT('Ctrl Pts',(-11.1582376083003,-2.62178859469227,
1496.7464297602));
#145436=CARTESIAN_POINT('Ctrl Pts',(-10.9990970108091,-3.1957609090983,
1496.35069718927));
#145437=CARTESIAN_POINT('Ctrl Pts',(-10.6944718935536,-4.10147232415352,
1495.44498577422));
#145438=CARTESIAN_POINT('Ctrl Pts',(-10.5275891593601,-4.49662578128932,
1494.87129209608));
#145439=CARTESIAN_POINT('Ctrl Pts',(-10.2855048387883,-5.02575113964846,
1493.60374744311));
#145440=CARTESIAN_POINT('Ctrl Pts',(-10.2149882823905,-5.1593750000001,
1492.90886096721));
#145441=CARTESIAN_POINT('Ctrl Pts',(-10.2149882823905,-5.15937500000009,
1492.25));
#145442=CARTESIAN_POINT('Origin',(-51.0189817055138,1.6136547197417E-13,
1492.25));
#145443=CARTESIAN_POINT('',(10.2149882823905,5.15937499999981,1492.25));
#145444=CARTESIAN_POINT('',(10.2149882823904,-5.15937500000023,1492.25));
#145445=CARTESIAN_POINT('Ctrl Pts',(10.2149882823905,5.15937499999981,1492.25));
#145446=CARTESIAN_POINT('Ctrl Pts',(10.2149882823905,5.15937499999981,1491.59113903279));
#145447=CARTESIAN_POINT('Ctrl Pts',(10.2855048387883,5.02575113964801,1490.89625255689));
#145448=CARTESIAN_POINT('Ctrl Pts',(10.5275891593602,4.49662578128873,1489.62870790392));
#145449=CARTESIAN_POINT('Ctrl Pts',(10.6944718935536,4.10147232415322,1489.05501422578));
#145450=CARTESIAN_POINT('Ctrl Pts',(10.9990970108091,3.19576090909801,1488.14930281073));
#145451=CARTESIAN_POINT('Ctrl Pts',(11.1582376083003,2.6217885946917,1487.7535702398));
#145452=CARTESIAN_POINT('Ctrl Pts',(11.3819664861004,1.35310050851075,1487.22399004237));
#145453=CARTESIAN_POINT('Ctrl Pts',(11.444,0.657734185747904,1487.090625));
#145454=CARTESIAN_POINT('Ctrl Pts',(11.444,-0.657734185748342,1487.090625));
#145455=CARTESIAN_POINT('Ctrl Pts',(11.3819664861004,-1.35310050851134,
1487.22399004237));
#145456=CARTESIAN_POINT('Ctrl Pts',(11.1582376083003,-2.62178859469216,
1487.7535702398));
#145457=CARTESIAN_POINT('Ctrl Pts',(10.999097010809,-3.19576090909844,1488.14930281073));
#145458=CARTESIAN_POINT('Ctrl Pts',(10.6944718935536,-4.10147232415365,
1489.05501422578));
#145459=CARTESIAN_POINT('Ctrl Pts',(10.5275891593601,-4.49662578128945,
1489.62870790392));
#145460=CARTESIAN_POINT('Ctrl Pts',(10.2855048387882,-5.02575113964858,
1490.89625255689));
#145461=CARTESIAN_POINT('Ctrl Pts',(10.2149882823905,-5.15937500000024,
1491.59113903279));
#145462=CARTESIAN_POINT('Ctrl Pts',(10.2149882823905,-5.15937500000024,
1492.25));
#145463=CARTESIAN_POINT('',(-51.0189817055139,-5.15937499999986,1492.25));
#145464=CARTESIAN_POINT('Ctrl Pts',(10.2149882823905,-5.15937500000024,
1492.25));
#145465=CARTESIAN_POINT('Ctrl Pts',(10.2149882823905,-5.15937500000024,
1492.90886096721));
#145466=CARTESIAN_POINT('Ctrl Pts',(10.2855048387882,-5.02575113964858,
1493.60374744311));
#145467=CARTESIAN_POINT('Ctrl Pts',(10.5275891593601,-4.49662578128945,
1494.87129209608));
#145468=CARTESIAN_POINT('Ctrl Pts',(10.6944718935536,-4.10147232415365,
1495.44498577422));
#145469=CARTESIAN_POINT('Ctrl Pts',(10.999097010809,-3.19576090909844,1496.35069718927));
#145470=CARTESIAN_POINT('Ctrl Pts',(11.1582376083003,-2.62178859469216,
1496.7464297602));
#145471=CARTESIAN_POINT('Ctrl Pts',(11.3819664861004,-1.35310050851134,
1497.27600995763));
#145472=CARTESIAN_POINT('Ctrl Pts',(11.444,-0.657734185748339,1497.409375));
#145473=CARTESIAN_POINT('Ctrl Pts',(11.444,0.657734185747905,1497.409375));
#145474=CARTESIAN_POINT('Ctrl Pts',(11.3819664861004,1.35310050851086,1497.27600995763));
#145475=CARTESIAN_POINT('Ctrl Pts',(11.1582376083003,2.62178859469168,1496.7464297602));
#145476=CARTESIAN_POINT('Ctrl Pts',(10.9990970108091,3.195760909098,1496.35069718927));
#145477=CARTESIAN_POINT('Ctrl Pts',(10.6944718935536,4.10147232415322,1495.44498577422));
#145478=CARTESIAN_POINT('Ctrl Pts',(10.5275891593601,4.49662578128903,1494.87129209608));
#145479=CARTESIAN_POINT('Ctrl Pts',(10.2855048387882,5.02575113964816,1493.60374744311));
#145480=CARTESIAN_POINT('Ctrl Pts',(10.2149882823905,5.15937499999979,1492.90886096721));
#145481=CARTESIAN_POINT('Ctrl Pts',(10.2149882823905,5.1593749999998,1492.25));
#145482=CARTESIAN_POINT('Origin',(0.,50.8013494805973,1441.45));
#145483=CARTESIAN_POINT('',(1.0718581768139E-15,11.4439999999998,1446.609375));
#145484=CARTESIAN_POINT('',(-6.31841207935097E-16,50.8013494805973,1446.609375));
#145485=CARTESIAN_POINT('',(-2.60620079334573E-21,11.4439999999998,1436.290625));
#145486=CARTESIAN_POINT('Ctrl Pts',(-3.19189119579733E-15,11.4439999999998,
1446.609375));
#145487=CARTESIAN_POINT('Ctrl Pts',(-0.657734185748133,11.4439999999998,
1446.609375));
#145488=CARTESIAN_POINT('Ctrl Pts',(-1.35310050851117,11.3819664861002,
1446.47600995763));
#145489=CARTESIAN_POINT('Ctrl Pts',(-2.62178859469199,11.1582376083001,
1445.9464297602));
#145490=CARTESIAN_POINT('Ctrl Pts',(-3.19576090909826,10.9990970108089,
1445.55069718927));
#145491=CARTESIAN_POINT('Ctrl Pts',(-4.10147232415348,10.6944718935534,
1444.64498577422));
#145492=CARTESIAN_POINT('Ctrl Pts',(-4.4966257812893,10.5275891593599,1444.07129209608));
#145493=CARTESIAN_POINT('Ctrl Pts',(-5.02575113964843,10.285504838788,1442.80374744311));
#145494=CARTESIAN_POINT('Ctrl Pts',(-5.15937500000008,10.2149882823903,
1442.10886096721));
#145495=CARTESIAN_POINT('Ctrl Pts',(-5.15937500000008,10.2149882823903,
1441.45));
#145496=CARTESIAN_POINT('Ctrl Pts',(-5.15937500000008,10.2149882823903,
1440.79113903279));
#145497=CARTESIAN_POINT('Ctrl Pts',(-5.02575113964843,10.285504838788,1440.09625255689));
#145498=CARTESIAN_POINT('Ctrl Pts',(-4.4966257812893,10.5275891593599,1438.82870790392));
#145499=CARTESIAN_POINT('Ctrl Pts',(-4.10147232415348,10.6944718935534,
1438.25501422579));
#145500=CARTESIAN_POINT('Ctrl Pts',(-3.19576090909827,10.9990970108089,
1437.34930281073));
#145501=CARTESIAN_POINT('Ctrl Pts',(-2.621788594692,11.1582376083001,1436.9535702398));
#145502=CARTESIAN_POINT('Ctrl Pts',(-1.35310050851117,11.3819664861002,
1436.42399004237));
#145503=CARTESIAN_POINT('Ctrl Pts',(-0.657734185748142,11.4439999999998,
1436.290625));
#145504=CARTESIAN_POINT('Ctrl Pts',(-1.08246744900953E-14,11.4439999999998,
1436.290625));
#145505=CARTESIAN_POINT('Ctrl Pts',(3.33066907387547E-15,11.4439999999998,
1436.290625));
#145506=CARTESIAN_POINT('Ctrl Pts',(0.657734185748133,11.4439999999998,
1436.290625));
#145507=CARTESIAN_POINT('Ctrl Pts',(1.35310050851117,11.3819664861002,1436.42399004237));
#145508=CARTESIAN_POINT('Ctrl Pts',(2.621788594692,11.1582376083001,1436.9535702398));
#145509=CARTESIAN_POINT('Ctrl Pts',(3.19576090909826,10.9990970108089,1437.34930281073));
#145510=CARTESIAN_POINT('Ctrl Pts',(4.10147232415348,10.6944718935534,1438.25501422579));
#145511=CARTESIAN_POINT('Ctrl Pts',(4.496625781289,10.52758915936,1438.82870790392));
#145512=CARTESIAN_POINT('Ctrl Pts',(5.02575113964828,10.2855048387881,1440.09625255689));
#145513=CARTESIAN_POINT('Ctrl Pts',(5.15937500000008,10.2149882823903,1440.79113903279));
#145514=CARTESIAN_POINT('Ctrl Pts',(5.15937500000008,10.2149882823903,1442.10886096721));
#145515=CARTESIAN_POINT('Ctrl Pts',(5.02575113964848,10.285504838788,1442.80374744311));
#145516=CARTESIAN_POINT('Ctrl Pts',(4.4966257812895,10.5275891593598,1444.07129209608));
#145517=CARTESIAN_POINT('Ctrl Pts',(4.10147232415348,10.6944718935534,1444.64498577422));
#145518=CARTESIAN_POINT('Ctrl Pts',(3.19576090909826,10.9990970108089,1445.55069718927));
#145519=CARTESIAN_POINT('Ctrl Pts',(2.62178859469199,11.1582376083001,1445.9464297602));
#145520=CARTESIAN_POINT('Ctrl Pts',(1.35310050851117,11.3819664861002,1446.47600995763));
#145521=CARTESIAN_POINT('Ctrl Pts',(0.657734185748116,11.4439999999998,
1446.609375));
#145522=CARTESIAN_POINT('Ctrl Pts',(-1.40165656858926E-14,11.4439999999998,
1446.609375));
#145523=CARTESIAN_POINT('Origin',(0.,50.8013494805973,1441.45));
#145524=CARTESIAN_POINT('',(-2.27105430665522E-14,-11.4440000000002,1436.290625));
#145525=CARTESIAN_POINT('',(4.40252725068937E-15,-11.4440000000002,1446.609375));
#145526=CARTESIAN_POINT('Ctrl Pts',(-8.32667268468867E-16,-11.4440000000002,
1436.290625));
#145527=CARTESIAN_POINT('Ctrl Pts',(-0.657734185748132,-11.4440000000002,
1436.290625));
#145528=CARTESIAN_POINT('Ctrl Pts',(-1.35310050851117,-11.3819664861006,
1436.42399004237));
#145529=CARTESIAN_POINT('Ctrl Pts',(-2.621788594692,-11.1582376083005,1436.9535702398));
#145530=CARTESIAN_POINT('Ctrl Pts',(-3.19576090909827,-10.9990970108092,
1437.34930281073));
#145531=CARTESIAN_POINT('Ctrl Pts',(-4.10147232415348,-10.6944718935538,
1438.25501422579));
#145532=CARTESIAN_POINT('Ctrl Pts',(-4.4966257812893,-10.5275891593602,
1438.82870790392));
#145533=CARTESIAN_POINT('Ctrl Pts',(-5.02575113964843,-10.2855048387884,
1440.09625255689));
#145534=CARTESIAN_POINT('Ctrl Pts',(-5.15937500000008,-10.2149882823906,
1440.79113903279));
#145535=CARTESIAN_POINT('Ctrl Pts',(-5.15937500000008,-10.2149882823906,
1441.45));
#145536=CARTESIAN_POINT('Ctrl Pts',(-5.15937500000008,-10.2149882823906,
1442.10886096721));
#145537=CARTESIAN_POINT('Ctrl Pts',(-5.02575113964843,-10.2855048387884,
1442.80374744311));
#145538=CARTESIAN_POINT('Ctrl Pts',(-4.4966257812893,-10.5275891593602,
1444.07129209608));
#145539=CARTESIAN_POINT('Ctrl Pts',(-4.10147232415348,-10.6944718935538,
1444.64498577422));
#145540=CARTESIAN_POINT('Ctrl Pts',(-3.19576090909826,-10.9990970108092,
1445.55069718927));
#145541=CARTESIAN_POINT('Ctrl Pts',(-2.62178859469199,-11.1582376083005,
1445.9464297602));
#145542=CARTESIAN_POINT('Ctrl Pts',(-1.35310050851117,-11.3819664861006,
1446.47600995763));
#145543=CARTESIAN_POINT('Ctrl Pts',(-0.657734185748134,-11.4440000000002,
1446.609375));
#145544=CARTESIAN_POINT('Ctrl Pts',(-3.7470027081099E-15,-11.4440000000002,
1446.609375));
#145545=CARTESIAN_POINT('',(-6.31841207935097E-16,50.8013494805973,1446.609375));
#145546=CARTESIAN_POINT('Ctrl Pts',(4.71844785465692E-15,-11.4440000000002,
1446.609375));
#145547=CARTESIAN_POINT('Ctrl Pts',(0.657734185748135,-11.4440000000002,
1446.609375));
#145548=CARTESIAN_POINT('Ctrl Pts',(1.35310050851117,-11.3819664861006,
1446.47600995763));
#145549=CARTESIAN_POINT('Ctrl Pts',(2.62178859469199,-11.1582376083005,
1445.9464297602));
#145550=CARTESIAN_POINT('Ctrl Pts',(3.19576090909826,-10.9990970108092,
1445.55069718927));
#145551=CARTESIAN_POINT('Ctrl Pts',(4.10147232415348,-10.6944718935538,
1444.64498577422));
#145552=CARTESIAN_POINT('Ctrl Pts',(4.4966257812893,-10.5275891593602,1444.07129209608));
#145553=CARTESIAN_POINT('Ctrl Pts',(5.02575113964843,-10.2855048387884,
1442.80374744311));
#145554=CARTESIAN_POINT('Ctrl Pts',(5.15937500000008,-10.2149882823906,
1442.10886096721));
#145555=CARTESIAN_POINT('Ctrl Pts',(5.15937500000008,-10.2149882823906,
1440.79113903279));
#145556=CARTESIAN_POINT('Ctrl Pts',(5.02575113964838,-10.2855048387884,
1440.09625255689));
#145557=CARTESIAN_POINT('Ctrl Pts',(4.4966257812891,-10.5275891593603,1438.82870790392));
#145558=CARTESIAN_POINT('Ctrl Pts',(4.10147232415348,-10.6944718935538,
1438.25501422578));
#145559=CARTESIAN_POINT('Ctrl Pts',(3.19576090909826,-10.9990970108092,
1437.34930281073));
#145560=CARTESIAN_POINT('Ctrl Pts',(2.62178859469186,-11.1582376083005,
1436.9535702398));
#145561=CARTESIAN_POINT('Ctrl Pts',(1.353100508511,-11.3819664861006,1436.42399004237));
#145562=CARTESIAN_POINT('Ctrl Pts',(0.657734185748139,-11.4440000000002,
1436.290625));
#145563=CARTESIAN_POINT('Ctrl Pts',(9.85322934354826E-15,-11.4440000000002,
1436.290625));
#145564=CARTESIAN_POINT('Origin',(0.,0.,-11.4051836540916));
#145565=CARTESIAN_POINT('',(0.,-39.,1500.98568435754));
#145566=CARTESIAN_POINT('Ctrl Pts',(-39.,1.41056610836188E-11,1475.58568435754));
#145567=CARTESIAN_POINT('Ctrl Pts',(-39.,-4.970368238445,1477.64942898041));
#145568=CARTESIAN_POINT('Ctrl Pts',(-38.0491535857389,-9.90306272484582,
1479.68930691437));
#145569=CARTESIAN_POINT('Ctrl Pts',(-34.1464428607401,-19.6276492723476,
1484.03976045586));
#145570=CARTESIAN_POINT('Ctrl Pts',(-31.0416401501891,-24.2411102676192,
1486.29373534575));
#145571=CARTESIAN_POINT('Ctrl Pts',(-23.4863841819941,-31.5346631935602,
1490.64510860141));
#145572=CARTESIAN_POINT('Ctrl Pts',(-19.247643648964,-34.2867807694761,
1492.70674499341));
#145573=CARTESIAN_POINT('Ctrl Pts',(-9.96719072828815,-38.035369756234,
1496.84987692723));
#145574=CARTESIAN_POINT('Ctrl Pts',(-5.00616845072917,-39.,1498.9159421232));
#145575=CARTESIAN_POINT('Ctrl Pts',(-4.88498130835069E-14,-39.,1500.98568435754));
#145576=CARTESIAN_POINT('',(0.,-39.,1504.15181564246));
#145577=CARTESIAN_POINT('',(0.,-39.,-11.4051836540916));
#145578=CARTESIAN_POINT('Ctrl Pts',(-1.77635683940025E-14,-39.,1504.15181564246));
#145579=CARTESIAN_POINT('Ctrl Pts',(-3.18484312075356,-39.,1502.83507922385));
#145580=CARTESIAN_POINT('Ctrl Pts',(-6.35799498342694,-38.6098072039276,
1501.51747455921));
#145581=CARTESIAN_POINT('Ctrl Pts',(-12.5382317252814,-37.0666925628971,
1498.8739996287));
#145582=CARTESIAN_POINT('Ctrl Pts',(-15.5230464279844,-35.9191078993228,
1497.55933873559));
#145583=CARTESIAN_POINT('Ctrl Pts',(-23.1893713136726,-31.8356576757199,
1493.95417215531));
#145584=CARTESIAN_POINT('Ctrl Pts',(-27.4446869642291,-28.2495705127348,
1491.69599437198));
#145585=CARTESIAN_POINT('Ctrl Pts',(-34.1852574911453,-19.5599468650915,
1487.14413355563));
#145586=CARTESIAN_POINT('Ctrl Pts',(-36.5996966347151,-14.5498824765313,
1484.8860801759));
#145587=CARTESIAN_POINT('Ctrl Pts',(-38.6318850891163,-6.18454031151119,
1481.31680557566));
#145588=CARTESIAN_POINT('Ctrl Pts',(-39.,-3.09314338229533,1480.03611847813));
#145589=CARTESIAN_POINT('Ctrl Pts',(-39.,3.61204122167891E-11,1478.75181564244));
#145590=CARTESIAN_POINT('Origin',(0.,0.,0.));
#145591=CARTESIAN_POINT('',(7.57979930842467E-5,14.9999999998085,738.1874185217));
#145592=CARTESIAN_POINT('Ctrl Pts',(-4.89098483935635E-10,-15.0000000000001,
788.987499999474));
#145593=CARTESIAN_POINT('Ctrl Pts',(-1.02771888238626,-14.9999999999666,
787.882764050382));
#145594=CARTESIAN_POINT('Ctrl Pts',(-2.05351531366403,-14.8946888393821,
786.773272543722));
#145595=CARTESIAN_POINT('Ctrl Pts',(-5.88144240218294,-14.0955300452956,
782.56250888796));
#145596=CARTESIAN_POINT('Ctrl Pts',(-8.47391997558319,-12.7069392000974,
779.515000164681));
#145597=CARTESIAN_POINT('Ctrl Pts',(-12.5749111849436,-8.66937272960075,
773.311268120249));
#145598=CARTESIAN_POINT('Ctrl Pts',(-14.0037987885581,-6.09791553059049,
770.2687459843));
#145599=CARTESIAN_POINT('Ctrl Pts',(-15.2665815114232,-0.478165236301349,
764.054778185987));
#145600=CARTESIAN_POINT('Ctrl Pts',(-15.0751907911456,2.45782223945693,
761.015845209898));
#145601=CARTESIAN_POINT('Ctrl Pts',(-13.0914001141734,7.86899513846603,
754.795079275443));
#145602=CARTESIAN_POINT('Ctrl Pts',(-11.3397878890973,10.2331405877126,
751.758113120992));
#145603=CARTESIAN_POINT('Ctrl Pts',(-7.74651260584957,12.9467120513458,
746.897151285694));
#145604=CARTESIAN_POINT('Ctrl Pts',(-6.30365555683432,13.7072852422168,
745.165589145661));
#145605=CARTESIAN_POINT('Ctrl Pts',(-3.22895029994973,14.7379152250953,
741.668537470621));
#145606=CARTESIAN_POINT('Ctrl Pts',(-1.61820297783865,15.000008177294,739.92697163094));
#145607=CARTESIAN_POINT('Ctrl Pts',(7.57979930842463E-5,14.9999999998084,
738.1874185217));
#145608=CARTESIAN_POINT('',(4.22080283094658,-14.3939161961195,692.000039859602));
#145609=CARTESIAN_POINT('Ctrl Pts',(7.57979930842468E-5,14.9999999998085,
738.1874185217));
#145610=CARTESIAN_POINT('Ctrl Pts',(0.281550833006751,14.999999286898,737.884849656782));
#145611=CARTESIAN_POINT('Ctrl Pts',(0.563038542676674,14.9920711836477,
737.581477601275));
#145612=CARTESIAN_POINT('Ctrl Pts',(0.843973186420159,14.9762396678864,
737.27791284127));
#145613=CARTESIAN_POINT('Ctrl Pts',(1.12481690390502,14.9604132760944,736.974446331903));
#145614=CARTESIAN_POINT('Ctrl Pts',(1.40510753881479,14.9366886541256,736.67078765209));
#145615=CARTESIAN_POINT('Ctrl Pts',(1.68428629575425,14.905141382265,736.367544974865));
#145616=CARTESIAN_POINT('Ctrl Pts',(1.96265216582003,14.8736859668319,736.065185251611));
#145617=CARTESIAN_POINT('Ctrl Pts',(2.23991227258382,14.8344535235122,735.763239502357));
#145618=CARTESIAN_POINT('Ctrl Pts',(2.51552447619478,14.787568766651,735.462302903552));
#145619=CARTESIAN_POINT('Ctrl Pts',(2.5959084857406,14.7738945363604,735.374532876992));
#145620=CARTESIAN_POINT('Ctrl Pts',(2.67615241441217,14.7595696908977,735.286848621306));
#145621=CARTESIAN_POINT('Ctrl Pts',(2.75624306674878,14.7445980974433,735.199264705882));
#145622=CARTESIAN_POINT('Ctrl Pts',(3.03135041722587,14.693171429193,734.898418374712));
#145623=CARTESIAN_POINT('Ctrl Pts',(3.30536110980185,14.6339768655788,734.596415852432));
#145624=CARTESIAN_POINT('Ctrl Pts',(3.57772157299117,14.5670840383446,734.293852494505));
#145625=CARTESIAN_POINT('Ctrl Pts',(3.85951208359147,14.497875153468,733.980813362023));
#145626=CARTESIAN_POINT('Ctrl Pts',(4.13953565571147,14.420425401538,733.667174273596));
#145627=CARTESIAN_POINT('Ctrl Pts',(4.41718621299959,14.3348692038643,733.353604256735));
#145628=CARTESIAN_POINT('Ctrl Pts',(4.6948367702877,14.2493130061907,733.040034239875));
#145629=CARTESIAN_POINT('Ctrl Pts',(4.97011387588181,14.1556504467663,732.726533773015));
#145630=CARTESIAN_POINT('Ctrl Pts',(5.24242510239044,14.054073405876,732.413774701343));
#145631=CARTESIAN_POINT('Ctrl Pts',(5.3013229633486,14.0321034323732,732.346128425599));
#145632=CARTESIAN_POINT('Ctrl Pts',(5.36005824713267,14.0097723288205,732.278544270074));
#145633=CARTESIAN_POINT('Ctrl Pts',(5.41862499612807,13.9870834496368,732.211029411765));
#145634=CARTESIAN_POINT('Ctrl Pts',(5.6695864337698,13.8898604718194,731.921724879855));
#145635=CARTESIAN_POINT('Ctrl Pts',(5.91807648535088,13.7858223151936,731.631529191763));
#145636=CARTESIAN_POINT('Ctrl Pts',(6.16359696334797,13.6751626241441,731.341016961021));
#145637=CARTESIAN_POINT('Ctrl Pts',(6.40920526581501,13.5644633493141,731.050400811931));
#145638=CARTESIAN_POINT('Ctrl Pts',(6.65184148726155,13.4471379709317,730.75946834466));
#145639=CARTESIAN_POINT('Ctrl Pts',(6.89102818973086,13.3234278919885,730.468797102226));
#145640=CARTESIAN_POINT('Ctrl Pts',(7.12957425966607,13.2000491554675,730.178904387413));
#145641=CARTESIAN_POINT('Ctrl Pts',(7.36468892711074,13.0703201158073,729.889271942079));
#145642=CARTESIAN_POINT('Ctrl Pts',(7.59592512409975,12.9345244117713,729.600468284286));
#145643=CARTESIAN_POINT('Ctrl Pts',(7.69686130700828,12.8752486573728,729.474403510659));
#145644=CARTESIAN_POINT('Ctrl Pts',(7.79705886486056,12.8148175183969,729.348496556582));
#145645=CARTESIAN_POINT('Ctrl Pts',(7.89648244705168,12.7532570422289,729.222794117647));
#145646=CARTESIAN_POINT('Ctrl Pts',(8.12430532712643,12.6121950861993,728.934754891545));
#145647=CARTESIAN_POINT('Ctrl Pts',(8.3486274609939,12.4648505962549,728.645644306878));
#145648=CARTESIAN_POINT('Ctrl Pts',(8.56898524697153,12.311478059254,728.356027316226));
#145649=CARTESIAN_POINT('Ctrl Pts',(8.78996907191286,12.1576697891399,728.065587520427));
#145650=CARTESIAN_POINT('Ctrl Pts',(9.00696561094669,11.997799342883,727.774638876241));
#145651=CARTESIAN_POINT('Ctrl Pts',(9.21953296179767,11.8321685296063,727.483758428849));
#145652=CARTESIAN_POINT('Ctrl Pts',(9.4251841105422,11.6719267667887,727.202342219286));
#145653=CARTESIAN_POINT('Ctrl Pts',(9.62668945470535,11.5062938109494,726.920990246791));
#145654=CARTESIAN_POINT('Ctrl Pts',(9.82367643067417,11.3355803369513,726.640225589426));
#145655=CARTESIAN_POINT('Ctrl Pts',(9.91869715856878,11.2532331742471,726.504792970195));
#145656=CARTESIAN_POINT('Ctrl Pts',(10.0126295933473,11.1697367600015,726.36955024063));
#145657=CARTESIAN_POINT('Ctrl Pts',(10.105434659685,11.0851337637799,726.234558823529));
#145658=CARTESIAN_POINT('Ctrl Pts',(10.2977526973862,10.9098127079468,725.954818875402));
#145659=CARTESIAN_POINT('Ctrl Pts',(10.4856902898329,10.7293149967496,725.674134857072));
#145660=CARTESIAN_POINT('Ctrl Pts',(10.6688588721195,10.5439769826085,725.393057705533));
#145661=CARTESIAN_POINT('Ctrl Pts',(10.85220513252,10.3584591859501,725.111707902115));
#145662=CARTESIAN_POINT('Ctrl Pts',(11.0307727964269,10.1680919790287,724.829964671725));
#145663=CARTESIAN_POINT('Ctrl Pts',(11.2042076602919,9.97325077005239,724.548385119335));
#145664=CARTESIAN_POINT('Ctrl Pts',(11.3772608440206,9.77883835040691,724.267425242365));
#145665=CARTESIAN_POINT('Ctrl Pts',(11.5452035346936,9.57997194837157,723.98662879142));
#145666=CARTESIAN_POINT('Ctrl Pts',(11.707723575922,9.37705757861438,723.706546708871));
#145667=CARTESIAN_POINT('Ctrl Pts',(11.7968818188589,9.26573906960191,723.552894112124));
#145668=CARTESIAN_POINT('Ctrl Pts',(11.884408780843,9.1532028338603,723.399456426814));
#145669=CARTESIAN_POINT('Ctrl Pts',(11.9702584125853,9.03951954824237,723.246323529412));
#145670=CARTESIAN_POINT('Ctrl Pts',(12.1267446422907,8.83229828956197,722.967193738496));
#145671=CARTESIAN_POINT('Ctrl Pts',(12.2780314854468,8.62076607850108,722.687061998882));
#145672=CARTESIAN_POINT('Ctrl Pts',(12.4237935186084,8.40531704755474,722.406475004631));
#145673=CARTESIAN_POINT('Ctrl Pts',(12.5699336917389,8.18930909266857,722.125160103703));
#145674=CARTESIAN_POINT('Ctrl Pts',(12.7105200582298,7.96936429288088,721.843388047227));
#145675=CARTESIAN_POINT('Ctrl Pts',(12.8452656387393,7.74591186917703,721.561715887111));
#145676=CARTESIAN_POINT('Ctrl Pts',(12.95616527364,7.56200385443744,721.329891291452));
#145677=CARTESIAN_POINT('Ctrl Pts',(13.0631091840619,7.37572053594736,721.098134595532));
#145678=CARTESIAN_POINT('Ctrl Pts',(13.165960058574,7.18731491838453,720.866756054193));
#145679=CARTESIAN_POINT('Ctrl Pts',(13.2563153441342,7.02179913199209,720.663488223225));
#145680=CARTESIAN_POINT('Ctrl Pts',(13.3435057150174,6.85465692241973,720.460526227376));
#145681=CARTESIAN_POINT('Ctrl Pts',(13.427449370526,6.6860753367475,720.258088235294));
#145682=CARTESIAN_POINT('Ctrl Pts',(13.5406317255301,6.45877452692322,719.985138379259));
#145683=CARTESIAN_POINT('Ctrl Pts',(13.6481759951956,6.22832192582482,719.711214507562));
#145684=CARTESIAN_POINT('Ctrl Pts',(13.7498401916303,5.99515593932086,719.436852309226));
#145685=CARTESIAN_POINT('Ctrl Pts',(13.8516418206169,5.76167475240564,719.162119220267));
#145686=CARTESIAN_POINT('Ctrl Pts',(13.9475472454033,5.52547322797553,718.886947097059));
#145687=CARTESIAN_POINT('Ctrl Pts',(14.0373597882222,5.28701524906024,718.611879605197));
#145688=CARTESIAN_POINT('Ctrl Pts',(14.1270049125188,5.04900177690535,718.337324863465));
#145689=CARTESIAN_POINT('Ctrl Pts',(14.2105797159508,4.80874068116805,718.062874844367));
#145690=CARTESIAN_POINT('Ctrl Pts',(14.2879373390108,4.56671070908823,717.789068748523));
#145691=CARTESIAN_POINT('Ctrl Pts',(14.3369205063337,4.41345632832305,717.615693594579));
#145692=CARTESIAN_POINT('Ctrl Pts',(14.3834118976418,4.2594930507057,717.442576567067));
#145693=CARTESIAN_POINT('Ctrl Pts',(14.4273846515339,4.10494485220273,717.269852941177));
#145694=CARTESIAN_POINT('Ctrl Pts',(14.4968417248649,3.86082856185289,716.997027691729));
#145695=CARTESIAN_POINT('Ctrl Pts',(14.5601755404354,3.61467881023674,716.723259252437));
#145696=CARTESIAN_POINT('Ctrl Pts',(14.6172331099927,3.36697139101017,716.449082865871));
#145697=CARTESIAN_POINT('Ctrl Pts',(14.674422462025,3.11869185668948,716.174273230412));
#145698=CARTESIAN_POINT('Ctrl Pts',(14.7253063946445,2.86884787430016,715.899054239511));
#145699=CARTESIAN_POINT('Ctrl Pts',(14.7697809208011,2.61793271182503,715.623969958683));
#145700=CARTESIAN_POINT('Ctrl Pts',(14.7983938528386,2.45650505623126,715.44699296731));
#145701=CARTESIAN_POINT('Ctrl Pts',(14.8243549155049,2.29463430283197,715.270071817007));
#145702=CARTESIAN_POINT('Ctrl Pts',(14.8476476804061,2.13245362629643,715.093351086719));
#145703=CARTESIAN_POINT('Ctrl Pts',(14.8833806436034,1.88365550505326,714.822247360802));
#145704=CARTESIAN_POINT('Ctrl Pts',(14.9128478753549,1.63401309449245,714.551490612981));
#145705=CARTESIAN_POINT('Ctrl Pts',(14.936012647393,1.38402539222435,714.281617647059));
#145706=CARTESIAN_POINT('Ctrl Pts',(14.9590391181592,1.13553019836948,714.013355911083));
#145707=CARTESIAN_POINT('Ctrl Pts',(14.9758914132006,0.886119743165234,
713.744106109306));
#145708=CARTESIAN_POINT('Ctrl Pts',(14.986498794157,0.636281385739037,713.474394367854));
#145709=CARTESIAN_POINT('Ctrl Pts',(14.9971225801966,0.386056635191933,
713.204265497653));
#145710=CARTESIAN_POINT('Ctrl Pts',(15.001482045022,0.135403105453872,712.933673741051));
#145711=CARTESIAN_POINT('Ctrl Pts',(14.9995577562733,-0.115183625524045,
712.663154096745));
#145712=CARTESIAN_POINT('Ctrl Pts',(14.9976367462435,-0.365343391752358,
712.393095380086));
#145713=CARTESIAN_POINT('Ctrl Pts',(14.9894534009396,-0.615436134420939,
712.123109018403));
#145714=CARTESIAN_POINT('Ctrl Pts',(14.9750401577341,-0.864969637016497,
711.853726381551));
#145715=CARTESIAN_POINT('Ctrl Pts',(14.9650277479948,-1.03831241879351,
711.666595053899));
#145716=CARTESIAN_POINT('Ctrl Pts',(14.9520101078572,-1.2113853461834,711.479755046204));
#145717=CARTESIAN_POINT('Ctrl Pts',(14.9360126519092,-1.38402539264299,
711.293382352941));
#145718=CARTESIAN_POINT('Ctrl Pts',(14.9129720146043,-1.63267347191893,
711.024955570398));
#145719=CARTESIAN_POINT('Ctrl Pts',(14.8836946574883,-1.88099800592914,
710.755634970035));
#145720=CARTESIAN_POINT('Ctrl Pts',(14.8482138789356,-2.12850765735087,
710.485948546402));
#145721=CARTESIAN_POINT('Ctrl Pts',(14.8126588775094,-2.3765350786264,710.21569796093));
#145722=CARTESIAN_POINT('Ctrl Pts',(14.7708744994095,-2.62374375064837,
709.945080506721));
#145723=CARTESIAN_POINT('Ctrl Pts',(14.722945983439,-2.86964488842252,709.674631773074));
#145724=CARTESIAN_POINT('Ctrl Pts',(14.7019882738472,-2.97717011697189,
709.55637261348));
#145725=CARTESIAN_POINT('Ctrl Pts',(14.679856436388,-3.08444545163411,709.4381457253));
#145726=CARTESIAN_POINT('Ctrl Pts',(14.656560656033,-3.19143070180115,709.319995777693));
#145727=CARTESIAN_POINT('Ctrl Pts',(14.6039181339553,-3.43319008088539,
709.053007029918));
#145728=CARTESIAN_POINT('Ctrl Pts',(14.5452834571176,-3.67367460155924,
708.786182476552));
#145729=CARTESIAN_POINT('Ctrl Pts',(14.480781628501,-3.91241147646642,708.520048618717));
#145730=CARTESIAN_POINT('Ctrl Pts',(14.4634070462039,-3.97671900959168,
708.448361277224));
#145731=CARTESIAN_POINT('Ctrl Pts',(14.4456070353278,-4.0408998169529,708.376724021998));
#145732=CARTESIAN_POINT('Ctrl Pts',(14.427384651626,-4.10494485222909,708.305147058823));
#145733=CARTESIAN_POINT('Ctrl Pts',(14.3598586870102,-4.34227399953762,
708.039907145005));
#145734=CARTESIAN_POINT('Ctrl Pts',(14.2863747232897,-4.57827959615286,
707.773676097403));
#145735=CARTESIAN_POINT('Ctrl Pts',(14.2070397540541,-4.81248600453167,
707.506974439535));
#145736=CARTESIAN_POINT('Ctrl Pts',(14.1275767982191,-5.04707024480546,
707.239842527032));
#145737=CARTESIAN_POINT('Ctrl Pts',(14.0422440323164,-5.2798490384921,706.972238970869));
#145738=CARTESIAN_POINT('Ctrl Pts',(13.9511993147848,-5.5103573213283,706.704693487103));
#145739=CARTESIAN_POINT('Ctrl Pts',(13.860307689284,-5.74047800363047,706.437597882061));
#145740=CARTESIAN_POINT('Ctrl Pts',(13.763723489821,-5.96833538710859,706.170560646299));
#145741=CARTESIAN_POINT('Ctrl Pts',(13.6616518215246,-6.19348606661768,
705.904108117904));
#145742=CARTESIAN_POINT('Ctrl Pts',(13.5865236513097,-6.35920451578658,
705.70799012315));
#145743=CARTESIAN_POINT('Ctrl Pts',(13.5084236875781,-6.52345699766309,
705.512188908077));
#145744=CARTESIAN_POINT('Ctrl Pts',(13.4274493751688,-6.68607533905936,
705.316911764706));
#145745=CARTESIAN_POINT('Ctrl Pts',(13.3173414711156,-6.90720181977887,
705.051376234656));
#145746=CARTESIAN_POINT('Ctrl Pts',(13.2016653434899,-7.12581135822056,
704.784986412623));
#145747=CARTESIAN_POINT('Ctrl Pts',(13.080631160973,-7.34146365485426,704.518265866849));
#145748=CARTESIAN_POINT('Ctrl Pts',(12.9593584746677,-7.55754090490723,
704.251019735167));
#145749=CARTESIAN_POINT('Ctrl Pts',(12.8327067931809,-7.77064883360974,
703.983442066405));
#145750=CARTESIAN_POINT('Ctrl Pts',(12.7009334371162,-7.98036903689955,
703.71606312886));
#145751=CARTESIAN_POINT('Ctrl Pts',(12.6731015715451,-8.02466406496766,
703.65958999295));
#145752=CARTESIAN_POINT('Ctrl Pts',(12.6450413858188,-8.06880806697079,
703.603125719969));
#145753=CARTESIAN_POINT('Ctrl Pts',(12.6167555513653,-8.11279726641198,
703.546675294356));
#145754=CARTESIAN_POINT('Ctrl Pts',(12.4837064090762,-8.31971091660871,
703.281147306415));
#145755=CARTESIAN_POINT('Ctrl Pts',(12.3455131459612,-8.52342765962367,
703.015630151262));
#145756=CARTESIAN_POINT('Ctrl Pts',(12.2024496090295,-8.72354421217255,
702.750649610741));
#145757=CARTESIAN_POINT('Ctrl Pts',(12.1264122948955,-8.82990482296075,
702.609814223674));
#145758=CARTESIAN_POINT('Ctrl Pts',(12.048999936094,-8.93524891659357,702.46913039669));
#145759=CARTESIAN_POINT('Ctrl Pts',(11.9702584108949,-9.03951954696603,
702.328676470588));
#145760=CARTESIAN_POINT('Ctrl Pts',(11.8224697257209,-9.23522339352024,
702.065060786061));
#145761=CARTESIAN_POINT('Ctrl Pts',(11.6696609069418,-9.42758811617559,
701.800457965802));
#145762=CARTESIAN_POINT('Ctrl Pts',(11.5121019326805,-9.61621074689837,
701.535385846013));
#145763=CARTESIAN_POINT('Ctrl Pts',(11.3542910307001,-9.8051349743366,701.269889891181));
#145764=CARTESIAN_POINT('Ctrl Pts',(11.1917150167255,-9.99030474597149,
701.003923622989));
#145765=CARTESIAN_POINT('Ctrl Pts',(11.0246874612152,-10.1713453586207,
700.738014032166));
#145766=CARTESIAN_POINT('Ctrl Pts',(10.8579517744045,-10.3520696157557,
700.472569099323));
#145767=CARTESIAN_POINT('Ctrl Pts',(10.6867804145302,-10.528678809136,700.207181139665));
#145768=CARTESIAN_POINT('Ctrl Pts',(10.5115231038306,-10.7008355773604,
699.942373645533));
#145769=CARTESIAN_POINT('Ctrl Pts',(10.3784595745027,-10.8315450301425,
699.741319437745));
#145770=CARTESIAN_POINT('Ctrl Pts',(10.2430414898439,-10.9596885536914,
699.540599879091));
#145771=CARTESIAN_POINT('Ctrl Pts',(10.1054346550857,-11.0851337587347,
699.340441176471));
#145772=CARTESIAN_POINT('Ctrl Pts',(9.92365192039655,-11.2508506176865,
699.076025557885));
#145773=CARTESIAN_POINT('Ctrl Pts',(9.73763449665069,-11.4122344480125,
698.810780717394));
#145774=CARTESIAN_POINT('Ctrl Pts',(9.54773966847933,-11.5689527290905,
698.545230782436));
#145775=CARTESIAN_POINT('Ctrl Pts',(9.36384501633439,-11.7207191255803,
698.28807152546));
#145776=CARTESIAN_POINT('Ctrl Pts',(9.17631459608406,-11.8681100780542,
698.030626608508));
#145777=CARTESIAN_POINT('Ctrl Pts',(8.9855029746898,-12.0108591004051,697.773374857605));
#145778=CARTESIAN_POINT('Ctrl Pts',(8.78880252026194,-12.1580136466555,
697.508183796729));
#145779=CARTESIAN_POINT('Ctrl Pts',(8.58837255017628,-12.3004165090796,
697.242871083569));
#145780=CARTESIAN_POINT('Ctrl Pts',(8.38460658247155,-12.4377800472919,
696.977962862677));
#145781=CARTESIAN_POINT('Ctrl Pts',(8.22390426457572,-12.5461133437386,
696.769040020425));
#145782=CARTESIAN_POINT('Ctrl Pts',(8.06112772889969,-12.6513129929349,
696.560368909545));
#145783=CARTESIAN_POINT('Ctrl Pts',(7.8964824440045,-12.7532570373073,696.352205882353));
#145784=CARTESIAN_POINT('Ctrl Pts',(7.68827459184559,-12.882173881374,696.088966173921));
#145785=CARTESIAN_POINT('Ctrl Pts',(7.47660549231053,-13.0061753066193,
695.824746896223));
#145786=CARTESIAN_POINT('Ctrl Pts',(7.26187257153882,-13.1249840684397,
695.560065518168));
#145787=CARTESIAN_POINT('Ctrl Pts',(7.04680900420729,-13.2439757724389,
695.294976582731));
#145788=CARTESIAN_POINT('Ctrl Pts',(6.82867254414394,-13.3577585382978,
695.029424611831));
#145789=CARTESIAN_POINT('Ctrl Pts',(6.60789087379473,-13.4660973645443,
694.763935985973));
#145790=CARTESIAN_POINT('Ctrl Pts',(6.38751841202005,-13.5742353898067,
694.498939430956));
#145791=CARTESIAN_POINT('Ctrl Pts',(6.16451095707521,-13.6769494552564,
694.234006480313));
#145792=CARTESIAN_POINT('Ctrl Pts',(5.93931613867606,-13.7740525563051,
693.969659695136));
#145793=CARTESIAN_POINT('Ctrl Pts',(5.76696412404157,-13.8483700526488,
693.767342868704));
#145794=CARTESIAN_POINT('Ctrl Pts',(5.5933313572213,-13.9194018353776,693.56536943067));
#145795=CARTESIAN_POINT('Ctrl Pts',(5.41862499293033,-13.9870834413829,
693.363970588235));
#145796=CARTESIAN_POINT('Ctrl Pts',(5.18968353158942,-14.0757758358909,
693.100050349918));
#145797=CARTESIAN_POINT('Ctrl Pts',(4.95837761299169,-14.1589149892218,
692.835315617544));
#145798=CARTESIAN_POINT('Ctrl Pts',(4.72516014117508,-14.2363219141141,
692.57028953527));
#145799=CARTESIAN_POINT('Ctrl Pts',(4.55797722240539,-14.2918113915349,
692.380304481237));
#145800=CARTESIAN_POINT('Ctrl Pts',(4.38981249519733,-14.3443561624571,
692.190169941154));
#145801=CARTESIAN_POINT('Ctrl Pts',(4.22083826280853,-14.3939058062505,
692.000079719204));
#145802=CARTESIAN_POINT('',(-0.139482600723335,-14.9993514727836,692.));
#145803=CARTESIAN_POINT('Origin',(0.,-8.44020893219807E-14,692.));
#145804=CARTESIAN_POINT('Ctrl Pts',(-0.139482600723493,-14.9993514727837,
692.));
#145805=CARTESIAN_POINT('Ctrl Pts',(-0.0929871732231087,-14.9997838450207,
692.050022854097));
#145806=CARTESIAN_POINT('Ctrl Pts',(-0.046497364483948,-15.0000000000001,
692.100018131429));
#145807=CARTESIAN_POINT('Ctrl Pts',(-3.60480930607215E-12,-15.0000000000001,
692.149999999996));
#145808=CARTESIAN_POINT('Origin',(0.,0.,0.));
#145809=CARTESIAN_POINT('',(-1.40148579694423E-15,-11.4440000000002,1504.95));
#145810=CARTESIAN_POINT('Origin',(0.,-1.83556249024732E-13,1504.95));
#145811=CARTESIAN_POINT('',(-1.40148579694423E-15,-11.444,-1.39580565057911E-15));
#145812=CARTESIAN_POINT('',(-1.40148579694423E-15,-11.4440000000001,692.));
#145813=CARTESIAN_POINT('',(-1.40148579694423E-15,-11.444,-1.39580565057911E-15));
#145814=CARTESIAN_POINT('Origin',(0.,-8.44020893219807E-14,692.));
#145815=CARTESIAN_POINT('Ctrl Pts',(0.,-50.8,1501.378125));
#145816=CARTESIAN_POINT('Ctrl Pts',(-4.70731322909511,-50.8,1499.88400735294));
#145817=CARTESIAN_POINT('Ctrl Pts',(-9.33447550508177,-49.9350334639422,
1498.38988970588));
#145818=CARTESIAN_POINT('Ctrl Pts',(-13.9616377810684,-49.0700669278844,
1496.89577205882));
#145819=CARTESIAN_POINT('Ctrl Pts',(-18.3510766423074,-47.3695892537413,
1495.40165441176));
#145820=CARTESIAN_POINT('Ctrl Pts',(-22.7405155035463,-45.6691115795981,
1493.90753676471));
#145821=CARTESIAN_POINT('Ctrl Pts',(-26.7427538741697,-43.1910304950644,
1492.41341911765));
#145822=CARTESIAN_POINT('Ctrl Pts',(-30.744992244793,-40.7129494105307,
1490.91930147059));
#145823=CARTESIAN_POINT('Ctrl Pts',(-34.2237386972451,-37.5416529948095,
1489.42518382353));
#145824=CARTESIAN_POINT('Ctrl Pts',(-37.7024851496972,-34.3703565790883,
1487.93106617647));
#145825=CARTESIAN_POINT('Ctrl Pts',(-40.5392751458362,-30.6138395280662,
1486.43694852941));
#145826=CARTESIAN_POINT('Ctrl Pts',(-43.3760651419751,-26.8573224770441,
1484.94283088235));
#145827=CARTESIAN_POINT('Ctrl Pts',(-45.4742952008371,-22.6435084734481,
1483.44871323529));
#145828=CARTESIAN_POINT('Ctrl Pts',(-47.5725252596992,-18.4296944698521,
1481.95459558824));
#145829=CARTESIAN_POINT('Ctrl Pts',(-48.8607426731792,-13.9020798956618,
1480.46047794118));
#145830=CARTESIAN_POINT('Ctrl Pts',(-50.1489600866593,-9.37446532147148,
1478.96636029412));
#145831=CARTESIAN_POINT('Ctrl Pts',(-50.5832961557877,-4.68723266073574,
1477.47224264706));
#145832=CARTESIAN_POINT('Ctrl Pts',(-51.0176322249162,-3.12392900021603E-15,
1475.978125));
#145833=CARTESIAN_POINT('Ctrl Pts',(-50.5832961557877,4.68723266073573,
1474.48400735294));
#145834=CARTESIAN_POINT('Ctrl Pts',(-50.1489600866593,9.37446532147149,
1472.98988970588));
#145835=CARTESIAN_POINT('Ctrl Pts',(-48.8607426731792,13.9020798956618,
1471.49577205882));
#145836=CARTESIAN_POINT('Ctrl Pts',(-47.5725252596992,18.4296944698521,
1470.00165441177));
#145837=CARTESIAN_POINT('Ctrl Pts',(-45.4742952008371,22.6435084734481,
1468.50753676471));
#145838=CARTESIAN_POINT('Ctrl Pts',(-43.3760651419751,26.8573224770442,
1467.01341911765));
#145839=CARTESIAN_POINT('Ctrl Pts',(-40.5392751458362,30.6138395280662,
1465.51930147059));
#145840=CARTESIAN_POINT('Ctrl Pts',(-37.7024851496972,34.3703565790883,
1464.02518382353));
#145841=CARTESIAN_POINT('Ctrl Pts',(-34.2237386972451,37.5416529948095,
1462.53106617647));
#145842=CARTESIAN_POINT('Ctrl Pts',(-30.744992244793,40.7129494105307,1461.03694852941));
#145843=CARTESIAN_POINT('Ctrl Pts',(-26.7427538741697,43.1910304950644,
1459.54283088235));
#145844=CARTESIAN_POINT('Ctrl Pts',(-22.7405155035463,45.6691115795981,
1458.04871323529));
#145845=CARTESIAN_POINT('Ctrl Pts',(-18.3510766423074,47.3695892537413,
1456.55459558824));
#145846=CARTESIAN_POINT('Ctrl Pts',(-13.9616377810684,49.0700669278844,
1455.06047794118));
#145847=CARTESIAN_POINT('Ctrl Pts',(-9.33447550508177,49.9350334639422,
1453.56636029412));
#145848=CARTESIAN_POINT('Ctrl Pts',(-4.7073132290951,50.8,1452.07224264706));
#145849=CARTESIAN_POINT('Ctrl Pts',(-6.22120573966855E-15,50.8,1450.578125));
#145850=CARTESIAN_POINT('Ctrl Pts',(4.70731322909511,50.8,1449.08400735294));
#145851=CARTESIAN_POINT('Ctrl Pts',(9.33447550508176,49.9350334639422,1447.58988970588));
#145852=CARTESIAN_POINT('Ctrl Pts',(13.9616377810684,49.0700669278844,1446.09577205882));
#145853=CARTESIAN_POINT('Ctrl Pts',(18.3510766423074,47.3695892537413,1444.60165441176));
#145854=CARTESIAN_POINT('Ctrl Pts',(22.7405155035463,45.6691115795981,1443.10753676471));
#145855=CARTESIAN_POINT('Ctrl Pts',(26.7427538741697,43.1910304950644,1441.61341911765));
#145856=CARTESIAN_POINT('Ctrl Pts',(30.744992244793,40.7129494105307,1440.11930147059));
#145857=CARTESIAN_POINT('Ctrl Pts',(34.2237386972451,37.5416529948095,1438.62518382353));
#145858=CARTESIAN_POINT('Ctrl Pts',(37.7024851496972,34.3703565790883,1437.13106617647));
#145859=CARTESIAN_POINT('Ctrl Pts',(40.5392751458362,30.6138395280662,1435.63694852941));
#145860=CARTESIAN_POINT('Ctrl Pts',(43.3760651419751,26.8573224770442,1434.14283088235));
#145861=CARTESIAN_POINT('Ctrl Pts',(45.4742952008372,22.6435084734481,1432.64871323529));
#145862=CARTESIAN_POINT('Ctrl Pts',(47.5725252596992,18.4296944698521,1431.15459558824));
#145863=CARTESIAN_POINT('Ctrl Pts',(48.8607426731792,13.9020798956618,1429.66047794118));
#145864=CARTESIAN_POINT('Ctrl Pts',(50.1489600866593,9.37446532147146,1428.16636029412));
#145865=CARTESIAN_POINT('Ctrl Pts',(50.5832961557877,4.68723266073574,1426.67224264706));
#145866=CARTESIAN_POINT('Ctrl Pts',(51.0176322249162,9.37178700064808E-15,
1425.178125));
#145867=CARTESIAN_POINT('Ctrl Pts',(50.5832961557877,-4.68723266073572,
1423.68400735294));
#145868=CARTESIAN_POINT('Ctrl Pts',(50.1489600866593,-9.37446532147149,
1422.18988970588));
#145869=CARTESIAN_POINT('Ctrl Pts',(48.8607426731792,-13.9020798956618,
1420.69577205882));
#145870=CARTESIAN_POINT('Ctrl Pts',(47.5725252596992,-18.4296944698521,
1419.20165441177));
#145871=CARTESIAN_POINT('Ctrl Pts',(45.4742952008371,-22.6435084734482,
1417.70753676471));
#145872=CARTESIAN_POINT('Ctrl Pts',(43.3760651419751,-26.8573224770441,
1416.21341911765));
#145873=CARTESIAN_POINT('Ctrl Pts',(40.5392751458362,-30.6138395280662,
1414.71930147059));
#145874=CARTESIAN_POINT('Ctrl Pts',(37.7024851496972,-34.3703565790883,
1413.22518382353));
#145875=CARTESIAN_POINT('Ctrl Pts',(34.2237386972451,-37.5416529948095,
1411.73106617647));
#145876=CARTESIAN_POINT('Ctrl Pts',(30.744992244793,-40.7129494105307,1410.23694852941));
#145877=CARTESIAN_POINT('Ctrl Pts',(26.7427538741697,-43.1910304950644,
1408.74283088235));
#145878=CARTESIAN_POINT('Ctrl Pts',(22.7405155035463,-45.6691115795981,
1407.24871323529));
#145879=CARTESIAN_POINT('Ctrl Pts',(18.3510766423074,-47.3695892537413,
1405.75459558824));
#145880=CARTESIAN_POINT('Ctrl Pts',(13.9616377810684,-49.0700669278844,
1404.26047794118));
#145881=CARTESIAN_POINT('Ctrl Pts',(9.33447550508176,-49.9350334639422,
1402.76636029412));
#145882=CARTESIAN_POINT('Ctrl Pts',(4.70731322909511,-50.8,1401.27224264706));
#145883=CARTESIAN_POINT('Ctrl Pts',(0.,-50.8,1399.778125));
#145884=CARTESIAN_POINT('Ctrl Pts',(-4.70731322909511,-50.8,1398.28400735294));
#145885=CARTESIAN_POINT('Ctrl Pts',(-9.33447550508177,-49.9350334639422,
1396.78988970588));
#145886=CARTESIAN_POINT('Ctrl Pts',(-13.9616377810684,-49.0700669278844,
1395.29577205882));
#145887=CARTESIAN_POINT('Ctrl Pts',(-18.3510766423074,-47.3695892537413,
1393.80165441176));
#145888=CARTESIAN_POINT('Ctrl Pts',(-22.7405155035463,-45.6691115795981,
1392.30753676471));
#145889=CARTESIAN_POINT('Ctrl Pts',(-26.7427538741697,-43.1910304950644,
1390.81341911765));
#145890=CARTESIAN_POINT('Ctrl Pts',(-30.744992244793,-40.7129494105307,
1389.31930147059));
#145891=CARTESIAN_POINT('Ctrl Pts',(-34.2237386972451,-37.5416529948095,
1387.82518382353));
#145892=CARTESIAN_POINT('Ctrl Pts',(-37.7024851496972,-34.3703565790883,
1386.33106617647));
#145893=CARTESIAN_POINT('Ctrl Pts',(-40.5392751458362,-30.6138395280662,
1384.83694852941));
#145894=CARTESIAN_POINT('Ctrl Pts',(-43.3760651419751,-26.8573224770441,
1383.34283088235));
#145895=CARTESIAN_POINT('Ctrl Pts',(-45.4742952008371,-22.6435084734481,
1381.84871323529));
#145896=CARTESIAN_POINT('Ctrl Pts',(-47.5725252596992,-18.4296944698521,
1380.35459558824));
#145897=CARTESIAN_POINT('Ctrl Pts',(-48.8607426731792,-13.9020798956618,
1378.86047794118));
#145898=CARTESIAN_POINT('Ctrl Pts',(-50.1489600866593,-9.37446532147148,
1377.36636029412));
#145899=CARTESIAN_POINT('Ctrl Pts',(-50.5832961557877,-4.68723266073574,
1375.87224264706));
#145900=CARTESIAN_POINT('Ctrl Pts',(-51.0176322249162,-3.12392900021603E-15,
1374.378125));
#145901=CARTESIAN_POINT('Ctrl Pts',(-50.5832961557877,4.68723266073573,
1372.88400735294));
#145902=CARTESIAN_POINT('Ctrl Pts',(-50.1489600866593,9.37446532147149,
1371.38988970588));
#145903=CARTESIAN_POINT('Ctrl Pts',(-48.8607426731792,13.9020798956618,
1369.89577205882));
#145904=CARTESIAN_POINT('Ctrl Pts',(-47.5725252596992,18.4296944698521,
1368.40165441177));
#145905=CARTESIAN_POINT('Ctrl Pts',(-45.4742952008371,22.6435084734481,
1366.90753676471));
#145906=CARTESIAN_POINT('Ctrl Pts',(-43.3760651419751,26.8573224770442,
1365.41341911765));
#145907=CARTESIAN_POINT('Ctrl Pts',(-40.5392751458362,30.6138395280662,
1363.91930147059));
#145908=CARTESIAN_POINT('Ctrl Pts',(-37.7024851496972,34.3703565790883,
1362.42518382353));
#145909=CARTESIAN_POINT('Ctrl Pts',(-34.2237386972451,37.5416529948095,
1360.93106617647));
#145910=CARTESIAN_POINT('Ctrl Pts',(-30.744992244793,40.7129494105307,1359.43694852941));
#145911=CARTESIAN_POINT('Ctrl Pts',(-26.7427538741697,43.1910304950644,
1357.94283088235));
#145912=CARTESIAN_POINT('Ctrl Pts',(-22.7405155035463,45.6691115795981,
1356.44871323529));
#145913=CARTESIAN_POINT('Ctrl Pts',(-18.3510766423074,47.3695892537413,
1354.95459558824));
#145914=CARTESIAN_POINT('Ctrl Pts',(-13.9616377810684,49.0700669278844,
1353.46047794118));
#145915=CARTESIAN_POINT('Ctrl Pts',(-9.33447550508177,49.9350334639422,
1351.96636029412));
#145916=CARTESIAN_POINT('Ctrl Pts',(-4.7073132290951,50.8,1350.47224264706));
#145917=CARTESIAN_POINT('Ctrl Pts',(-6.22120573966855E-15,50.8,1348.978125));
#145918=CARTESIAN_POINT('Ctrl Pts',(4.70731322909511,50.8,1347.48400735294));
#145919=CARTESIAN_POINT('Ctrl Pts',(9.33447550508176,49.9350334639422,1345.98988970588));
#145920=CARTESIAN_POINT('Ctrl Pts',(13.9616377810684,49.0700669278844,1344.49577205882));
#145921=CARTESIAN_POINT('Ctrl Pts',(18.3510766423074,47.3695892537413,1343.00165441176));
#145922=CARTESIAN_POINT('Ctrl Pts',(22.7405155035463,45.6691115795981,1341.50753676471));
#145923=CARTESIAN_POINT('Ctrl Pts',(26.7427538741697,43.1910304950644,1340.01341911765));
#145924=CARTESIAN_POINT('Ctrl Pts',(30.744992244793,40.7129494105307,1338.51930147059));
#145925=CARTESIAN_POINT('Ctrl Pts',(34.2237386972451,37.5416529948095,1337.02518382353));
#145926=CARTESIAN_POINT('Ctrl Pts',(37.7024851496972,34.3703565790883,1335.53106617647));
#145927=CARTESIAN_POINT('Ctrl Pts',(40.5392751458362,30.6138395280662,1334.03694852941));
#145928=CARTESIAN_POINT('Ctrl Pts',(43.3760651419751,26.8573224770442,1332.54283088235));
#145929=CARTESIAN_POINT('Ctrl Pts',(45.4742952008372,22.6435084734481,1331.04871323529));
#145930=CARTESIAN_POINT('Ctrl Pts',(47.5725252596992,18.4296944698521,1329.55459558824));
#145931=CARTESIAN_POINT('Ctrl Pts',(48.8607426731792,13.9020798956618,1328.06047794118));
#145932=CARTESIAN_POINT('Ctrl Pts',(50.1489600866593,9.37446532147146,1326.56636029412));
#145933=CARTESIAN_POINT('Ctrl Pts',(50.5832961557877,4.68723266073574,1325.07224264706));
#145934=CARTESIAN_POINT('Ctrl Pts',(51.0176322249162,9.37178700064808E-15,
1323.578125));
#145935=CARTESIAN_POINT('Ctrl Pts',(50.5832961557877,-4.68723266073572,
1322.08400735294));
#145936=CARTESIAN_POINT('Ctrl Pts',(50.1489600866593,-9.37446532147149,
1320.58988970588));
#145937=CARTESIAN_POINT('Ctrl Pts',(48.8607426731792,-13.9020798956618,
1319.09577205882));
#145938=CARTESIAN_POINT('Ctrl Pts',(47.5725252596992,-18.4296944698521,
1317.60165441176));
#145939=CARTESIAN_POINT('Ctrl Pts',(45.4742952008371,-22.6435084734482,
1316.10753676471));
#145940=CARTESIAN_POINT('Ctrl Pts',(43.3760651419751,-26.8573224770441,
1314.61341911765));
#145941=CARTESIAN_POINT('Ctrl Pts',(40.5392751458362,-30.6138395280662,
1313.11930147059));
#145942=CARTESIAN_POINT('Ctrl Pts',(37.7024851496972,-34.3703565790883,
1311.62518382353));
#145943=CARTESIAN_POINT('Ctrl Pts',(34.2237386972451,-37.5416529948095,
1310.13106617647));
#145944=CARTESIAN_POINT('Ctrl Pts',(30.744992244793,-40.7129494105307,1308.63694852941));
#145945=CARTESIAN_POINT('Ctrl Pts',(26.7427538741697,-43.1910304950644,
1307.14283088235));
#145946=CARTESIAN_POINT('Ctrl Pts',(22.7405155035463,-45.6691115795981,
1305.64871323529));
#145947=CARTESIAN_POINT('Ctrl Pts',(18.3510766423074,-47.3695892537413,
1304.15459558824));
#145948=CARTESIAN_POINT('Ctrl Pts',(13.9616377810684,-49.0700669278844,
1302.66047794118));
#145949=CARTESIAN_POINT('Ctrl Pts',(9.33447550508176,-49.9350334639422,
1301.16636029412));
#145950=CARTESIAN_POINT('Ctrl Pts',(4.70731322909511,-50.8,1299.67224264706));
#145951=CARTESIAN_POINT('Ctrl Pts',(0.,-50.8,1298.178125));
#145952=CARTESIAN_POINT('Ctrl Pts',(-4.70731322909511,-50.8,1296.68400735294));
#145953=CARTESIAN_POINT('Ctrl Pts',(-9.33447550508177,-49.9350334639422,
1295.18988970588));
#145954=CARTESIAN_POINT('Ctrl Pts',(-13.9616377810684,-49.0700669278844,
1293.69577205882));
#145955=CARTESIAN_POINT('Ctrl Pts',(-18.3510766423074,-47.3695892537413,
1292.20165441176));
#145956=CARTESIAN_POINT('Ctrl Pts',(-22.7405155035463,-45.6691115795981,
1290.70753676471));
#145957=CARTESIAN_POINT('Ctrl Pts',(-26.7427538741697,-43.1910304950644,
1289.21341911765));
#145958=CARTESIAN_POINT('Ctrl Pts',(-30.744992244793,-40.7129494105307,
1287.71930147059));
#145959=CARTESIAN_POINT('Ctrl Pts',(-34.2237386972451,-37.5416529948095,
1286.22518382353));
#145960=CARTESIAN_POINT('Ctrl Pts',(-37.7024851496972,-34.3703565790883,
1284.73106617647));
#145961=CARTESIAN_POINT('Ctrl Pts',(-40.5392751458362,-30.6138395280662,
1283.23694852941));
#145962=CARTESIAN_POINT('Ctrl Pts',(-43.3760651419751,-26.8573224770441,
1281.74283088235));
#145963=CARTESIAN_POINT('Ctrl Pts',(-45.4742952008371,-22.6435084734481,
1280.24871323529));
#145964=CARTESIAN_POINT('Ctrl Pts',(-47.5725252596992,-18.4296944698521,
1278.75459558824));
#145965=CARTESIAN_POINT('Ctrl Pts',(-48.8607426731792,-13.9020798956618,
1277.26047794118));
#145966=CARTESIAN_POINT('Ctrl Pts',(-50.1489600866593,-9.37446532147148,
1275.76636029412));
#145967=CARTESIAN_POINT('Ctrl Pts',(-50.5832961557877,-4.68723266073574,
1274.27224264706));
#145968=CARTESIAN_POINT('Ctrl Pts',(-51.0176322249162,-3.12392900021603E-15,
1272.778125));
#145969=CARTESIAN_POINT('Ctrl Pts',(-50.5832961557877,4.68723266073573,
1271.28400735294));
#145970=CARTESIAN_POINT('Ctrl Pts',(-50.1489600866593,9.37446532147149,
1269.78988970588));
#145971=CARTESIAN_POINT('Ctrl Pts',(-48.8607426731792,13.9020798956618,
1268.29577205882));
#145972=CARTESIAN_POINT('Ctrl Pts',(-47.5725252596992,18.4296944698521,
1266.80165441176));
#145973=CARTESIAN_POINT('Ctrl Pts',(-45.4742952008371,22.6435084734481,
1265.30753676471));
#145974=CARTESIAN_POINT('Ctrl Pts',(-43.3760651419751,26.8573224770442,
1263.81341911765));
#145975=CARTESIAN_POINT('Ctrl Pts',(-40.5392751458362,30.6138395280662,
1262.31930147059));
#145976=CARTESIAN_POINT('Ctrl Pts',(-37.7024851496972,34.3703565790883,
1260.82518382353));
#145977=CARTESIAN_POINT('Ctrl Pts',(-34.2237386972451,37.5416529948095,
1259.33106617647));
#145978=CARTESIAN_POINT('Ctrl Pts',(-30.744992244793,40.7129494105307,1257.83694852941));
#145979=CARTESIAN_POINT('Ctrl Pts',(-26.7427538741697,43.1910304950644,
1256.34283088235));
#145980=CARTESIAN_POINT('Ctrl Pts',(-22.7405155035463,45.6691115795981,
1254.84871323529));
#145981=CARTESIAN_POINT('Ctrl Pts',(-18.3510766423074,47.3695892537413,
1253.35459558824));
#145982=CARTESIAN_POINT('Ctrl Pts',(-13.9616377810684,49.0700669278844,
1251.86047794118));
#145983=CARTESIAN_POINT('Ctrl Pts',(-9.33447550508177,49.9350334639422,
1250.36636029412));
#145984=CARTESIAN_POINT('Ctrl Pts',(-4.7073132290951,50.8,1248.87224264706));
#145985=CARTESIAN_POINT('Ctrl Pts',(-6.22120573966855E-15,50.8,1247.378125));
#145986=CARTESIAN_POINT('Ctrl Pts',(4.70731322909511,50.8,1245.88400735294));
#145987=CARTESIAN_POINT('Ctrl Pts',(9.33447550508176,49.9350334639422,1244.38988970588));
#145988=CARTESIAN_POINT('Ctrl Pts',(13.9616377810684,49.0700669278844,1242.89577205882));
#145989=CARTESIAN_POINT('Ctrl Pts',(18.3510766423074,47.3695892537413,1241.40165441176));
#145990=CARTESIAN_POINT('Ctrl Pts',(22.7405155035463,45.6691115795981,1239.90753676471));
#145991=CARTESIAN_POINT('Ctrl Pts',(26.7427538741697,43.1910304950644,1238.41341911765));
#145992=CARTESIAN_POINT('Ctrl Pts',(30.744992244793,40.7129494105307,1236.91930147059));
#145993=CARTESIAN_POINT('Ctrl Pts',(34.2237386972451,37.5416529948095,1235.42518382353));
#145994=CARTESIAN_POINT('Ctrl Pts',(37.7024851496972,34.3703565790883,1233.93106617647));
#145995=CARTESIAN_POINT('Ctrl Pts',(40.5392751458362,30.6138395280662,1232.43694852941));
#145996=CARTESIAN_POINT('Ctrl Pts',(43.3760651419751,26.8573224770442,1230.94283088235));
#145997=CARTESIAN_POINT('Ctrl Pts',(45.4742952008372,22.6435084734481,1229.44871323529));
#145998=CARTESIAN_POINT('Ctrl Pts',(47.5725252596992,18.4296944698521,1227.95459558824));
#145999=CARTESIAN_POINT('Ctrl Pts',(48.8607426731792,13.9020798956618,1226.46047794118));
#146000=CARTESIAN_POINT('Ctrl Pts',(50.1489600866593,9.37446532147146,1224.96636029412));
#146001=CARTESIAN_POINT('Ctrl Pts',(50.5832961557877,4.68723266073574,1223.47224264706));
#146002=CARTESIAN_POINT('Ctrl Pts',(51.0176322249162,9.37178700064808E-15,
1221.978125));
#146003=CARTESIAN_POINT('Ctrl Pts',(50.5832961557877,-4.68723266073572,
1220.48400735294));
#146004=CARTESIAN_POINT('Ctrl Pts',(50.1489600866593,-9.37446532147149,
1218.98988970588));
#146005=CARTESIAN_POINT('Ctrl Pts',(48.8607426731792,-13.9020798956618,
1217.49577205882));
#146006=CARTESIAN_POINT('Ctrl Pts',(47.5725252596992,-18.4296944698521,
1216.00165441176));
#146007=CARTESIAN_POINT('Ctrl Pts',(45.4742952008371,-22.6435084734482,
1214.50753676471));
#146008=CARTESIAN_POINT('Ctrl Pts',(43.3760651419751,-26.8573224770441,
1213.01341911765));
#146009=CARTESIAN_POINT('Ctrl Pts',(40.5392751458362,-30.6138395280662,
1211.51930147059));
#146010=CARTESIAN_POINT('Ctrl Pts',(37.7024851496972,-34.3703565790883,
1210.02518382353));
#146011=CARTESIAN_POINT('Ctrl Pts',(34.2237386972451,-37.5416529948095,
1208.53106617647));
#146012=CARTESIAN_POINT('Ctrl Pts',(30.744992244793,-40.7129494105307,1207.03694852941));
#146013=CARTESIAN_POINT('Ctrl Pts',(26.7427538741697,-43.1910304950644,
1205.54283088235));
#146014=CARTESIAN_POINT('Ctrl Pts',(22.7405155035463,-45.6691115795981,
1204.04871323529));
#146015=CARTESIAN_POINT('Ctrl Pts',(18.3510766423074,-47.3695892537413,
1202.55459558824));
#146016=CARTESIAN_POINT('Ctrl Pts',(13.9616377810684,-49.0700669278844,
1201.06047794118));
#146017=CARTESIAN_POINT('Ctrl Pts',(9.33447550508176,-49.9350334639422,
1199.56636029412));
#146018=CARTESIAN_POINT('Ctrl Pts',(4.70731322909511,-50.8,1198.07224264706));
#146019=CARTESIAN_POINT('Ctrl Pts',(0.,-50.8,1196.578125));
#146020=CARTESIAN_POINT('Ctrl Pts',(-4.70731322909511,-50.8,1195.08400735294));
#146021=CARTESIAN_POINT('Ctrl Pts',(-9.33447550508177,-49.9350334639422,
1193.58988970588));
#146022=CARTESIAN_POINT('Ctrl Pts',(-13.9616377810684,-49.0700669278844,
1192.09577205882));
#146023=CARTESIAN_POINT('Ctrl Pts',(-18.3510766423074,-47.3695892537413,
1190.60165441176));
#146024=CARTESIAN_POINT('Ctrl Pts',(-22.7405155035463,-45.6691115795981,
1189.10753676471));
#146025=CARTESIAN_POINT('Ctrl Pts',(-26.7427538741697,-43.1910304950644,
1187.61341911765));
#146026=CARTESIAN_POINT('Ctrl Pts',(-30.744992244793,-40.7129494105307,
1186.11930147059));
#146027=CARTESIAN_POINT('Ctrl Pts',(-34.2237386972451,-37.5416529948095,
1184.62518382353));
#146028=CARTESIAN_POINT('Ctrl Pts',(-37.7024851496972,-34.3703565790883,
1183.13106617647));
#146029=CARTESIAN_POINT('Ctrl Pts',(-40.5392751458362,-30.6138395280662,
1181.63694852941));
#146030=CARTESIAN_POINT('Ctrl Pts',(-43.3760651419751,-26.8573224770441,
1180.14283088235));
#146031=CARTESIAN_POINT('Ctrl Pts',(-45.4742952008371,-22.6435084734481,
1178.64871323529));
#146032=CARTESIAN_POINT('Ctrl Pts',(-47.5725252596992,-18.4296944698521,
1177.15459558824));
#146033=CARTESIAN_POINT('Ctrl Pts',(-48.8607426731792,-13.9020798956618,
1175.66047794118));
#146034=CARTESIAN_POINT('Ctrl Pts',(-50.1489600866593,-9.37446532147148,
1174.16636029412));
#146035=CARTESIAN_POINT('Ctrl Pts',(-50.5832961557877,-4.68723266073574,
1172.67224264706));
#146036=CARTESIAN_POINT('Ctrl Pts',(-51.0176322249162,-3.12392900021603E-15,
1171.178125));
#146037=CARTESIAN_POINT('Ctrl Pts',(-50.5832961557877,4.68723266073573,
1169.68400735294));
#146038=CARTESIAN_POINT('Ctrl Pts',(-50.1489600866593,9.37446532147149,
1168.18988970588));
#146039=CARTESIAN_POINT('Ctrl Pts',(-48.8607426731792,13.9020798956618,
1166.69577205882));
#146040=CARTESIAN_POINT('Ctrl Pts',(-47.5725252596992,18.4296944698521,
1165.20165441177));
#146041=CARTESIAN_POINT('Ctrl Pts',(-45.4742952008371,22.6435084734481,
1163.70753676471));
#146042=CARTESIAN_POINT('Ctrl Pts',(-43.3760651419751,26.8573224770442,
1162.21341911765));
#146043=CARTESIAN_POINT('Ctrl Pts',(-40.5392751458362,30.6138395280662,
1160.71930147059));
#146044=CARTESIAN_POINT('Ctrl Pts',(-37.7024851496972,34.3703565790883,
1159.22518382353));
#146045=CARTESIAN_POINT('Ctrl Pts',(-34.2237386972451,37.5416529948095,
1157.73106617647));
#146046=CARTESIAN_POINT('Ctrl Pts',(-30.744992244793,40.7129494105307,1156.23694852941));
#146047=CARTESIAN_POINT('Ctrl Pts',(-26.7427538741697,43.1910304950644,
1154.74283088235));
#146048=CARTESIAN_POINT('Ctrl Pts',(-22.7405155035463,45.6691115795981,
1153.24871323529));
#146049=CARTESIAN_POINT('Ctrl Pts',(-18.3510766423074,47.3695892537413,
1151.75459558824));
#146050=CARTESIAN_POINT('Ctrl Pts',(-13.9616377810684,49.0700669278844,
1150.26047794118));
#146051=CARTESIAN_POINT('Ctrl Pts',(-9.33447550508177,49.9350334639422,
1148.76636029412));
#146052=CARTESIAN_POINT('Ctrl Pts',(-4.7073132290951,50.8,1147.27224264706));
#146053=CARTESIAN_POINT('Ctrl Pts',(-6.22120573966855E-15,50.8,1145.778125));
#146054=CARTESIAN_POINT('Ctrl Pts',(4.70731322909511,50.8,1144.28400735294));
#146055=CARTESIAN_POINT('Ctrl Pts',(9.33447550508176,49.9350334639422,1142.78988970588));
#146056=CARTESIAN_POINT('Ctrl Pts',(13.9616377810684,49.0700669278844,1141.29577205882));
#146057=CARTESIAN_POINT('Ctrl Pts',(18.3510766423074,47.3695892537413,1139.80165441176));
#146058=CARTESIAN_POINT('Ctrl Pts',(22.7405155035463,45.6691115795981,1138.30753676471));
#146059=CARTESIAN_POINT('Ctrl Pts',(26.7427538741697,43.1910304950644,1136.81341911765));
#146060=CARTESIAN_POINT('Ctrl Pts',(30.744992244793,40.7129494105307,1135.31930147059));
#146061=CARTESIAN_POINT('Ctrl Pts',(34.2237386972451,37.5416529948095,1133.82518382353));
#146062=CARTESIAN_POINT('Ctrl Pts',(37.7024851496972,34.3703565790883,1132.33106617647));
#146063=CARTESIAN_POINT('Ctrl Pts',(40.5392751458362,30.6138395280662,1130.83694852941));
#146064=CARTESIAN_POINT('Ctrl Pts',(43.3760651419751,26.8573224770442,1129.34283088235));
#146065=CARTESIAN_POINT('Ctrl Pts',(45.4742952008372,22.6435084734481,1127.84871323529));
#146066=CARTESIAN_POINT('Ctrl Pts',(47.5725252596992,18.4296944698521,1126.35459558824));
#146067=CARTESIAN_POINT('Ctrl Pts',(48.8607426731792,13.9020798956618,1124.86047794118));
#146068=CARTESIAN_POINT('Ctrl Pts',(50.1489600866593,9.37446532147146,1123.36636029412));
#146069=CARTESIAN_POINT('Ctrl Pts',(50.5832961557877,4.68723266073574,1121.87224264706));
#146070=CARTESIAN_POINT('Ctrl Pts',(51.0176322249162,9.37178700064808E-15,
1120.378125));
#146071=CARTESIAN_POINT('Ctrl Pts',(50.5832961557877,-4.68723266073572,
1118.88400735294));
#146072=CARTESIAN_POINT('Ctrl Pts',(50.1489600866593,-9.37446532147149,
1117.38988970588));
#146073=CARTESIAN_POINT('Ctrl Pts',(48.8607426731792,-13.9020798956618,
1115.89577205882));
#146074=CARTESIAN_POINT('Ctrl Pts',(47.5725252596992,-18.4296944698521,
1114.40165441176));
#146075=CARTESIAN_POINT('Ctrl Pts',(45.4742952008371,-22.6435084734482,
1112.90753676471));
#146076=CARTESIAN_POINT('Ctrl Pts',(43.3760651419751,-26.8573224770441,
1111.41341911765));
#146077=CARTESIAN_POINT('Ctrl Pts',(40.5392751458362,-30.6138395280662,
1109.91930147059));
#146078=CARTESIAN_POINT('Ctrl Pts',(37.7024851496972,-34.3703565790883,
1108.42518382353));
#146079=CARTESIAN_POINT('Ctrl Pts',(34.2237386972451,-37.5416529948095,
1106.93106617647));
#146080=CARTESIAN_POINT('Ctrl Pts',(30.744992244793,-40.7129494105307,1105.43694852941));
#146081=CARTESIAN_POINT('Ctrl Pts',(26.7427538741697,-43.1910304950644,
1103.94283088235));
#146082=CARTESIAN_POINT('Ctrl Pts',(22.7405155035463,-45.6691115795981,
1102.44871323529));
#146083=CARTESIAN_POINT('Ctrl Pts',(18.3510766423074,-47.3695892537413,
1100.95459558824));
#146084=CARTESIAN_POINT('Ctrl Pts',(13.9616377810684,-49.0700669278844,
1099.46047794118));
#146085=CARTESIAN_POINT('Ctrl Pts',(9.33447550508176,-49.9350334639422,
1097.96636029412));
#146086=CARTESIAN_POINT('Ctrl Pts',(4.70731322909511,-50.8,1096.47224264706));
#146087=CARTESIAN_POINT('Ctrl Pts',(0.,-50.8,1094.978125));
#146088=CARTESIAN_POINT('Ctrl Pts',(-4.70731322909511,-50.8,1093.48400735294));
#146089=CARTESIAN_POINT('Ctrl Pts',(-9.33447550508177,-49.9350334639422,
1091.98988970588));
#146090=CARTESIAN_POINT('Ctrl Pts',(-13.9616377810684,-49.0700669278844,
1090.49577205882));
#146091=CARTESIAN_POINT('Ctrl Pts',(-18.3510766423074,-47.3695892537413,
1089.00165441176));
#146092=CARTESIAN_POINT('Ctrl Pts',(-22.7405155035463,-45.6691115795981,
1087.50753676471));
#146093=CARTESIAN_POINT('Ctrl Pts',(-26.7427538741697,-43.1910304950644,
1086.01341911765));
#146094=CARTESIAN_POINT('Ctrl Pts',(-30.744992244793,-40.7129494105307,
1084.51930147059));
#146095=CARTESIAN_POINT('Ctrl Pts',(-34.2237386972451,-37.5416529948095,
1083.02518382353));
#146096=CARTESIAN_POINT('Ctrl Pts',(-37.7024851496972,-34.3703565790883,
1081.53106617647));
#146097=CARTESIAN_POINT('Ctrl Pts',(-40.5392751458362,-30.6138395280662,
1080.03694852941));
#146098=CARTESIAN_POINT('Ctrl Pts',(-43.3760651419751,-26.8573224770441,
1078.54283088235));
#146099=CARTESIAN_POINT('Ctrl Pts',(-45.4742952008371,-22.6435084734481,
1077.04871323529));
#146100=CARTESIAN_POINT('Ctrl Pts',(-47.5725252596992,-18.4296944698521,
1075.55459558824));
#146101=CARTESIAN_POINT('Ctrl Pts',(-48.8607426731792,-13.9020798956618,
1074.06047794118));
#146102=CARTESIAN_POINT('Ctrl Pts',(-50.1489600866593,-9.37446532147148,
1072.56636029412));
#146103=CARTESIAN_POINT('Ctrl Pts',(-50.5832961557877,-4.68723266073574,
1071.07224264706));
#146104=CARTESIAN_POINT('Ctrl Pts',(-51.0176322249162,-3.12392900021603E-15,
1069.578125));
#146105=CARTESIAN_POINT('Ctrl Pts',(-50.5832961557877,4.68723266073573,
1068.08400735294));
#146106=CARTESIAN_POINT('Ctrl Pts',(-50.1489600866593,9.37446532147149,
1066.58988970588));
#146107=CARTESIAN_POINT('Ctrl Pts',(-48.8607426731792,13.9020798956618,
1065.09577205882));
#146108=CARTESIAN_POINT('Ctrl Pts',(-47.5725252596992,18.4296944698521,
1063.60165441176));
#146109=CARTESIAN_POINT('Ctrl Pts',(-45.4742952008371,22.6435084734481,
1062.10753676471));
#146110=CARTESIAN_POINT('Ctrl Pts',(-43.3760651419751,26.8573224770442,
1060.61341911765));
#146111=CARTESIAN_POINT('Ctrl Pts',(-40.5392751458362,30.6138395280662,
1059.11930147059));
#146112=CARTESIAN_POINT('Ctrl Pts',(-37.7024851496972,34.3703565790883,
1057.62518382353));
#146113=CARTESIAN_POINT('Ctrl Pts',(-34.2237386972451,37.5416529948095,
1056.13106617647));
#146114=CARTESIAN_POINT('Ctrl Pts',(-30.744992244793,40.7129494105307,1054.63694852941));
#146115=CARTESIAN_POINT('Ctrl Pts',(-26.7427538741697,43.1910304950644,
1053.14283088235));
#146116=CARTESIAN_POINT('Ctrl Pts',(-22.7405155035463,45.6691115795981,
1051.64871323529));
#146117=CARTESIAN_POINT('Ctrl Pts',(-18.3510766423074,47.3695892537413,
1050.15459558824));
#146118=CARTESIAN_POINT('Ctrl Pts',(-13.9616377810684,49.0700669278844,
1048.66047794118));
#146119=CARTESIAN_POINT('Ctrl Pts',(-9.33447550508177,49.9350334639422,
1047.16636029412));
#146120=CARTESIAN_POINT('Ctrl Pts',(-4.7073132290951,50.8,1045.67224264706));
#146121=CARTESIAN_POINT('Ctrl Pts',(-6.22120573966855E-15,50.8,1044.178125));
#146122=CARTESIAN_POINT('Ctrl Pts',(4.70731322909511,50.8,1042.68400735294));
#146123=CARTESIAN_POINT('Ctrl Pts',(9.33447550508176,49.9350334639422,1041.18988970588));
#146124=CARTESIAN_POINT('Ctrl Pts',(13.9616377810684,49.0700669278844,1039.69577205882));
#146125=CARTESIAN_POINT('Ctrl Pts',(18.3510766423074,47.3695892537413,1038.20165441176));
#146126=CARTESIAN_POINT('Ctrl Pts',(22.7405155035463,45.6691115795981,1036.70753676471));
#146127=CARTESIAN_POINT('Ctrl Pts',(26.7427538741697,43.1910304950644,1035.21341911765));
#146128=CARTESIAN_POINT('Ctrl Pts',(30.744992244793,40.7129494105307,1033.71930147059));
#146129=CARTESIAN_POINT('Ctrl Pts',(34.2237386972451,37.5416529948095,1032.22518382353));
#146130=CARTESIAN_POINT('Ctrl Pts',(37.7024851496972,34.3703565790883,1030.73106617647));
#146131=CARTESIAN_POINT('Ctrl Pts',(40.5392751458362,30.6138395280662,1029.23694852941));
#146132=CARTESIAN_POINT('Ctrl Pts',(43.3760651419751,26.8573224770442,1027.74283088235));
#146133=CARTESIAN_POINT('Ctrl Pts',(45.4742952008372,22.6435084734481,1026.24871323529));
#146134=CARTESIAN_POINT('Ctrl Pts',(47.5725252596992,18.4296944698521,1024.75459558824));
#146135=CARTESIAN_POINT('Ctrl Pts',(48.8607426731792,13.9020798956618,1023.26047794118));
#146136=CARTESIAN_POINT('Ctrl Pts',(50.1489600866593,9.37446532147146,1021.76636029412));
#146137=CARTESIAN_POINT('Ctrl Pts',(50.5832961557877,4.68723266073574,1020.27224264706));
#146138=CARTESIAN_POINT('Ctrl Pts',(51.0176322249162,9.37178700064808E-15,
1018.778125));
#146139=CARTESIAN_POINT('Ctrl Pts',(50.5832961557877,-4.68723266073572,
1017.28400735294));
#146140=CARTESIAN_POINT('Ctrl Pts',(50.1489600866593,-9.37446532147149,
1015.78988970588));
#146141=CARTESIAN_POINT('Ctrl Pts',(48.8607426731792,-13.9020798956618,
1014.29577205882));
#146142=CARTESIAN_POINT('Ctrl Pts',(47.5725252596992,-18.4296944698521,
1012.80165441176));
#146143=CARTESIAN_POINT('Ctrl Pts',(45.4742952008371,-22.6435084734482,
1011.30753676471));
#146144=CARTESIAN_POINT('Ctrl Pts',(43.3760651419751,-26.8573224770441,
1009.81341911765));
#146145=CARTESIAN_POINT('Ctrl Pts',(40.5392751458362,-30.6138395280662,
1008.31930147059));
#146146=CARTESIAN_POINT('Ctrl Pts',(37.7024851496972,-34.3703565790883,
1006.82518382353));
#146147=CARTESIAN_POINT('Ctrl Pts',(34.2237386972451,-37.5416529948095,
1005.33106617647));
#146148=CARTESIAN_POINT('Ctrl Pts',(30.744992244793,-40.7129494105307,1003.83694852941));
#146149=CARTESIAN_POINT('Ctrl Pts',(26.7427538741697,-43.1910304950644,
1002.34283088235));
#146150=CARTESIAN_POINT('Ctrl Pts',(22.7405155035463,-45.6691115795981,
1000.84871323529));
#146151=CARTESIAN_POINT('Ctrl Pts',(18.3510766423074,-47.3695892537413,
999.354595588235));
#146152=CARTESIAN_POINT('Ctrl Pts',(13.9616377810684,-49.0700669278844,
997.860477941177));
#146153=CARTESIAN_POINT('Ctrl Pts',(9.33447550508176,-49.9350334639422,
996.366360294118));
#146154=CARTESIAN_POINT('Ctrl Pts',(4.70731322909511,-50.8,994.872242647059));
#146155=CARTESIAN_POINT('Ctrl Pts',(0.,-50.8,993.378125));
#146156=CARTESIAN_POINT('Ctrl Pts',(-4.70731322909511,-50.8,991.884007352941));
#146157=CARTESIAN_POINT('Ctrl Pts',(-9.33447550508177,-49.9350334639422,
990.389889705883));
#146158=CARTESIAN_POINT('Ctrl Pts',(-13.9616377810684,-49.0700669278844,
988.895772058824));
#146159=CARTESIAN_POINT('Ctrl Pts',(-18.3510766423074,-47.3695892537413,
987.401654411765));
#146160=CARTESIAN_POINT('Ctrl Pts',(-22.7405155035463,-45.6691115795981,
985.907536764706));
#146161=CARTESIAN_POINT('Ctrl Pts',(-26.7427538741697,-43.1910304950644,
984.413419117647));
#146162=CARTESIAN_POINT('Ctrl Pts',(-30.744992244793,-40.7129494105307,
982.919301470588));
#146163=CARTESIAN_POINT('Ctrl Pts',(-34.2237386972451,-37.5416529948095,
981.425183823529));
#146164=CARTESIAN_POINT('Ctrl Pts',(-37.7024851496972,-34.3703565790883,
979.931066176471));
#146165=CARTESIAN_POINT('Ctrl Pts',(-40.5392751458362,-30.6138395280662,
978.436948529412));
#146166=CARTESIAN_POINT('Ctrl Pts',(-43.3760651419751,-26.8573224770441,
976.942830882353));
#146167=CARTESIAN_POINT('Ctrl Pts',(-45.4742952008371,-22.6435084734481,
975.448713235294));
#146168=CARTESIAN_POINT('Ctrl Pts',(-47.5725252596992,-18.4296944698521,
973.954595588235));
#146169=CARTESIAN_POINT('Ctrl Pts',(-48.8607426731792,-13.9020798956618,
972.460477941177));
#146170=CARTESIAN_POINT('Ctrl Pts',(-50.1489600866593,-9.37446532147148,
970.966360294118));
#146171=CARTESIAN_POINT('Ctrl Pts',(-50.5832961557877,-4.68723266073574,
969.472242647059));
#146172=CARTESIAN_POINT('Ctrl Pts',(-51.0176322249162,-3.12392900021603E-15,
967.978125));
#146173=CARTESIAN_POINT('Ctrl Pts',(-50.5832961557877,4.68723266073573,
966.484007352941));
#146174=CARTESIAN_POINT('Ctrl Pts',(-50.1489600866593,9.37446532147149,
964.989889705882));
#146175=CARTESIAN_POINT('Ctrl Pts',(-48.8607426731792,13.9020798956618,
963.495772058824));
#146176=CARTESIAN_POINT('Ctrl Pts',(-47.5725252596992,18.4296944698521,
962.001654411765));
#146177=CARTESIAN_POINT('Ctrl Pts',(-45.4742952008371,22.6435084734481,
960.507536764706));
#146178=CARTESIAN_POINT('Ctrl Pts',(-43.3760651419751,26.8573224770442,
959.013419117647));
#146179=CARTESIAN_POINT('Ctrl Pts',(-40.5392751458362,30.6138395280662,
957.519301470588));
#146180=CARTESIAN_POINT('Ctrl Pts',(-37.7024851496972,34.3703565790883,
956.02518382353));
#146181=CARTESIAN_POINT('Ctrl Pts',(-34.2237386972451,37.5416529948095,
954.531066176471));
#146182=CARTESIAN_POINT('Ctrl Pts',(-30.744992244793,40.7129494105307,953.036948529412));
#146183=CARTESIAN_POINT('Ctrl Pts',(-26.7427538741697,43.1910304950644,
951.542830882353));
#146184=CARTESIAN_POINT('Ctrl Pts',(-22.7405155035463,45.6691115795981,
950.048713235294));
#146185=CARTESIAN_POINT('Ctrl Pts',(-18.3510766423074,47.3695892537413,
948.554595588235));
#146186=CARTESIAN_POINT('Ctrl Pts',(-13.9616377810684,49.0700669278844,
947.060477941177));
#146187=CARTESIAN_POINT('Ctrl Pts',(-9.33447550508177,49.9350334639422,
945.566360294118));
#146188=CARTESIAN_POINT('Ctrl Pts',(-4.7073132290951,50.8,944.072242647059));
#146189=CARTESIAN_POINT('Ctrl Pts',(-6.22120573966855E-15,50.8,942.578125));
#146190=CARTESIAN_POINT('Ctrl Pts',(4.70731322909511,50.8,941.084007352941));
#146191=CARTESIAN_POINT('Ctrl Pts',(9.33447550508176,49.9350334639422,939.589889705883));
#146192=CARTESIAN_POINT('Ctrl Pts',(13.9616377810684,49.0700669278844,938.095772058824));
#146193=CARTESIAN_POINT('Ctrl Pts',(18.3510766423074,47.3695892537413,936.601654411765));
#146194=CARTESIAN_POINT('Ctrl Pts',(22.7405155035463,45.6691115795981,935.107536764706));
#146195=CARTESIAN_POINT('Ctrl Pts',(26.7427538741697,43.1910304950644,933.613419117647));
#146196=CARTESIAN_POINT('Ctrl Pts',(30.744992244793,40.7129494105307,932.119301470589));
#146197=CARTESIAN_POINT('Ctrl Pts',(34.2237386972451,37.5416529948095,930.625183823529));
#146198=CARTESIAN_POINT('Ctrl Pts',(37.7024851496972,34.3703565790883,929.131066176471));
#146199=CARTESIAN_POINT('Ctrl Pts',(40.5392751458362,30.6138395280662,927.636948529412));
#146200=CARTESIAN_POINT('Ctrl Pts',(43.3760651419751,26.8573224770442,926.142830882353));
#146201=CARTESIAN_POINT('Ctrl Pts',(45.4742952008372,22.6435084734481,924.648713235294));
#146202=CARTESIAN_POINT('Ctrl Pts',(47.5725252596992,18.4296944698521,923.154595588235));
#146203=CARTESIAN_POINT('Ctrl Pts',(48.8607426731792,13.9020798956618,921.660477941176));
#146204=CARTESIAN_POINT('Ctrl Pts',(50.1489600866593,9.37446532147146,920.166360294118));
#146205=CARTESIAN_POINT('Ctrl Pts',(50.5832961557877,4.68723266073574,918.672242647059));
#146206=CARTESIAN_POINT('Ctrl Pts',(51.0176322249162,9.37178700064808E-15,
917.178125));
#146207=CARTESIAN_POINT('Ctrl Pts',(50.5832961557877,-4.68723266073572,
915.684007352941));
#146208=CARTESIAN_POINT('Ctrl Pts',(50.1489600866593,-9.37446532147149,
914.189889705882));
#146209=CARTESIAN_POINT('Ctrl Pts',(48.8607426731792,-13.9020798956618,
912.695772058824));
#146210=CARTESIAN_POINT('Ctrl Pts',(47.5725252596992,-18.4296944698521,
911.201654411765));
#146211=CARTESIAN_POINT('Ctrl Pts',(45.4742952008371,-22.6435084734482,
909.707536764706));
#146212=CARTESIAN_POINT('Ctrl Pts',(43.3760651419751,-26.8573224770441,
908.213419117647));
#146213=CARTESIAN_POINT('Ctrl Pts',(40.5392751458362,-30.6138395280662,
906.719301470588));
#146214=CARTESIAN_POINT('Ctrl Pts',(37.7024851496972,-34.3703565790883,
905.22518382353));
#146215=CARTESIAN_POINT('Ctrl Pts',(34.2237386972451,-37.5416529948095,
903.731066176471));
#146216=CARTESIAN_POINT('Ctrl Pts',(30.744992244793,-40.7129494105307,902.236948529412));
#146217=CARTESIAN_POINT('Ctrl Pts',(26.7427538741697,-43.1910304950644,
900.742830882353));
#146218=CARTESIAN_POINT('Ctrl Pts',(22.7405155035463,-45.6691115795981,
899.248713235294));
#146219=CARTESIAN_POINT('Ctrl Pts',(18.3510766423074,-47.3695892537413,
897.754595588235));
#146220=CARTESIAN_POINT('Ctrl Pts',(13.9616377810684,-49.0700669278844,
896.260477941177));
#146221=CARTESIAN_POINT('Ctrl Pts',(9.33447550508176,-49.9350334639422,
894.766360294118));
#146222=CARTESIAN_POINT('Ctrl Pts',(4.70731322909511,-50.8,893.272242647059));
#146223=CARTESIAN_POINT('Ctrl Pts',(0.,-50.8,891.778125));
#146224=CARTESIAN_POINT('Ctrl Pts',(-4.70731322909511,-50.8,890.284007352941));
#146225=CARTESIAN_POINT('Ctrl Pts',(-9.33447550508177,-49.9350334639422,
888.789889705882));
#146226=CARTESIAN_POINT('Ctrl Pts',(-13.9616377810684,-49.0700669278844,
887.295772058824));
#146227=CARTESIAN_POINT('Ctrl Pts',(-18.3510766423074,-47.3695892537413,
885.801654411765));
#146228=CARTESIAN_POINT('Ctrl Pts',(-22.7405155035463,-45.6691115795981,
884.307536764706));
#146229=CARTESIAN_POINT('Ctrl Pts',(-26.7427538741697,-43.1910304950644,
882.813419117647));
#146230=CARTESIAN_POINT('Ctrl Pts',(-30.744992244793,-40.7129494105307,
881.319301470588));
#146231=CARTESIAN_POINT('Ctrl Pts',(-34.2237386972451,-37.5416529948095,
879.82518382353));
#146232=CARTESIAN_POINT('Ctrl Pts',(-37.7024851496972,-34.3703565790883,
878.331066176471));
#146233=CARTESIAN_POINT('Ctrl Pts',(-40.5392751458362,-30.6138395280662,
876.836948529412));
#146234=CARTESIAN_POINT('Ctrl Pts',(-43.3760651419751,-26.8573224770441,
875.342830882353));
#146235=CARTESIAN_POINT('Ctrl Pts',(-45.4742952008371,-22.6435084734481,
873.848713235294));
#146236=CARTESIAN_POINT('Ctrl Pts',(-47.5725252596992,-18.4296944698521,
872.354595588235));
#146237=CARTESIAN_POINT('Ctrl Pts',(-48.8607426731792,-13.9020798956618,
870.860477941176));
#146238=CARTESIAN_POINT('Ctrl Pts',(-50.1489600866593,-9.37446532147148,
869.366360294118));
#146239=CARTESIAN_POINT('Ctrl Pts',(-50.5832961557877,-4.68723266073574,
867.872242647059));
#146240=CARTESIAN_POINT('Ctrl Pts',(-51.0176322249162,-3.12392900021603E-15,
866.378125));
#146241=CARTESIAN_POINT('Ctrl Pts',(-50.5832961557877,4.68723266073573,
864.884007352941));
#146242=CARTESIAN_POINT('Ctrl Pts',(-50.1489600866593,9.37446532147149,
863.389889705882));
#146243=CARTESIAN_POINT('Ctrl Pts',(-48.8607426731792,13.9020798956618,
861.895772058824));
#146244=CARTESIAN_POINT('Ctrl Pts',(-47.5725252596992,18.4296944698521,
860.401654411765));
#146245=CARTESIAN_POINT('Ctrl Pts',(-45.4742952008371,22.6435084734481,
858.907536764706));
#146246=CARTESIAN_POINT('Ctrl Pts',(-43.3760651419751,26.8573224770442,
857.413419117647));
#146247=CARTESIAN_POINT('Ctrl Pts',(-40.5392751458362,30.6138395280662,
855.919301470588));
#146248=CARTESIAN_POINT('Ctrl Pts',(-37.7024851496972,34.3703565790883,
854.425183823529));
#146249=CARTESIAN_POINT('Ctrl Pts',(-34.2237386972451,37.5416529948095,
852.931066176471));
#146250=CARTESIAN_POINT('Ctrl Pts',(-30.744992244793,40.7129494105307,851.436948529412));
#146251=CARTESIAN_POINT('Ctrl Pts',(-26.7427538741697,43.1910304950644,
849.942830882353));
#146252=CARTESIAN_POINT('Ctrl Pts',(-22.7405155035463,45.6691115795981,
848.448713235294));
#146253=CARTESIAN_POINT('Ctrl Pts',(-18.3510766423074,47.3695892537413,
846.954595588235));
#146254=CARTESIAN_POINT('Ctrl Pts',(-13.9616377810684,49.0700669278844,
845.460477941177));
#146255=CARTESIAN_POINT('Ctrl Pts',(-9.33447550508177,49.9350334639422,
843.966360294118));
#146256=CARTESIAN_POINT('Ctrl Pts',(-4.7073132290951,50.8,842.472242647059));
#146257=CARTESIAN_POINT('Ctrl Pts',(-6.22120573966855E-15,50.8,840.978125));
#146258=CARTESIAN_POINT('Ctrl Pts',(4.70731322909511,50.8,839.484007352941));
#146259=CARTESIAN_POINT('Ctrl Pts',(9.33447550508176,49.9350334639422,837.989889705883));
#146260=CARTESIAN_POINT('Ctrl Pts',(13.9616377810684,49.0700669278844,836.495772058824));
#146261=CARTESIAN_POINT('Ctrl Pts',(18.3510766423074,47.3695892537413,835.001654411765));
#146262=CARTESIAN_POINT('Ctrl Pts',(22.7405155035463,45.6691115795981,833.507536764706));
#146263=CARTESIAN_POINT('Ctrl Pts',(26.7427538741697,43.1910304950644,832.013419117647));
#146264=CARTESIAN_POINT('Ctrl Pts',(30.744992244793,40.7129494105307,830.519301470588));
#146265=CARTESIAN_POINT('Ctrl Pts',(34.2237386972451,37.5416529948095,829.025183823529));
#146266=CARTESIAN_POINT('Ctrl Pts',(37.7024851496972,34.3703565790883,827.531066176471));
#146267=CARTESIAN_POINT('Ctrl Pts',(40.5392751458362,30.6138395280662,826.036948529412));
#146268=CARTESIAN_POINT('Ctrl Pts',(43.3760651419751,26.8573224770442,824.542830882353));
#146269=CARTESIAN_POINT('Ctrl Pts',(45.4742952008372,22.6435084734481,823.048713235294));
#146270=CARTESIAN_POINT('Ctrl Pts',(47.5725252596992,18.4296944698521,821.554595588236));
#146271=CARTESIAN_POINT('Ctrl Pts',(48.8607426731792,13.9020798956618,820.060477941176));
#146272=CARTESIAN_POINT('Ctrl Pts',(50.1489600866593,9.37446532147146,818.566360294118));
#146273=CARTESIAN_POINT('Ctrl Pts',(50.5832961557877,4.68723266073574,817.072242647059));
#146274=CARTESIAN_POINT('Ctrl Pts',(51.0176322249162,9.37178700064808E-15,
815.578125));
#146275=CARTESIAN_POINT('Ctrl Pts',(50.5832961557877,-4.68723266073572,
814.084007352941));
#146276=CARTESIAN_POINT('Ctrl Pts',(50.1489600866593,-9.37446532147149,
812.589889705883));
#146277=CARTESIAN_POINT('Ctrl Pts',(48.8607426731792,-13.9020798956618,
811.095772058824));
#146278=CARTESIAN_POINT('Ctrl Pts',(47.5725252596992,-18.4296944698521,
809.601654411765));
#146279=CARTESIAN_POINT('Ctrl Pts',(45.4742952008371,-22.6435084734482,
808.107536764706));
#146280=CARTESIAN_POINT('Ctrl Pts',(43.3760651419751,-26.8573224770441,
806.613419117647));
#146281=CARTESIAN_POINT('Ctrl Pts',(40.5392751458362,-30.6138395280662,
805.119301470588));
#146282=CARTESIAN_POINT('Ctrl Pts',(37.7024851496972,-34.3703565790883,
803.625183823529));
#146283=CARTESIAN_POINT('Ctrl Pts',(34.2237386972451,-37.5416529948095,
802.131066176471));
#146284=CARTESIAN_POINT('Ctrl Pts',(30.744992244793,-40.7129494105307,800.636948529412));
#146285=CARTESIAN_POINT('Ctrl Pts',(26.7427538741697,-43.1910304950644,
799.142830882353));
#146286=CARTESIAN_POINT('Ctrl Pts',(22.7405155035463,-45.6691115795981,
797.648713235294));
#146287=CARTESIAN_POINT('Ctrl Pts',(18.3510766423074,-47.3695892537413,
796.154595588235));
#146288=CARTESIAN_POINT('Ctrl Pts',(13.9616377810684,-49.0700669278844,
794.660477941177));
#146289=CARTESIAN_POINT('Ctrl Pts',(9.33447550508176,-49.9350334639422,
793.166360294118));
#146290=CARTESIAN_POINT('Ctrl Pts',(4.70731322909511,-50.8,791.672242647059));
#146291=CARTESIAN_POINT('Ctrl Pts',(0.,-50.8,790.178125));
#146292=CARTESIAN_POINT('Ctrl Pts',(-4.70731322909511,-50.8,788.684007352941));
#146293=CARTESIAN_POINT('Ctrl Pts',(-9.33447550508177,-49.9350334639422,
787.189889705882));
#146294=CARTESIAN_POINT('Ctrl Pts',(-13.9616377810684,-49.0700669278844,
785.695772058824));
#146295=CARTESIAN_POINT('Ctrl Pts',(-18.3510766423074,-47.3695892537413,
784.201654411765));
#146296=CARTESIAN_POINT('Ctrl Pts',(-22.7405155035463,-45.6691115795981,
782.707536764706));
#146297=CARTESIAN_POINT('Ctrl Pts',(-26.7427538741697,-43.1910304950644,
781.213419117647));
#146298=CARTESIAN_POINT('Ctrl Pts',(-30.744992244793,-40.7129494105307,
779.719301470588));
#146299=CARTESIAN_POINT('Ctrl Pts',(-34.2237386972451,-37.5416529948095,
778.22518382353));
#146300=CARTESIAN_POINT('Ctrl Pts',(-37.7024851496972,-34.3703565790883,
776.731066176471));
#146301=CARTESIAN_POINT('Ctrl Pts',(-40.5392751458362,-30.6138395280662,
775.236948529412));
#146302=CARTESIAN_POINT('Ctrl Pts',(-43.3760651419751,-26.8573224770441,
773.742830882353));
#146303=CARTESIAN_POINT('Ctrl Pts',(-45.4742952008371,-22.6435084734481,
772.248713235294));
#146304=CARTESIAN_POINT('Ctrl Pts',(-47.5725252596992,-18.4296944698521,
770.754595588236));
#146305=CARTESIAN_POINT('Ctrl Pts',(-48.8607426731792,-13.9020798956618,
769.260477941177));
#146306=CARTESIAN_POINT('Ctrl Pts',(-50.1489600866593,-9.37446532147148,
767.766360294118));
#146307=CARTESIAN_POINT('Ctrl Pts',(-50.5832961557877,-4.68723266073574,
766.272242647059));
#146308=CARTESIAN_POINT('Ctrl Pts',(-51.0176322249162,-3.12392900021603E-15,
764.778125));
#146309=CARTESIAN_POINT('Ctrl Pts',(-50.5832961557877,4.68723266073573,
763.284007352941));
#146310=CARTESIAN_POINT('Ctrl Pts',(-50.1489600866593,9.37446532147149,
761.789889705883));
#146311=CARTESIAN_POINT('Ctrl Pts',(-48.8607426731792,13.9020798956618,
760.295772058824));
#146312=CARTESIAN_POINT('Ctrl Pts',(-47.5725252596992,18.4296944698521,
758.801654411765));
#146313=CARTESIAN_POINT('Ctrl Pts',(-45.4742952008371,22.6435084734481,
757.307536764706));
#146314=CARTESIAN_POINT('Ctrl Pts',(-43.3760651419751,26.8573224770442,
755.813419117647));
#146315=CARTESIAN_POINT('Ctrl Pts',(-40.5392751458362,30.6138395280662,
754.319301470588));
#146316=CARTESIAN_POINT('Ctrl Pts',(-37.7024851496972,34.3703565790883,
752.825183823529));
#146317=CARTESIAN_POINT('Ctrl Pts',(-34.2237386972451,37.5416529948095,
751.331066176471));
#146318=CARTESIAN_POINT('Ctrl Pts',(-30.744992244793,40.7129494105307,749.836948529412));
#146319=CARTESIAN_POINT('Ctrl Pts',(-26.7427538741697,43.1910304950644,
748.342830882353));
#146320=CARTESIAN_POINT('Ctrl Pts',(-22.7405155035463,45.6691115795981,
746.848713235294));
#146321=CARTESIAN_POINT('Ctrl Pts',(-18.3510766423074,47.3695892537413,
745.354595588235));
#146322=CARTESIAN_POINT('Ctrl Pts',(-13.9616377810684,49.0700669278844,
743.860477941176));
#146323=CARTESIAN_POINT('Ctrl Pts',(-9.33447550508177,49.9350334639422,
742.366360294118));
#146324=CARTESIAN_POINT('Ctrl Pts',(-4.7073132290951,50.8,740.872242647059));
#146325=CARTESIAN_POINT('Ctrl Pts',(-6.22120573966855E-15,50.8,739.378125));
#146326=CARTESIAN_POINT('Ctrl Pts',(4.70731322909511,50.8,737.884007352941));
#146327=CARTESIAN_POINT('Ctrl Pts',(9.33447550508176,49.9350334639422,736.389889705882));
#146328=CARTESIAN_POINT('Ctrl Pts',(13.9616377810684,49.0700669278844,734.895772058824));
#146329=CARTESIAN_POINT('Ctrl Pts',(18.3510766423074,47.3695892537413,733.401654411765));
#146330=CARTESIAN_POINT('Ctrl Pts',(22.7405155035463,45.6691115795981,731.907536764706));
#146331=CARTESIAN_POINT('Ctrl Pts',(26.7427538741697,43.1910304950644,730.413419117647));
#146332=CARTESIAN_POINT('Ctrl Pts',(30.744992244793,40.7129494105307,728.919301470588));
#146333=CARTESIAN_POINT('Ctrl Pts',(34.2237386972451,37.5416529948095,727.425183823529));
#146334=CARTESIAN_POINT('Ctrl Pts',(37.7024851496972,34.3703565790883,725.931066176471));
#146335=CARTESIAN_POINT('Ctrl Pts',(40.5392751458362,30.6138395280662,724.436948529412));
#146336=CARTESIAN_POINT('Ctrl Pts',(43.3760651419751,26.8573224770442,722.942830882353));
#146337=CARTESIAN_POINT('Ctrl Pts',(45.4742952008372,22.6435084734481,721.448713235294));
#146338=CARTESIAN_POINT('Ctrl Pts',(47.5725252596992,18.4296944698521,719.954595588235));
#146339=CARTESIAN_POINT('Ctrl Pts',(48.8607426731792,13.9020798956618,718.460477941177));
#146340=CARTESIAN_POINT('Ctrl Pts',(50.1489600866593,9.37446532147146,716.966360294118));
#146341=CARTESIAN_POINT('Ctrl Pts',(50.5832961557877,4.68723266073574,715.472242647059));
#146342=CARTESIAN_POINT('Ctrl Pts',(51.0176322249162,9.37178700064808E-15,
713.978125));
#146343=CARTESIAN_POINT('Ctrl Pts',(50.5832961557877,-4.68723266073572,
712.484007352941));
#146344=CARTESIAN_POINT('Ctrl Pts',(50.1489600866593,-9.37446532147149,
710.989889705883));
#146345=CARTESIAN_POINT('Ctrl Pts',(48.8607426731792,-13.9020798956618,
709.495772058823));
#146346=CARTESIAN_POINT('Ctrl Pts',(47.5725252596992,-18.4296944698521,
708.001654411765));
#146347=CARTESIAN_POINT('Ctrl Pts',(45.4742952008371,-22.6435084734482,
706.507536764706));
#146348=CARTESIAN_POINT('Ctrl Pts',(43.3760651419751,-26.8573224770441,
705.013419117647));
#146349=CARTESIAN_POINT('Ctrl Pts',(40.5392751458362,-30.6138395280662,
703.519301470588));
#146350=CARTESIAN_POINT('Ctrl Pts',(37.7024851496972,-34.3703565790883,
702.025183823529));
#146351=CARTESIAN_POINT('Ctrl Pts',(34.2237386972451,-37.5416529948095,
700.531066176471));
#146352=CARTESIAN_POINT('Ctrl Pts',(30.744992244793,-40.7129494105307,699.036948529412));
#146353=CARTESIAN_POINT('Ctrl Pts',(26.7427538741697,-43.1910304950644,
697.542830882353));
#146354=CARTESIAN_POINT('Ctrl Pts',(22.7405155035463,-45.6691115795981,
696.048713235294));
#146355=CARTESIAN_POINT('Ctrl Pts',(18.3510766423074,-47.3695892537413,
694.554595588235));
#146356=CARTESIAN_POINT('Ctrl Pts',(13.9616377810684,-49.0700669278844,
693.060477941176));
#146357=CARTESIAN_POINT('Ctrl Pts',(9.33447550508176,-49.9350334639422,
691.566360294118));
#146358=CARTESIAN_POINT('Ctrl Pts',(4.70731322909511,-50.8,690.072242647059));
#146359=CARTESIAN_POINT('Ctrl Pts',(0.,-50.8,688.578125));
#146360=CARTESIAN_POINT('Ctrl Pts',(-4.70731322909511,-50.8,687.084007352941));
#146361=CARTESIAN_POINT('Ctrl Pts',(-9.33447550508177,-49.9350334639422,
685.589889705882));
#146362=CARTESIAN_POINT('Ctrl Pts',(-13.9616377810684,-49.0700669278844,
684.095772058824));
#146363=CARTESIAN_POINT('Ctrl Pts',(-18.3510766423074,-47.3695892537413,
682.601654411765));
#146364=CARTESIAN_POINT('Ctrl Pts',(-22.7405155035463,-45.6691115795981,
681.107536764706));
#146365=CARTESIAN_POINT('Ctrl Pts',(-26.7427538741697,-43.1910304950644,
679.613419117647));
#146366=CARTESIAN_POINT('Ctrl Pts',(-30.744992244793,-40.7129494105307,
678.119301470588));
#146367=CARTESIAN_POINT('Ctrl Pts',(-34.2237386972451,-37.5416529948095,
676.62518382353));
#146368=CARTESIAN_POINT('Ctrl Pts',(-37.7024851496972,-34.3703565790883,
675.131066176471));
#146369=CARTESIAN_POINT('Ctrl Pts',(-40.5392751458362,-30.6138395280662,
673.636948529412));
#146370=CARTESIAN_POINT('Ctrl Pts',(-43.3760651419751,-26.8573224770441,
672.142830882353));
#146371=CARTESIAN_POINT('Ctrl Pts',(-45.4742952008371,-22.6435084734481,
670.648713235294));
#146372=CARTESIAN_POINT('Ctrl Pts',(-47.5725252596992,-18.4296944698521,
669.154595588235));
#146373=CARTESIAN_POINT('Ctrl Pts',(-48.8607426731792,-13.9020798956618,
667.660477941176));
#146374=CARTESIAN_POINT('Ctrl Pts',(-50.1489600866593,-9.37446532147148,
666.166360294118));
#146375=CARTESIAN_POINT('Ctrl Pts',(-50.5832961557877,-4.68723266073574,
664.672242647059));
#146376=CARTESIAN_POINT('Ctrl Pts',(-51.0176322249162,-3.12392900021603E-15,
663.178125));
#146377=CARTESIAN_POINT('Ctrl Pts',(-50.5832961557877,4.68723266073573,
661.684007352941));
#146378=CARTESIAN_POINT('Ctrl Pts',(-50.1489600866593,9.37446532147149,
660.189889705882));
#146379=CARTESIAN_POINT('Ctrl Pts',(-48.8607426731792,13.9020798956618,
658.695772058824));
#146380=CARTESIAN_POINT('Ctrl Pts',(-47.5725252596992,18.4296944698521,
657.201654411765));
#146381=CARTESIAN_POINT('Ctrl Pts',(-45.4742952008371,22.6435084734481,
655.707536764706));
#146382=CARTESIAN_POINT('Ctrl Pts',(-43.3760651419751,26.8573224770442,
654.213419117647));
#146383=CARTESIAN_POINT('Ctrl Pts',(-40.5392751458362,30.6138395280662,
652.719301470588));
#146384=CARTESIAN_POINT('Ctrl Pts',(-37.7024851496972,34.3703565790883,
651.22518382353));
#146385=CARTESIAN_POINT('Ctrl Pts',(-34.2237386972451,37.5416529948095,
649.731066176471));
#146386=CARTESIAN_POINT('Ctrl Pts',(-30.744992244793,40.7129494105307,648.236948529412));
#146387=CARTESIAN_POINT('Ctrl Pts',(-26.7427538741697,43.1910304950644,
646.742830882353));
#146388=CARTESIAN_POINT('Ctrl Pts',(-22.7405155035463,45.6691115795981,
645.248713235294));
#146389=CARTESIAN_POINT('Ctrl Pts',(-18.3510766423074,47.3695892537413,
643.754595588235));
#146390=CARTESIAN_POINT('Ctrl Pts',(-13.9616377810684,49.0700669278844,
642.260477941177));
#146391=CARTESIAN_POINT('Ctrl Pts',(-9.33447550508177,49.9350334639422,
640.766360294118));
#146392=CARTESIAN_POINT('Ctrl Pts',(-4.7073132290951,50.8,639.272242647059));
#146393=CARTESIAN_POINT('Ctrl Pts',(-6.22120573966855E-15,50.8,637.778125));
#146394=CARTESIAN_POINT('Ctrl Pts',(4.70731322909511,50.8,636.284007352941));
#146395=CARTESIAN_POINT('Ctrl Pts',(9.33447550508176,49.9350334639422,634.789889705882));
#146396=CARTESIAN_POINT('Ctrl Pts',(13.9616377810684,49.0700669278844,633.295772058824));
#146397=CARTESIAN_POINT('Ctrl Pts',(18.3510766423074,47.3695892537413,631.801654411765));
#146398=CARTESIAN_POINT('Ctrl Pts',(22.7405155035463,45.6691115795981,630.307536764706));
#146399=CARTESIAN_POINT('Ctrl Pts',(26.7427538741697,43.1910304950644,628.813419117647));
#146400=CARTESIAN_POINT('Ctrl Pts',(30.744992244793,40.7129494105307,627.319301470588));
#146401=CARTESIAN_POINT('Ctrl Pts',(34.2237386972451,37.5416529948095,625.82518382353));
#146402=CARTESIAN_POINT('Ctrl Pts',(37.7024851496972,34.3703565790883,624.331066176471));
#146403=CARTESIAN_POINT('Ctrl Pts',(40.5392751458362,30.6138395280662,622.836948529412));
#146404=CARTESIAN_POINT('Ctrl Pts',(43.3760651419751,26.8573224770442,621.342830882353));
#146405=CARTESIAN_POINT('Ctrl Pts',(45.4742952008372,22.6435084734481,619.848713235294));
#146406=CARTESIAN_POINT('Ctrl Pts',(47.5725252596992,18.4296944698521,618.354595588235));
#146407=CARTESIAN_POINT('Ctrl Pts',(48.8607426731792,13.9020798956618,616.860477941176));
#146408=CARTESIAN_POINT('Ctrl Pts',(50.1489600866593,9.37446532147146,615.366360294118));
#146409=CARTESIAN_POINT('Ctrl Pts',(50.5832961557877,4.68723266073574,613.872242647059));
#146410=CARTESIAN_POINT('Ctrl Pts',(51.0176322249162,9.37178700064808E-15,
612.378125));
#146411=CARTESIAN_POINT('Ctrl Pts',(50.5832961557877,-4.68723266073572,
610.884007352941));
#146412=CARTESIAN_POINT('Ctrl Pts',(50.1489600866593,-9.37446532147149,
609.389889705882));
#146413=CARTESIAN_POINT('Ctrl Pts',(48.8607426731792,-13.9020798956618,
607.895772058823));
#146414=CARTESIAN_POINT('Ctrl Pts',(47.5725252596992,-18.4296944698521,
606.401654411765));
#146415=CARTESIAN_POINT('Ctrl Pts',(45.4742952008371,-22.6435084734482,
604.907536764706));
#146416=CARTESIAN_POINT('Ctrl Pts',(43.3760651419751,-26.8573224770441,
603.413419117647));
#146417=CARTESIAN_POINT('Ctrl Pts',(40.5392751458362,-30.6138395280662,
601.919301470588));
#146418=CARTESIAN_POINT('Ctrl Pts',(37.7024851496972,-34.3703565790883,
600.42518382353));
#146419=CARTESIAN_POINT('Ctrl Pts',(34.2237386972451,-37.5416529948095,
598.931066176471));
#146420=CARTESIAN_POINT('Ctrl Pts',(30.744992244793,-40.7129494105307,597.436948529412));
#146421=CARTESIAN_POINT('Ctrl Pts',(26.7427538741697,-43.1910304950644,
595.942830882353));
#146422=CARTESIAN_POINT('Ctrl Pts',(22.7405155035463,-45.6691115795981,
594.448713235294));
#146423=CARTESIAN_POINT('Ctrl Pts',(18.3510766423074,-47.3695892537413,
592.954595588235));
#146424=CARTESIAN_POINT('Ctrl Pts',(13.9616377810684,-49.0700669278844,
591.460477941176));
#146425=CARTESIAN_POINT('Ctrl Pts',(9.33447550508176,-49.9350334639422,
589.966360294118));
#146426=CARTESIAN_POINT('Ctrl Pts',(4.70731322909511,-50.8,588.472242647059));
#146427=CARTESIAN_POINT('Ctrl Pts',(0.,-50.8,586.978125));
#146428=CARTESIAN_POINT('Ctrl Pts',(-4.70731322909511,-50.8,585.484007352941));
#146429=CARTESIAN_POINT('Ctrl Pts',(-9.33447550508177,-49.9350334639422,
583.989889705882));
#146430=CARTESIAN_POINT('Ctrl Pts',(-13.9616377810684,-49.0700669278844,
582.495772058823));
#146431=CARTESIAN_POINT('Ctrl Pts',(-18.3510766423074,-47.3695892537413,
581.001654411765));
#146432=CARTESIAN_POINT('Ctrl Pts',(-22.7405155035463,-45.6691115795981,
579.507536764706));
#146433=CARTESIAN_POINT('Ctrl Pts',(-26.7427538741697,-43.1910304950644,
578.013419117647));
#146434=CARTESIAN_POINT('Ctrl Pts',(-30.744992244793,-40.7129494105307,
576.519301470588));
#146435=CARTESIAN_POINT('Ctrl Pts',(-34.2237386972451,-37.5416529948095,
575.025183823529));
#146436=CARTESIAN_POINT('Ctrl Pts',(-37.7024851496972,-34.3703565790883,
573.531066176471));
#146437=CARTESIAN_POINT('Ctrl Pts',(-40.5392751458362,-30.6138395280662,
572.036948529412));
#146438=CARTESIAN_POINT('Ctrl Pts',(-43.3760651419751,-26.8573224770441,
570.542830882353));
#146439=CARTESIAN_POINT('Ctrl Pts',(-45.4742952008371,-22.6435084734481,
569.048713235294));
#146440=CARTESIAN_POINT('Ctrl Pts',(-47.5725252596992,-18.4296944698521,
567.554595588235));
#146441=CARTESIAN_POINT('Ctrl Pts',(-48.8607426731792,-13.9020798956618,
566.060477941176));
#146442=CARTESIAN_POINT('Ctrl Pts',(-50.1489600866593,-9.37446532147148,
564.566360294118));
#146443=CARTESIAN_POINT('Ctrl Pts',(-50.5832961557877,-4.68723266073574,
563.072242647059));
#146444=CARTESIAN_POINT('Ctrl Pts',(-51.0176322249162,-3.12392900021603E-15,
561.578125));
#146445=CARTESIAN_POINT('Ctrl Pts',(-50.5832961557877,4.68723266073573,
560.084007352941));
#146446=CARTESIAN_POINT('Ctrl Pts',(-50.1489600866593,9.37446532147149,
558.589889705882));
#146447=CARTESIAN_POINT('Ctrl Pts',(-48.8607426731792,13.9020798956618,
557.095772058824));
#146448=CARTESIAN_POINT('Ctrl Pts',(-47.5725252596992,18.4296944698521,
555.601654411765));
#146449=CARTESIAN_POINT('Ctrl Pts',(-45.4742952008371,22.6435084734481,
554.107536764706));
#146450=CARTESIAN_POINT('Ctrl Pts',(-43.3760651419751,26.8573224770442,
552.613419117647));
#146451=CARTESIAN_POINT('Ctrl Pts',(-40.5392751458362,30.6138395280662,
551.119301470588));
#146452=CARTESIAN_POINT('Ctrl Pts',(-37.7024851496972,34.3703565790883,
549.62518382353));
#146453=CARTESIAN_POINT('Ctrl Pts',(-34.2237386972451,37.5416529948095,
548.131066176471));
#146454=CARTESIAN_POINT('Ctrl Pts',(-30.744992244793,40.7129494105307,546.636948529412));
#146455=CARTESIAN_POINT('Ctrl Pts',(-26.7427538741697,43.1910304950644,
545.142830882353));
#146456=CARTESIAN_POINT('Ctrl Pts',(-22.7405155035463,45.6691115795981,
543.648713235294));
#146457=CARTESIAN_POINT('Ctrl Pts',(-18.3510766423074,47.3695892537413,
542.154595588235));
#146458=CARTESIAN_POINT('Ctrl Pts',(-13.9616377810684,49.0700669278844,
540.660477941176));
#146459=CARTESIAN_POINT('Ctrl Pts',(-9.33447550508177,49.9350334639422,
539.166360294118));
#146460=CARTESIAN_POINT('Ctrl Pts',(-4.7073132290951,50.8,537.672242647059));
#146461=CARTESIAN_POINT('Ctrl Pts',(-6.22120573966855E-15,50.8,536.178125));
#146462=CARTESIAN_POINT('Ctrl Pts',(4.70731322909511,50.8,534.684007352941));
#146463=CARTESIAN_POINT('Ctrl Pts',(9.33447550508176,49.9350334639422,533.189889705882));
#146464=CARTESIAN_POINT('Ctrl Pts',(13.9616377810684,49.0700669278844,531.695772058824));
#146465=CARTESIAN_POINT('Ctrl Pts',(18.3510766423074,47.3695892537413,530.201654411765));
#146466=CARTESIAN_POINT('Ctrl Pts',(22.7405155035463,45.6691115795981,528.707536764706));
#146467=CARTESIAN_POINT('Ctrl Pts',(26.7427538741697,43.1910304950644,527.213419117647));
#146468=CARTESIAN_POINT('Ctrl Pts',(30.744992244793,40.7129494105307,525.719301470588));
#146469=CARTESIAN_POINT('Ctrl Pts',(34.2237386972451,37.5416529948095,524.22518382353));
#146470=CARTESIAN_POINT('Ctrl Pts',(37.7024851496972,34.3703565790883,522.731066176471));
#146471=CARTESIAN_POINT('Ctrl Pts',(40.5392751458362,30.6138395280662,521.236948529412));
#146472=CARTESIAN_POINT('Ctrl Pts',(43.3760651419751,26.8573224770442,519.742830882353));
#146473=CARTESIAN_POINT('Ctrl Pts',(45.4742952008372,22.6435084734481,518.248713235294));
#146474=CARTESIAN_POINT('Ctrl Pts',(47.5725252596992,18.4296944698521,516.754595588235));
#146475=CARTESIAN_POINT('Ctrl Pts',(48.8607426731792,13.9020798956618,515.260477941176));
#146476=CARTESIAN_POINT('Ctrl Pts',(50.1489600866593,9.37446532147146,513.766360294118));
#146477=CARTESIAN_POINT('Ctrl Pts',(50.5832961557877,4.68723266073574,512.272242647059));
#146478=CARTESIAN_POINT('Ctrl Pts',(51.0176322249162,9.37178700064808E-15,
510.778125));
#146479=CARTESIAN_POINT('Ctrl Pts',(50.5832961557877,-4.68723266073572,
509.284007352941));
#146480=CARTESIAN_POINT('Ctrl Pts',(50.1489600866593,-9.37446532147149,
507.789889705882));
#146481=CARTESIAN_POINT('Ctrl Pts',(48.8607426731792,-13.9020798956618,
506.295772058824));
#146482=CARTESIAN_POINT('Ctrl Pts',(47.5725252596992,-18.4296944698521,
504.801654411765));
#146483=CARTESIAN_POINT('Ctrl Pts',(45.4742952008371,-22.6435084734482,
503.307536764706));
#146484=CARTESIAN_POINT('Ctrl Pts',(43.3760651419751,-26.8573224770441,
501.813419117647));
#146485=CARTESIAN_POINT('Ctrl Pts',(40.5392751458362,-30.6138395280662,
500.319301470588));
#146486=CARTESIAN_POINT('Ctrl Pts',(37.7024851496972,-34.3703565790883,
498.825183823529));
#146487=CARTESIAN_POINT('Ctrl Pts',(34.2237386972451,-37.5416529948095,
497.331066176471));
#146488=CARTESIAN_POINT('Ctrl Pts',(30.744992244793,-40.7129494105307,495.836948529412));
#146489=CARTESIAN_POINT('Ctrl Pts',(26.7427538741697,-43.1910304950644,
494.342830882353));
#146490=CARTESIAN_POINT('Ctrl Pts',(22.7405155035463,-45.6691115795981,
492.848713235294));
#146491=CARTESIAN_POINT('Ctrl Pts',(18.3510766423074,-47.3695892537413,
491.354595588235));
#146492=CARTESIAN_POINT('Ctrl Pts',(13.9616377810684,-49.0700669278844,
489.860477941177));
#146493=CARTESIAN_POINT('Ctrl Pts',(9.33447550508176,-49.9350334639422,
488.366360294118));
#146494=CARTESIAN_POINT('Ctrl Pts',(4.70731322909511,-50.8,486.872242647059));
#146495=CARTESIAN_POINT('Ctrl Pts',(0.,-50.8,485.378125));
#146496=CARTESIAN_POINT('Ctrl Pts',(-4.70731322909511,-50.8,483.884007352941));
#146497=CARTESIAN_POINT('Ctrl Pts',(-9.33447550508177,-49.9350334639422,
482.389889705883));
#146498=CARTESIAN_POINT('Ctrl Pts',(-13.9616377810684,-49.0700669278844,
480.895772058824));
#146499=CARTESIAN_POINT('Ctrl Pts',(-18.3510766423074,-47.3695892537413,
479.401654411765));
#146500=CARTESIAN_POINT('Ctrl Pts',(-22.7405155035463,-45.6691115795981,
477.907536764706));
#146501=CARTESIAN_POINT('Ctrl Pts',(-26.7427538741697,-43.1910304950644,
476.413419117647));
#146502=CARTESIAN_POINT('Ctrl Pts',(-30.744992244793,-40.7129494105307,
474.919301470588));
#146503=CARTESIAN_POINT('Ctrl Pts',(-34.2237386972451,-37.5416529948095,
473.425183823529));
#146504=CARTESIAN_POINT('Ctrl Pts',(-37.7024851496972,-34.3703565790883,
471.931066176471));
#146505=CARTESIAN_POINT('Ctrl Pts',(-40.5392751458362,-30.6138395280662,
470.436948529412));
#146506=CARTESIAN_POINT('Ctrl Pts',(-43.3760651419751,-26.8573224770441,
468.942830882353));
#146507=CARTESIAN_POINT('Ctrl Pts',(-45.4742952008371,-22.6435084734481,
467.448713235294));
#146508=CARTESIAN_POINT('Ctrl Pts',(-47.5725252596992,-18.4296944698521,
465.954595588235));
#146509=CARTESIAN_POINT('Ctrl Pts',(-48.8607426731792,-13.9020798956618,
464.460477941177));
#146510=CARTESIAN_POINT('Ctrl Pts',(-50.1489600866593,-9.37446532147148,
462.966360294118));
#146511=CARTESIAN_POINT('Ctrl Pts',(-50.5832961557877,-4.68723266073574,
461.472242647059));
#146512=CARTESIAN_POINT('Ctrl Pts',(-51.0176322249162,-3.12392900021603E-15,
459.978125));
#146513=CARTESIAN_POINT('Ctrl Pts',(-50.5832961557877,4.68723266073573,
458.484007352941));
#146514=CARTESIAN_POINT('Ctrl Pts',(-50.1489600866593,9.37446532147149,
456.989889705882));
#146515=CARTESIAN_POINT('Ctrl Pts',(-48.8607426731792,13.9020798956618,
455.495772058824));
#146516=CARTESIAN_POINT('Ctrl Pts',(-47.5725252596992,18.4296944698521,
454.001654411765));
#146517=CARTESIAN_POINT('Ctrl Pts',(-45.4742952008371,22.6435084734481,
452.507536764706));
#146518=CARTESIAN_POINT('Ctrl Pts',(-43.3760651419751,26.8573224770442,
451.013419117647));
#146519=CARTESIAN_POINT('Ctrl Pts',(-40.5392751458362,30.6138395280662,
449.519301470588));
#146520=CARTESIAN_POINT('Ctrl Pts',(-37.7024851496972,34.3703565790883,
448.02518382353));
#146521=CARTESIAN_POINT('Ctrl Pts',(-34.2237386972451,37.5416529948095,
446.531066176471));
#146522=CARTESIAN_POINT('Ctrl Pts',(-30.744992244793,40.7129494105307,445.036948529412));
#146523=CARTESIAN_POINT('Ctrl Pts',(-26.7427538741697,43.1910304950644,
443.542830882353));
#146524=CARTESIAN_POINT('Ctrl Pts',(-22.7405155035463,45.6691115795981,
442.048713235294));
#146525=CARTESIAN_POINT('Ctrl Pts',(-18.3510766423074,47.3695892537413,
440.554595588235));
#146526=CARTESIAN_POINT('Ctrl Pts',(-13.9616377810684,49.0700669278844,
439.060477941176));
#146527=CARTESIAN_POINT('Ctrl Pts',(-9.33447550508177,49.9350334639422,
437.566360294118));
#146528=CARTESIAN_POINT('Ctrl Pts',(-4.7073132290951,50.8,436.072242647059));
#146529=CARTESIAN_POINT('Ctrl Pts',(-6.22120573966855E-15,50.8,434.578125));
#146530=CARTESIAN_POINT('Ctrl Pts',(4.70731322909511,50.8,433.084007352941));
#146531=CARTESIAN_POINT('Ctrl Pts',(9.33447550508176,49.9350334639422,431.589889705882));
#146532=CARTESIAN_POINT('Ctrl Pts',(13.9616377810684,49.0700669278844,430.095772058824));
#146533=CARTESIAN_POINT('Ctrl Pts',(18.3510766423074,47.3695892537413,428.601654411765));
#146534=CARTESIAN_POINT('Ctrl Pts',(22.7405155035463,45.6691115795981,427.107536764706));
#146535=CARTESIAN_POINT('Ctrl Pts',(26.7427538741697,43.1910304950644,425.613419117647));
#146536=CARTESIAN_POINT('Ctrl Pts',(30.744992244793,40.7129494105307,424.119301470588));
#146537=CARTESIAN_POINT('Ctrl Pts',(34.2237386972451,37.5416529948095,422.62518382353));
#146538=CARTESIAN_POINT('Ctrl Pts',(37.7024851496972,34.3703565790883,421.131066176471));
#146539=CARTESIAN_POINT('Ctrl Pts',(40.5392751458362,30.6138395280662,419.636948529412));
#146540=CARTESIAN_POINT('Ctrl Pts',(43.3760651419751,26.8573224770442,418.142830882353));
#146541=CARTESIAN_POINT('Ctrl Pts',(45.4742952008372,22.6435084734481,416.648713235294));
#146542=CARTESIAN_POINT('Ctrl Pts',(47.5725252596992,18.4296944698521,415.154595588236));
#146543=CARTESIAN_POINT('Ctrl Pts',(48.8607426731792,13.9020798956618,413.660477941177));
#146544=CARTESIAN_POINT('Ctrl Pts',(50.1489600866593,9.37446532147146,412.166360294118));
#146545=CARTESIAN_POINT('Ctrl Pts',(50.5832961557877,4.68723266073574,410.672242647059));
#146546=CARTESIAN_POINT('Ctrl Pts',(51.0176322249162,9.37178700064808E-15,
409.178125));
#146547=CARTESIAN_POINT('Ctrl Pts',(50.5832961557877,-4.68723266073572,
407.684007352941));
#146548=CARTESIAN_POINT('Ctrl Pts',(50.1489600866593,-9.37446532147149,
406.189889705882));
#146549=CARTESIAN_POINT('Ctrl Pts',(48.8607426731792,-13.9020798956618,
404.695772058824));
#146550=CARTESIAN_POINT('Ctrl Pts',(47.5725252596992,-18.4296944698521,
403.201654411765));
#146551=CARTESIAN_POINT('Ctrl Pts',(45.4742952008371,-22.6435084734482,
401.707536764706));
#146552=CARTESIAN_POINT('Ctrl Pts',(43.3760651419751,-26.8573224770441,
400.213419117647));
#146553=CARTESIAN_POINT('Ctrl Pts',(40.5392751458362,-30.6138395280662,
398.719301470588));
#146554=CARTESIAN_POINT('Ctrl Pts',(37.7024851496972,-34.3703565790883,
397.22518382353));
#146555=CARTESIAN_POINT('Ctrl Pts',(34.2237386972451,-37.5416529948095,
395.731066176471));
#146556=CARTESIAN_POINT('Ctrl Pts',(30.744992244793,-40.7129494105307,394.236948529412));
#146557=CARTESIAN_POINT('Ctrl Pts',(26.7427538741697,-43.1910304950644,
392.742830882353));
#146558=CARTESIAN_POINT('Ctrl Pts',(22.7405155035463,-45.6691115795981,
391.248713235294));
#146559=CARTESIAN_POINT('Ctrl Pts',(18.3510766423074,-47.3695892537413,
389.754595588235));
#146560=CARTESIAN_POINT('Ctrl Pts',(13.9616377810684,-49.0700669278844,
388.260477941176));
#146561=CARTESIAN_POINT('Ctrl Pts',(9.33447550508176,-49.9350334639422,
386.766360294118));
#146562=CARTESIAN_POINT('Ctrl Pts',(4.70731322909511,-50.8,385.272242647059));
#146563=CARTESIAN_POINT('Ctrl Pts',(0.,-50.8,383.778125));
#146564=CARTESIAN_POINT('Ctrl Pts',(-4.70731322909511,-50.8,382.284007352941));
#146565=CARTESIAN_POINT('Ctrl Pts',(-9.33447550508177,-49.9350334639422,
380.789889705882));
#146566=CARTESIAN_POINT('Ctrl Pts',(-13.9616377810684,-49.0700669278844,
379.295772058823));
#146567=CARTESIAN_POINT('Ctrl Pts',(-18.3510766423074,-47.3695892537413,
377.801654411765));
#146568=CARTESIAN_POINT('Ctrl Pts',(-22.7405155035463,-45.6691115795981,
376.307536764706));
#146569=CARTESIAN_POINT('Ctrl Pts',(-26.7427538741697,-43.1910304950644,
374.813419117647));
#146570=CARTESIAN_POINT('Ctrl Pts',(-30.744992244793,-40.7129494105307,
373.319301470588));
#146571=CARTESIAN_POINT('Ctrl Pts',(-34.2237386972451,-37.5416529948095,
371.825183823529));
#146572=CARTESIAN_POINT('Ctrl Pts',(-37.7024851496972,-34.3703565790883,
370.331066176471));
#146573=CARTESIAN_POINT('Ctrl Pts',(-40.5392751458362,-30.6138395280662,
368.836948529412));
#146574=CARTESIAN_POINT('Ctrl Pts',(-43.3760651419751,-26.8573224770441,
367.342830882353));
#146575=CARTESIAN_POINT('Ctrl Pts',(-45.4742952008371,-22.6435084734481,
365.848713235294));
#146576=CARTESIAN_POINT('Ctrl Pts',(-47.5725252596992,-18.4296944698521,
364.354595588235));
#146577=CARTESIAN_POINT('Ctrl Pts',(-48.8607426731792,-13.9020798956618,
362.860477941177));
#146578=CARTESIAN_POINT('Ctrl Pts',(-50.1489600866593,-9.37446532147148,
361.366360294118));
#146579=CARTESIAN_POINT('Ctrl Pts',(-50.5832961557877,-4.68723266073574,
359.872242647059));
#146580=CARTESIAN_POINT('Ctrl Pts',(-51.0176322249162,-3.12392900021603E-15,
358.378125));
#146581=CARTESIAN_POINT('Ctrl Pts',(-50.5832961557877,4.68723266073573,
356.884007352941));
#146582=CARTESIAN_POINT('Ctrl Pts',(-50.1489600866593,9.37446532147149,
355.389889705882));
#146583=CARTESIAN_POINT('Ctrl Pts',(-48.8607426731792,13.9020798956618,
353.895772058824));
#146584=CARTESIAN_POINT('Ctrl Pts',(-47.5725252596992,18.4296944698521,
352.401654411765));
#146585=CARTESIAN_POINT('Ctrl Pts',(-45.4742952008371,22.6435084734481,
350.907536764706));
#146586=CARTESIAN_POINT('Ctrl Pts',(-43.3760651419751,26.8573224770442,
349.413419117647));
#146587=CARTESIAN_POINT('Ctrl Pts',(-40.5392751458362,30.6138395280662,
347.919301470588));
#146588=CARTESIAN_POINT('Ctrl Pts',(-37.7024851496972,34.3703565790883,
346.42518382353));
#146589=CARTESIAN_POINT('Ctrl Pts',(-34.2237386972451,37.5416529948095,
344.931066176471));
#146590=CARTESIAN_POINT('Ctrl Pts',(-30.744992244793,40.7129494105307,343.436948529412));
#146591=CARTESIAN_POINT('Ctrl Pts',(-26.7427538741697,43.1910304950644,
341.942830882353));
#146592=CARTESIAN_POINT('Ctrl Pts',(-22.7405155035463,45.6691115795981,
340.448713235294));
#146593=CARTESIAN_POINT('Ctrl Pts',(-18.3510766423074,47.3695892537413,
338.954595588235));
#146594=CARTESIAN_POINT('Ctrl Pts',(-13.9616377810684,49.0700669278844,
337.460477941177));
#146595=CARTESIAN_POINT('Ctrl Pts',(-9.33447550508177,49.9350334639422,
335.966360294118));
#146596=CARTESIAN_POINT('Ctrl Pts',(-4.7073132290951,50.8,334.472242647059));
#146597=CARTESIAN_POINT('Ctrl Pts',(-6.22120573966855E-15,50.8,332.978125));
#146598=CARTESIAN_POINT('Ctrl Pts',(4.70731322909511,50.8,331.484007352941));
#146599=CARTESIAN_POINT('Ctrl Pts',(9.33447550508176,49.9350334639422,329.989889705882));
#146600=CARTESIAN_POINT('Ctrl Pts',(13.9616377810684,49.0700669278844,328.495772058823));
#146601=CARTESIAN_POINT('Ctrl Pts',(18.3510766423074,47.3695892537413,327.001654411765));
#146602=CARTESIAN_POINT('Ctrl Pts',(22.7405155035463,45.6691115795981,325.507536764706));
#146603=CARTESIAN_POINT('Ctrl Pts',(26.7427538741697,43.1910304950644,324.013419117647));
#146604=CARTESIAN_POINT('Ctrl Pts',(30.744992244793,40.7129494105307,322.519301470588));
#146605=CARTESIAN_POINT('Ctrl Pts',(34.2237386972451,37.5416529948095,321.025183823529));
#146606=CARTESIAN_POINT('Ctrl Pts',(37.7024851496972,34.3703565790883,319.531066176471));
#146607=CARTESIAN_POINT('Ctrl Pts',(40.5392751458362,30.6138395280662,318.036948529412));
#146608=CARTESIAN_POINT('Ctrl Pts',(43.3760651419751,26.8573224770442,316.542830882353));
#146609=CARTESIAN_POINT('Ctrl Pts',(45.4742952008372,22.6435084734481,315.048713235294));
#146610=CARTESIAN_POINT('Ctrl Pts',(47.5725252596992,18.4296944698521,313.554595588235));
#146611=CARTESIAN_POINT('Ctrl Pts',(48.8607426731792,13.9020798956618,312.060477941176));
#146612=CARTESIAN_POINT('Ctrl Pts',(50.1489600866593,9.37446532147146,310.566360294118));
#146613=CARTESIAN_POINT('Ctrl Pts',(50.5832961557877,4.68723266073574,309.072242647059));
#146614=CARTESIAN_POINT('Ctrl Pts',(51.0176322249162,9.37178700064808E-15,
307.578125));
#146615=CARTESIAN_POINT('Ctrl Pts',(50.5832961557877,-4.68723266073572,
306.084007352941));
#146616=CARTESIAN_POINT('Ctrl Pts',(50.1489600866593,-9.37446532147149,
304.589889705882));
#146617=CARTESIAN_POINT('Ctrl Pts',(48.8607426731792,-13.9020798956618,
303.095772058824));
#146618=CARTESIAN_POINT('Ctrl Pts',(47.5725252596992,-18.4296944698521,
301.601654411765));
#146619=CARTESIAN_POINT('Ctrl Pts',(45.4742952008371,-22.6435084734482,
300.107536764706));
#146620=CARTESIAN_POINT('Ctrl Pts',(43.3760651419751,-26.8573224770441,
298.613419117647));
#146621=CARTESIAN_POINT('Ctrl Pts',(40.5392751458362,-30.6138395280662,
297.119301470588));
#146622=CARTESIAN_POINT('Ctrl Pts',(37.7024851496972,-34.3703565790883,
295.625183823529));
#146623=CARTESIAN_POINT('Ctrl Pts',(34.2237386972451,-37.5416529948095,
294.131066176471));
#146624=CARTESIAN_POINT('Ctrl Pts',(30.744992244793,-40.7129494105307,292.636948529412));
#146625=CARTESIAN_POINT('Ctrl Pts',(26.7427538741697,-43.1910304950644,
291.142830882353));
#146626=CARTESIAN_POINT('Ctrl Pts',(22.7405155035463,-45.6691115795981,
289.648713235294));
#146627=CARTESIAN_POINT('Ctrl Pts',(18.3510766423074,-47.3695892537413,
288.154595588235));
#146628=CARTESIAN_POINT('Ctrl Pts',(13.9616377810684,-49.0700669278844,
286.660477941177));
#146629=CARTESIAN_POINT('Ctrl Pts',(9.33447550508176,-49.9350334639422,
285.166360294118));
#146630=CARTESIAN_POINT('Ctrl Pts',(4.70731322909511,-50.8,283.672242647059));
#146631=CARTESIAN_POINT('Ctrl Pts',(0.,-50.8,282.178125));
#146632=CARTESIAN_POINT('Ctrl Pts',(-4.70731322909511,-50.8,280.684007352941));
#146633=CARTESIAN_POINT('Ctrl Pts',(-9.33447550508177,-49.9350334639422,
279.189889705882));
#146634=CARTESIAN_POINT('Ctrl Pts',(-13.9616377810684,-49.0700669278844,
277.695772058824));
#146635=CARTESIAN_POINT('Ctrl Pts',(-18.3510766423074,-47.3695892537413,
276.201654411765));
#146636=CARTESIAN_POINT('Ctrl Pts',(-22.7405155035463,-45.6691115795981,
274.707536764706));
#146637=CARTESIAN_POINT('Ctrl Pts',(-26.7427538741697,-43.1910304950644,
273.213419117647));
#146638=CARTESIAN_POINT('Ctrl Pts',(-30.744992244793,-40.7129494105307,
271.719301470588));
#146639=CARTESIAN_POINT('Ctrl Pts',(-34.2237386972451,-37.5416529948095,
270.225183823529));
#146640=CARTESIAN_POINT('Ctrl Pts',(-37.7024851496972,-34.3703565790883,
268.731066176471));
#146641=CARTESIAN_POINT('Ctrl Pts',(-40.5392751458362,-30.6138395280662,
267.236948529412));
#146642=CARTESIAN_POINT('Ctrl Pts',(-43.3760651419751,-26.8573224770441,
265.742830882353));
#146643=CARTESIAN_POINT('Ctrl Pts',(-45.4742952008371,-22.6435084734481,
264.248713235294));
#146644=CARTESIAN_POINT('Ctrl Pts',(-47.5725252596992,-18.4296944698521,
262.754595588235));
#146645=CARTESIAN_POINT('Ctrl Pts',(-48.8607426731792,-13.9020798956618,
261.260477941176));
#146646=CARTESIAN_POINT('Ctrl Pts',(-50.1489600866593,-9.37446532147148,
259.766360294118));
#146647=CARTESIAN_POINT('Ctrl Pts',(-50.5832961557877,-4.68723266073574,
258.272242647059));
#146648=CARTESIAN_POINT('Ctrl Pts',(-51.0176322249162,-3.12392900021603E-15,
256.778125));
#146649=CARTESIAN_POINT('Ctrl Pts',(-50.5832961557877,4.68723266073573,
255.284007352941));
#146650=CARTESIAN_POINT('Ctrl Pts',(-50.1489600866593,9.37446532147149,
253.789889705882));
#146651=CARTESIAN_POINT('Ctrl Pts',(-48.8607426731792,13.9020798956618,
252.295772058824));
#146652=CARTESIAN_POINT('Ctrl Pts',(-47.5725252596992,18.4296944698521,
250.801654411765));
#146653=CARTESIAN_POINT('Ctrl Pts',(-45.4742952008371,22.6435084734481,
249.307536764706));
#146654=CARTESIAN_POINT('Ctrl Pts',(-43.3760651419751,26.8573224770442,
247.813419117647));
#146655=CARTESIAN_POINT('Ctrl Pts',(-40.5392751458362,30.6138395280662,
246.319301470588));
#146656=CARTESIAN_POINT('Ctrl Pts',(-37.7024851496972,34.3703565790883,
244.825183823529));
#146657=CARTESIAN_POINT('Ctrl Pts',(-34.2237386972451,37.5416529948095,
243.331066176471));
#146658=CARTESIAN_POINT('Ctrl Pts',(-30.744992244793,40.7129494105307,241.836948529412));
#146659=CARTESIAN_POINT('Ctrl Pts',(-26.7427538741697,43.1910304950644,
240.342830882353));
#146660=CARTESIAN_POINT('Ctrl Pts',(-22.7405155035463,45.6691115795981,
238.848713235294));
#146661=CARTESIAN_POINT('Ctrl Pts',(-18.3510766423074,47.3695892537413,
237.354595588235));
#146662=CARTESIAN_POINT('Ctrl Pts',(-13.9616377810684,49.0700669278844,
235.860477941177));
#146663=CARTESIAN_POINT('Ctrl Pts',(-9.33447550508177,49.9350334639422,
234.366360294118));
#146664=CARTESIAN_POINT('Ctrl Pts',(-4.7073132290951,50.8,232.872242647059));
#146665=CARTESIAN_POINT('Ctrl Pts',(-6.22120573966855E-15,50.8,231.378125));
#146666=CARTESIAN_POINT('Ctrl Pts',(4.70731322909511,50.8,229.884007352941));
#146667=CARTESIAN_POINT('Ctrl Pts',(9.33447550508176,49.9350334639422,228.389889705882));
#146668=CARTESIAN_POINT('Ctrl Pts',(13.9616377810684,49.0700669278844,226.895772058824));
#146669=CARTESIAN_POINT('Ctrl Pts',(18.3510766423074,47.3695892537413,225.401654411765));
#146670=CARTESIAN_POINT('Ctrl Pts',(22.7405155035463,45.6691115795981,223.907536764706));
#146671=CARTESIAN_POINT('Ctrl Pts',(26.7427538741697,43.1910304950644,222.413419117647));
#146672=CARTESIAN_POINT('Ctrl Pts',(30.744992244793,40.7129494105307,220.919301470588));
#146673=CARTESIAN_POINT('Ctrl Pts',(34.2237386972451,37.5416529948095,219.425183823529));
#146674=CARTESIAN_POINT('Ctrl Pts',(37.7024851496972,34.3703565790883,217.931066176471));
#146675=CARTESIAN_POINT('Ctrl Pts',(40.5392751458362,30.6138395280662,216.436948529412));
#146676=CARTESIAN_POINT('Ctrl Pts',(43.3760651419751,26.8573224770442,214.942830882353));
#146677=CARTESIAN_POINT('Ctrl Pts',(45.4742952008372,22.6435084734481,213.448713235294));
#146678=CARTESIAN_POINT('Ctrl Pts',(47.5725252596992,18.4296944698521,211.954595588235));
#146679=CARTESIAN_POINT('Ctrl Pts',(48.8607426731792,13.9020798956618,210.460477941177));
#146680=CARTESIAN_POINT('Ctrl Pts',(50.1489600866593,9.37446532147146,208.966360294118));
#146681=CARTESIAN_POINT('Ctrl Pts',(50.5832961557877,4.68723266073574,207.472242647059));
#146682=CARTESIAN_POINT('Ctrl Pts',(51.0176322249162,9.37178700064808E-15,
205.978125));
#146683=CARTESIAN_POINT('Ctrl Pts',(50.5832961557877,-4.68723266073572,
204.484007352941));
#146684=CARTESIAN_POINT('Ctrl Pts',(50.1489600866593,-9.37446532147149,
202.989889705882));
#146685=CARTESIAN_POINT('Ctrl Pts',(48.8607426731792,-13.9020798956618,
201.495772058824));
#146686=CARTESIAN_POINT('Ctrl Pts',(47.5725252596992,-18.4296944698521,
200.001654411765));
#146687=CARTESIAN_POINT('Ctrl Pts',(45.4742952008371,-22.6435084734482,
198.507536764706));
#146688=CARTESIAN_POINT('Ctrl Pts',(43.3760651419751,-26.8573224770441,
197.013419117647));
#146689=CARTESIAN_POINT('Ctrl Pts',(40.5392751458362,-30.6138395280662,
195.519301470588));
#146690=CARTESIAN_POINT('Ctrl Pts',(37.7024851496972,-34.3703565790883,
194.025183823529));
#146691=CARTESIAN_POINT('Ctrl Pts',(34.2237386972451,-37.5416529948095,
192.531066176471));
#146692=CARTESIAN_POINT('Ctrl Pts',(30.744992244793,-40.7129494105307,191.036948529412));
#146693=CARTESIAN_POINT('Ctrl Pts',(26.7427538741697,-43.1910304950644,
189.542830882353));
#146694=CARTESIAN_POINT('Ctrl Pts',(22.7405155035463,-45.6691115795981,
188.048713235294));
#146695=CARTESIAN_POINT('Ctrl Pts',(18.3510766423074,-47.3695892537413,
186.554595588235));
#146696=CARTESIAN_POINT('Ctrl Pts',(13.9616377810684,-49.0700669278844,
185.060477941176));
#146697=CARTESIAN_POINT('Ctrl Pts',(9.33447550508176,-49.9350334639422,
183.566360294118));
#146698=CARTESIAN_POINT('Ctrl Pts',(4.70731322909511,-50.8,182.072242647059));
#146699=CARTESIAN_POINT('Ctrl Pts',(0.,-50.8,180.578125));
#146700=CARTESIAN_POINT('Ctrl Pts',(-4.70731322909511,-50.8,179.084007352941));
#146701=CARTESIAN_POINT('Ctrl Pts',(-9.33447550508177,-49.9350334639422,
177.589889705882));
#146702=CARTESIAN_POINT('Ctrl Pts',(-13.9616377810684,-49.0700669278844,
176.095772058824));
#146703=CARTESIAN_POINT('Ctrl Pts',(-18.3510766423074,-47.3695892537413,
174.601654411765));
#146704=CARTESIAN_POINT('Ctrl Pts',(-22.7405155035463,-45.6691115795981,
173.107536764706));
#146705=CARTESIAN_POINT('Ctrl Pts',(-26.7427538741697,-43.1910304950644,
171.613419117647));
#146706=CARTESIAN_POINT('Ctrl Pts',(-30.744992244793,-40.7129494105307,
170.119301470588));
#146707=CARTESIAN_POINT('Ctrl Pts',(-34.2237386972451,-37.5416529948095,
168.62518382353));
#146708=CARTESIAN_POINT('Ctrl Pts',(-37.7024851496972,-34.3703565790883,
167.131066176471));
#146709=CARTESIAN_POINT('Ctrl Pts',(-40.5392751458362,-30.6138395280662,
165.636948529412));
#146710=CARTESIAN_POINT('Ctrl Pts',(-43.3760651419751,-26.8573224770441,
164.142830882353));
#146711=CARTESIAN_POINT('Ctrl Pts',(-45.4742952008371,-22.6435084734481,
162.648713235294));
#146712=CARTESIAN_POINT('Ctrl Pts',(-47.5725252596992,-18.4296944698521,
161.154595588235));
#146713=CARTESIAN_POINT('Ctrl Pts',(-48.8607426731792,-13.9020798956618,
159.660477941177));
#146714=CARTESIAN_POINT('Ctrl Pts',(-50.1489600866593,-9.37446532147148,
158.166360294118));
#146715=CARTESIAN_POINT('Ctrl Pts',(-50.5832961557877,-4.68723266073574,
156.672242647059));
#146716=CARTESIAN_POINT('Ctrl Pts',(-51.0176322249162,-3.12392900021603E-15,
155.178125));
#146717=CARTESIAN_POINT('Ctrl Pts',(-50.5832961557877,4.68723266073573,
153.684007352941));
#146718=CARTESIAN_POINT('Ctrl Pts',(-50.1489600866593,9.37446532147149,
152.189889705882));
#146719=CARTESIAN_POINT('Ctrl Pts',(-48.8607426731792,13.9020798956618,
150.695772058824));
#146720=CARTESIAN_POINT('Ctrl Pts',(-47.5725252596992,18.4296944698521,
149.201654411765));
#146721=CARTESIAN_POINT('Ctrl Pts',(-45.4742952008371,22.6435084734481,
147.707536764706));
#146722=CARTESIAN_POINT('Ctrl Pts',(-43.3760651419751,26.8573224770442,
146.213419117647));
#146723=CARTESIAN_POINT('Ctrl Pts',(-40.5392751458362,30.6138395280662,
144.719301470588));
#146724=CARTESIAN_POINT('Ctrl Pts',(-37.7024851496972,34.3703565790883,
143.225183823529));
#146725=CARTESIAN_POINT('Ctrl Pts',(-34.2237386972451,37.5416529948095,
141.731066176471));
#146726=CARTESIAN_POINT('Ctrl Pts',(-30.744992244793,40.7129494105307,140.236948529412));
#146727=CARTESIAN_POINT('Ctrl Pts',(-26.7427538741697,43.1910304950644,
138.742830882353));
#146728=CARTESIAN_POINT('Ctrl Pts',(-22.7405155035463,45.6691115795981,
137.248713235294));
#146729=CARTESIAN_POINT('Ctrl Pts',(-18.3510766423074,47.3695892537413,
135.754595588235));
#146730=CARTESIAN_POINT('Ctrl Pts',(-13.9616377810684,49.0700669278844,
134.260477941176));
#146731=CARTESIAN_POINT('Ctrl Pts',(-9.33447550508177,49.9350334639422,
132.766360294118));
#146732=CARTESIAN_POINT('Ctrl Pts',(-4.7073132290951,50.8,131.272242647059));
#146733=CARTESIAN_POINT('Ctrl Pts',(-6.22120573966855E-15,50.8,129.778125));
#146734=CARTESIAN_POINT('Ctrl Pts',(4.70731322909511,50.8,128.284007352941));
#146735=CARTESIAN_POINT('Ctrl Pts',(9.33447550508176,49.9350334639422,126.789889705882));
#146736=CARTESIAN_POINT('Ctrl Pts',(13.9616377810684,49.0700669278844,125.295772058823));
#146737=CARTESIAN_POINT('Ctrl Pts',(18.3510766423074,47.3695892537413,123.801654411765));
#146738=CARTESIAN_POINT('Ctrl Pts',(22.7405155035463,45.6691115795981,122.307536764706));
#146739=CARTESIAN_POINT('Ctrl Pts',(26.7427538741697,43.1910304950644,120.813419117647));
#146740=CARTESIAN_POINT('Ctrl Pts',(30.744992244793,40.7129494105307,119.319301470588));
#146741=CARTESIAN_POINT('Ctrl Pts',(34.2237386972451,37.5416529948095,117.825183823529));
#146742=CARTESIAN_POINT('Ctrl Pts',(37.7024851496972,34.3703565790883,116.331066176471));
#146743=CARTESIAN_POINT('Ctrl Pts',(40.5392751458362,30.6138395280662,114.836948529412));
#146744=CARTESIAN_POINT('Ctrl Pts',(43.3760651419751,26.8573224770442,113.342830882353));
#146745=CARTESIAN_POINT('Ctrl Pts',(45.4742952008372,22.6435084734481,111.848713235294));
#146746=CARTESIAN_POINT('Ctrl Pts',(47.5725252596992,18.4296944698521,110.354595588235));
#146747=CARTESIAN_POINT('Ctrl Pts',(48.8607426731792,13.9020798956618,108.860477941177));
#146748=CARTESIAN_POINT('Ctrl Pts',(50.1489600866593,9.37446532147146,107.366360294118));
#146749=CARTESIAN_POINT('Ctrl Pts',(50.5832961557877,4.68723266073574,105.872242647059));
#146750=CARTESIAN_POINT('Ctrl Pts',(51.0176322249162,9.37178700064808E-15,
104.378125));
#146751=CARTESIAN_POINT('Ctrl Pts',(50.5832961557877,-4.68723266073572,
102.884007352941));
#146752=CARTESIAN_POINT('Ctrl Pts',(50.1489600866593,-9.37446532147149,
101.389889705882));
#146753=CARTESIAN_POINT('Ctrl Pts',(48.8607426731792,-13.9020798956618,
99.8957720588236));
#146754=CARTESIAN_POINT('Ctrl Pts',(47.5725252596992,-18.4296944698521,
98.4016544117648));
#146755=CARTESIAN_POINT('Ctrl Pts',(45.4742952008371,-22.6435084734482,
96.9075367647059));
#146756=CARTESIAN_POINT('Ctrl Pts',(43.3760651419751,-26.8573224770441,
95.413419117647));
#146757=CARTESIAN_POINT('Ctrl Pts',(40.5392751458362,-30.6138395280662,
93.9193014705884));
#146758=CARTESIAN_POINT('Ctrl Pts',(37.7024851496972,-34.3703565790883,
92.4251838235295));
#146759=CARTESIAN_POINT('Ctrl Pts',(34.2237386972451,-37.5416529948095,
90.9310661764706));
#146760=CARTESIAN_POINT('Ctrl Pts',(30.744992244793,-40.7129494105307,89.4369485294118));
#146761=CARTESIAN_POINT('Ctrl Pts',(26.7427538741697,-43.1910304950644,
87.9428308823529));
#146762=CARTESIAN_POINT('Ctrl Pts',(22.7405155035463,-45.6691115795981,
86.4487132352943));
#146763=CARTESIAN_POINT('Ctrl Pts',(18.3510766423074,-47.3695892537413,
84.9545955882354));
#146764=CARTESIAN_POINT('Ctrl Pts',(13.9616377810684,-49.0700669278844,
83.4604779411765));
#146765=CARTESIAN_POINT('Ctrl Pts',(9.33447550508176,-49.9350334639422,
81.9663602941176));
#146766=CARTESIAN_POINT('Ctrl Pts',(4.70731322909511,-50.8,80.4722426470588));
#146767=CARTESIAN_POINT('Ctrl Pts',(0.,-50.8,78.9781250000001));
#146768=CARTESIAN_POINT('Ctrl Pts',(-4.70731322909511,-50.8,77.4840073529412));
#146769=CARTESIAN_POINT('Ctrl Pts',(-9.33447550508177,-49.9350334639422,
75.9898897058824));
#146770=CARTESIAN_POINT('Ctrl Pts',(-13.9616377810684,-49.0700669278844,
74.4957720588235));
#146771=CARTESIAN_POINT('Ctrl Pts',(-18.3510766423074,-47.3695892537413,
73.0016544117646));
#146772=CARTESIAN_POINT('Ctrl Pts',(-22.7405155035463,-45.6691115795981,
71.507536764706));
#146773=CARTESIAN_POINT('Ctrl Pts',(-26.7427538741697,-43.1910304950644,
70.0134191176471));
#146774=CARTESIAN_POINT('Ctrl Pts',(-30.744992244793,-40.7129494105307,
68.5193014705883));
#146775=CARTESIAN_POINT('Ctrl Pts',(-34.2237386972451,-37.5416529948095,
67.0251838235294));
#146776=CARTESIAN_POINT('Ctrl Pts',(-37.7024851496972,-34.3703565790883,
65.5310661764705));
#146777=CARTESIAN_POINT('Ctrl Pts',(-40.5392751458362,-30.6138395280662,
64.0369485294119));
#146778=CARTESIAN_POINT('Ctrl Pts',(-43.3760651419751,-26.8573224770441,
62.542830882353));
#146779=CARTESIAN_POINT('Ctrl Pts',(-45.4742952008371,-22.6435084734481,
61.0487132352942));
#146780=CARTESIAN_POINT('Ctrl Pts',(-47.5725252596992,-18.4296944698521,
59.5545955882353));
#146781=CARTESIAN_POINT('Ctrl Pts',(-48.8607426731792,-13.9020798956618,
58.0604779411764));
#146782=CARTESIAN_POINT('Ctrl Pts',(-50.1489600866593,-9.37446532147148,
56.5663602941178));
#146783=CARTESIAN_POINT('Ctrl Pts',(-50.5832961557877,-4.68723266073574,
55.0722426470589));
#146784=CARTESIAN_POINT('Ctrl Pts',(-51.0176322249162,-3.12392900021603E-15,
53.578125));
#146785=CARTESIAN_POINT('Ctrl Pts',(-50.5832961557877,4.68723266073573,
52.0840073529412));
#146786=CARTESIAN_POINT('Ctrl Pts',(-50.1489600866593,9.37446532147149,
50.5898897058823));
#146787=CARTESIAN_POINT('Ctrl Pts',(-48.8607426731792,13.9020798956618,
49.0957720588236));
#146788=CARTESIAN_POINT('Ctrl Pts',(-47.5725252596992,18.4296944698521,
47.6016544117648));
#146789=CARTESIAN_POINT('Ctrl Pts',(-45.4742952008371,22.6435084734481,
46.1075367647059));
#146790=CARTESIAN_POINT('Ctrl Pts',(-43.3760651419751,26.8573224770442,
44.613419117647));
#146791=CARTESIAN_POINT('Ctrl Pts',(-40.5392751458362,30.6138395280662,
43.1193014705882));
#146792=CARTESIAN_POINT('Ctrl Pts',(-37.7024851496972,34.3703565790883,
41.6251838235295));
#146793=CARTESIAN_POINT('Ctrl Pts',(-34.2237386972451,37.5416529948095,
40.1310661764707));
#146794=CARTESIAN_POINT('Ctrl Pts',(-30.744992244793,40.7129494105307,38.6369485294118));
#146795=CARTESIAN_POINT('Ctrl Pts',(-26.7427538741697,43.1910304950644,
37.1428308823529));
#146796=CARTESIAN_POINT('Ctrl Pts',(-22.7405155035463,45.6691115795981,
35.6487132352941));
#146797=CARTESIAN_POINT('Ctrl Pts',(-18.3510766423074,47.3695892537413,
34.1545955882354));
#146798=CARTESIAN_POINT('Ctrl Pts',(-13.9616377810684,49.0700669278844,
32.6604779411765));
#146799=CARTESIAN_POINT('Ctrl Pts',(-9.33447550508177,49.9350334639422,
31.1663602941177));
#146800=CARTESIAN_POINT('Ctrl Pts',(-4.7073132290951,50.8,29.6722426470588));
#146801=CARTESIAN_POINT('Ctrl Pts',(-6.22120573966855E-15,50.8,28.1781249999999));
#146802=CARTESIAN_POINT('Ctrl Pts',(4.70731322909511,50.8,26.6840073529413));
#146803=CARTESIAN_POINT('Ctrl Pts',(9.33447550508176,49.9350334639422,25.1898897058824));
#146804=CARTESIAN_POINT('Ctrl Pts',(13.9616377810684,49.0700669278844,23.6957720588236));
#146805=CARTESIAN_POINT('Ctrl Pts',(18.3510766423074,47.3695892537413,22.2016544117647));
#146806=CARTESIAN_POINT('Ctrl Pts',(22.7405155035463,45.6691115795981,20.7075367647058));
#146807=CARTESIAN_POINT('Ctrl Pts',(26.7427538741697,43.1910304950644,19.2134191176472));
#146808=CARTESIAN_POINT('Ctrl Pts',(30.744992244793,40.7129494105307,17.7193014705883));
#146809=CARTESIAN_POINT('Ctrl Pts',(34.2237386972451,37.5416529948095,16.2251838235294));
#146810=CARTESIAN_POINT('Ctrl Pts',(37.7024851496972,34.3703565790883,14.7310661764706));
#146811=CARTESIAN_POINT('Ctrl Pts',(40.5392751458362,30.6138395280662,13.2369485294117));
#146812=CARTESIAN_POINT('Ctrl Pts',(43.3760651419751,26.8573224770442,11.7428308823531));
#146813=CARTESIAN_POINT('Ctrl Pts',(45.4742952008372,22.6435084734481,10.2487132352942));
#146814=CARTESIAN_POINT('Ctrl Pts',(47.5725252596992,18.4296944698521,8.75459558823533));
#146815=CARTESIAN_POINT('Ctrl Pts',(48.8607426731792,13.9020798956618,7.26047794117646));
#146816=CARTESIAN_POINT('Ctrl Pts',(50.1489600866593,9.37446532147146,5.76636029411759));
#146817=CARTESIAN_POINT('Ctrl Pts',(50.5832961557877,4.68723266073574,4.27224264705894));
#146818=CARTESIAN_POINT('Ctrl Pts',(51.0176322249162,9.37178700064808E-15,
2.77812500000008));
#146819=CARTESIAN_POINT('Ctrl Pts',(50.5832961557877,-4.68723266073572,
1.28400735294121));
#146820=CARTESIAN_POINT('Ctrl Pts',(50.1489600866593,-9.37446532147149,
-0.21011029411766));
#146821=CARTESIAN_POINT('Ctrl Pts',(48.8607426731792,-13.9020798956618,
-1.70422794117653));
#146822=CARTESIAN_POINT('Ctrl Pts',(47.5725252596992,-18.4296944698521,
-3.19834558823517));
#146823=CARTESIAN_POINT('Ctrl Pts',(45.4742952008371,-22.6435084734482,
-4.69246323529404));
#146824=CARTESIAN_POINT('Ctrl Pts',(43.3760651419751,-26.8573224770441,
-6.18658088235291));
#146825=CARTESIAN_POINT('Ctrl Pts',(40.5392751458362,-30.6138395280662,
-7.68069852941178));
#146826=CARTESIAN_POINT('Ctrl Pts',(37.7024851496972,-34.3703565790883,
-9.17481617647065));
#146827=CARTESIAN_POINT('Ctrl Pts',(34.2237386972451,-37.5416529948095,
-10.6689338235293));
#146828=CARTESIAN_POINT('Ctrl Pts',(30.744992244793,-40.7129494105307,-12.1630514705882));
#146829=CARTESIAN_POINT('Ctrl Pts',(26.7427538741697,-43.1910304950644,
-13.657169117647));
#146830=CARTESIAN_POINT('Ctrl Pts',(22.7405155035463,-45.6691115795981,
-15.1512867647059));
#146831=CARTESIAN_POINT('Ctrl Pts',(18.3510766423074,-47.3695892537413,
-16.6454044117648));
#146832=CARTESIAN_POINT('Ctrl Pts',(13.9616377810684,-49.0700669278844,
-18.1395220588234));
#146833=CARTESIAN_POINT('Ctrl Pts',(9.33447550508176,-49.9350334639422,
-19.6336397058823));
#146834=CARTESIAN_POINT('Ctrl Pts',(4.70731322909511,-50.8,-21.1277573529411));
#146835=CARTESIAN_POINT('Ctrl Pts',(0.,-50.8,-22.621875));
#146836=CARTESIAN_POINT('Ctrl Pts',(-4.70731322909511,-50.8,-24.1159926470589));
#146837=CARTESIAN_POINT('Ctrl Pts',(-9.33447550508177,-49.9350334639422,
-25.6101102941175));
#146838=CARTESIAN_POINT('Ctrl Pts',(-13.9616377810684,-49.0700669278844,
-27.1042279411764));
#146839=CARTESIAN_POINT('Ctrl Pts',(-18.3510766423074,-47.3695892537413,
-28.5983455882353));
#146840=CARTESIAN_POINT('Ctrl Pts',(-22.7405155035463,-45.6691115795981,
-30.0924632352941));
#146841=CARTESIAN_POINT('Ctrl Pts',(-26.7427538741697,-43.1910304950644,
-31.586580882353));
#146842=CARTESIAN_POINT('Ctrl Pts',(-30.744992244793,-40.7129494105307,
-33.0806985294116));
#146843=CARTESIAN_POINT('Ctrl Pts',(-34.2237386972451,-37.5416529948095,
-34.5748161764705));
#146844=CARTESIAN_POINT('Ctrl Pts',(-37.7024851496972,-34.3703565790883,
-36.0689338235294));
#146845=CARTESIAN_POINT('Ctrl Pts',(-40.5392751458362,-30.6138395280662,
-37.5630514705882));
#146846=CARTESIAN_POINT('Ctrl Pts',(-43.3760651419751,-26.8573224770441,
-39.0571691176471));
#146847=CARTESIAN_POINT('Ctrl Pts',(-45.4742952008371,-22.6435084734481,
-40.5512867647058));
#146848=CARTESIAN_POINT('Ctrl Pts',(-47.5725252596992,-18.4296944698521,
-42.0454044117646));
#146849=CARTESIAN_POINT('Ctrl Pts',(-48.8607426731792,-13.9020798956618,
-43.5395220588235));
#146850=CARTESIAN_POINT('Ctrl Pts',(-50.1489600866593,-9.37446532147148,
-45.0336397058824));
#146851=CARTESIAN_POINT('Ctrl Pts',(-50.5832961557877,-4.68723266073574,
-46.5277573529412));
#146852=CARTESIAN_POINT('Ctrl Pts',(-51.0176322249162,-3.12392900021603E-15,
-48.0218749999999));
#146853=CARTESIAN_POINT('Ctrl Pts',(-50.5832961557877,4.68723266073573,
-49.5159926470588));
#146854=CARTESIAN_POINT('Ctrl Pts',(-50.1489600866593,9.37446532147149,
-51.0101102941176));
#146855=CARTESIAN_POINT('Ctrl Pts',(-48.8607426731792,13.9020798956618,
-52.5042279411765));
#146856=CARTESIAN_POINT('Ctrl Pts',(-47.5725252596992,18.4296944698521,
-53.9983455882354));
#146857=CARTESIAN_POINT('Ctrl Pts',(-45.4742952008371,22.6435084734481,
-55.492463235294));
#146858=CARTESIAN_POINT('Ctrl Pts',(-43.3760651419751,26.8573224770442,
-56.9865808823529));
#146859=CARTESIAN_POINT('Ctrl Pts',(-40.5392751458362,30.6138395280662,
-58.4806985294117));
#146860=CARTESIAN_POINT('Ctrl Pts',(-37.7024851496972,34.3703565790883,
-59.9748161764706));
#146861=CARTESIAN_POINT('Ctrl Pts',(-34.2237386972451,37.5416529948095,
-61.4689338235295));
#146862=CARTESIAN_POINT('Ctrl Pts',(-30.744992244793,40.7129494105307,-62.9630514705881));
#146863=CARTESIAN_POINT('Ctrl Pts',(-26.7427538741697,43.1910304950644,
-64.457169117647));
#146864=CARTESIAN_POINT('Ctrl Pts',(-22.7405155035463,45.6691115795981,
-65.9512867647058));
#146865=CARTESIAN_POINT('Ctrl Pts',(-18.3510766423074,47.3695892537413,
-67.4454044117647));
#146866=CARTESIAN_POINT('Ctrl Pts',(-13.9616377810684,49.0700669278844,
-68.9395220588236));
#146867=CARTESIAN_POINT('Ctrl Pts',(-9.33447550508177,49.9350334639422,
-70.4336397058822));
#146868=CARTESIAN_POINT('Ctrl Pts',(-4.7073132290951,50.8,-71.9277573529411));
#146869=CARTESIAN_POINT('Ctrl Pts',(-6.22120573966855E-15,50.8,-73.421875));
#146870=CARTESIAN_POINT('Ctrl Pts',(4.70731322909511,50.8,-74.9159926470588));
#146871=CARTESIAN_POINT('Ctrl Pts',(9.33447550508176,49.9350334639422,-76.4101102941177));
#146872=CARTESIAN_POINT('Ctrl Pts',(13.9616377810684,49.0700669278844,-77.9042279411764));
#146873=CARTESIAN_POINT('Ctrl Pts',(18.3510766423074,47.3695892537413,-79.3983455882352));
#146874=CARTESIAN_POINT('Ctrl Pts',(22.7405155035463,45.6691115795981,-80.8924632352941));
#146875=CARTESIAN_POINT('Ctrl Pts',(26.7427538741697,43.1910304950644,-82.386580882353));
#146876=CARTESIAN_POINT('Ctrl Pts',(30.744992244793,40.7129494105307,-83.8806985294118));
#146877=CARTESIAN_POINT('Ctrl Pts',(34.2237386972451,37.5416529948095,-85.3748161764705));
#146878=CARTESIAN_POINT('Ctrl Pts',(37.7024851496972,34.3703565790883,-86.8689338235293));
#146879=CARTESIAN_POINT('Ctrl Pts',(40.5392751458362,30.6138395280662,-88.3630514705882));
#146880=CARTESIAN_POINT('Ctrl Pts',(43.3760651419751,26.8573224770442,-89.8571691176471));
#146881=CARTESIAN_POINT('Ctrl Pts',(45.4742952008372,22.6435084734481,-91.3512867647059));
#146882=CARTESIAN_POINT('Ctrl Pts',(47.5725252596992,18.4296944698521,-92.8454044117646));
#146883=CARTESIAN_POINT('Ctrl Pts',(48.8607426731792,13.9020798956618,-94.3395220588235));
#146884=CARTESIAN_POINT('Ctrl Pts',(50.1489600866593,9.37446532147146,-95.8336397058823));
#146885=CARTESIAN_POINT('Ctrl Pts',(50.5832961557877,4.68723266073574,-97.3277573529412));
#146886=CARTESIAN_POINT('Ctrl Pts',(51.0176322249162,9.37178700064808E-15,
-98.8218750000001));
#146887=CARTESIAN_POINT('Ctrl Pts',(50.5832961557877,-4.68723266073572,
-100.315992647059));
#146888=CARTESIAN_POINT('Ctrl Pts',(50.1489600866593,-9.37446532147149,
-101.810110294118));
#146889=CARTESIAN_POINT('Ctrl Pts',(48.8607426731792,-13.9020798956618,
-103.304227941176));
#146890=CARTESIAN_POINT('Ctrl Pts',(47.5725252596992,-18.4296944698521,
-104.798345588235));
#146891=CARTESIAN_POINT('Ctrl Pts',(45.4742952008371,-22.6435084734482,
-106.292463235294));
#146892=CARTESIAN_POINT('Ctrl Pts',(43.3760651419751,-26.8573224770441,
-107.786580882353));
#146893=CARTESIAN_POINT('Ctrl Pts',(40.5392751458362,-30.6138395280662,
-109.280698529412));
#146894=CARTESIAN_POINT('Ctrl Pts',(37.7024851496972,-34.3703565790883,
-110.774816176471));
#146895=CARTESIAN_POINT('Ctrl Pts',(34.2237386972451,-37.5416529948095,
-112.268933823529));
#146896=CARTESIAN_POINT('Ctrl Pts',(30.744992244793,-40.7129494105307,-113.763051470588));
#146897=CARTESIAN_POINT('Ctrl Pts',(26.7427538741697,-43.1910304950644,
-115.257169117647));
#146898=CARTESIAN_POINT('Ctrl Pts',(22.7405155035463,-45.6691115795981,
-116.751286764706));
#146899=CARTESIAN_POINT('Ctrl Pts',(18.3510766423074,-47.3695892537413,
-118.245404411765));
#146900=CARTESIAN_POINT('Ctrl Pts',(13.9616377810684,-49.0700669278844,
-119.739522058824));
#146901=CARTESIAN_POINT('Ctrl Pts',(9.33447550508176,-49.9350334639422,
-121.233639705882));
#146902=CARTESIAN_POINT('Ctrl Pts',(4.70731322909511,-50.8,-122.727757352941));
#146903=CARTESIAN_POINT('Ctrl Pts',(0.,-50.8,-124.221875));
#146904=CARTESIAN_POINT('Ctrl Pts',(-4.70731322909511,-50.8,-125.715992647059));
#146905=CARTESIAN_POINT('Ctrl Pts',(-9.33447550508177,-49.9350334639422,
-127.210110294118));
#146906=CARTESIAN_POINT('Ctrl Pts',(-13.9616377810684,-49.0700669278844,
-128.704227941177));
#146907=CARTESIAN_POINT('Ctrl Pts',(-18.3510766423074,-47.3695892537413,
-130.198345588235));
#146908=CARTESIAN_POINT('Ctrl Pts',(-22.7405155035463,-45.6691115795981,
-131.692463235294));
#146909=CARTESIAN_POINT('Ctrl Pts',(-26.7427538741697,-43.1910304950644,
-133.186580882353));
#146910=CARTESIAN_POINT('Ctrl Pts',(-30.744992244793,-40.7129494105307,
-134.680698529412));
#146911=CARTESIAN_POINT('Ctrl Pts',(-34.2237386972451,-37.5416529948095,
-136.174816176471));
#146912=CARTESIAN_POINT('Ctrl Pts',(-37.7024851496972,-34.3703565790883,
-137.668933823529));
#146913=CARTESIAN_POINT('Ctrl Pts',(-40.5392751458362,-30.6138395280662,
-139.163051470588));
#146914=CARTESIAN_POINT('Ctrl Pts',(-43.3760651419751,-26.8573224770441,
-140.657169117647));
#146915=CARTESIAN_POINT('Ctrl Pts',(-45.4742952008371,-22.6435084734481,
-142.151286764706));
#146916=CARTESIAN_POINT('Ctrl Pts',(-47.5725252596992,-18.4296944698521,
-143.645404411765));
#146917=CARTESIAN_POINT('Ctrl Pts',(-48.8607426731792,-13.9020798956618,
-145.139522058823));
#146918=CARTESIAN_POINT('Ctrl Pts',(-50.1489600866593,-9.37446532147148,
-146.633639705882));
#146919=CARTESIAN_POINT('Ctrl Pts',(-50.5832961557877,-4.68723266073574,
-148.127757352941));
#146920=CARTESIAN_POINT('Ctrl Pts',(-51.0176322249162,-3.12392900021603E-15,
-149.621875));
#146921=CARTESIAN_POINT('Ctrl Pts',(-50.5832961557877,4.68723266073573,
-151.115992647059));
#146922=CARTESIAN_POINT('Ctrl Pts',(-50.1489600866593,9.37446532147149,
-152.610110294118));
#146923=CARTESIAN_POINT('Ctrl Pts',(-48.8607426731792,13.9020798956618,
-154.104227941176));
#146924=CARTESIAN_POINT('Ctrl Pts',(-47.5725252596992,18.4296944698521,
-155.598345588235));
#146925=CARTESIAN_POINT('Ctrl Pts',(-45.4742952008371,22.6435084734481,
-157.092463235294));
#146926=CARTESIAN_POINT('Ctrl Pts',(-43.3760651419751,26.8573224770442,
-158.586580882353));
#146927=CARTESIAN_POINT('Ctrl Pts',(-40.5392751458362,30.6138395280662,
-160.080698529412));
#146928=CARTESIAN_POINT('Ctrl Pts',(-37.7024851496972,34.3703565790883,
-161.574816176471));
#146929=CARTESIAN_POINT('Ctrl Pts',(-34.2237386972451,37.5416529948095,
-163.068933823529));
#146930=CARTESIAN_POINT('Ctrl Pts',(-30.744992244793,40.7129494105307,-164.563051470588));
#146931=CARTESIAN_POINT('Ctrl Pts',(-26.7427538741697,43.1910304950644,
-166.057169117647));
#146932=CARTESIAN_POINT('Ctrl Pts',(-22.7405155035463,45.6691115795981,
-167.551286764706));
#146933=CARTESIAN_POINT('Ctrl Pts',(-18.3510766423074,47.3695892537413,
-169.045404411765));
#146934=CARTESIAN_POINT('Ctrl Pts',(-13.9616377810684,49.0700669278844,
-170.539522058824));
#146935=CARTESIAN_POINT('Ctrl Pts',(-9.33447550508177,49.9350334639422,
-172.033639705882));
#146936=CARTESIAN_POINT('Ctrl Pts',(-4.7073132290951,50.8,-173.527757352941));
#146937=CARTESIAN_POINT('Ctrl Pts',(-6.22120573966855E-15,50.8,-175.021875));
#146938=CARTESIAN_POINT('Ctrl Pts',(4.70731322909511,50.8,-176.515992647059));
#146939=CARTESIAN_POINT('Ctrl Pts',(9.33447550508176,49.9350334639422,-178.010110294118));
#146940=CARTESIAN_POINT('Ctrl Pts',(13.9616377810684,49.0700669278844,-179.504227941177));
#146941=CARTESIAN_POINT('Ctrl Pts',(18.3510766423074,47.3695892537413,-180.998345588235));
#146942=CARTESIAN_POINT('Ctrl Pts',(22.7405155035463,45.6691115795981,-182.492463235294));
#146943=CARTESIAN_POINT('Ctrl Pts',(26.7427538741697,43.1910304950644,-183.986580882353));
#146944=CARTESIAN_POINT('Ctrl Pts',(30.744992244793,40.7129494105307,-185.480698529412));
#146945=CARTESIAN_POINT('Ctrl Pts',(34.2237386972451,37.5416529948095,-186.974816176471));
#146946=CARTESIAN_POINT('Ctrl Pts',(37.7024851496972,34.3703565790883,-188.468933823529));
#146947=CARTESIAN_POINT('Ctrl Pts',(40.5392751458362,30.6138395280662,-189.963051470588));
#146948=CARTESIAN_POINT('Ctrl Pts',(43.3760651419751,26.8573224770442,-191.457169117647));
#146949=CARTESIAN_POINT('Ctrl Pts',(45.4742952008372,22.6435084734481,-192.951286764706));
#146950=CARTESIAN_POINT('Ctrl Pts',(47.5725252596992,18.4296944698521,-194.445404411765));
#146951=CARTESIAN_POINT('Ctrl Pts',(48.8607426731792,13.9020798956618,-195.939522058824));
#146952=CARTESIAN_POINT('Ctrl Pts',(50.1489600866593,9.37446532147146,-197.433639705882));
#146953=CARTESIAN_POINT('Ctrl Pts',(50.5832961557877,4.68723266073574,-198.927757352941));
#146954=CARTESIAN_POINT('Ctrl Pts',(51.0176322249162,9.37178700064808E-15,
-200.421875));
#146955=CARTESIAN_POINT('Ctrl Pts',(50.5832961557877,-4.68723266073572,
-201.915992647059));
#146956=CARTESIAN_POINT('Ctrl Pts',(50.1489600866593,-9.37446532147149,
-203.410110294118));
#146957=CARTESIAN_POINT('Ctrl Pts',(48.8607426731792,-13.9020798956618,
-204.904227941176));
#146958=CARTESIAN_POINT('Ctrl Pts',(47.5725252596992,-18.4296944698521,
-206.398345588235));
#146959=CARTESIAN_POINT('Ctrl Pts',(45.4742952008371,-22.6435084734482,
-207.892463235294));
#146960=CARTESIAN_POINT('Ctrl Pts',(43.3760651419751,-26.8573224770441,
-209.386580882353));
#146961=CARTESIAN_POINT('Ctrl Pts',(40.5392751458362,-30.6138395280662,
-210.880698529412));
#146962=CARTESIAN_POINT('Ctrl Pts',(37.7024851496972,-34.3703565790883,
-212.374816176471));
#146963=CARTESIAN_POINT('Ctrl Pts',(34.2237386972451,-37.5416529948095,
-213.868933823529));
#146964=CARTESIAN_POINT('Ctrl Pts',(30.744992244793,-40.7129494105307,-215.363051470588));
#146965=CARTESIAN_POINT('Ctrl Pts',(26.7427538741697,-43.1910304950644,
-216.857169117647));
#146966=CARTESIAN_POINT('Ctrl Pts',(22.7405155035463,-45.6691115795981,
-218.351286764706));
#146967=CARTESIAN_POINT('Ctrl Pts',(18.3510766423074,-47.3695892537413,
-219.845404411765));
#146968=CARTESIAN_POINT('Ctrl Pts',(13.9616377810684,-49.0700669278844,
-221.339522058823));
#146969=CARTESIAN_POINT('Ctrl Pts',(9.33447550508176,-49.9350334639422,
-222.833639705882));
#146970=CARTESIAN_POINT('Ctrl Pts',(4.70731322909511,-50.8,-224.327757352941));
#146971=CARTESIAN_POINT('Ctrl Pts',(0.,-50.8,-225.821875));
#146972=CARTESIAN_POINT('Ctrl Pts',(-4.70731322909511,-50.8,-227.315992647059));
#146973=CARTESIAN_POINT('Ctrl Pts',(-9.33447550508177,-49.9350334639422,
-228.810110294118));
#146974=CARTESIAN_POINT('Ctrl Pts',(-13.9616377810684,-49.0700669278844,
-230.304227941176));
#146975=CARTESIAN_POINT('Ctrl Pts',(-18.3510766423074,-47.3695892537413,
-231.798345588235));
#146976=CARTESIAN_POINT('Ctrl Pts',(-22.7405155035463,-45.6691115795981,
-233.292463235294));
#146977=CARTESIAN_POINT('Ctrl Pts',(-26.7427538741697,-43.1910304950644,
-234.786580882353));
#146978=CARTESIAN_POINT('Ctrl Pts',(-30.744992244793,-40.7129494105307,
-236.280698529412));
#146979=CARTESIAN_POINT('Ctrl Pts',(-34.2237386972451,-37.5416529948095,
-237.774816176471));
#146980=CARTESIAN_POINT('Ctrl Pts',(-37.7024851496972,-34.3703565790883,
-239.268933823529));
#146981=CARTESIAN_POINT('Ctrl Pts',(-40.5392751458362,-30.6138395280662,
-240.763051470588));
#146982=CARTESIAN_POINT('Ctrl Pts',(-43.3760651419751,-26.8573224770441,
-242.257169117647));
#146983=CARTESIAN_POINT('Ctrl Pts',(-45.4742952008371,-22.6435084734481,
-243.751286764706));
#146984=CARTESIAN_POINT('Ctrl Pts',(-47.5725252596992,-18.4296944698521,
-245.245404411765));
#146985=CARTESIAN_POINT('Ctrl Pts',(-48.8607426731792,-13.9020798956618,
-246.739522058824));
#146986=CARTESIAN_POINT('Ctrl Pts',(-50.1489600866593,-9.37446532147148,
-248.233639705882));
#146987=CARTESIAN_POINT('Ctrl Pts',(-50.5832961557877,-4.68723266073574,
-249.727757352941));
#146988=CARTESIAN_POINT('Ctrl Pts',(-51.0176322249162,-3.12392900021603E-15,
-251.221875));
#146989=CARTESIAN_POINT('Ctrl Pts',(-50.5832961557877,4.68723266073573,
-252.715992647059));
#146990=CARTESIAN_POINT('Ctrl Pts',(-50.1489600866593,9.37446532147149,
-254.210110294118));
#146991=CARTESIAN_POINT('Ctrl Pts',(-48.8607426731792,13.9020798956618,
-255.704227941177));
#146992=CARTESIAN_POINT('Ctrl Pts',(-47.5725252596992,18.4296944698521,
-257.198345588235));
#146993=CARTESIAN_POINT('Ctrl Pts',(-45.4742952008371,22.6435084734481,
-258.692463235294));
#146994=CARTESIAN_POINT('Ctrl Pts',(-43.3760651419751,26.8573224770442,
-260.186580882353));
#146995=CARTESIAN_POINT('Ctrl Pts',(-40.5392751458362,30.6138395280662,
-261.680698529412));
#146996=CARTESIAN_POINT('Ctrl Pts',(-37.7024851496972,34.3703565790883,
-263.174816176471));
#146997=CARTESIAN_POINT('Ctrl Pts',(-34.2237386972451,37.5416529948095,
-264.668933823529));
#146998=CARTESIAN_POINT('Ctrl Pts',(-30.744992244793,40.7129494105307,-266.163051470588));
#146999=CARTESIAN_POINT('Ctrl Pts',(-26.7427538741697,43.1910304950644,
-267.657169117647));
#147000=CARTESIAN_POINT('Ctrl Pts',(-22.7405155035463,45.6691115795981,
-269.151286764706));
#147001=CARTESIAN_POINT('Ctrl Pts',(-18.3510766423074,47.3695892537413,
-270.645404411765));
#147002=CARTESIAN_POINT('Ctrl Pts',(-13.9616377810684,49.0700669278844,
-272.139522058824));
#147003=CARTESIAN_POINT('Ctrl Pts',(-9.33447550508177,49.9350334639422,
-273.633639705882));
#147004=CARTESIAN_POINT('Ctrl Pts',(-4.7073132290951,50.8,-275.127757352941));
#147005=CARTESIAN_POINT('Ctrl Pts',(-6.22120573966855E-15,50.8,-276.621875));
#147006=CARTESIAN_POINT('Ctrl Pts',(4.70731322909511,50.8,-278.115992647059));
#147007=CARTESIAN_POINT('Ctrl Pts',(9.33447550508176,49.9350334639422,-279.610110294118));
#147008=CARTESIAN_POINT('Ctrl Pts',(13.9616377810684,49.0700669278844,-281.104227941176));
#147009=CARTESIAN_POINT('Ctrl Pts',(18.3510766423074,47.3695892537413,-282.598345588235));
#147010=CARTESIAN_POINT('Ctrl Pts',(22.7405155035463,45.6691115795981,-284.092463235294));
#147011=CARTESIAN_POINT('Ctrl Pts',(26.7427538741697,43.1910304950644,-285.586580882353));
#147012=CARTESIAN_POINT('Ctrl Pts',(30.744992244793,40.7129494105307,-287.080698529412));
#147013=CARTESIAN_POINT('Ctrl Pts',(34.2237386972451,37.5416529948095,-288.574816176471));
#147014=CARTESIAN_POINT('Ctrl Pts',(37.7024851496972,34.3703565790883,-290.068933823529));
#147015=CARTESIAN_POINT('Ctrl Pts',(40.5392751458362,30.6138395280662,-291.563051470588));
#147016=CARTESIAN_POINT('Ctrl Pts',(43.3760651419751,26.8573224770442,-293.057169117647));
#147017=CARTESIAN_POINT('Ctrl Pts',(45.4742952008372,22.6435084734481,-294.551286764706));
#147018=CARTESIAN_POINT('Ctrl Pts',(47.5725252596992,18.4296944698521,-296.045404411765));
#147019=CARTESIAN_POINT('Ctrl Pts',(48.8607426731792,13.9020798956618,-297.539522058823));
#147020=CARTESIAN_POINT('Ctrl Pts',(50.1489600866593,9.37446532147146,-299.033639705882));
#147021=CARTESIAN_POINT('Ctrl Pts',(50.5832961557877,4.68723266073574,-300.527757352941));
#147022=CARTESIAN_POINT('Ctrl Pts',(51.0176322249162,9.37178700064808E-15,
-302.021875));
#147023=CARTESIAN_POINT('Ctrl Pts',(50.5832961557877,-4.68723266073572,
-303.515992647059));
#147024=CARTESIAN_POINT('Ctrl Pts',(50.1489600866593,-9.37446532147149,
-305.010110294118));
#147025=CARTESIAN_POINT('Ctrl Pts',(48.8607426731792,-13.9020798956618,
-306.504227941177));
#147026=CARTESIAN_POINT('Ctrl Pts',(47.5725252596992,-18.4296944698521,
-307.998345588235));
#147027=CARTESIAN_POINT('Ctrl Pts',(45.4742952008371,-22.6435084734482,
-309.492463235294));
#147028=CARTESIAN_POINT('Ctrl Pts',(43.3760651419751,-26.8573224770441,
-310.986580882353));
#147029=CARTESIAN_POINT('Ctrl Pts',(40.5392751458362,-30.6138395280662,
-312.480698529412));
#147030=CARTESIAN_POINT('Ctrl Pts',(37.7024851496972,-34.3703565790883,
-313.974816176471));
#147031=CARTESIAN_POINT('Ctrl Pts',(34.2237386972451,-37.5416529948095,
-315.468933823529));
#147032=CARTESIAN_POINT('Ctrl Pts',(30.744992244793,-40.7129494105307,-316.963051470588));
#147033=CARTESIAN_POINT('Ctrl Pts',(26.7427538741697,-43.1910304950644,
-318.457169117647));
#147034=CARTESIAN_POINT('Ctrl Pts',(22.7405155035463,-45.6691115795981,
-319.951286764706));
#147035=CARTESIAN_POINT('Ctrl Pts',(18.3510766423074,-47.3695892537413,
-321.445404411765));
#147036=CARTESIAN_POINT('Ctrl Pts',(13.9616377810684,-49.0700669278844,
-322.939522058824));
#147037=CARTESIAN_POINT('Ctrl Pts',(9.33447550508176,-49.9350334639422,
-324.433639705882));
#147038=CARTESIAN_POINT('Ctrl Pts',(4.70731322909511,-50.8,-325.927757352941));
#147039=CARTESIAN_POINT('Ctrl Pts',(0.,-50.8,-327.421875));
#147040=CARTESIAN_POINT('Ctrl Pts',(-4.70731322909511,-50.8,-328.915992647059));
#147041=CARTESIAN_POINT('Ctrl Pts',(-9.33447550508177,-49.9350334639422,
-330.410110294118));
#147042=CARTESIAN_POINT('Ctrl Pts',(-13.9616377810684,-49.0700669278844,
-331.904227941176));
#147043=CARTESIAN_POINT('Ctrl Pts',(-18.3510766423074,-47.3695892537413,
-333.398345588235));
#147044=CARTESIAN_POINT('Ctrl Pts',(-22.7405155035463,-45.6691115795981,
-334.892463235294));
#147045=CARTESIAN_POINT('Ctrl Pts',(-26.7427538741697,-43.1910304950644,
-336.386580882353));
#147046=CARTESIAN_POINT('Ctrl Pts',(-30.744992244793,-40.7129494105307,
-337.880698529412));
#147047=CARTESIAN_POINT('Ctrl Pts',(-34.2237386972451,-37.5416529948095,
-339.37481617647));
#147048=CARTESIAN_POINT('Ctrl Pts',(-37.7024851496972,-34.3703565790883,
-340.868933823529));
#147049=CARTESIAN_POINT('Ctrl Pts',(-40.5392751458362,-30.6138395280662,
-342.363051470588));
#147050=CARTESIAN_POINT('Ctrl Pts',(-43.3760651419751,-26.8573224770441,
-343.857169117647));
#147051=CARTESIAN_POINT('Ctrl Pts',(-45.4742952008371,-22.6435084734481,
-345.351286764706));
#147052=CARTESIAN_POINT('Ctrl Pts',(-47.5725252596992,-18.4296944698521,
-346.845404411765));
#147053=CARTESIAN_POINT('Ctrl Pts',(-48.8607426731792,-13.9020798956618,
-348.339522058823));
#147054=CARTESIAN_POINT('Ctrl Pts',(-50.1489600866593,-9.37446532147148,
-349.833639705882));
#147055=CARTESIAN_POINT('Ctrl Pts',(-50.5832961557877,-4.68723266073574,
-351.327757352941));
#147056=CARTESIAN_POINT('Ctrl Pts',(-51.0176322249162,-3.12392900021603E-15,
-352.821875));
#147057=CARTESIAN_POINT('Ctrl Pts',(-50.5832961557877,4.68723266073573,
-354.315992647059));
#147058=CARTESIAN_POINT('Ctrl Pts',(-50.1489600866593,9.37446532147149,
-355.810110294118));
#147059=CARTESIAN_POINT('Ctrl Pts',(-48.8607426731792,13.9020798956618,
-357.304227941177));
#147060=CARTESIAN_POINT('Ctrl Pts',(-47.5725252596992,18.4296944698521,
-358.798345588235));
#147061=CARTESIAN_POINT('Ctrl Pts',(-45.4742952008371,22.6435084734481,
-360.292463235294));
#147062=CARTESIAN_POINT('Ctrl Pts',(-43.3760651419751,26.8573224770442,
-361.786580882353));
#147063=CARTESIAN_POINT('Ctrl Pts',(-40.5392751458362,30.6138395280662,
-363.280698529412));
#147064=CARTESIAN_POINT('Ctrl Pts',(-37.7024851496972,34.3703565790883,
-364.774816176471));
#147065=CARTESIAN_POINT('Ctrl Pts',(-34.2237386972451,37.5416529948095,
-366.268933823529));
#147066=CARTESIAN_POINT('Ctrl Pts',(-30.744992244793,40.7129494105307,-367.763051470588));
#147067=CARTESIAN_POINT('Ctrl Pts',(-26.7427538741697,43.1910304950644,
-369.257169117647));
#147068=CARTESIAN_POINT('Ctrl Pts',(-22.7405155035463,45.6691115795981,
-370.751286764706));
#147069=CARTESIAN_POINT('Ctrl Pts',(-18.3510766423074,47.3695892537413,
-372.245404411765));
#147070=CARTESIAN_POINT('Ctrl Pts',(-13.9616377810684,49.0700669278844,
-373.739522058824));
#147071=CARTESIAN_POINT('Ctrl Pts',(-9.33447550508177,49.9350334639422,
-375.233639705882));
#147072=CARTESIAN_POINT('Ctrl Pts',(-4.7073132290951,50.8,-376.727757352941));
#147073=CARTESIAN_POINT('Ctrl Pts',(-6.22120573966855E-15,50.8,-378.221875));
#147074=CARTESIAN_POINT('Ctrl Pts',(4.70731322909511,50.8,-379.715992647059));
#147075=CARTESIAN_POINT('Ctrl Pts',(9.33447550508176,49.9350334639422,-381.210110294118));
#147076=CARTESIAN_POINT('Ctrl Pts',(13.9616377810684,49.0700669278844,-382.704227941177));
#147077=CARTESIAN_POINT('Ctrl Pts',(18.3510766423074,47.3695892537413,-384.198345588235));
#147078=CARTESIAN_POINT('Ctrl Pts',(22.7405155035463,45.6691115795981,-385.692463235294));
#147079=CARTESIAN_POINT('Ctrl Pts',(26.7427538741697,43.1910304950644,-387.186580882353));
#147080=CARTESIAN_POINT('Ctrl Pts',(30.744992244793,40.7129494105307,-388.680698529412));
#147081=CARTESIAN_POINT('Ctrl Pts',(34.2237386972451,37.5416529948095,-390.174816176471));
#147082=CARTESIAN_POINT('Ctrl Pts',(37.7024851496972,34.3703565790883,-391.668933823529));
#147083=CARTESIAN_POINT('Ctrl Pts',(40.5392751458362,30.6138395280662,-393.163051470588));
#147084=CARTESIAN_POINT('Ctrl Pts',(43.3760651419751,26.8573224770442,-394.657169117647));
#147085=CARTESIAN_POINT('Ctrl Pts',(45.4742952008372,22.6435084734481,-396.151286764706));
#147086=CARTESIAN_POINT('Ctrl Pts',(47.5725252596992,18.4296944698521,-397.645404411765));
#147087=CARTESIAN_POINT('Ctrl Pts',(48.8607426731792,13.9020798956618,-399.139522058823));
#147088=CARTESIAN_POINT('Ctrl Pts',(50.1489600866593,9.37446532147146,-400.633639705882));
#147089=CARTESIAN_POINT('Ctrl Pts',(50.5832961557877,4.68723266073574,-402.127757352941));
#147090=CARTESIAN_POINT('Ctrl Pts',(51.0176322249162,9.37178700064808E-15,
-403.621875));
#147091=CARTESIAN_POINT('Ctrl Pts',(50.5832961557877,-4.68723266073572,
-405.115992647059));
#147092=CARTESIAN_POINT('Ctrl Pts',(50.1489600866593,-9.37446532147149,
-406.610110294118));
#147093=CARTESIAN_POINT('Ctrl Pts',(48.8607426731792,-13.9020798956618,
-408.104227941176));
#147094=CARTESIAN_POINT('Ctrl Pts',(47.5725252596992,-18.4296944698521,
-409.598345588235));
#147095=CARTESIAN_POINT('Ctrl Pts',(45.4742952008371,-22.6435084734482,
-411.092463235294));
#147096=CARTESIAN_POINT('Ctrl Pts',(43.3760651419751,-26.8573224770441,
-412.586580882353));
#147097=CARTESIAN_POINT('Ctrl Pts',(40.5392751458362,-30.6138395280662,
-414.080698529412));
#147098=CARTESIAN_POINT('Ctrl Pts',(37.7024851496972,-34.3703565790883,
-415.574816176471));
#147099=CARTESIAN_POINT('Ctrl Pts',(34.2237386972451,-37.5416529948095,
-417.068933823529));
#147100=CARTESIAN_POINT('Ctrl Pts',(30.744992244793,-40.7129494105307,-418.563051470588));
#147101=CARTESIAN_POINT('Ctrl Pts',(26.7427538741697,-43.1910304950644,
-420.057169117647));
#147102=CARTESIAN_POINT('Ctrl Pts',(22.7405155035463,-45.6691115795981,
-421.551286764706));
#147103=CARTESIAN_POINT('Ctrl Pts',(18.3510766423074,-47.3695892537413,
-423.045404411765));
#147104=CARTESIAN_POINT('Ctrl Pts',(13.9616377810684,-49.0700669278844,
-424.539522058824));
#147105=CARTESIAN_POINT('Ctrl Pts',(9.33447550508176,-49.9350334639422,
-426.033639705882));
#147106=CARTESIAN_POINT('Ctrl Pts',(4.70731322909511,-50.8,-427.527757352941));
#147107=CARTESIAN_POINT('Ctrl Pts',(0.,-50.8,-429.021875));
#147108=CARTESIAN_POINT('Ctrl Pts',(-4.70731322909511,-50.8,-430.515992647059));
#147109=CARTESIAN_POINT('Ctrl Pts',(-9.33447550508177,-49.9350334639422,
-432.010110294118));
#147110=CARTESIAN_POINT('Ctrl Pts',(-13.9616377810684,-49.0700669278844,
-433.504227941177));
#147111=CARTESIAN_POINT('Ctrl Pts',(-18.3510766423074,-47.3695892537413,
-434.998345588235));
#147112=CARTESIAN_POINT('Ctrl Pts',(-22.7405155035463,-45.6691115795981,
-436.492463235294));
#147113=CARTESIAN_POINT('Ctrl Pts',(-26.7427538741697,-43.1910304950644,
-437.986580882353));
#147114=CARTESIAN_POINT('Ctrl Pts',(-30.744992244793,-40.7129494105307,
-439.480698529412));
#147115=CARTESIAN_POINT('Ctrl Pts',(-34.2237386972451,-37.5416529948095,
-440.974816176471));
#147116=CARTESIAN_POINT('Ctrl Pts',(-37.7024851496972,-34.3703565790883,
-442.46893382353));
#147117=CARTESIAN_POINT('Ctrl Pts',(-40.5392751458362,-30.6138395280662,
-443.963051470588));
#147118=CARTESIAN_POINT('Ctrl Pts',(-43.3760651419751,-26.8573224770441,
-445.457169117647));
#147119=CARTESIAN_POINT('Ctrl Pts',(-45.4742952008371,-22.6435084734481,
-446.951286764706));
#147120=CARTESIAN_POINT('Ctrl Pts',(-47.5725252596992,-18.4296944698521,
-448.445404411765));
#147121=CARTESIAN_POINT('Ctrl Pts',(-48.8607426731792,-13.9020798956618,
-449.939522058824));
#147122=CARTESIAN_POINT('Ctrl Pts',(-50.1489600866593,-9.37446532147148,
-451.433639705882));
#147123=CARTESIAN_POINT('Ctrl Pts',(-50.5832961557877,-4.68723266073574,
-452.927757352941));
#147124=CARTESIAN_POINT('Ctrl Pts',(-51.0176322249162,-3.12392900021603E-15,
-454.421875));
#147125=CARTESIAN_POINT('Ctrl Pts',(-50.5832961557877,4.68723266073573,
-455.915992647059));
#147126=CARTESIAN_POINT('Ctrl Pts',(-50.1489600866593,9.37446532147149,
-457.410110294118));
#147127=CARTESIAN_POINT('Ctrl Pts',(-48.8607426731792,13.9020798956618,
-458.904227941176));
#147128=CARTESIAN_POINT('Ctrl Pts',(-47.5725252596992,18.4296944698521,
-460.398345588235));
#147129=CARTESIAN_POINT('Ctrl Pts',(-45.4742952008371,22.6435084734481,
-461.892463235294));
#147130=CARTESIAN_POINT('Ctrl Pts',(-43.3760651419751,26.8573224770442,
-463.386580882353));
#147131=CARTESIAN_POINT('Ctrl Pts',(-40.5392751458362,30.6138395280662,
-464.880698529412));
#147132=CARTESIAN_POINT('Ctrl Pts',(-37.7024851496972,34.3703565790883,
-466.374816176471));
#147133=CARTESIAN_POINT('Ctrl Pts',(-34.2237386972451,37.5416529948095,
-467.868933823529));
#147134=CARTESIAN_POINT('Ctrl Pts',(-30.744992244793,40.7129494105307,-469.363051470588));
#147135=CARTESIAN_POINT('Ctrl Pts',(-26.7427538741697,43.1910304950644,
-470.857169117647));
#147136=CARTESIAN_POINT('Ctrl Pts',(-22.7405155035463,45.6691115795981,
-472.351286764706));
#147137=CARTESIAN_POINT('Ctrl Pts',(-18.3510766423074,47.3695892537413,
-473.845404411765));
#147138=CARTESIAN_POINT('Ctrl Pts',(-13.9616377810684,49.0700669278844,
-475.339522058823));
#147139=CARTESIAN_POINT('Ctrl Pts',(-9.33447550508177,49.9350334639422,
-476.833639705882));
#147140=CARTESIAN_POINT('Ctrl Pts',(-4.7073132290951,50.8,-478.327757352941));
#147141=CARTESIAN_POINT('Ctrl Pts',(-6.22120573966855E-15,50.8,-479.821875));
#147142=CARTESIAN_POINT('Ctrl Pts',(4.70731322909511,50.8,-481.315992647059));
#147143=CARTESIAN_POINT('Ctrl Pts',(9.33447550508176,49.9350334639422,-482.810110294118));
#147144=CARTESIAN_POINT('Ctrl Pts',(13.9616377810684,49.0700669278844,-484.304227941176));
#147145=CARTESIAN_POINT('Ctrl Pts',(18.3510766423074,47.3695892537413,-485.798345588235));
#147146=CARTESIAN_POINT('Ctrl Pts',(22.7405155035463,45.6691115795981,-487.292463235294));
#147147=CARTESIAN_POINT('Ctrl Pts',(26.7427538741697,43.1910304950644,-488.786580882353));
#147148=CARTESIAN_POINT('Ctrl Pts',(30.744992244793,40.7129494105307,-490.280698529412));
#147149=CARTESIAN_POINT('Ctrl Pts',(34.2237386972451,37.5416529948095,-491.774816176471));
#147150=CARTESIAN_POINT('Ctrl Pts',(37.7024851496972,34.3703565790883,-493.268933823529));
#147151=CARTESIAN_POINT('Ctrl Pts',(40.5392751458362,30.6138395280662,-494.763051470588));
#147152=CARTESIAN_POINT('Ctrl Pts',(43.3760651419751,26.8573224770442,-496.257169117647));
#147153=CARTESIAN_POINT('Ctrl Pts',(45.4742952008372,22.6435084734481,-497.751286764706));
#147154=CARTESIAN_POINT('Ctrl Pts',(47.5725252596992,18.4296944698521,-499.245404411765));
#147155=CARTESIAN_POINT('Ctrl Pts',(48.8607426731792,13.9020798956618,-500.739522058824));
#147156=CARTESIAN_POINT('Ctrl Pts',(50.1489600866593,9.37446532147146,-502.233639705883));
#147157=CARTESIAN_POINT('Ctrl Pts',(50.5832961557877,4.68723266073574,-503.727757352941));
#147158=CARTESIAN_POINT('Ctrl Pts',(51.0176322249162,9.37178700064808E-15,
-505.221875));
#147159=CARTESIAN_POINT('Ctrl Pts',(50.5832961557877,-4.68723266073572,
-506.715992647059));
#147160=CARTESIAN_POINT('Ctrl Pts',(50.1489600866593,-9.37446532147149,
-508.210110294117));
#147161=CARTESIAN_POINT('Ctrl Pts',(48.8607426731792,-13.9020798956618,
-509.704227941176));
#147162=CARTESIAN_POINT('Ctrl Pts',(47.5725252596992,-18.4296944698521,
-511.198345588235));
#147163=CARTESIAN_POINT('Ctrl Pts',(45.4742952008371,-22.6435084734482,
-512.692463235294));
#147164=CARTESIAN_POINT('Ctrl Pts',(43.3760651419751,-26.8573224770441,
-514.186580882353));
#147165=CARTESIAN_POINT('Ctrl Pts',(40.5392751458362,-30.6138395280662,
-515.680698529412));
#147166=CARTESIAN_POINT('Ctrl Pts',(37.7024851496972,-34.3703565790883,
-517.174816176471));
#147167=CARTESIAN_POINT('Ctrl Pts',(34.2237386972451,-37.5416529948095,
-518.66893382353));
#147168=CARTESIAN_POINT('Ctrl Pts',(30.744992244793,-40.7129494105307,-520.163051470588));
#147169=CARTESIAN_POINT('Ctrl Pts',(26.7427538741697,-43.1910304950644,
-521.657169117647));
#147170=CARTESIAN_POINT('Ctrl Pts',(22.7405155035463,-45.6691115795981,
-523.151286764706));
#147171=CARTESIAN_POINT('Ctrl Pts',(18.3510766423074,-47.3695892537413,
-524.645404411765));
#147172=CARTESIAN_POINT('Ctrl Pts',(13.9616377810684,-49.0700669278844,
-526.139522058823));
#147173=CARTESIAN_POINT('Ctrl Pts',(9.33447550508176,-49.9350334639422,
-527.633639705882));
#147174=CARTESIAN_POINT('Ctrl Pts',(4.70731322909511,-50.8,-529.127757352941));
#147175=CARTESIAN_POINT('Ctrl Pts',(0.,-50.8,-530.621875));
#147176=CARTESIAN_POINT('Ctrl Pts',(-4.70731322909511,-50.8,-532.115992647059));
#147177=CARTESIAN_POINT('Ctrl Pts',(-9.33447550508177,-49.9350334639422,
-533.610110294118));
#147178=CARTESIAN_POINT('Ctrl Pts',(-13.9616377810684,-49.0700669278844,
-535.104227941177));
#147179=CARTESIAN_POINT('Ctrl Pts',(-18.3510766423074,-47.3695892537413,
-536.598345588235));
#147180=CARTESIAN_POINT('Ctrl Pts',(-22.7405155035463,-45.6691115795981,
-538.092463235294));
#147181=CARTESIAN_POINT('Ctrl Pts',(-26.7427538741697,-43.1910304950644,
-539.586580882353));
#147182=CARTESIAN_POINT('Ctrl Pts',(-30.744992244793,-40.7129494105307,
-541.080698529412));
#147183=CARTESIAN_POINT('Ctrl Pts',(-34.2237386972451,-37.5416529948095,
-542.574816176471));
#147184=CARTESIAN_POINT('Ctrl Pts',(-37.7024851496972,-34.3703565790883,
-544.068933823529));
#147185=CARTESIAN_POINT('Ctrl Pts',(-40.5392751458362,-30.6138395280662,
-545.563051470588));
#147186=CARTESIAN_POINT('Ctrl Pts',(-43.3760651419751,-26.8573224770441,
-547.057169117647));
#147187=CARTESIAN_POINT('Ctrl Pts',(-45.4742952008371,-22.6435084734481,
-548.551286764706));
#147188=CARTESIAN_POINT('Ctrl Pts',(-47.5725252596992,-18.4296944698521,
-550.045404411765));
#147189=CARTESIAN_POINT('Ctrl Pts',(-48.8607426731792,-13.9020798956618,
-551.539522058823));
#147190=CARTESIAN_POINT('Ctrl Pts',(-50.1489600866593,-9.37446532147148,
-553.033639705882));
#147191=CARTESIAN_POINT('Ctrl Pts',(-50.5832961557877,-4.68723266073574,
-554.527757352941));
#147192=CARTESIAN_POINT('Ctrl Pts',(-51.0176322249162,-3.12392900021603E-15,
-556.021875));
#147193=CARTESIAN_POINT('Ctrl Pts',(-50.5832961557877,4.68723266073573,
-557.515992647059));
#147194=CARTESIAN_POINT('Ctrl Pts',(-50.1489600866593,9.37446532147149,
-559.010110294118));
#147195=CARTESIAN_POINT('Ctrl Pts',(-48.8607426731792,13.9020798956618,
-560.504227941177));
#147196=CARTESIAN_POINT('Ctrl Pts',(-47.5725252596992,18.4296944698521,
-561.998345588236));
#147197=CARTESIAN_POINT('Ctrl Pts',(-45.4742952008371,22.6435084734481,
-563.492463235294));
#147198=CARTESIAN_POINT('Ctrl Pts',(-43.3760651419751,26.8573224770442,
-564.986580882353));
#147199=CARTESIAN_POINT('Ctrl Pts',(-40.5392751458362,30.6138395280662,
-566.480698529411));
#147200=CARTESIAN_POINT('Ctrl Pts',(-37.7024851496972,34.3703565790883,
-567.974816176471));
#147201=CARTESIAN_POINT('Ctrl Pts',(-34.2237386972451,37.5416529948095,
-569.468933823529));
#147202=CARTESIAN_POINT('Ctrl Pts',(-30.744992244793,40.7129494105307,-570.963051470588));
#147203=CARTESIAN_POINT('Ctrl Pts',(-26.7427538741697,43.1910304950644,
-572.457169117647));
#147204=CARTESIAN_POINT('Ctrl Pts',(-22.7405155035463,45.6691115795981,
-573.951286764706));
#147205=CARTESIAN_POINT('Ctrl Pts',(-18.3510766423074,47.3695892537413,
-575.445404411765));
#147206=CARTESIAN_POINT('Ctrl Pts',(-13.9616377810684,49.0700669278844,
-576.939522058824));
#147207=CARTESIAN_POINT('Ctrl Pts',(-9.33447550508177,49.9350334639422,
-578.433639705882));
#147208=CARTESIAN_POINT('Ctrl Pts',(-4.7073132290951,50.8,-579.927757352941));
#147209=CARTESIAN_POINT('Ctrl Pts',(-6.22120573966855E-15,50.8,-581.421875));
#147210=CARTESIAN_POINT('Ctrl Pts',(4.70731322909511,50.8,-582.915992647059));
#147211=CARTESIAN_POINT('Ctrl Pts',(9.33447550508176,49.9350334639422,-584.410110294118));
#147212=CARTESIAN_POINT('Ctrl Pts',(13.9616377810684,49.0700669278844,-585.904227941176));
#147213=CARTESIAN_POINT('Ctrl Pts',(18.3510766423074,47.3695892537413,-587.398345588235));
#147214=CARTESIAN_POINT('Ctrl Pts',(22.7405155035463,45.6691115795981,-588.892463235294));
#147215=CARTESIAN_POINT('Ctrl Pts',(26.7427538741697,43.1910304950644,-590.386580882353));
#147216=CARTESIAN_POINT('Ctrl Pts',(30.744992244793,40.7129494105307,-591.880698529412));
#147217=CARTESIAN_POINT('Ctrl Pts',(34.2237386972451,37.5416529948095,-593.374816176471));
#147218=CARTESIAN_POINT('Ctrl Pts',(37.7024851496972,34.3703565790883,-594.86893382353));
#147219=CARTESIAN_POINT('Ctrl Pts',(40.5392751458362,30.6138395280662,-596.363051470588));
#147220=CARTESIAN_POINT('Ctrl Pts',(43.3760651419751,26.8573224770442,-597.857169117647));
#147221=CARTESIAN_POINT('Ctrl Pts',(45.4742952008372,22.6435084734481,-599.351286764706));
#147222=CARTESIAN_POINT('Ctrl Pts',(47.5725252596992,18.4296944698521,-600.845404411765));
#147223=CARTESIAN_POINT('Ctrl Pts',(48.8607426731792,13.9020798956618,-602.339522058823));
#147224=CARTESIAN_POINT('Ctrl Pts',(50.1489600866593,9.37446532147146,-603.833639705882));
#147225=CARTESIAN_POINT('Ctrl Pts',(50.5832961557877,4.68723266073574,-605.327757352941));
#147226=CARTESIAN_POINT('Ctrl Pts',(51.0176322249162,9.37178700064808E-15,
-606.821875));
#147227=CARTESIAN_POINT('Ctrl Pts',(50.5832961557877,-4.68723266073572,
-608.315992647059));
#147228=CARTESIAN_POINT('Ctrl Pts',(50.1489600866593,-9.37446532147149,
-609.810110294118));
#147229=CARTESIAN_POINT('Ctrl Pts',(48.8607426731792,-13.9020798956618,
-611.304227941176));
#147230=CARTESIAN_POINT('Ctrl Pts',(47.5725252596992,-18.4296944698521,
-612.798345588235));
#147231=CARTESIAN_POINT('Ctrl Pts',(45.4742952008371,-22.6435084734482,
-614.292463235294));
#147232=CARTESIAN_POINT('Ctrl Pts',(43.3760651419751,-26.8573224770441,
-615.786580882353));
#147233=CARTESIAN_POINT('Ctrl Pts',(40.5392751458362,-30.6138395280662,
-617.280698529412));
#147234=CARTESIAN_POINT('Ctrl Pts',(37.7024851496972,-34.3703565790883,
-618.774816176471));
#147235=CARTESIAN_POINT('Ctrl Pts',(34.2237386972451,-37.5416529948095,
-620.268933823529));
#147236=CARTESIAN_POINT('Ctrl Pts',(30.744992244793,-40.7129494105307,-621.763051470588));
#147237=CARTESIAN_POINT('Ctrl Pts',(26.7427538741697,-43.1910304950644,
-623.257169117647));
#147238=CARTESIAN_POINT('Ctrl Pts',(22.7405155035463,-45.6691115795981,
-624.751286764706));
#147239=CARTESIAN_POINT('Ctrl Pts',(18.3510766423074,-47.3695892537413,
-626.245404411764));
#147240=CARTESIAN_POINT('Ctrl Pts',(13.9616377810684,-49.0700669278844,
-627.739522058823));
#147241=CARTESIAN_POINT('Ctrl Pts',(9.33447550508176,-49.9350334639422,
-629.233639705882));
#147242=CARTESIAN_POINT('Ctrl Pts',(4.70731322909511,-50.8,-630.727757352941));
#147243=CARTESIAN_POINT('Ctrl Pts',(0.,-50.8,-632.221875));
#147244=CARTESIAN_POINT('Ctrl Pts',(-4.70731322909511,-50.8,-633.715992647059));
#147245=CARTESIAN_POINT('Ctrl Pts',(-9.33447550508177,-49.9350334639422,
-635.210110294118));
#147246=CARTESIAN_POINT('Ctrl Pts',(-13.9616377810684,-49.0700669278844,
-636.704227941177));
#147247=CARTESIAN_POINT('Ctrl Pts',(-18.3510766423074,-47.3695892537413,
-638.198345588235));
#147248=CARTESIAN_POINT('Ctrl Pts',(-22.7405155035463,-45.6691115795981,
-639.692463235294));
#147249=CARTESIAN_POINT('Ctrl Pts',(-26.7427538741697,-43.1910304950644,
-641.186580882353));
#147250=CARTESIAN_POINT('Ctrl Pts',(-30.744992244793,-40.7129494105307,
-642.680698529412));
#147251=CARTESIAN_POINT('Ctrl Pts',(-34.2237386972451,-37.5416529948095,
-644.174816176471));
#147252=CARTESIAN_POINT('Ctrl Pts',(-37.7024851496972,-34.3703565790883,
-645.668933823529));
#147253=CARTESIAN_POINT('Ctrl Pts',(-40.5392751458362,-30.6138395280662,
-647.163051470588));
#147254=CARTESIAN_POINT('Ctrl Pts',(-43.3760651419751,-26.8573224770441,
-648.657169117647));
#147255=CARTESIAN_POINT('Ctrl Pts',(-45.4742952008371,-22.6435084734481,
-650.151286764706));
#147256=CARTESIAN_POINT('Ctrl Pts',(-47.5725252596992,-18.4296944698521,
-651.645404411765));
#147257=CARTESIAN_POINT('Ctrl Pts',(-48.8607426731792,-13.9020798956618,
-653.139522058824));
#147258=CARTESIAN_POINT('Ctrl Pts',(-50.1489600866593,-9.37446532147148,
-654.633639705883));
#147259=CARTESIAN_POINT('Ctrl Pts',(-50.5832961557877,-4.68723266073574,
-656.127757352941));
#147260=CARTESIAN_POINT('Ctrl Pts',(-51.0176322249162,-3.12392900021603E-15,
-657.621875));
#147261=CARTESIAN_POINT('Ctrl Pts',(-50.5832961557877,4.68723266073573,
-659.115992647059));
#147262=CARTESIAN_POINT('Ctrl Pts',(-50.1489600866593,9.37446532147149,
-660.610110294118));
#147263=CARTESIAN_POINT('Ctrl Pts',(-48.8607426731792,13.9020798956618,
-662.104227941177));
#147264=CARTESIAN_POINT('Ctrl Pts',(-47.5725252596992,18.4296944698521,
-663.598345588235));
#147265=CARTESIAN_POINT('Ctrl Pts',(-45.4742952008371,22.6435084734481,
-665.092463235294));
#147266=CARTESIAN_POINT('Ctrl Pts',(-43.3760651419751,26.8573224770442,
-666.586580882353));
#147267=CARTESIAN_POINT('Ctrl Pts',(-40.5392751458362,30.6138395280662,
-668.080698529412));
#147268=CARTESIAN_POINT('Ctrl Pts',(-37.7024851496972,34.3703565790883,
-669.574816176471));
#147269=CARTESIAN_POINT('Ctrl Pts',(-34.2237386972451,37.5416529948095,
-671.068933823529));
#147270=CARTESIAN_POINT('Ctrl Pts',(-30.744992244793,40.7129494105307,-672.563051470588));
#147271=CARTESIAN_POINT('Ctrl Pts',(-26.7427538741697,43.1910304950644,
-674.057169117647));
#147272=CARTESIAN_POINT('Ctrl Pts',(-22.7405155035463,45.6691115795981,
-675.551286764706));
#147273=CARTESIAN_POINT('Ctrl Pts',(-18.3510766423074,47.3695892537413,
-677.045404411765));
#147274=CARTESIAN_POINT('Ctrl Pts',(-13.9616377810684,49.0700669278844,
-678.539522058824));
#147275=CARTESIAN_POINT('Ctrl Pts',(-9.33447550508177,49.9350334639422,
-680.033639705882));
#147276=CARTESIAN_POINT('Ctrl Pts',(-4.7073132290951,50.8,-681.527757352941));
#147277=CARTESIAN_POINT('Ctrl Pts',(-6.22120573966855E-15,50.8,-683.021875));
#147278=CARTESIAN_POINT('Ctrl Pts',(4.70731322909511,50.8,-684.515992647059));
#147279=CARTESIAN_POINT('Ctrl Pts',(9.33447550508176,49.9350334639422,-686.010110294118));
#147280=CARTESIAN_POINT('Ctrl Pts',(13.9616377810684,49.0700669278844,-687.504227941176));
#147281=CARTESIAN_POINT('Ctrl Pts',(18.3510766423074,47.3695892537413,-688.998345588235));
#147282=CARTESIAN_POINT('Ctrl Pts',(22.7405155035463,45.6691115795981,-690.492463235294));
#147283=CARTESIAN_POINT('Ctrl Pts',(26.7427538741697,43.1910304950644,-691.986580882353));
#147284=CARTESIAN_POINT('Ctrl Pts',(30.744992244793,40.7129494105307,-693.480698529412));
#147285=CARTESIAN_POINT('Ctrl Pts',(34.2237386972451,37.5416529948095,-694.974816176471));
#147286=CARTESIAN_POINT('Ctrl Pts',(37.7024851496972,34.3703565790883,-696.46893382353));
#147287=CARTESIAN_POINT('Ctrl Pts',(40.5392751458362,30.6138395280662,-697.963051470588));
#147288=CARTESIAN_POINT('Ctrl Pts',(43.3760651419751,26.8573224770442,-699.457169117647));
#147289=CARTESIAN_POINT('Ctrl Pts',(45.4742952008372,22.6435084734481,-700.951286764706));
#147290=CARTESIAN_POINT('Ctrl Pts',(47.5725252596992,18.4296944698521,-702.445404411765));
#147291=CARTESIAN_POINT('Ctrl Pts',(48.8607426731792,13.9020798956618,-703.939522058823));
#147292=CARTESIAN_POINT('Ctrl Pts',(50.1489600866593,9.37446532147146,-705.433639705882));
#147293=CARTESIAN_POINT('Ctrl Pts',(50.5832961557877,4.68723266073574,-706.927757352941));
#147294=CARTESIAN_POINT('Ctrl Pts',(51.0176322249162,9.37178700064808E-15,
-708.421875));
#147295=CARTESIAN_POINT('Ctrl Pts',(50.5832961557877,-4.68723266073572,
-709.915992647059));
#147296=CARTESIAN_POINT('Ctrl Pts',(50.1489600866593,-9.37446532147149,
-711.410110294118));
#147297=CARTESIAN_POINT('Ctrl Pts',(48.8607426731792,-13.9020798956618,
-712.904227941177));
#147298=CARTESIAN_POINT('Ctrl Pts',(47.5725252596992,-18.4296944698521,
-714.398345588236));
#147299=CARTESIAN_POINT('Ctrl Pts',(45.4742952008371,-22.6435084734482,
-715.892463235294));
#147300=CARTESIAN_POINT('Ctrl Pts',(43.3760651419751,-26.8573224770441,
-717.386580882353));
#147301=CARTESIAN_POINT('Ctrl Pts',(40.5392751458362,-30.6138395280662,
-718.880698529412));
#147302=CARTESIAN_POINT('Ctrl Pts',(37.7024851496972,-34.3703565790883,
-720.374816176471));
#147303=CARTESIAN_POINT('Ctrl Pts',(34.2237386972451,-37.5416529948095,
-721.868933823529));
#147304=CARTESIAN_POINT('Ctrl Pts',(30.744992244793,-40.7129494105307,-723.363051470588));
#147305=CARTESIAN_POINT('Ctrl Pts',(26.7427538741697,-43.1910304950644,
-724.857169117647));
#147306=CARTESIAN_POINT('Ctrl Pts',(22.7405155035463,-45.6691115795981,
-726.351286764706));
#147307=CARTESIAN_POINT('Ctrl Pts',(18.3510766423074,-47.3695892537413,
-727.845404411765));
#147308=CARTESIAN_POINT('Ctrl Pts',(13.9616377810684,-49.0700669278844,
-729.339522058824));
#147309=CARTESIAN_POINT('Ctrl Pts',(9.33447550508176,-49.9350334639422,
-730.833639705882));
#147310=CARTESIAN_POINT('Ctrl Pts',(4.70731322909511,-50.8,-732.327757352941));
#147311=CARTESIAN_POINT('Ctrl Pts',(0.,-50.8,-733.821875));
#147312=CARTESIAN_POINT('Ctrl Pts',(-4.70731322909511,-50.8,-735.315992647059));
#147313=CARTESIAN_POINT('Ctrl Pts',(-9.33447550508177,-49.9350334639422,
-736.810110294118));
#147314=CARTESIAN_POINT('Ctrl Pts',(-13.9616377810684,-49.0700669278844,
-738.304227941177));
#147315=CARTESIAN_POINT('Ctrl Pts',(-18.3510766423074,-47.3695892537413,
-739.798345588235));
#147316=CARTESIAN_POINT('Ctrl Pts',(-22.7405155035463,-45.6691115795981,
-741.292463235294));
#147317=CARTESIAN_POINT('Ctrl Pts',(-26.7427538741697,-43.1910304950644,
-742.786580882353));
#147318=CARTESIAN_POINT('Ctrl Pts',(-30.744992244793,-40.7129494105307,
-744.280698529412));
#147319=CARTESIAN_POINT('Ctrl Pts',(-34.2237386972451,-37.5416529948095,
-745.77481617647));
#147320=CARTESIAN_POINT('Ctrl Pts',(-37.7024851496972,-34.3703565790883,
-747.268933823529));
#147321=CARTESIAN_POINT('Ctrl Pts',(-40.5392751458362,-30.6138395280662,
-748.763051470588));
#147322=CARTESIAN_POINT('Ctrl Pts',(-43.3760651419751,-26.8573224770441,
-750.257169117647));
#147323=CARTESIAN_POINT('Ctrl Pts',(-45.4742952008371,-22.6435084734481,
-751.751286764706));
#147324=CARTESIAN_POINT('Ctrl Pts',(-47.5725252596992,-18.4296944698521,
-753.245404411765));
#147325=CARTESIAN_POINT('Ctrl Pts',(-48.8607426731792,-13.9020798956618,
-754.739522058824));
#147326=CARTESIAN_POINT('Ctrl Pts',(-50.1489600866593,-9.37446532147148,
-756.233639705882));
#147327=CARTESIAN_POINT('Ctrl Pts',(-50.5832961557877,-4.68723266073574,
-757.727757352941));
#147328=CARTESIAN_POINT('Ctrl Pts',(-51.0176322249162,-3.12392900021603E-15,
-759.221875000001));
#147329=CARTESIAN_POINT('Ctrl Pts',(-50.5832961557877,4.68723266073573,
-760.715992647059));
#147330=CARTESIAN_POINT('Ctrl Pts',(-50.1489600866593,9.37446532147149,
-762.210110294118));
#147331=CARTESIAN_POINT('Ctrl Pts',(-48.8607426731792,13.9020798956618,
-763.704227941176));
#147332=CARTESIAN_POINT('Ctrl Pts',(-47.5725252596992,18.4296944698521,
-765.198345588235));
#147333=CARTESIAN_POINT('Ctrl Pts',(-45.4742952008371,22.6435084734481,
-766.692463235294));
#147334=CARTESIAN_POINT('Ctrl Pts',(-43.3760651419751,26.8573224770442,
-768.186580882353));
#147335=CARTESIAN_POINT('Ctrl Pts',(-40.5392751458362,30.6138395280662,
-769.680698529412));
#147336=CARTESIAN_POINT('Ctrl Pts',(-37.7024851496972,34.3703565790883,
-771.174816176471));
#147337=CARTESIAN_POINT('Ctrl Pts',(-34.2237386972451,37.5416529948095,
-772.66893382353));
#147338=CARTESIAN_POINT('Ctrl Pts',(-30.744992244793,40.7129494105307,-774.163051470589));
#147339=CARTESIAN_POINT('Ctrl Pts',(-26.7427538741697,43.1910304950644,
-775.657169117647));
#147340=CARTESIAN_POINT('Ctrl Pts',(-22.7405155035463,45.6691115795981,
-777.151286764706));
#147341=CARTESIAN_POINT('Ctrl Pts',(-18.3510766423074,47.3695892537413,
-778.645404411765));
#147342=CARTESIAN_POINT('Ctrl Pts',(-13.9616377810684,49.0700669278844,
-780.139522058824));
#147343=CARTESIAN_POINT('Ctrl Pts',(-9.33447550508177,49.9350334639422,
-781.633639705882));
#147344=CARTESIAN_POINT('Ctrl Pts',(-4.7073132290951,50.8,-783.127757352941));
#147345=CARTESIAN_POINT('Ctrl Pts',(-6.22120573966855E-15,50.8,-784.621875));
#147346=CARTESIAN_POINT('Ctrl Pts',(4.70731322909511,50.8,-786.115992647059));
#147347=CARTESIAN_POINT('Ctrl Pts',(9.33447550508176,49.9350334639422,-787.610110294118));
#147348=CARTESIAN_POINT('Ctrl Pts',(13.9616377810684,49.0700669278844,-789.104227941177));
#147349=CARTESIAN_POINT('Ctrl Pts',(18.3510766423074,47.3695892537413,-790.598345588235));
#147350=CARTESIAN_POINT('Ctrl Pts',(22.7405155035463,45.6691115795981,-792.092463235294));
#147351=CARTESIAN_POINT('Ctrl Pts',(26.7427538741697,43.1910304950644,-793.586580882353));
#147352=CARTESIAN_POINT('Ctrl Pts',(30.744992244793,40.7129494105307,-795.080698529412));
#147353=CARTESIAN_POINT('Ctrl Pts',(34.2237386972451,37.5416529948095,-796.574816176471));
#147354=CARTESIAN_POINT('Ctrl Pts',(37.7024851496972,34.3703565790883,-798.068933823529));
#147355=CARTESIAN_POINT('Ctrl Pts',(40.5392751458362,30.6138395280662,-799.563051470588));
#147356=CARTESIAN_POINT('Ctrl Pts',(43.3760651419751,26.8573224770442,-801.057169117647));
#147357=CARTESIAN_POINT('Ctrl Pts',(45.4742952008372,22.6435084734481,-802.551286764706));
#147358=CARTESIAN_POINT('Ctrl Pts',(47.5725252596992,18.4296944698521,-804.045404411765));
#147359=CARTESIAN_POINT('Ctrl Pts',(48.8607426731792,13.9020798956618,-805.539522058823));
#147360=CARTESIAN_POINT('Ctrl Pts',(50.1489600866593,9.37446532147146,-807.033639705882));
#147361=CARTESIAN_POINT('Ctrl Pts',(50.5832961557877,4.68723266073574,-808.527757352941));
#147362=CARTESIAN_POINT('Ctrl Pts',(51.0176322249162,9.37178700064808E-15,
-810.021875));
#147363=CARTESIAN_POINT('Ctrl Pts',(50.5832961557877,-4.68723266073572,
-811.515992647059));
#147364=CARTESIAN_POINT('Ctrl Pts',(50.1489600866593,-9.37446532147149,
-813.010110294118));
#147365=CARTESIAN_POINT('Ctrl Pts',(48.8607426731792,-13.9020798956618,
-814.504227941177));
#147366=CARTESIAN_POINT('Ctrl Pts',(47.5725252596992,-18.4296944698521,
-815.998345588235));
#147367=CARTESIAN_POINT('Ctrl Pts',(45.4742952008371,-22.6435084734482,
-817.492463235294));
#147368=CARTESIAN_POINT('Ctrl Pts',(43.3760651419751,-26.8573224770441,
-818.986580882353));
#147369=CARTESIAN_POINT('Ctrl Pts',(40.5392751458362,-30.6138395280662,
-820.480698529411));
#147370=CARTESIAN_POINT('Ctrl Pts',(37.7024851496972,-34.3703565790883,
-821.97481617647));
#147371=CARTESIAN_POINT('Ctrl Pts',(34.2237386972451,-37.5416529948095,
-823.468933823529));
#147372=CARTESIAN_POINT('Ctrl Pts',(30.744992244793,-40.7129494105307,-824.963051470588));
#147373=CARTESIAN_POINT('Ctrl Pts',(26.7427538741697,-43.1910304950644,
-826.457169117647));
#147374=CARTESIAN_POINT('Ctrl Pts',(22.7405155035463,-45.6691115795981,
-827.951286764706));
#147375=CARTESIAN_POINT('Ctrl Pts',(18.3510766423074,-47.3695892537413,
-829.445404411765));
#147376=CARTESIAN_POINT('Ctrl Pts',(13.9616377810684,-49.0700669278844,
-830.939522058824));
#147377=CARTESIAN_POINT('Ctrl Pts',(9.33447550508176,-49.9350334639422,
-832.433639705882));
#147378=CARTESIAN_POINT('Ctrl Pts',(4.70731322909511,-50.8,-833.927757352942));
#147379=CARTESIAN_POINT('Ctrl Pts',(0.,-50.8,-835.421875));
#147380=CARTESIAN_POINT('Ctrl Pts',(-4.70731322909511,-50.8,-836.915992647059));
#147381=CARTESIAN_POINT('Ctrl Pts',(-9.33447550508177,-49.9350334639422,
-838.410110294118));
#147382=CARTESIAN_POINT('Ctrl Pts',(-13.9616377810684,-49.0700669278844,
-839.904227941177));
#147383=CARTESIAN_POINT('Ctrl Pts',(-18.3510766423074,-47.3695892537413,
-841.398345588235));
#147384=CARTESIAN_POINT('Ctrl Pts',(-22.7405155035463,-45.6691115795981,
-842.892463235294));
#147385=CARTESIAN_POINT('Ctrl Pts',(-26.7427538741697,-43.1910304950644,
-844.386580882353));
#147386=CARTESIAN_POINT('Ctrl Pts',(-30.744992244793,-40.7129494105307,
-845.880698529412));
#147387=CARTESIAN_POINT('Ctrl Pts',(-34.2237386972451,-37.5416529948095,
-847.374816176471));
#147388=CARTESIAN_POINT('Ctrl Pts',(-37.7024851496972,-34.3703565790883,
-848.86893382353));
#147389=CARTESIAN_POINT('Ctrl Pts',(-40.5392751458362,-30.6138395280662,
-850.363051470588));
#147390=CARTESIAN_POINT('Ctrl Pts',(-43.3760651419751,-26.8573224770441,
-851.857169117647));
#147391=CARTESIAN_POINT('Ctrl Pts',(-45.4742952008371,-22.6435084734481,
-853.351286764706));
#147392=CARTESIAN_POINT('Ctrl Pts',(-47.5725252596992,-18.4296944698521,
-854.845404411765));
#147393=CARTESIAN_POINT('Ctrl Pts',(-48.8607426731792,-13.9020798956618,
-856.339522058823));
#147394=CARTESIAN_POINT('Ctrl Pts',(-50.1489600866593,-9.37446532147148,
-857.833639705882));
#147395=CARTESIAN_POINT('Ctrl Pts',(-50.5832961557877,-4.68723266073574,
-859.327757352941));
#147396=CARTESIAN_POINT('Ctrl Pts',(-51.0176322249162,-3.12392900021603E-15,
-860.821875));
#147397=CARTESIAN_POINT('Ctrl Pts',(-50.5832961557877,4.68723266073573,
-862.315992647059));
#147398=CARTESIAN_POINT('Ctrl Pts',(-50.1489600866593,9.37446532147149,
-863.810110294118));
#147399=CARTESIAN_POINT('Ctrl Pts',(-48.8607426731792,13.9020798956618,
-865.304227941176));
#147400=CARTESIAN_POINT('Ctrl Pts',(-47.5725252596992,18.4296944698521,
-866.798345588235));
#147401=CARTESIAN_POINT('Ctrl Pts',(-45.4742952008371,22.6435084734481,
-868.292463235294));
#147402=CARTESIAN_POINT('Ctrl Pts',(-43.3760651419751,26.8573224770442,
-869.786580882353));
#147403=CARTESIAN_POINT('Ctrl Pts',(-40.5392751458362,30.6138395280662,
-871.280698529412));
#147404=CARTESIAN_POINT('Ctrl Pts',(-37.7024851496972,34.3703565790883,
-872.774816176471));
#147405=CARTESIAN_POINT('Ctrl Pts',(-34.2237386972451,37.5416529948095,
-874.268933823529));
#147406=CARTESIAN_POINT('Ctrl Pts',(-30.744992244793,40.7129494105307,-875.763051470589));
#147407=CARTESIAN_POINT('Ctrl Pts',(-26.7427538741697,43.1910304950644,
-877.257169117647));
#147408=CARTESIAN_POINT('Ctrl Pts',(-22.7405155035463,45.6691115795981,
-878.751286764706));
#147409=CARTESIAN_POINT('Ctrl Pts',(-18.3510766423074,47.3695892537413,
-880.245404411764));
#147410=CARTESIAN_POINT('Ctrl Pts',(-13.9616377810684,49.0700669278844,
-881.739522058823));
#147411=CARTESIAN_POINT('Ctrl Pts',(-9.33447550508177,49.9350334639422,
-883.233639705882));
#147412=CARTESIAN_POINT('Ctrl Pts',(-4.7073132290951,50.8,-884.727757352941));
#147413=CARTESIAN_POINT('Ctrl Pts',(-6.22120573966855E-15,50.8,-886.221875));
#147414=CARTESIAN_POINT('Ctrl Pts',(4.70731322909511,50.8,-887.715992647059));
#147415=CARTESIAN_POINT('Ctrl Pts',(9.33447550508176,49.9350334639422,-889.210110294118));
#147416=CARTESIAN_POINT('Ctrl Pts',(13.9616377810684,49.0700669278844,-890.704227941177));
#147417=CARTESIAN_POINT('Ctrl Pts',(18.3510766423074,47.3695892537413,-892.198345588235));
#147418=CARTESIAN_POINT('Ctrl Pts',(22.7405155035463,45.6691115795981,-893.692463235295));
#147419=CARTESIAN_POINT('Ctrl Pts',(26.7427538741697,43.1910304950644,-895.186580882353));
#147420=CARTESIAN_POINT('Ctrl Pts',(30.744992244793,40.7129494105307,-896.680698529412));
#147421=CARTESIAN_POINT('Ctrl Pts',(34.2237386972451,37.5416529948095,-898.17481617647));
#147422=CARTESIAN_POINT('Ctrl Pts',(37.7024851496972,34.3703565790883,-899.66893382353));
#147423=CARTESIAN_POINT('Ctrl Pts',(40.5392751458362,30.6138395280662,-901.163051470588));
#147424=CARTESIAN_POINT('Ctrl Pts',(43.3760651419751,26.8573224770442,-902.657169117647));
#147425=CARTESIAN_POINT('Ctrl Pts',(45.4742952008372,22.6435084734481,-904.151286764706));
#147426=CARTESIAN_POINT('Ctrl Pts',(47.5725252596992,18.4296944698521,-905.645404411765));
#147427=CARTESIAN_POINT('Ctrl Pts',(48.8607426731792,13.9020798956618,-907.139522058824));
#147428=CARTESIAN_POINT('Ctrl Pts',(50.1489600866593,9.37446532147146,-908.633639705883));
#147429=CARTESIAN_POINT('Ctrl Pts',(50.5832961557877,4.68723266073574,-910.127757352941));
#147430=CARTESIAN_POINT('Ctrl Pts',(51.0176322249162,9.37178700064808E-15,
-911.621875));
#147431=CARTESIAN_POINT('Ctrl Pts',(50.5832961557877,-4.68723266073572,
-913.115992647059));
#147432=CARTESIAN_POINT('Ctrl Pts',(50.1489600866593,-9.37446532147149,
-914.610110294118));
#147433=CARTESIAN_POINT('Ctrl Pts',(48.8607426731792,-13.9020798956618,
-916.104227941177));
#147434=CARTESIAN_POINT('Ctrl Pts',(47.5725252596992,-18.4296944698521,
-917.598345588235));
#147435=CARTESIAN_POINT('Ctrl Pts',(45.4742952008371,-22.6435084734482,
-919.092463235294));
#147436=CARTESIAN_POINT('Ctrl Pts',(43.3760651419751,-26.8573224770441,
-920.586580882353));
#147437=CARTESIAN_POINT('Ctrl Pts',(40.5392751458362,-30.6138395280662,
-922.080698529412));
#147438=CARTESIAN_POINT('Ctrl Pts',(37.7024851496972,-34.3703565790883,
-923.574816176471));
#147439=CARTESIAN_POINT('Ctrl Pts',(34.2237386972451,-37.5416529948095,
-925.068933823529));
#147440=CARTESIAN_POINT('Ctrl Pts',(30.744992244793,-40.7129494105307,-926.563051470588));
#147441=CARTESIAN_POINT('Ctrl Pts',(26.7427538741697,-43.1910304950644,
-928.057169117647));
#147442=CARTESIAN_POINT('Ctrl Pts',(22.7405155035463,-45.6691115795981,
-929.551286764706));
#147443=CARTESIAN_POINT('Ctrl Pts',(18.3510766423074,-47.3695892537413,
-931.045404411765));
#147444=CARTESIAN_POINT('Ctrl Pts',(13.9616377810684,-49.0700669278844,
-932.539522058824));
#147445=CARTESIAN_POINT('Ctrl Pts',(9.33447550508176,-49.9350334639422,
-934.033639705882));
#147446=CARTESIAN_POINT('Ctrl Pts',(4.70731322909511,-50.8,-935.527757352942));
#147447=CARTESIAN_POINT('Ctrl Pts',(0.,-50.8,-937.021875));
#147448=CARTESIAN_POINT('Ctrl Pts',(-4.70731322909511,-50.8,-938.515992647059));
#147449=CARTESIAN_POINT('Ctrl Pts',(-9.33447550508177,-49.9350334639422,
-940.010110294118));
#147450=CARTESIAN_POINT('Ctrl Pts',(-13.9616377810684,-49.0700669278844,
-941.504227941176));
#147451=CARTESIAN_POINT('Ctrl Pts',(-18.3510766423074,-47.3695892537413,
-942.998345588235));
#147452=CARTESIAN_POINT('Ctrl Pts',(-22.7405155035463,-45.6691115795981,
-944.492463235294));
#147453=CARTESIAN_POINT('Ctrl Pts',(-26.7427538741697,-43.1910304950644,
-945.986580882353));
#147454=CARTESIAN_POINT('Ctrl Pts',(-30.744992244793,-40.7129494105307,
-947.480698529412));
#147455=CARTESIAN_POINT('Ctrl Pts',(-34.2237386972451,-37.5416529948095,
-948.974816176471));
#147456=CARTESIAN_POINT('Ctrl Pts',(-37.7024851496972,-34.3703565790883,
-950.46893382353));
#147457=CARTESIAN_POINT('Ctrl Pts',(-40.5392751458362,-30.6138395280662,
-951.963051470588));
#147458=CARTESIAN_POINT('Ctrl Pts',(-43.3760651419751,-26.8573224770441,
-953.457169117647));
#147459=CARTESIAN_POINT('Ctrl Pts',(-45.4742952008371,-22.6435084734481,
-954.951286764706));
#147460=CARTESIAN_POINT('Ctrl Pts',(-47.5725252596992,-18.4296944698521,
-956.445404411765));
#147461=CARTESIAN_POINT('Ctrl Pts',(-48.8607426731792,-13.9020798956618,
-957.939522058824));
#147462=CARTESIAN_POINT('Ctrl Pts',(-50.1489600866593,-9.37446532147148,
-959.433639705883));
#147463=CARTESIAN_POINT('Ctrl Pts',(-50.5832961557877,-4.68723266073574,
-960.927757352941));
#147464=CARTESIAN_POINT('Ctrl Pts',(-51.0176322249162,-3.12392900021603E-15,
-962.421875));
#147465=CARTESIAN_POINT('Ctrl Pts',(-50.5832961557877,4.68723266073573,
-963.915992647059));
#147466=CARTESIAN_POINT('Ctrl Pts',(-50.1489600866593,9.37446532147149,
-965.410110294118));
#147467=CARTESIAN_POINT('Ctrl Pts',(-48.8607426731792,13.9020798956618,
-966.904227941177));
#147468=CARTESIAN_POINT('Ctrl Pts',(-47.5725252596992,18.4296944698521,
-968.398345588236));
#147469=CARTESIAN_POINT('Ctrl Pts',(-45.4742952008371,22.6435084734481,
-969.892463235294));
#147470=CARTESIAN_POINT('Ctrl Pts',(-43.3760651419751,26.8573224770442,
-971.386580882353));
#147471=CARTESIAN_POINT('Ctrl Pts',(-40.5392751458362,30.6138395280662,
-972.880698529412));
#147472=CARTESIAN_POINT('Ctrl Pts',(-37.7024851496972,34.3703565790883,
-974.374816176471));
#147473=CARTESIAN_POINT('Ctrl Pts',(-34.2237386972451,37.5416529948095,
-975.868933823529));
#147474=CARTESIAN_POINT('Ctrl Pts',(-30.744992244793,40.7129494105307,-977.363051470588));
#147475=CARTESIAN_POINT('Ctrl Pts',(-26.7427538741697,43.1910304950644,
-978.857169117647));
#147476=CARTESIAN_POINT('Ctrl Pts',(-22.7405155035463,45.6691115795981,
-980.351286764706));
#147477=CARTESIAN_POINT('Ctrl Pts',(-18.3510766423074,47.3695892537413,
-981.845404411765));
#147478=CARTESIAN_POINT('Ctrl Pts',(-13.9616377810684,49.0700669278844,
-983.339522058824));
#147479=CARTESIAN_POINT('Ctrl Pts',(-9.33447550508177,49.9350334639422,
-984.833639705882));
#147480=CARTESIAN_POINT('Ctrl Pts',(-4.7073132290951,50.8,-986.327757352941));
#147481=CARTESIAN_POINT('Ctrl Pts',(-6.22120573966855E-15,50.8,-987.821875));
#147482=CARTESIAN_POINT('Ctrl Pts',(4.70731322909511,50.8,-989.315992647059));
#147483=CARTESIAN_POINT('Ctrl Pts',(9.33447550508176,49.9350334639422,-990.810110294118));
#147484=CARTESIAN_POINT('Ctrl Pts',(13.9616377810684,49.0700669278844,-992.304227941177));
#147485=CARTESIAN_POINT('Ctrl Pts',(18.3510766423074,47.3695892537413,-993.798345588235));
#147486=CARTESIAN_POINT('Ctrl Pts',(22.7405155035463,45.6691115795981,-995.292463235294));
#147487=CARTESIAN_POINT('Ctrl Pts',(26.7427538741697,43.1910304950644,-996.786580882353));
#147488=CARTESIAN_POINT('Ctrl Pts',(30.744992244793,40.7129494105307,-998.280698529412));
#147489=CARTESIAN_POINT('Ctrl Pts',(34.2237386972451,37.5416529948095,-999.77481617647));
#147490=CARTESIAN_POINT('Ctrl Pts',(37.7024851496972,34.3703565790883,-1001.26893382353));
#147491=CARTESIAN_POINT('Ctrl Pts',(40.5392751458362,30.6138395280662,-1002.76305147059));
#147492=CARTESIAN_POINT('Ctrl Pts',(43.3760651419751,26.8573224770442,-1004.25716911765));
#147493=CARTESIAN_POINT('Ctrl Pts',(45.4742952008372,22.6435084734481,-1005.75128676471));
#147494=CARTESIAN_POINT('Ctrl Pts',(47.5725252596992,18.4296944698521,-1007.24540441176));
#147495=CARTESIAN_POINT('Ctrl Pts',(48.8607426731792,13.9020798956618,-1008.73952205882));
#147496=CARTESIAN_POINT('Ctrl Pts',(50.1489600866593,9.37446532147146,-1010.23363970588));
#147497=CARTESIAN_POINT('Ctrl Pts',(50.5832961557877,4.68723266073574,-1011.72775735294));
#147498=CARTESIAN_POINT('Ctrl Pts',(51.0176322249162,9.37178700064808E-15,
-1013.221875));
#147499=CARTESIAN_POINT('Ctrl Pts',(50.5832961557877,-4.68723266073572,
-1014.71599264706));
#147500=CARTESIAN_POINT('Ctrl Pts',(50.1489600866593,-9.37446532147149,
-1016.21011029412));
#147501=CARTESIAN_POINT('Ctrl Pts',(48.8607426731792,-13.9020798956618,
-1017.70422794118));
#147502=CARTESIAN_POINT('Ctrl Pts',(47.5725252596992,-18.4296944698521,
-1019.19834558824));
#147503=CARTESIAN_POINT('Ctrl Pts',(45.4742952008371,-22.6435084734482,
-1020.69246323529));
#147504=CARTESIAN_POINT('Ctrl Pts',(43.3760651419751,-26.8573224770441,
-1022.18658088235));
#147505=CARTESIAN_POINT('Ctrl Pts',(40.5392751458362,-30.6138395280662,
-1023.68069852941));
#147506=CARTESIAN_POINT('Ctrl Pts',(37.7024851496972,-34.3703565790883,
-1025.17481617647));
#147507=CARTESIAN_POINT('Ctrl Pts',(34.2237386972451,-37.5416529948095,
-1026.66893382353));
#147508=CARTESIAN_POINT('Ctrl Pts',(30.744992244793,-40.7129494105307,-1028.16305147059));
#147509=CARTESIAN_POINT('Ctrl Pts',(26.7427538741697,-43.1910304950644,
-1029.65716911765));
#147510=CARTESIAN_POINT('Ctrl Pts',(22.7405155035463,-45.6691115795981,
-1031.15128676471));
#147511=CARTESIAN_POINT('Ctrl Pts',(18.3510766423074,-47.3695892537413,
-1032.64540441176));
#147512=CARTESIAN_POINT('Ctrl Pts',(13.9616377810684,-49.0700669278844,
-1034.13952205882));
#147513=CARTESIAN_POINT('Ctrl Pts',(9.33447550508176,-49.9350334639422,
-1035.63363970588));
#147514=CARTESIAN_POINT('Ctrl Pts',(4.70731322909511,-50.8,-1037.12775735294));
#147515=CARTESIAN_POINT('Ctrl Pts',(0.,-50.8,-1038.621875));
#147516=CARTESIAN_POINT('Ctrl Pts',(-4.70731322909511,-50.8,-1040.11599264706));
#147517=CARTESIAN_POINT('Ctrl Pts',(-9.33447550508177,-49.9350334639422,
-1041.61011029412));
#147518=CARTESIAN_POINT('Ctrl Pts',(-13.9616377810684,-49.0700669278844,
-1043.10422794118));
#147519=CARTESIAN_POINT('Ctrl Pts',(-18.3510766423074,-47.3695892537413,
-1044.59834558824));
#147520=CARTESIAN_POINT('Ctrl Pts',(-22.7405155035463,-45.6691115795981,
-1046.09246323529));
#147521=CARTESIAN_POINT('Ctrl Pts',(-26.7427538741697,-43.1910304950644,
-1047.58658088235));
#147522=CARTESIAN_POINT('Ctrl Pts',(-30.744992244793,-40.7129494105307,
-1049.08069852941));
#147523=CARTESIAN_POINT('Ctrl Pts',(-34.2237386972451,-37.5416529948095,
-1050.57481617647));
#147524=CARTESIAN_POINT('Ctrl Pts',(-37.7024851496972,-34.3703565790883,
-1052.06893382353));
#147525=CARTESIAN_POINT('Ctrl Pts',(-40.5392751458362,-30.6138395280662,
-1053.56305147059));
#147526=CARTESIAN_POINT('Ctrl Pts',(-43.3760651419751,-26.8573224770441,
-1055.05716911765));
#147527=CARTESIAN_POINT('Ctrl Pts',(-45.4742952008371,-22.6435084734481,
-1056.55128676471));
#147528=CARTESIAN_POINT('Ctrl Pts',(-47.5725252596992,-18.4296944698521,
-1058.04540441177));
#147529=CARTESIAN_POINT('Ctrl Pts',(-48.8607426731792,-13.9020798956618,
-1059.53952205882));
#147530=CARTESIAN_POINT('Ctrl Pts',(-50.1489600866593,-9.37446532147148,
-1061.03363970588));
#147531=CARTESIAN_POINT('Ctrl Pts',(-50.5832961557877,-4.68723266073574,
-1062.52775735294));
#147532=CARTESIAN_POINT('Ctrl Pts',(-51.0176322249162,-3.12392900021603E-15,
-1064.021875));
#147533=CARTESIAN_POINT('Ctrl Pts',(-50.5832961557877,4.68723266073573,
-1065.51599264706));
#147534=CARTESIAN_POINT('Ctrl Pts',(-50.1489600866593,9.37446532147149,
-1067.01011029412));
#147535=CARTESIAN_POINT('Ctrl Pts',(-48.8607426731792,13.9020798956618,
-1068.50422794118));
#147536=CARTESIAN_POINT('Ctrl Pts',(-47.5725252596992,18.4296944698521,
-1069.99834558824));
#147537=CARTESIAN_POINT('Ctrl Pts',(-45.4742952008371,22.6435084734481,
-1071.49246323529));
#147538=CARTESIAN_POINT('Ctrl Pts',(-43.3760651419751,26.8573224770442,
-1072.98658088235));
#147539=CARTESIAN_POINT('Ctrl Pts',(-40.5392751458362,30.6138395280662,
-1074.48069852941));
#147540=CARTESIAN_POINT('Ctrl Pts',(-37.7024851496972,34.3703565790883,
-1075.97481617647));
#147541=CARTESIAN_POINT('Ctrl Pts',(-34.2237386972451,37.5416529948095,
-1077.46893382353));
#147542=CARTESIAN_POINT('Ctrl Pts',(-30.744992244793,40.7129494105307,-1078.96305147059));
#147543=CARTESIAN_POINT('Ctrl Pts',(-26.7427538741697,43.1910304950644,
-1080.45716911765));
#147544=CARTESIAN_POINT('Ctrl Pts',(-22.7405155035463,45.6691115795981,
-1081.95128676471));
#147545=CARTESIAN_POINT('Ctrl Pts',(-18.3510766423074,47.3695892537413,
-1083.44540441176));
#147546=CARTESIAN_POINT('Ctrl Pts',(-13.9616377810684,49.0700669278844,
-1084.93952205882));
#147547=CARTESIAN_POINT('Ctrl Pts',(-9.33447550508177,49.9350334639422,
-1086.43363970588));
#147548=CARTESIAN_POINT('Ctrl Pts',(-4.7073132290951,50.8,-1087.92775735294));
#147549=CARTESIAN_POINT('Ctrl Pts',(-6.22120573966855E-15,50.8,-1089.421875));
#147550=CARTESIAN_POINT('Ctrl Pts',(4.70731322909511,50.8,-1090.91599264706));
#147551=CARTESIAN_POINT('Ctrl Pts',(9.33447550508176,49.9350334639422,-1092.41011029412));
#147552=CARTESIAN_POINT('Ctrl Pts',(13.9616377810684,49.0700669278844,-1093.90422794118));
#147553=CARTESIAN_POINT('Ctrl Pts',(18.3510766423074,47.3695892537413,-1095.39834558824));
#147554=CARTESIAN_POINT('Ctrl Pts',(22.7405155035463,45.6691115795981,-1096.89246323529));
#147555=CARTESIAN_POINT('Ctrl Pts',(26.7427538741697,43.1910304950644,-1098.38658088235));
#147556=CARTESIAN_POINT('Ctrl Pts',(30.744992244793,40.7129494105307,-1099.88069852941));
#147557=CARTESIAN_POINT('Ctrl Pts',(34.2237386972451,37.5416529948095,-1101.37481617647));
#147558=CARTESIAN_POINT('Ctrl Pts',(37.7024851496972,34.3703565790883,-1102.86893382353));
#147559=CARTESIAN_POINT('Ctrl Pts',(40.5392751458362,30.6138395280662,-1104.36305147059));
#147560=CARTESIAN_POINT('Ctrl Pts',(43.3760651419751,26.8573224770442,-1105.85716911765));
#147561=CARTESIAN_POINT('Ctrl Pts',(45.4742952008372,22.6435084734481,-1107.35128676471));
#147562=CARTESIAN_POINT('Ctrl Pts',(47.5725252596992,18.4296944698521,-1108.84540441177));
#147563=CARTESIAN_POINT('Ctrl Pts',(48.8607426731792,13.9020798956618,-1110.33952205882));
#147564=CARTESIAN_POINT('Ctrl Pts',(50.1489600866593,9.37446532147146,-1111.83363970588));
#147565=CARTESIAN_POINT('Ctrl Pts',(50.5832961557877,4.68723266073574,-1113.32775735294));
#147566=CARTESIAN_POINT('Ctrl Pts',(51.0176322249162,9.37178700064808E-15,
-1114.821875));
#147567=CARTESIAN_POINT('Ctrl Pts',(50.5832961557877,-4.68723266073572,
-1116.31599264706));
#147568=CARTESIAN_POINT('Ctrl Pts',(50.1489600866593,-9.37446532147149,
-1117.81011029412));
#147569=CARTESIAN_POINT('Ctrl Pts',(48.8607426731792,-13.9020798956618,
-1119.30422794118));
#147570=CARTESIAN_POINT('Ctrl Pts',(47.5725252596992,-18.4296944698521,
-1120.79834558823));
#147571=CARTESIAN_POINT('Ctrl Pts',(45.4742952008371,-22.6435084734482,
-1122.29246323529));
#147572=CARTESIAN_POINT('Ctrl Pts',(43.3760651419751,-26.8573224770441,
-1123.78658088235));
#147573=CARTESIAN_POINT('Ctrl Pts',(40.5392751458362,-30.6138395280662,
-1125.28069852941));
#147574=CARTESIAN_POINT('Ctrl Pts',(37.7024851496972,-34.3703565790883,
-1126.77481617647));
#147575=CARTESIAN_POINT('Ctrl Pts',(34.2237386972451,-37.5416529948095,
-1128.26893382353));
#147576=CARTESIAN_POINT('Ctrl Pts',(30.744992244793,-40.7129494105307,-1129.76305147059));
#147577=CARTESIAN_POINT('Ctrl Pts',(26.7427538741697,-43.1910304950644,
-1131.25716911765));
#147578=CARTESIAN_POINT('Ctrl Pts',(22.7405155035463,-45.6691115795981,
-1132.75128676471));
#147579=CARTESIAN_POINT('Ctrl Pts',(18.3510766423074,-47.3695892537413,
-1134.24540441176));
#147580=CARTESIAN_POINT('Ctrl Pts',(13.9616377810684,-49.0700669278844,
-1135.73952205882));
#147581=CARTESIAN_POINT('Ctrl Pts',(9.33447550508176,-49.9350334639422,
-1137.23363970588));
#147582=CARTESIAN_POINT('Ctrl Pts',(4.70731322909511,-50.8,-1138.72775735294));
#147583=CARTESIAN_POINT('Ctrl Pts',(0.,-50.8,-1140.221875));
#147584=CARTESIAN_POINT('Ctrl Pts',(-4.70731322909511,-50.8,-1141.71599264706));
#147585=CARTESIAN_POINT('Ctrl Pts',(-9.33447550508177,-49.9350334639422,
-1143.21011029412));
#147586=CARTESIAN_POINT('Ctrl Pts',(-13.9616377810684,-49.0700669278844,
-1144.70422794118));
#147587=CARTESIAN_POINT('Ctrl Pts',(-18.3510766423074,-47.3695892537413,
-1146.19834558824));
#147588=CARTESIAN_POINT('Ctrl Pts',(-22.7405155035463,-45.6691115795981,
-1147.69246323529));
#147589=CARTESIAN_POINT('Ctrl Pts',(-26.7427538741697,-43.1910304950644,
-1149.18658088235));
#147590=CARTESIAN_POINT('Ctrl Pts',(-30.744992244793,-40.7129494105307,
-1150.68069852941));
#147591=CARTESIAN_POINT('Ctrl Pts',(-34.2237386972451,-37.5416529948095,
-1152.17481617647));
#147592=CARTESIAN_POINT('Ctrl Pts',(-37.7024851496972,-34.3703565790883,
-1153.66893382353));
#147593=CARTESIAN_POINT('Ctrl Pts',(-40.5392751458362,-30.6138395280662,
-1155.16305147059));
#147594=CARTESIAN_POINT('Ctrl Pts',(-43.3760651419751,-26.8573224770441,
-1156.65716911765));
#147595=CARTESIAN_POINT('Ctrl Pts',(-45.4742952008371,-22.6435084734481,
-1158.15128676471));
#147596=CARTESIAN_POINT('Ctrl Pts',(-47.5725252596992,-18.4296944698521,
-1159.64540441176));
#147597=CARTESIAN_POINT('Ctrl Pts',(-48.8607426731792,-13.9020798956618,
-1161.13952205882));
#147598=CARTESIAN_POINT('Ctrl Pts',(-50.1489600866593,-9.37446532147148,
-1162.63363970588));
#147599=CARTESIAN_POINT('Ctrl Pts',(-50.5832961557877,-4.68723266073574,
-1164.12775735294));
#147600=CARTESIAN_POINT('Ctrl Pts',(-51.0176322249162,-3.12392900021603E-15,
-1165.621875));
#147601=CARTESIAN_POINT('Ctrl Pts',(-50.5832961557877,4.68723266073573,
-1167.11599264706));
#147602=CARTESIAN_POINT('Ctrl Pts',(-50.1489600866593,9.37446532147149,
-1168.61011029412));
#147603=CARTESIAN_POINT('Ctrl Pts',(-48.8607426731792,13.9020798956618,
-1170.10422794118));
#147604=CARTESIAN_POINT('Ctrl Pts',(-47.5725252596992,18.4296944698521,
-1171.59834558824));
#147605=CARTESIAN_POINT('Ctrl Pts',(-45.4742952008371,22.6435084734481,
-1173.09246323529));
#147606=CARTESIAN_POINT('Ctrl Pts',(-43.3760651419751,26.8573224770442,
-1174.58658088235));
#147607=CARTESIAN_POINT('Ctrl Pts',(-40.5392751458362,30.6138395280662,
-1176.08069852941));
#147608=CARTESIAN_POINT('Ctrl Pts',(-37.7024851496972,34.3703565790883,
-1177.57481617647));
#147609=CARTESIAN_POINT('Ctrl Pts',(-34.2237386972451,37.5416529948095,
-1179.06893382353));
#147610=CARTESIAN_POINT('Ctrl Pts',(-30.744992244793,40.7129494105307,-1180.56305147059));
#147611=CARTESIAN_POINT('Ctrl Pts',(-26.7427538741697,43.1910304950644,
-1182.05716911765));
#147612=CARTESIAN_POINT('Ctrl Pts',(-22.7405155035463,45.6691115795981,
-1183.55128676471));
#147613=CARTESIAN_POINT('Ctrl Pts',(-18.3510766423074,47.3695892537413,
-1185.04540441176));
#147614=CARTESIAN_POINT('Ctrl Pts',(-13.9616377810684,49.0700669278844,
-1186.53952205882));
#147615=CARTESIAN_POINT('Ctrl Pts',(-9.33447550508177,49.9350334639422,
-1188.03363970588));
#147616=CARTESIAN_POINT('Ctrl Pts',(-4.7073132290951,50.8,-1189.52775735294));
#147617=CARTESIAN_POINT('Ctrl Pts',(-6.22120573966855E-15,50.8,-1191.021875));
#147618=CARTESIAN_POINT('Ctrl Pts',(4.70731322909511,50.8,-1192.51599264706));
#147619=CARTESIAN_POINT('Ctrl Pts',(9.33447550508176,49.9350334639422,-1194.01011029412));
#147620=CARTESIAN_POINT('Ctrl Pts',(13.9616377810684,49.0700669278844,-1195.50422794118));
#147621=CARTESIAN_POINT('Ctrl Pts',(18.3510766423074,47.3695892537413,-1196.99834558824));
#147622=CARTESIAN_POINT('Ctrl Pts',(22.7405155035463,45.6691115795981,-1198.49246323529));
#147623=CARTESIAN_POINT('Ctrl Pts',(26.7427538741697,43.1910304950644,-1199.98658088235));
#147624=CARTESIAN_POINT('Ctrl Pts',(30.744992244793,40.7129494105307,-1201.48069852941));
#147625=CARTESIAN_POINT('Ctrl Pts',(34.2237386972451,37.5416529948095,-1202.97481617647));
#147626=CARTESIAN_POINT('Ctrl Pts',(37.7024851496972,34.3703565790883,-1204.46893382353));
#147627=CARTESIAN_POINT('Ctrl Pts',(40.5392751458362,30.6138395280662,-1205.96305147059));
#147628=CARTESIAN_POINT('Ctrl Pts',(43.3760651419751,26.8573224770442,-1207.45716911765));
#147629=CARTESIAN_POINT('Ctrl Pts',(45.4742952008372,22.6435084734481,-1208.95128676471));
#147630=CARTESIAN_POINT('Ctrl Pts',(47.5725252596992,18.4296944698521,-1210.44540441176));
#147631=CARTESIAN_POINT('Ctrl Pts',(48.8607426731792,13.9020798956618,-1211.93952205882));
#147632=CARTESIAN_POINT('Ctrl Pts',(50.1489600866593,9.37446532147146,-1213.43363970588));
#147633=CARTESIAN_POINT('Ctrl Pts',(50.5832961557877,4.68723266073574,-1214.92775735294));
#147634=CARTESIAN_POINT('Ctrl Pts',(51.0176322249162,9.37178700064808E-15,
-1216.421875));
#147635=CARTESIAN_POINT('Ctrl Pts',(50.5832961557877,-4.68723266073572,
-1217.91599264706));
#147636=CARTESIAN_POINT('Ctrl Pts',(50.1489600866593,-9.37446532147149,
-1219.41011029412));
#147637=CARTESIAN_POINT('Ctrl Pts',(48.8607426731792,-13.9020798956618,
-1220.90422794118));
#147638=CARTESIAN_POINT('Ctrl Pts',(47.5725252596992,-18.4296944698521,
-1222.39834558824));
#147639=CARTESIAN_POINT('Ctrl Pts',(45.4742952008371,-22.6435084734482,
-1223.89246323529));
#147640=CARTESIAN_POINT('Ctrl Pts',(43.3760651419751,-26.8573224770441,
-1225.38658088235));
#147641=CARTESIAN_POINT('Ctrl Pts',(40.5392751458362,-30.6138395280662,
-1226.88069852941));
#147642=CARTESIAN_POINT('Ctrl Pts',(37.7024851496972,-34.3703565790883,
-1228.37481617647));
#147643=CARTESIAN_POINT('Ctrl Pts',(34.2237386972451,-37.5416529948095,
-1229.86893382353));
#147644=CARTESIAN_POINT('Ctrl Pts',(30.744992244793,-40.7129494105307,-1231.36305147059));
#147645=CARTESIAN_POINT('Ctrl Pts',(26.7427538741697,-43.1910304950644,
-1232.85716911765));
#147646=CARTESIAN_POINT('Ctrl Pts',(22.7405155035463,-45.6691115795981,
-1234.35128676471));
#147647=CARTESIAN_POINT('Ctrl Pts',(18.3510766423074,-47.3695892537413,
-1235.84540441176));
#147648=CARTESIAN_POINT('Ctrl Pts',(13.9616377810684,-49.0700669278844,
-1237.33952205882));
#147649=CARTESIAN_POINT('Ctrl Pts',(9.33447550508176,-49.9350334639422,
-1238.83363970588));
#147650=CARTESIAN_POINT('Ctrl Pts',(4.70731322909511,-50.8,-1240.32775735294));
#147651=CARTESIAN_POINT('Ctrl Pts',(0.,-50.8,-1241.821875));
#147652=CARTESIAN_POINT('Ctrl Pts',(-4.70731322909511,-50.8,-1243.31599264706));
#147653=CARTESIAN_POINT('Ctrl Pts',(-9.33447550508177,-49.9350334639422,
-1244.81011029412));
#147654=CARTESIAN_POINT('Ctrl Pts',(-13.9616377810684,-49.0700669278844,
-1246.30422794118));
#147655=CARTESIAN_POINT('Ctrl Pts',(-18.3510766423074,-47.3695892537413,
-1247.79834558824));
#147656=CARTESIAN_POINT('Ctrl Pts',(-22.7405155035463,-45.6691115795981,
-1249.29246323529));
#147657=CARTESIAN_POINT('Ctrl Pts',(-26.7427538741697,-43.1910304950644,
-1250.78658088235));
#147658=CARTESIAN_POINT('Ctrl Pts',(-30.744992244793,-40.7129494105307,
-1252.28069852941));
#147659=CARTESIAN_POINT('Ctrl Pts',(-34.2237386972451,-37.5416529948095,
-1253.77481617647));
#147660=CARTESIAN_POINT('Ctrl Pts',(-37.7024851496972,-34.3703565790883,
-1255.26893382353));
#147661=CARTESIAN_POINT('Ctrl Pts',(-40.5392751458362,-30.6138395280662,
-1256.76305147059));
#147662=CARTESIAN_POINT('Ctrl Pts',(-43.3760651419751,-26.8573224770441,
-1258.25716911765));
#147663=CARTESIAN_POINT('Ctrl Pts',(-45.4742952008371,-22.6435084734481,
-1259.75128676471));
#147664=CARTESIAN_POINT('Ctrl Pts',(-47.5725252596992,-18.4296944698521,
-1261.24540441176));
#147665=CARTESIAN_POINT('Ctrl Pts',(-48.8607426731792,-13.9020798956618,
-1262.73952205882));
#147666=CARTESIAN_POINT('Ctrl Pts',(-50.1489600866593,-9.37446532147148,
-1264.23363970588));
#147667=CARTESIAN_POINT('Ctrl Pts',(-50.5832961557877,-4.68723266073574,
-1265.72775735294));
#147668=CARTESIAN_POINT('Ctrl Pts',(-51.0176322249162,-3.12392900021603E-15,
-1267.221875));
#147669=CARTESIAN_POINT('Ctrl Pts',(-50.5832961557877,4.68723266073573,
-1268.71599264706));
#147670=CARTESIAN_POINT('Ctrl Pts',(-50.1489600866593,9.37446532147149,
-1270.21011029412));
#147671=CARTESIAN_POINT('Ctrl Pts',(-48.8607426731792,13.9020798956618,
-1271.70422794118));
#147672=CARTESIAN_POINT('Ctrl Pts',(-47.5725252596992,18.4296944698521,
-1273.19834558824));
#147673=CARTESIAN_POINT('Ctrl Pts',(-45.4742952008371,22.6435084734481,
-1274.69246323529));
#147674=CARTESIAN_POINT('Ctrl Pts',(-43.3760651419751,26.8573224770442,
-1276.18658088235));
#147675=CARTESIAN_POINT('Ctrl Pts',(-40.5392751458362,30.6138395280662,
-1277.68069852941));
#147676=CARTESIAN_POINT('Ctrl Pts',(-37.7024851496972,34.3703565790883,
-1279.17481617647));
#147677=CARTESIAN_POINT('Ctrl Pts',(-34.2237386972451,37.5416529948095,
-1280.66893382353));
#147678=CARTESIAN_POINT('Ctrl Pts',(-30.744992244793,40.7129494105307,-1282.16305147059));
#147679=CARTESIAN_POINT('Ctrl Pts',(-26.7427538741697,43.1910304950644,
-1283.65716911765));
#147680=CARTESIAN_POINT('Ctrl Pts',(-22.7405155035463,45.6691115795981,
-1285.15128676471));
#147681=CARTESIAN_POINT('Ctrl Pts',(-18.3510766423074,47.3695892537413,
-1286.64540441176));
#147682=CARTESIAN_POINT('Ctrl Pts',(-13.9616377810684,49.0700669278844,
-1288.13952205882));
#147683=CARTESIAN_POINT('Ctrl Pts',(-9.33447550508177,49.9350334639422,
-1289.63363970588));
#147684=CARTESIAN_POINT('Ctrl Pts',(-4.7073132290951,50.8,-1291.12775735294));
#147685=CARTESIAN_POINT('Ctrl Pts',(-6.22120573966855E-15,50.8,-1292.621875));
#147686=CARTESIAN_POINT('Ctrl Pts',(4.70731322909511,50.8,-1294.11599264706));
#147687=CARTESIAN_POINT('Ctrl Pts',(9.33447550508176,49.9350334639422,-1295.61011029412));
#147688=CARTESIAN_POINT('Ctrl Pts',(13.9616377810684,49.0700669278844,-1297.10422794118));
#147689=CARTESIAN_POINT('Ctrl Pts',(18.3510766423074,47.3695892537413,-1298.59834558824));
#147690=CARTESIAN_POINT('Ctrl Pts',(22.7405155035463,45.6691115795981,-1300.09246323529));
#147691=CARTESIAN_POINT('Ctrl Pts',(26.7427538741697,43.1910304950644,-1301.58658088235));
#147692=CARTESIAN_POINT('Ctrl Pts',(30.744992244793,40.7129494105307,-1303.08069852941));
#147693=CARTESIAN_POINT('Ctrl Pts',(34.2237386972451,37.5416529948095,-1304.57481617647));
#147694=CARTESIAN_POINT('Ctrl Pts',(37.7024851496972,34.3703565790883,-1306.06893382353));
#147695=CARTESIAN_POINT('Ctrl Pts',(40.5392751458362,30.6138395280662,-1307.56305147059));
#147696=CARTESIAN_POINT('Ctrl Pts',(43.3760651419751,26.8573224770442,-1309.05716911765));
#147697=CARTESIAN_POINT('Ctrl Pts',(45.4742952008372,22.6435084734481,-1310.55128676471));
#147698=CARTESIAN_POINT('Ctrl Pts',(47.5725252596992,18.4296944698521,-1312.04540441176));
#147699=CARTESIAN_POINT('Ctrl Pts',(48.8607426731792,13.9020798956618,-1313.53952205882));
#147700=CARTESIAN_POINT('Ctrl Pts',(50.1489600866593,9.37446532147146,-1315.03363970588));
#147701=CARTESIAN_POINT('Ctrl Pts',(50.5832961557877,4.68723266073574,-1316.52775735294));
#147702=CARTESIAN_POINT('Ctrl Pts',(51.0176322249162,9.37178700064808E-15,
-1318.021875));
#147703=CARTESIAN_POINT('Ctrl Pts',(50.5832961557877,-4.68723266073572,
-1319.51599264706));
#147704=CARTESIAN_POINT('Ctrl Pts',(50.1489600866593,-9.37446532147149,
-1321.01011029412));
#147705=CARTESIAN_POINT('Ctrl Pts',(48.8607426731792,-13.9020798956618,
-1322.50422794118));
#147706=CARTESIAN_POINT('Ctrl Pts',(47.5725252596992,-18.4296944698521,
-1323.99834558824));
#147707=CARTESIAN_POINT('Ctrl Pts',(45.4742952008371,-22.6435084734482,
-1325.49246323529));
#147708=CARTESIAN_POINT('Ctrl Pts',(43.3760651419751,-26.8573224770441,
-1326.98658088235));
#147709=CARTESIAN_POINT('Ctrl Pts',(40.5392751458362,-30.6138395280662,
-1328.48069852941));
#147710=CARTESIAN_POINT('Ctrl Pts',(37.7024851496972,-34.3703565790883,
-1329.97481617647));
#147711=CARTESIAN_POINT('Ctrl Pts',(34.2237386972451,-37.5416529948095,
-1331.46893382353));
#147712=CARTESIAN_POINT('Ctrl Pts',(30.744992244793,-40.7129494105307,-1332.96305147059));
#147713=CARTESIAN_POINT('Ctrl Pts',(26.7427538741697,-43.1910304950644,
-1334.45716911765));
#147714=CARTESIAN_POINT('Ctrl Pts',(22.7405155035463,-45.6691115795981,
-1335.95128676471));
#147715=CARTESIAN_POINT('Ctrl Pts',(18.3510766423074,-47.3695892537413,
-1337.44540441176));
#147716=CARTESIAN_POINT('Ctrl Pts',(13.9616377810684,-49.0700669278844,
-1338.93952205882));
#147717=CARTESIAN_POINT('Ctrl Pts',(9.33447550508176,-49.9350334639422,
-1340.43363970588));
#147718=CARTESIAN_POINT('Ctrl Pts',(4.70731322909511,-50.8,-1341.92775735294));
#147719=CARTESIAN_POINT('Ctrl Pts',(0.,-50.8,-1343.421875));
#147720=CARTESIAN_POINT('Ctrl Pts',(-4.70731322909511,-50.8,-1344.91599264706));
#147721=CARTESIAN_POINT('Ctrl Pts',(-9.33447550508177,-49.9350334639422,
-1346.41011029412));
#147722=CARTESIAN_POINT('Ctrl Pts',(-13.9616377810684,-49.0700669278844,
-1347.90422794118));
#147723=CARTESIAN_POINT('Ctrl Pts',(-18.3510766423074,-47.3695892537413,
-1349.39834558824));
#147724=CARTESIAN_POINT('Ctrl Pts',(-22.7405155035463,-45.6691115795981,
-1350.89246323529));
#147725=CARTESIAN_POINT('Ctrl Pts',(-26.7427538741697,-43.1910304950644,
-1352.38658088235));
#147726=CARTESIAN_POINT('Ctrl Pts',(-30.744992244793,-40.7129494105307,
-1353.88069852941));
#147727=CARTESIAN_POINT('Ctrl Pts',(-34.2237386972451,-37.5416529948095,
-1355.37481617647));
#147728=CARTESIAN_POINT('Ctrl Pts',(-37.7024851496972,-34.3703565790883,
-1356.86893382353));
#147729=CARTESIAN_POINT('Ctrl Pts',(-40.5392751458362,-30.6138395280662,
-1358.36305147059));
#147730=CARTESIAN_POINT('Ctrl Pts',(-43.3760651419751,-26.8573224770441,
-1359.85716911765));
#147731=CARTESIAN_POINT('Ctrl Pts',(-45.4742952008371,-22.6435084734481,
-1361.35128676471));
#147732=CARTESIAN_POINT('Ctrl Pts',(-47.5725252596992,-18.4296944698521,
-1362.84540441176));
#147733=CARTESIAN_POINT('Ctrl Pts',(-48.8607426731792,-13.9020798956618,
-1364.33952205882));
#147734=CARTESIAN_POINT('Ctrl Pts',(-50.1489600866593,-9.37446532147148,
-1365.83363970588));
#147735=CARTESIAN_POINT('Ctrl Pts',(-50.5832961557877,-4.68723266073574,
-1367.32775735294));
#147736=CARTESIAN_POINT('Ctrl Pts',(-51.0176322249162,-3.12392900021603E-15,
-1368.821875));
#147737=CARTESIAN_POINT('Ctrl Pts',(-50.5832961557877,4.68723266073573,
-1370.31599264706));
#147738=CARTESIAN_POINT('Ctrl Pts',(-50.1489600866593,9.37446532147149,
-1371.81011029412));
#147739=CARTESIAN_POINT('Ctrl Pts',(-48.8607426731792,13.9020798956618,
-1373.30422794118));
#147740=CARTESIAN_POINT('Ctrl Pts',(-47.5725252596992,18.4296944698521,
-1374.79834558824));
#147741=CARTESIAN_POINT('Ctrl Pts',(-45.4742952008371,22.6435084734481,
-1376.29246323529));
#147742=CARTESIAN_POINT('Ctrl Pts',(-43.3760651419751,26.8573224770442,
-1377.78658088235));
#147743=CARTESIAN_POINT('Ctrl Pts',(-40.5392751458362,30.6138395280662,
-1379.28069852941));
#147744=CARTESIAN_POINT('Ctrl Pts',(-37.7024851496972,34.3703565790883,
-1380.77481617647));
#147745=CARTESIAN_POINT('Ctrl Pts',(-34.2237386972451,37.5416529948095,
-1382.26893382353));
#147746=CARTESIAN_POINT('Ctrl Pts',(-30.744992244793,40.7129494105307,-1383.76305147059));
#147747=CARTESIAN_POINT('Ctrl Pts',(-26.7427538741697,43.1910304950644,
-1385.25716911765));
#147748=CARTESIAN_POINT('Ctrl Pts',(-22.7405155035463,45.6691115795981,
-1386.75128676471));
#147749=CARTESIAN_POINT('Ctrl Pts',(-18.3510766423074,47.3695892537413,
-1388.24540441176));
#147750=CARTESIAN_POINT('Ctrl Pts',(-13.9616377810684,49.0700669278844,
-1389.73952205882));
#147751=CARTESIAN_POINT('Ctrl Pts',(-9.33447550508177,49.9350334639422,
-1391.23363970588));
#147752=CARTESIAN_POINT('Ctrl Pts',(-4.7073132290951,50.8,-1392.72775735294));
#147753=CARTESIAN_POINT('Ctrl Pts',(-6.22120573966855E-15,50.8,-1394.221875));
#147754=CARTESIAN_POINT('Ctrl Pts',(4.70731322909511,50.8,-1395.71599264706));
#147755=CARTESIAN_POINT('Ctrl Pts',(9.33447550508176,49.9350334639422,-1397.21011029412));
#147756=CARTESIAN_POINT('Ctrl Pts',(13.9616377810684,49.0700669278844,-1398.70422794118));
#147757=CARTESIAN_POINT('Ctrl Pts',(18.3510766423074,47.3695892537413,-1400.19834558824));
#147758=CARTESIAN_POINT('Ctrl Pts',(22.7405155035463,45.6691115795981,-1401.69246323529));
#147759=CARTESIAN_POINT('Ctrl Pts',(26.7427538741697,43.1910304950644,-1403.18658088235));
#147760=CARTESIAN_POINT('Ctrl Pts',(30.744992244793,40.7129494105307,-1404.68069852941));
#147761=CARTESIAN_POINT('Ctrl Pts',(34.2237386972451,37.5416529948095,-1406.17481617647));
#147762=CARTESIAN_POINT('Ctrl Pts',(37.7024851496972,34.3703565790883,-1407.66893382353));
#147763=CARTESIAN_POINT('Ctrl Pts',(40.5392751458362,30.6138395280662,-1409.16305147059));
#147764=CARTESIAN_POINT('Ctrl Pts',(43.3760651419751,26.8573224770442,-1410.65716911765));
#147765=CARTESIAN_POINT('Ctrl Pts',(45.4742952008372,22.6435084734481,-1412.15128676471));
#147766=CARTESIAN_POINT('Ctrl Pts',(47.5725252596992,18.4296944698521,-1413.64540441176));
#147767=CARTESIAN_POINT('Ctrl Pts',(48.8607426731792,13.9020798956618,-1415.13952205882));
#147768=CARTESIAN_POINT('Ctrl Pts',(50.1489600866593,9.37446532147146,-1416.63363970588));
#147769=CARTESIAN_POINT('Ctrl Pts',(50.5832961557877,4.68723266073574,-1418.12775735294));
#147770=CARTESIAN_POINT('Ctrl Pts',(51.0176322249162,9.37178700064808E-15,
-1419.621875));
#147771=CARTESIAN_POINT('Ctrl Pts',(50.5832961557877,-4.68723266073572,
-1421.11599264706));
#147772=CARTESIAN_POINT('Ctrl Pts',(50.1489600866593,-9.37446532147149,
-1422.61011029412));
#147773=CARTESIAN_POINT('Ctrl Pts',(48.8607426731792,-13.9020798956618,
-1424.10422794118));
#147774=CARTESIAN_POINT('Ctrl Pts',(47.5725252596992,-18.4296944698521,
-1425.59834558824));
#147775=CARTESIAN_POINT('Ctrl Pts',(45.4742952008371,-22.6435084734482,
-1427.09246323529));
#147776=CARTESIAN_POINT('Ctrl Pts',(43.3760651419751,-26.8573224770441,
-1428.58658088235));
#147777=CARTESIAN_POINT('Ctrl Pts',(40.5392751458362,-30.6138395280662,
-1430.08069852941));
#147778=CARTESIAN_POINT('Ctrl Pts',(37.7024851496972,-34.3703565790883,
-1431.57481617647));
#147779=CARTESIAN_POINT('Ctrl Pts',(34.2237386972451,-37.5416529948095,
-1433.06893382353));
#147780=CARTESIAN_POINT('Ctrl Pts',(30.744992244793,-40.7129494105307,-1434.56305147059));
#147781=CARTESIAN_POINT('Ctrl Pts',(26.7427538741697,-43.1910304950644,
-1436.05716911765));
#147782=CARTESIAN_POINT('Ctrl Pts',(22.7405155035463,-45.6691115795981,
-1437.55128676471));
#147783=CARTESIAN_POINT('Ctrl Pts',(18.3510766423074,-47.3695892537413,
-1439.04540441176));
#147784=CARTESIAN_POINT('Ctrl Pts',(13.9616377810684,-49.0700669278844,
-1440.53952205882));
#147785=CARTESIAN_POINT('Ctrl Pts',(9.33447550508176,-49.9350334639422,
-1442.03363970588));
#147786=CARTESIAN_POINT('Ctrl Pts',(4.70731322909511,-50.8,-1443.52775735294));
#147787=CARTESIAN_POINT('Ctrl Pts',(0.,-50.8,-1445.021875));
#147788=CARTESIAN_POINT('Ctrl Pts',(-4.70731322909511,-50.8,-1446.51599264706));
#147789=CARTESIAN_POINT('Ctrl Pts',(-9.33447550508177,-49.9350334639422,
-1448.01011029412));
#147790=CARTESIAN_POINT('Ctrl Pts',(-13.9616377810684,-49.0700669278844,
-1449.50422794118));
#147791=CARTESIAN_POINT('Ctrl Pts',(-18.3510766423074,-47.3695892537413,
-1450.99834558824));
#147792=CARTESIAN_POINT('Ctrl Pts',(-22.7405155035463,-45.6691115795981,
-1452.49246323529));
#147793=CARTESIAN_POINT('Ctrl Pts',(-26.7427538741697,-43.1910304950644,
-1453.98658088235));
#147794=CARTESIAN_POINT('Ctrl Pts',(-30.744992244793,-40.7129494105307,
-1455.48069852941));
#147795=CARTESIAN_POINT('Ctrl Pts',(-34.2237386972451,-37.5416529948095,
-1456.97481617647));
#147796=CARTESIAN_POINT('Ctrl Pts',(-37.7024851496972,-34.3703565790883,
-1458.46893382353));
#147797=CARTESIAN_POINT('Ctrl Pts',(-40.5392751458362,-30.6138395280662,
-1459.96305147059));
#147798=CARTESIAN_POINT('Ctrl Pts',(-43.3760651419751,-26.8573224770441,
-1461.45716911765));
#147799=CARTESIAN_POINT('Ctrl Pts',(-45.4742952008371,-22.6435084734481,
-1462.95128676471));
#147800=CARTESIAN_POINT('Ctrl Pts',(-47.5725252596992,-18.4296944698521,
-1464.44540441176));
#147801=CARTESIAN_POINT('Ctrl Pts',(-48.8607426731792,-13.9020798956618,
-1465.93952205882));
#147802=CARTESIAN_POINT('Ctrl Pts',(-50.1489600866593,-9.37446532147148,
-1467.43363970588));
#147803=CARTESIAN_POINT('Ctrl Pts',(-50.5832961557877,-4.68723266073574,
-1468.92775735294));
#147804=CARTESIAN_POINT('Ctrl Pts',(-51.0176322249162,-3.12392900021603E-15,
-1470.421875));
#147805=CARTESIAN_POINT('Ctrl Pts',(-50.5832961557877,4.68723266073573,
-1471.91599264706));
#147806=CARTESIAN_POINT('Ctrl Pts',(-50.1489600866593,9.37446532147149,
-1473.41011029412));
#147807=CARTESIAN_POINT('Ctrl Pts',(-48.8607426731792,13.9020798956618,
-1474.90422794118));
#147808=CARTESIAN_POINT('Ctrl Pts',(-47.5725252596992,18.4296944698521,
-1476.39834558824));
#147809=CARTESIAN_POINT('Ctrl Pts',(-45.4742952008371,22.6435084734481,
-1477.89246323529));
#147810=CARTESIAN_POINT('Ctrl Pts',(-43.3760651419751,26.8573224770442,
-1479.38658088235));
#147811=CARTESIAN_POINT('Ctrl Pts',(-40.5392751458362,30.6138395280662,
-1480.88069852941));
#147812=CARTESIAN_POINT('Ctrl Pts',(-37.7024851496972,34.3703565790883,
-1482.37481617647));
#147813=CARTESIAN_POINT('Ctrl Pts',(-34.2237386972451,37.5416529948095,
-1483.86893382353));
#147814=CARTESIAN_POINT('Ctrl Pts',(-30.744992244793,40.7129494105307,-1485.36305147059));
#147815=CARTESIAN_POINT('Ctrl Pts',(-26.7427538741697,43.1910304950644,
-1486.85716911765));
#147816=CARTESIAN_POINT('Ctrl Pts',(-22.7405155035463,45.6691115795981,
-1488.35128676471));
#147817=CARTESIAN_POINT('Ctrl Pts',(-18.3510766423074,47.3695892537413,
-1489.84540441176));
#147818=CARTESIAN_POINT('Ctrl Pts',(-13.9616377810684,49.0700669278844,
-1491.33952205882));
#147819=CARTESIAN_POINT('Ctrl Pts',(-9.33447550508177,49.9350334639422,
-1492.83363970588));
#147820=CARTESIAN_POINT('Ctrl Pts',(-4.7073132290951,50.8,-1494.32775735294));
#147821=CARTESIAN_POINT('Ctrl Pts',(-6.22120573966855E-15,50.8,-1495.821875));
#147822=CARTESIAN_POINT('Ctrl Pts',(4.70731322909511,50.8,-1497.31599264706));
#147823=CARTESIAN_POINT('Ctrl Pts',(9.33447550508176,49.9350334639422,-1498.81011029412));
#147824=CARTESIAN_POINT('Ctrl Pts',(13.9616377810684,49.0700669278844,-1500.30422794118));
#147825=CARTESIAN_POINT('Ctrl Pts',(18.3510766423074,47.3695892537413,-1501.79834558824));
#147826=CARTESIAN_POINT('Ctrl Pts',(21.2268878088737,46.2554940724685,-1502.77724069292));
#147827=CARTESIAN_POINT('Ctrl Pts',(23.9468011449081,44.8016820546531,-1503.75991977561));
#147828=CARTESIAN_POINT('Ctrl Pts',(0.,-18.048,1500.28886941341));
#147829=CARTESIAN_POINT('Ctrl Pts',(-1.67239348737615,-18.048,1498.79475176635));
#147830=CARTESIAN_POINT('Ctrl Pts',(-3.31631129755346,-17.7406985030951,
1497.30063411929));
#147831=CARTESIAN_POINT('Ctrl Pts',(-4.96022910773077,-17.4333970061901,
1495.80651647223));
#147832=CARTESIAN_POINT('Ctrl Pts',(-6.51968959134574,-16.8292587962898,
1494.31239882517));
#147833=CARTESIAN_POINT('Ctrl Pts',(-8.07915007496071,-16.2251205863895,
1492.81828117811));
#147834=CARTESIAN_POINT('Ctrl Pts',(-9.50104767561052,-15.3447188656481,
1491.32416353106));
#147835=CARTESIAN_POINT('Ctrl Pts',(-10.9229452762603,-14.4643171449067,
1489.830045884));
#147836=CARTESIAN_POINT('Ctrl Pts',(-12.1588589765331,-13.3376329379985,
1488.33592823694));
#147837=CARTESIAN_POINT('Ctrl Pts',(-13.3947726768058,-12.2109487310903,
1486.84181058988));
#147838=CARTESIAN_POINT('Ctrl Pts',(-14.4026149179538,-10.8763499173728,
1485.34769294282));
#147839=CARTESIAN_POINT('Ctrl Pts',(-15.4104571591017,-9.54175110365538,
1483.85357529576));
#147840=CARTESIAN_POINT('Ctrl Pts',(-16.1559070823762,-8.04468584505497,
1482.3594576487));
#147841=CARTESIAN_POINT('Ctrl Pts',(-16.9013570056506,-6.54762058645456,
1480.86534000164));
#147842=CARTESIAN_POINT('Ctrl Pts',(-17.3590292079831,-4.93906964482095,
1479.37122235458));
#147843=CARTESIAN_POINT('Ctrl Pts',(-17.8167014103155,-3.33051870318735,
1477.87710470753));
#147844=CARTESIAN_POINT('Ctrl Pts',(-17.9710104137728,-1.66525935159368,
1476.38298706047));
#147845=CARTESIAN_POINT('Ctrl Pts',(-18.1253194172301,-1.10985572039171E-15,
1474.88886941341));
#147846=CARTESIAN_POINT('Ctrl Pts',(-17.9710104137728,1.66525935159367,
1473.39475176635));
#147847=CARTESIAN_POINT('Ctrl Pts',(-17.8167014103155,3.33051870318735,
1471.90063411929));
#147848=CARTESIAN_POINT('Ctrl Pts',(-17.3590292079831,4.93906964482096,
1470.40651647223));
#147849=CARTESIAN_POINT('Ctrl Pts',(-16.9013570056506,6.54762058645456,
1468.91239882517));
#147850=CARTESIAN_POINT('Ctrl Pts',(-16.1559070823762,8.04468584505497,
1467.41828117811));
#147851=CARTESIAN_POINT('Ctrl Pts',(-15.4104571591017,9.54175110365538,
1465.92416353106));
#147852=CARTESIAN_POINT('Ctrl Pts',(-14.4026149179538,10.8763499173728,
1464.430045884));
#147853=CARTESIAN_POINT('Ctrl Pts',(-13.3947726768058,12.2109487310903,
1462.93592823694));
#147854=CARTESIAN_POINT('Ctrl Pts',(-12.1588589765331,13.3376329379985,
1461.44181058988));
#147855=CARTESIAN_POINT('Ctrl Pts',(-10.9229452762603,14.4643171449067,
1459.94769294282));
#147856=CARTESIAN_POINT('Ctrl Pts',(-9.50104767561052,15.3447188656481,
1458.45357529576));
#147857=CARTESIAN_POINT('Ctrl Pts',(-8.07915007496071,16.2251205863895,
1456.9594576487));
#147858=CARTESIAN_POINT('Ctrl Pts',(-6.51968959134574,16.8292587962898,
1455.46534000164));
#147859=CARTESIAN_POINT('Ctrl Pts',(-4.96022910773078,17.4333970061901,
1453.97122235458));
#147860=CARTESIAN_POINT('Ctrl Pts',(-3.31631129755346,17.7406985030951,
1452.47710470753));
#147861=CARTESIAN_POINT('Ctrl Pts',(-1.67239348737615,18.048,1450.98298706047));
#147862=CARTESIAN_POINT('Ctrl Pts',(-2.21024254310115E-15,18.048,1449.48886941341));
#147863=CARTESIAN_POINT('Ctrl Pts',(1.67239348737616,18.048,1447.99475176635));
#147864=CARTESIAN_POINT('Ctrl Pts',(3.31631129755346,17.7406985030951,1446.50063411929));
#147865=CARTESIAN_POINT('Ctrl Pts',(4.96022910773077,17.4333970061901,1445.00651647223));
#147866=CARTESIAN_POINT('Ctrl Pts',(6.51968959134575,16.8292587962898,1443.51239882517));
#147867=CARTESIAN_POINT('Ctrl Pts',(8.07915007496071,16.2251205863895,1442.01828117811));
#147868=CARTESIAN_POINT('Ctrl Pts',(9.50104767561053,15.3447188656481,1440.52416353105));
#147869=CARTESIAN_POINT('Ctrl Pts',(10.9229452762603,14.4643171449067,1439.030045884));
#147870=CARTESIAN_POINT('Ctrl Pts',(12.1588589765331,13.3376329379985,1437.53592823694));
#147871=CARTESIAN_POINT('Ctrl Pts',(13.3947726768058,12.2109487310903,1436.04181058988));
#147872=CARTESIAN_POINT('Ctrl Pts',(14.4026149179538,10.8763499173728,1434.54769294282));
#147873=CARTESIAN_POINT('Ctrl Pts',(15.4104571591017,9.54175110365538,1433.05357529576));
#147874=CARTESIAN_POINT('Ctrl Pts',(16.1559070823762,8.04468584505496,1431.5594576487));
#147875=CARTESIAN_POINT('Ctrl Pts',(16.9013570056506,6.54762058645456,1430.06534000164));
#147876=CARTESIAN_POINT('Ctrl Pts',(17.3590292079831,4.93906964482096,1428.57122235458));
#147877=CARTESIAN_POINT('Ctrl Pts',(17.8167014103155,3.33051870318735,1427.07710470753));
#147878=CARTESIAN_POINT('Ctrl Pts',(17.9710104137728,1.66525935159367,1425.58298706047));
#147879=CARTESIAN_POINT('Ctrl Pts',(18.1253194172301,3.32956716117513E-15,
1424.08886941341));
#147880=CARTESIAN_POINT('Ctrl Pts',(17.9710104137728,-1.66525935159367,
1422.59475176635));
#147881=CARTESIAN_POINT('Ctrl Pts',(17.8167014103155,-3.33051870318736,
1421.10063411929));
#147882=CARTESIAN_POINT('Ctrl Pts',(17.3590292079831,-4.93906964482095,
1419.60651647223));
#147883=CARTESIAN_POINT('Ctrl Pts',(16.9013570056506,-6.54762058645456,
1418.11239882517));
#147884=CARTESIAN_POINT('Ctrl Pts',(16.1559070823762,-8.04468584505497,
1416.61828117811));
#147885=CARTESIAN_POINT('Ctrl Pts',(15.4104571591017,-9.54175110365538,
1415.12416353105));
#147886=CARTESIAN_POINT('Ctrl Pts',(14.4026149179538,-10.8763499173728,
1413.630045884));
#147887=CARTESIAN_POINT('Ctrl Pts',(13.3947726768058,-12.2109487310903,
1412.13592823694));
#147888=CARTESIAN_POINT('Ctrl Pts',(12.1588589765331,-13.3376329379985,
1410.64181058988));
#147889=CARTESIAN_POINT('Ctrl Pts',(10.9229452762603,-14.4643171449067,
1409.14769294282));
#147890=CARTESIAN_POINT('Ctrl Pts',(9.50104767561053,-15.3447188656481,
1407.65357529576));
#147891=CARTESIAN_POINT('Ctrl Pts',(8.07915007496071,-16.2251205863895,
1406.1594576487));
#147892=CARTESIAN_POINT('Ctrl Pts',(6.51968959134574,-16.8292587962898,
1404.66534000164));
#147893=CARTESIAN_POINT('Ctrl Pts',(4.96022910773078,-17.4333970061901,
1403.17122235458));
#147894=CARTESIAN_POINT('Ctrl Pts',(3.31631129755346,-17.7406985030951,
1401.67710470753));
#147895=CARTESIAN_POINT('Ctrl Pts',(1.67239348737615,-18.048,1400.18298706047));
#147896=CARTESIAN_POINT('Ctrl Pts',(0.,-18.048,1398.68886941341));
#147897=CARTESIAN_POINT('Ctrl Pts',(-1.67239348737615,-18.048,1397.19475176635));
#147898=CARTESIAN_POINT('Ctrl Pts',(-3.31631129755346,-17.7406985030951,
1395.70063411929));
#147899=CARTESIAN_POINT('Ctrl Pts',(-4.96022910773077,-17.4333970061901,
1394.20651647223));
#147900=CARTESIAN_POINT('Ctrl Pts',(-6.51968959134574,-16.8292587962898,
1392.71239882517));
#147901=CARTESIAN_POINT('Ctrl Pts',(-8.07915007496071,-16.2251205863895,
1391.21828117811));
#147902=CARTESIAN_POINT('Ctrl Pts',(-9.50104767561052,-15.3447188656481,
1389.72416353105));
#147903=CARTESIAN_POINT('Ctrl Pts',(-10.9229452762603,-14.4643171449067,
1388.230045884));
#147904=CARTESIAN_POINT('Ctrl Pts',(-12.1588589765331,-13.3376329379985,
1386.73592823694));
#147905=CARTESIAN_POINT('Ctrl Pts',(-13.3947726768058,-12.2109487310903,
1385.24181058988));
#147906=CARTESIAN_POINT('Ctrl Pts',(-14.4026149179538,-10.8763499173728,
1383.74769294282));
#147907=CARTESIAN_POINT('Ctrl Pts',(-15.4104571591017,-9.54175110365538,
1382.25357529576));
#147908=CARTESIAN_POINT('Ctrl Pts',(-16.1559070823762,-8.04468584505497,
1380.7594576487));
#147909=CARTESIAN_POINT('Ctrl Pts',(-16.9013570056506,-6.54762058645456,
1379.26534000164));
#147910=CARTESIAN_POINT('Ctrl Pts',(-17.3590292079831,-4.93906964482095,
1377.77122235458));
#147911=CARTESIAN_POINT('Ctrl Pts',(-17.8167014103155,-3.33051870318735,
1376.27710470753));
#147912=CARTESIAN_POINT('Ctrl Pts',(-17.9710104137728,-1.66525935159368,
1374.78298706047));
#147913=CARTESIAN_POINT('Ctrl Pts',(-18.1253194172301,-1.10985572039171E-15,
1373.28886941341));
#147914=CARTESIAN_POINT('Ctrl Pts',(-17.9710104137728,1.66525935159367,
1371.79475176635));
#147915=CARTESIAN_POINT('Ctrl Pts',(-17.8167014103155,3.33051870318735,
1370.30063411929));
#147916=CARTESIAN_POINT('Ctrl Pts',(-17.3590292079831,4.93906964482096,
1368.80651647223));
#147917=CARTESIAN_POINT('Ctrl Pts',(-16.9013570056506,6.54762058645456,
1367.31239882517));
#147918=CARTESIAN_POINT('Ctrl Pts',(-16.1559070823762,8.04468584505497,
1365.81828117811));
#147919=CARTESIAN_POINT('Ctrl Pts',(-15.4104571591017,9.54175110365538,
1364.32416353105));
#147920=CARTESIAN_POINT('Ctrl Pts',(-14.4026149179538,10.8763499173728,
1362.830045884));
#147921=CARTESIAN_POINT('Ctrl Pts',(-13.3947726768058,12.2109487310903,
1361.33592823694));
#147922=CARTESIAN_POINT('Ctrl Pts',(-12.1588589765331,13.3376329379985,
1359.84181058988));
#147923=CARTESIAN_POINT('Ctrl Pts',(-10.9229452762603,14.4643171449067,
1358.34769294282));
#147924=CARTESIAN_POINT('Ctrl Pts',(-9.50104767561052,15.3447188656481,
1356.85357529576));
#147925=CARTESIAN_POINT('Ctrl Pts',(-8.07915007496071,16.2251205863895,
1355.3594576487));
#147926=CARTESIAN_POINT('Ctrl Pts',(-6.51968959134574,16.8292587962898,
1353.86534000164));
#147927=CARTESIAN_POINT('Ctrl Pts',(-4.96022910773078,17.4333970061901,
1352.37122235458));
#147928=CARTESIAN_POINT('Ctrl Pts',(-3.31631129755346,17.7406985030951,
1350.87710470753));
#147929=CARTESIAN_POINT('Ctrl Pts',(-1.67239348737615,18.048,1349.38298706047));
#147930=CARTESIAN_POINT('Ctrl Pts',(-2.21024254310115E-15,18.048,1347.88886941341));
#147931=CARTESIAN_POINT('Ctrl Pts',(1.67239348737616,18.048,1346.39475176635));
#147932=CARTESIAN_POINT('Ctrl Pts',(3.31631129755346,17.7406985030951,1344.90063411929));
#147933=CARTESIAN_POINT('Ctrl Pts',(4.96022910773077,17.4333970061901,1343.40651647223));
#147934=CARTESIAN_POINT('Ctrl Pts',(6.51968959134575,16.8292587962898,1341.91239882517));
#147935=CARTESIAN_POINT('Ctrl Pts',(8.07915007496071,16.2251205863895,1340.41828117811));
#147936=CARTESIAN_POINT('Ctrl Pts',(9.50104767561053,15.3447188656481,1338.92416353106));
#147937=CARTESIAN_POINT('Ctrl Pts',(10.9229452762603,14.4643171449067,1337.430045884));
#147938=CARTESIAN_POINT('Ctrl Pts',(12.1588589765331,13.3376329379985,1335.93592823694));
#147939=CARTESIAN_POINT('Ctrl Pts',(13.3947726768058,12.2109487310903,1334.44181058988));
#147940=CARTESIAN_POINT('Ctrl Pts',(14.4026149179538,10.8763499173728,1332.94769294282));
#147941=CARTESIAN_POINT('Ctrl Pts',(15.4104571591017,9.54175110365538,1331.45357529576));
#147942=CARTESIAN_POINT('Ctrl Pts',(16.1559070823762,8.04468584505496,1329.9594576487));
#147943=CARTESIAN_POINT('Ctrl Pts',(16.9013570056506,6.54762058645456,1328.46534000164));
#147944=CARTESIAN_POINT('Ctrl Pts',(17.3590292079831,4.93906964482096,1326.97122235458));
#147945=CARTESIAN_POINT('Ctrl Pts',(17.8167014103155,3.33051870318735,1325.47710470753));
#147946=CARTESIAN_POINT('Ctrl Pts',(17.9710104137728,1.66525935159367,1323.98298706047));
#147947=CARTESIAN_POINT('Ctrl Pts',(18.1253194172301,3.32956716117513E-15,
1322.48886941341));
#147948=CARTESIAN_POINT('Ctrl Pts',(17.9710104137728,-1.66525935159367,
1320.99475176635));
#147949=CARTESIAN_POINT('Ctrl Pts',(17.8167014103155,-3.33051870318736,
1319.50063411929));
#147950=CARTESIAN_POINT('Ctrl Pts',(17.3590292079831,-4.93906964482095,
1318.00651647223));
#147951=CARTESIAN_POINT('Ctrl Pts',(16.9013570056506,-6.54762058645456,
1316.51239882517));
#147952=CARTESIAN_POINT('Ctrl Pts',(16.1559070823762,-8.04468584505497,
1315.01828117811));
#147953=CARTESIAN_POINT('Ctrl Pts',(15.4104571591017,-9.54175110365538,
1313.52416353105));
#147954=CARTESIAN_POINT('Ctrl Pts',(14.4026149179538,-10.8763499173728,
1312.030045884));
#147955=CARTESIAN_POINT('Ctrl Pts',(13.3947726768058,-12.2109487310903,
1310.53592823694));
#147956=CARTESIAN_POINT('Ctrl Pts',(12.1588589765331,-13.3376329379985,
1309.04181058988));
#147957=CARTESIAN_POINT('Ctrl Pts',(10.9229452762603,-14.4643171449067,
1307.54769294282));
#147958=CARTESIAN_POINT('Ctrl Pts',(9.50104767561053,-15.3447188656481,
1306.05357529576));
#147959=CARTESIAN_POINT('Ctrl Pts',(8.07915007496071,-16.2251205863895,
1304.5594576487));
#147960=CARTESIAN_POINT('Ctrl Pts',(6.51968959134574,-16.8292587962898,
1303.06534000164));
#147961=CARTESIAN_POINT('Ctrl Pts',(4.96022910773078,-17.4333970061901,
1301.57122235458));
#147962=CARTESIAN_POINT('Ctrl Pts',(3.31631129755346,-17.7406985030951,
1300.07710470753));
#147963=CARTESIAN_POINT('Ctrl Pts',(1.67239348737615,-18.048,1298.58298706047));
#147964=CARTESIAN_POINT('Ctrl Pts',(0.,-18.048,1297.08886941341));
#147965=CARTESIAN_POINT('Ctrl Pts',(-1.67239348737615,-18.048,1295.59475176635));
#147966=CARTESIAN_POINT('Ctrl Pts',(-3.31631129755346,-17.7406985030951,
1294.10063411929));
#147967=CARTESIAN_POINT('Ctrl Pts',(-4.96022910773077,-17.4333970061901,
1292.60651647223));
#147968=CARTESIAN_POINT('Ctrl Pts',(-6.51968959134574,-16.8292587962898,
1291.11239882517));
#147969=CARTESIAN_POINT('Ctrl Pts',(-8.07915007496071,-16.2251205863895,
1289.61828117811));
#147970=CARTESIAN_POINT('Ctrl Pts',(-9.50104767561052,-15.3447188656481,
1288.12416353105));
#147971=CARTESIAN_POINT('Ctrl Pts',(-10.9229452762603,-14.4643171449067,
1286.630045884));
#147972=CARTESIAN_POINT('Ctrl Pts',(-12.1588589765331,-13.3376329379985,
1285.13592823694));
#147973=CARTESIAN_POINT('Ctrl Pts',(-13.3947726768058,-12.2109487310903,
1283.64181058988));
#147974=CARTESIAN_POINT('Ctrl Pts',(-14.4026149179538,-10.8763499173728,
1282.14769294282));
#147975=CARTESIAN_POINT('Ctrl Pts',(-15.4104571591017,-9.54175110365538,
1280.65357529576));
#147976=CARTESIAN_POINT('Ctrl Pts',(-16.1559070823762,-8.04468584505497,
1279.1594576487));
#147977=CARTESIAN_POINT('Ctrl Pts',(-16.9013570056506,-6.54762058645456,
1277.66534000164));
#147978=CARTESIAN_POINT('Ctrl Pts',(-17.3590292079831,-4.93906964482095,
1276.17122235458));
#147979=CARTESIAN_POINT('Ctrl Pts',(-17.8167014103155,-3.33051870318735,
1274.67710470753));
#147980=CARTESIAN_POINT('Ctrl Pts',(-17.9710104137728,-1.66525935159368,
1273.18298706047));
#147981=CARTESIAN_POINT('Ctrl Pts',(-18.1253194172301,-1.10985572039171E-15,
1271.68886941341));
#147982=CARTESIAN_POINT('Ctrl Pts',(-17.9710104137728,1.66525935159367,
1270.19475176635));
#147983=CARTESIAN_POINT('Ctrl Pts',(-17.8167014103155,3.33051870318735,
1268.70063411929));
#147984=CARTESIAN_POINT('Ctrl Pts',(-17.3590292079831,4.93906964482096,
1267.20651647223));
#147985=CARTESIAN_POINT('Ctrl Pts',(-16.9013570056506,6.54762058645456,
1265.71239882517));
#147986=CARTESIAN_POINT('Ctrl Pts',(-16.1559070823762,8.04468584505497,
1264.21828117811));
#147987=CARTESIAN_POINT('Ctrl Pts',(-15.4104571591017,9.54175110365538,
1262.72416353105));
#147988=CARTESIAN_POINT('Ctrl Pts',(-14.4026149179538,10.8763499173728,
1261.230045884));
#147989=CARTESIAN_POINT('Ctrl Pts',(-13.3947726768058,12.2109487310903,
1259.73592823694));
#147990=CARTESIAN_POINT('Ctrl Pts',(-12.1588589765331,13.3376329379985,
1258.24181058988));
#147991=CARTESIAN_POINT('Ctrl Pts',(-10.9229452762603,14.4643171449067,
1256.74769294282));
#147992=CARTESIAN_POINT('Ctrl Pts',(-9.50104767561052,15.3447188656481,
1255.25357529576));
#147993=CARTESIAN_POINT('Ctrl Pts',(-8.07915007496071,16.2251205863895,
1253.7594576487));
#147994=CARTESIAN_POINT('Ctrl Pts',(-6.51968959134574,16.8292587962898,
1252.26534000164));
#147995=CARTESIAN_POINT('Ctrl Pts',(-4.96022910773078,17.4333970061901,
1250.77122235458));
#147996=CARTESIAN_POINT('Ctrl Pts',(-3.31631129755346,17.7406985030951,
1249.27710470753));
#147997=CARTESIAN_POINT('Ctrl Pts',(-1.67239348737615,18.048,1247.78298706047));
#147998=CARTESIAN_POINT('Ctrl Pts',(-2.21024254310115E-15,18.048,1246.28886941341));
#147999=CARTESIAN_POINT('Ctrl Pts',(1.67239348737616,18.048,1244.79475176635));
#148000=CARTESIAN_POINT('Ctrl Pts',(3.31631129755346,17.7406985030951,1243.30063411929));
#148001=CARTESIAN_POINT('Ctrl Pts',(4.96022910773077,17.4333970061901,1241.80651647223));
#148002=CARTESIAN_POINT('Ctrl Pts',(6.51968959134575,16.8292587962898,1240.31239882517));
#148003=CARTESIAN_POINT('Ctrl Pts',(8.07915007496071,16.2251205863895,1238.81828117811));
#148004=CARTESIAN_POINT('Ctrl Pts',(9.50104767561053,15.3447188656481,1237.32416353105));
#148005=CARTESIAN_POINT('Ctrl Pts',(10.9229452762603,14.4643171449067,1235.830045884));
#148006=CARTESIAN_POINT('Ctrl Pts',(12.1588589765331,13.3376329379985,1234.33592823694));
#148007=CARTESIAN_POINT('Ctrl Pts',(13.3947726768058,12.2109487310903,1232.84181058988));
#148008=CARTESIAN_POINT('Ctrl Pts',(14.4026149179538,10.8763499173728,1231.34769294282));
#148009=CARTESIAN_POINT('Ctrl Pts',(15.4104571591017,9.54175110365538,1229.85357529576));
#148010=CARTESIAN_POINT('Ctrl Pts',(16.1559070823762,8.04468584505496,1228.3594576487));
#148011=CARTESIAN_POINT('Ctrl Pts',(16.9013570056506,6.54762058645456,1226.86534000164));
#148012=CARTESIAN_POINT('Ctrl Pts',(17.3590292079831,4.93906964482096,1225.37122235458));
#148013=CARTESIAN_POINT('Ctrl Pts',(17.8167014103155,3.33051870318735,1223.87710470753));
#148014=CARTESIAN_POINT('Ctrl Pts',(17.9710104137728,1.66525935159367,1222.38298706047));
#148015=CARTESIAN_POINT('Ctrl Pts',(18.1253194172301,3.32956716117513E-15,
1220.88886941341));
#148016=CARTESIAN_POINT('Ctrl Pts',(17.9710104137728,-1.66525935159367,
1219.39475176635));
#148017=CARTESIAN_POINT('Ctrl Pts',(17.8167014103155,-3.33051870318736,
1217.90063411929));
#148018=CARTESIAN_POINT('Ctrl Pts',(17.3590292079831,-4.93906964482095,
1216.40651647223));
#148019=CARTESIAN_POINT('Ctrl Pts',(16.9013570056506,-6.54762058645456,
1214.91239882517));
#148020=CARTESIAN_POINT('Ctrl Pts',(16.1559070823762,-8.04468584505497,
1213.41828117811));
#148021=CARTESIAN_POINT('Ctrl Pts',(15.4104571591017,-9.54175110365538,
1211.92416353105));
#148022=CARTESIAN_POINT('Ctrl Pts',(14.4026149179538,-10.8763499173728,
1210.430045884));
#148023=CARTESIAN_POINT('Ctrl Pts',(13.3947726768058,-12.2109487310903,
1208.93592823694));
#148024=CARTESIAN_POINT('Ctrl Pts',(12.1588589765331,-13.3376329379985,
1207.44181058988));
#148025=CARTESIAN_POINT('Ctrl Pts',(10.9229452762603,-14.4643171449067,
1205.94769294282));
#148026=CARTESIAN_POINT('Ctrl Pts',(9.50104767561053,-15.3447188656481,
1204.45357529576));
#148027=CARTESIAN_POINT('Ctrl Pts',(8.07915007496071,-16.2251205863895,
1202.9594576487));
#148028=CARTESIAN_POINT('Ctrl Pts',(6.51968959134574,-16.8292587962898,
1201.46534000164));
#148029=CARTESIAN_POINT('Ctrl Pts',(4.96022910773078,-17.4333970061901,
1199.97122235458));
#148030=CARTESIAN_POINT('Ctrl Pts',(3.31631129755346,-17.7406985030951,
1198.47710470753));
#148031=CARTESIAN_POINT('Ctrl Pts',(1.67239348737615,-18.048,1196.98298706047));
#148032=CARTESIAN_POINT('Ctrl Pts',(0.,-18.048,1195.48886941341));
#148033=CARTESIAN_POINT('Ctrl Pts',(-1.67239348737615,-18.048,1193.99475176635));
#148034=CARTESIAN_POINT('Ctrl Pts',(-3.31631129755346,-17.7406985030951,
1192.50063411929));
#148035=CARTESIAN_POINT('Ctrl Pts',(-4.96022910773077,-17.4333970061901,
1191.00651647223));
#148036=CARTESIAN_POINT('Ctrl Pts',(-6.51968959134574,-16.8292587962898,
1189.51239882517));
#148037=CARTESIAN_POINT('Ctrl Pts',(-8.07915007496071,-16.2251205863895,
1188.01828117811));
#148038=CARTESIAN_POINT('Ctrl Pts',(-9.50104767561052,-15.3447188656481,
1186.52416353105));
#148039=CARTESIAN_POINT('Ctrl Pts',(-10.9229452762603,-14.4643171449067,
1185.030045884));
#148040=CARTESIAN_POINT('Ctrl Pts',(-12.1588589765331,-13.3376329379985,
1183.53592823694));
#148041=CARTESIAN_POINT('Ctrl Pts',(-13.3947726768058,-12.2109487310903,
1182.04181058988));
#148042=CARTESIAN_POINT('Ctrl Pts',(-14.4026149179538,-10.8763499173728,
1180.54769294282));
#148043=CARTESIAN_POINT('Ctrl Pts',(-15.4104571591017,-9.54175110365538,
1179.05357529576));
#148044=CARTESIAN_POINT('Ctrl Pts',(-16.1559070823762,-8.04468584505497,
1177.5594576487));
#148045=CARTESIAN_POINT('Ctrl Pts',(-16.9013570056506,-6.54762058645456,
1176.06534000164));
#148046=CARTESIAN_POINT('Ctrl Pts',(-17.3590292079831,-4.93906964482095,
1174.57122235458));
#148047=CARTESIAN_POINT('Ctrl Pts',(-17.8167014103155,-3.33051870318735,
1173.07710470753));
#148048=CARTESIAN_POINT('Ctrl Pts',(-17.9710104137728,-1.66525935159368,
1171.58298706047));
#148049=CARTESIAN_POINT('Ctrl Pts',(-18.1253194172301,-1.10985572039171E-15,
1170.08886941341));
#148050=CARTESIAN_POINT('Ctrl Pts',(-17.9710104137728,1.66525935159367,
1168.59475176635));
#148051=CARTESIAN_POINT('Ctrl Pts',(-17.8167014103155,3.33051870318735,
1167.10063411929));
#148052=CARTESIAN_POINT('Ctrl Pts',(-17.3590292079831,4.93906964482096,
1165.60651647223));
#148053=CARTESIAN_POINT('Ctrl Pts',(-16.9013570056506,6.54762058645456,
1164.11239882517));
#148054=CARTESIAN_POINT('Ctrl Pts',(-16.1559070823762,8.04468584505497,
1162.61828117811));
#148055=CARTESIAN_POINT('Ctrl Pts',(-15.4104571591017,9.54175110365538,
1161.12416353106));
#148056=CARTESIAN_POINT('Ctrl Pts',(-14.4026149179538,10.8763499173728,
1159.630045884));
#148057=CARTESIAN_POINT('Ctrl Pts',(-13.3947726768058,12.2109487310903,
1158.13592823694));
#148058=CARTESIAN_POINT('Ctrl Pts',(-12.1588589765331,13.3376329379985,
1156.64181058988));
#148059=CARTESIAN_POINT('Ctrl Pts',(-10.9229452762603,14.4643171449067,
1155.14769294282));
#148060=CARTESIAN_POINT('Ctrl Pts',(-9.50104767561052,15.3447188656481,
1153.65357529576));
#148061=CARTESIAN_POINT('Ctrl Pts',(-8.07915007496071,16.2251205863895,
1152.1594576487));
#148062=CARTESIAN_POINT('Ctrl Pts',(-6.51968959134574,16.8292587962898,
1150.66534000164));
#148063=CARTESIAN_POINT('Ctrl Pts',(-4.96022910773078,17.4333970061901,
1149.17122235458));
#148064=CARTESIAN_POINT('Ctrl Pts',(-3.31631129755346,17.7406985030951,
1147.67710470753));
#148065=CARTESIAN_POINT('Ctrl Pts',(-1.67239348737615,18.048,1146.18298706047));
#148066=CARTESIAN_POINT('Ctrl Pts',(-2.21024254310115E-15,18.048,1144.68886941341));
#148067=CARTESIAN_POINT('Ctrl Pts',(1.67239348737616,18.048,1143.19475176635));
#148068=CARTESIAN_POINT('Ctrl Pts',(3.31631129755346,17.7406985030951,1141.70063411929));
#148069=CARTESIAN_POINT('Ctrl Pts',(4.96022910773077,17.4333970061901,1140.20651647223));
#148070=CARTESIAN_POINT('Ctrl Pts',(6.51968959134575,16.8292587962898,1138.71239882517));
#148071=CARTESIAN_POINT('Ctrl Pts',(8.07915007496071,16.2251205863895,1137.21828117811));
#148072=CARTESIAN_POINT('Ctrl Pts',(9.50104767561053,15.3447188656481,1135.72416353105));
#148073=CARTESIAN_POINT('Ctrl Pts',(10.9229452762603,14.4643171449067,1134.230045884));
#148074=CARTESIAN_POINT('Ctrl Pts',(12.1588589765331,13.3376329379985,1132.73592823694));
#148075=CARTESIAN_POINT('Ctrl Pts',(13.3947726768058,12.2109487310903,1131.24181058988));
#148076=CARTESIAN_POINT('Ctrl Pts',(14.4026149179538,10.8763499173728,1129.74769294282));
#148077=CARTESIAN_POINT('Ctrl Pts',(15.4104571591017,9.54175110365538,1128.25357529576));
#148078=CARTESIAN_POINT('Ctrl Pts',(16.1559070823762,8.04468584505496,1126.7594576487));
#148079=CARTESIAN_POINT('Ctrl Pts',(16.9013570056506,6.54762058645456,1125.26534000164));
#148080=CARTESIAN_POINT('Ctrl Pts',(17.3590292079831,4.93906964482096,1123.77122235458));
#148081=CARTESIAN_POINT('Ctrl Pts',(17.8167014103155,3.33051870318735,1122.27710470753));
#148082=CARTESIAN_POINT('Ctrl Pts',(17.9710104137728,1.66525935159367,1120.78298706047));
#148083=CARTESIAN_POINT('Ctrl Pts',(18.1253194172301,3.32956716117513E-15,
1119.28886941341));
#148084=CARTESIAN_POINT('Ctrl Pts',(17.9710104137728,-1.66525935159367,
1117.79475176635));
#148085=CARTESIAN_POINT('Ctrl Pts',(17.8167014103155,-3.33051870318736,
1116.30063411929));
#148086=CARTESIAN_POINT('Ctrl Pts',(17.3590292079831,-4.93906964482095,
1114.80651647223));
#148087=CARTESIAN_POINT('Ctrl Pts',(16.9013570056506,-6.54762058645456,
1113.31239882517));
#148088=CARTESIAN_POINT('Ctrl Pts',(16.1559070823762,-8.04468584505497,
1111.81828117811));
#148089=CARTESIAN_POINT('Ctrl Pts',(15.4104571591017,-9.54175110365538,
1110.32416353105));
#148090=CARTESIAN_POINT('Ctrl Pts',(14.4026149179538,-10.8763499173728,
1108.830045884));
#148091=CARTESIAN_POINT('Ctrl Pts',(13.3947726768058,-12.2109487310903,
1107.33592823694));
#148092=CARTESIAN_POINT('Ctrl Pts',(12.1588589765331,-13.3376329379985,
1105.84181058988));
#148093=CARTESIAN_POINT('Ctrl Pts',(10.9229452762603,-14.4643171449067,
1104.34769294282));
#148094=CARTESIAN_POINT('Ctrl Pts',(9.50104767561053,-15.3447188656481,
1102.85357529576));
#148095=CARTESIAN_POINT('Ctrl Pts',(8.07915007496071,-16.2251205863895,
1101.3594576487));
#148096=CARTESIAN_POINT('Ctrl Pts',(6.51968959134574,-16.8292587962898,
1099.86534000164));
#148097=CARTESIAN_POINT('Ctrl Pts',(4.96022910773078,-17.4333970061901,
1098.37122235458));
#148098=CARTESIAN_POINT('Ctrl Pts',(3.31631129755346,-17.7406985030951,
1096.87710470753));
#148099=CARTESIAN_POINT('Ctrl Pts',(1.67239348737615,-18.048,1095.38298706047));
#148100=CARTESIAN_POINT('Ctrl Pts',(0.,-18.048,1093.88886941341));
#148101=CARTESIAN_POINT('Ctrl Pts',(-1.67239348737615,-18.048,1092.39475176635));
#148102=CARTESIAN_POINT('Ctrl Pts',(-3.31631129755346,-17.7406985030951,
1090.90063411929));
#148103=CARTESIAN_POINT('Ctrl Pts',(-4.96022910773077,-17.4333970061901,
1089.40651647223));
#148104=CARTESIAN_POINT('Ctrl Pts',(-6.51968959134574,-16.8292587962898,
1087.91239882517));
#148105=CARTESIAN_POINT('Ctrl Pts',(-8.07915007496071,-16.2251205863895,
1086.41828117811));
#148106=CARTESIAN_POINT('Ctrl Pts',(-9.50104767561052,-15.3447188656481,
1084.92416353106));
#148107=CARTESIAN_POINT('Ctrl Pts',(-10.9229452762603,-14.4643171449067,
1083.430045884));
#148108=CARTESIAN_POINT('Ctrl Pts',(-12.1588589765331,-13.3376329379985,
1081.93592823694));
#148109=CARTESIAN_POINT('Ctrl Pts',(-13.3947726768058,-12.2109487310903,
1080.44181058988));
#148110=CARTESIAN_POINT('Ctrl Pts',(-14.4026149179538,-10.8763499173728,
1078.94769294282));
#148111=CARTESIAN_POINT('Ctrl Pts',(-15.4104571591017,-9.54175110365538,
1077.45357529576));
#148112=CARTESIAN_POINT('Ctrl Pts',(-16.1559070823762,-8.04468584505497,
1075.9594576487));
#148113=CARTESIAN_POINT('Ctrl Pts',(-16.9013570056506,-6.54762058645456,
1074.46534000164));
#148114=CARTESIAN_POINT('Ctrl Pts',(-17.3590292079831,-4.93906964482095,
1072.97122235458));
#148115=CARTESIAN_POINT('Ctrl Pts',(-17.8167014103155,-3.33051870318735,
1071.47710470753));
#148116=CARTESIAN_POINT('Ctrl Pts',(-17.9710104137728,-1.66525935159368,
1069.98298706047));
#148117=CARTESIAN_POINT('Ctrl Pts',(-18.1253194172301,-1.10985572039171E-15,
1068.48886941341));
#148118=CARTESIAN_POINT('Ctrl Pts',(-17.9710104137728,1.66525935159367,
1066.99475176635));
#148119=CARTESIAN_POINT('Ctrl Pts',(-17.8167014103155,3.33051870318735,
1065.50063411929));
#148120=CARTESIAN_POINT('Ctrl Pts',(-17.3590292079831,4.93906964482096,
1064.00651647223));
#148121=CARTESIAN_POINT('Ctrl Pts',(-16.9013570056506,6.54762058645456,
1062.51239882517));
#148122=CARTESIAN_POINT('Ctrl Pts',(-16.1559070823762,8.04468584505497,
1061.01828117811));
#148123=CARTESIAN_POINT('Ctrl Pts',(-15.4104571591017,9.54175110365538,
1059.52416353105));
#148124=CARTESIAN_POINT('Ctrl Pts',(-14.4026149179538,10.8763499173728,
1058.030045884));
#148125=CARTESIAN_POINT('Ctrl Pts',(-13.3947726768058,12.2109487310903,
1056.53592823694));
#148126=CARTESIAN_POINT('Ctrl Pts',(-12.1588589765331,13.3376329379985,
1055.04181058988));
#148127=CARTESIAN_POINT('Ctrl Pts',(-10.9229452762603,14.4643171449067,
1053.54769294282));
#148128=CARTESIAN_POINT('Ctrl Pts',(-9.50104767561052,15.3447188656481,
1052.05357529576));
#148129=CARTESIAN_POINT('Ctrl Pts',(-8.07915007496071,16.2251205863895,
1050.5594576487));
#148130=CARTESIAN_POINT('Ctrl Pts',(-6.51968959134574,16.8292587962898,
1049.06534000164));
#148131=CARTESIAN_POINT('Ctrl Pts',(-4.96022910773078,17.4333970061901,
1047.57122235458));
#148132=CARTESIAN_POINT('Ctrl Pts',(-3.31631129755346,17.7406985030951,
1046.07710470753));
#148133=CARTESIAN_POINT('Ctrl Pts',(-1.67239348737615,18.048,1044.58298706047));
#148134=CARTESIAN_POINT('Ctrl Pts',(-2.21024254310115E-15,18.048,1043.08886941341));
#148135=CARTESIAN_POINT('Ctrl Pts',(1.67239348737616,18.048,1041.59475176635));
#148136=CARTESIAN_POINT('Ctrl Pts',(3.31631129755346,17.7406985030951,1040.10063411929));
#148137=CARTESIAN_POINT('Ctrl Pts',(4.96022910773077,17.4333970061901,1038.60651647223));
#148138=CARTESIAN_POINT('Ctrl Pts',(6.51968959134575,16.8292587962898,1037.11239882517));
#148139=CARTESIAN_POINT('Ctrl Pts',(8.07915007496071,16.2251205863895,1035.61828117811));
#148140=CARTESIAN_POINT('Ctrl Pts',(9.50104767561053,15.3447188656481,1034.12416353105));
#148141=CARTESIAN_POINT('Ctrl Pts',(10.9229452762603,14.4643171449067,1032.630045884));
#148142=CARTESIAN_POINT('Ctrl Pts',(12.1588589765331,13.3376329379985,1031.13592823694));
#148143=CARTESIAN_POINT('Ctrl Pts',(13.3947726768058,12.2109487310903,1029.64181058988));
#148144=CARTESIAN_POINT('Ctrl Pts',(14.4026149179538,10.8763499173728,1028.14769294282));
#148145=CARTESIAN_POINT('Ctrl Pts',(15.4104571591017,9.54175110365538,1026.65357529576));
#148146=CARTESIAN_POINT('Ctrl Pts',(16.1559070823762,8.04468584505496,1025.1594576487));
#148147=CARTESIAN_POINT('Ctrl Pts',(16.9013570056506,6.54762058645456,1023.66534000164));
#148148=CARTESIAN_POINT('Ctrl Pts',(17.3590292079831,4.93906964482096,1022.17122235458));
#148149=CARTESIAN_POINT('Ctrl Pts',(17.8167014103155,3.33051870318735,1020.67710470753));
#148150=CARTESIAN_POINT('Ctrl Pts',(17.9710104137728,1.66525935159367,1019.18298706047));
#148151=CARTESIAN_POINT('Ctrl Pts',(18.1253194172301,3.32956716117513E-15,
1017.68886941341));
#148152=CARTESIAN_POINT('Ctrl Pts',(17.9710104137728,-1.66525935159367,
1016.19475176635));
#148153=CARTESIAN_POINT('Ctrl Pts',(17.8167014103155,-3.33051870318736,
1014.70063411929));
#148154=CARTESIAN_POINT('Ctrl Pts',(17.3590292079831,-4.93906964482095,
1013.20651647223));
#148155=CARTESIAN_POINT('Ctrl Pts',(16.9013570056506,-6.54762058645456,
1011.71239882517));
#148156=CARTESIAN_POINT('Ctrl Pts',(16.1559070823762,-8.04468584505497,
1010.21828117811));
#148157=CARTESIAN_POINT('Ctrl Pts',(15.4104571591017,-9.54175110365538,
1008.72416353105));
#148158=CARTESIAN_POINT('Ctrl Pts',(14.4026149179538,-10.8763499173728,
1007.230045884));
#148159=CARTESIAN_POINT('Ctrl Pts',(13.3947726768058,-12.2109487310903,
1005.73592823694));
#148160=CARTESIAN_POINT('Ctrl Pts',(12.1588589765331,-13.3376329379985,
1004.24181058988));
#148161=CARTESIAN_POINT('Ctrl Pts',(10.9229452762603,-14.4643171449067,
1002.74769294282));
#148162=CARTESIAN_POINT('Ctrl Pts',(9.50104767561053,-15.3447188656481,
1001.25357529576));
#148163=CARTESIAN_POINT('Ctrl Pts',(8.07915007496071,-16.2251205863895,
999.759457648702));
#148164=CARTESIAN_POINT('Ctrl Pts',(6.51968959134574,-16.8292587962898,
998.265340001643));
#148165=CARTESIAN_POINT('Ctrl Pts',(4.96022910773078,-17.4333970061901,
996.771222354585));
#148166=CARTESIAN_POINT('Ctrl Pts',(3.31631129755346,-17.7406985030951,
995.277104707525));
#148167=CARTESIAN_POINT('Ctrl Pts',(1.67239348737615,-18.048,993.782987060467));
#148168=CARTESIAN_POINT('Ctrl Pts',(0.,-18.048,992.288869413408));
#148169=CARTESIAN_POINT('Ctrl Pts',(-1.67239348737615,-18.048,990.794751766349));
#148170=CARTESIAN_POINT('Ctrl Pts',(-3.31631129755346,-17.7406985030951,
989.30063411929));
#148171=CARTESIAN_POINT('Ctrl Pts',(-4.96022910773077,-17.4333970061901,
987.806516472232));
#148172=CARTESIAN_POINT('Ctrl Pts',(-6.51968959134574,-16.8292587962898,
986.312398825173));
#148173=CARTESIAN_POINT('Ctrl Pts',(-8.07915007496071,-16.2251205863895,
984.818281178114));
#148174=CARTESIAN_POINT('Ctrl Pts',(-9.50104767561052,-15.3447188656481,
983.324163531055));
#148175=CARTESIAN_POINT('Ctrl Pts',(-10.9229452762603,-14.4643171449067,
981.830045883996));
#148176=CARTESIAN_POINT('Ctrl Pts',(-12.1588589765331,-13.3376329379985,
980.335928236937));
#148177=CARTESIAN_POINT('Ctrl Pts',(-13.3947726768058,-12.2109487310903,
978.841810589878));
#148178=CARTESIAN_POINT('Ctrl Pts',(-14.4026149179538,-10.8763499173728,
977.34769294282));
#148179=CARTESIAN_POINT('Ctrl Pts',(-15.4104571591017,-9.54175110365538,
975.853575295761));
#148180=CARTESIAN_POINT('Ctrl Pts',(-16.1559070823762,-8.04468584505497,
974.359457648702));
#148181=CARTESIAN_POINT('Ctrl Pts',(-16.9013570056506,-6.54762058645456,
972.865340001643));
#148182=CARTESIAN_POINT('Ctrl Pts',(-17.3590292079831,-4.93906964482095,
971.371222354584));
#148183=CARTESIAN_POINT('Ctrl Pts',(-17.8167014103155,-3.33051870318735,
969.877104707525));
#148184=CARTESIAN_POINT('Ctrl Pts',(-17.9710104137728,-1.66525935159368,
968.382987060467));
#148185=CARTESIAN_POINT('Ctrl Pts',(-18.1253194172301,-1.10985572039171E-15,
966.888869413408));
#148186=CARTESIAN_POINT('Ctrl Pts',(-17.9710104137728,1.66525935159367,
965.394751766349));
#148187=CARTESIAN_POINT('Ctrl Pts',(-17.8167014103155,3.33051870318735,
963.90063411929));
#148188=CARTESIAN_POINT('Ctrl Pts',(-17.3590292079831,4.93906964482096,
962.406516472231));
#148189=CARTESIAN_POINT('Ctrl Pts',(-16.9013570056506,6.54762058645456,
960.912398825173));
#148190=CARTESIAN_POINT('Ctrl Pts',(-16.1559070823762,8.04468584505497,
959.418281178114));
#148191=CARTESIAN_POINT('Ctrl Pts',(-15.4104571591017,9.54175110365538,
957.924163531055));
#148192=CARTESIAN_POINT('Ctrl Pts',(-14.4026149179538,10.8763499173728,
956.430045883996));
#148193=CARTESIAN_POINT('Ctrl Pts',(-13.3947726768058,12.2109487310903,
954.935928236937));
#148194=CARTESIAN_POINT('Ctrl Pts',(-12.1588589765331,13.3376329379985,
953.441810589878));
#148195=CARTESIAN_POINT('Ctrl Pts',(-10.9229452762603,14.4643171449067,
951.94769294282));
#148196=CARTESIAN_POINT('Ctrl Pts',(-9.50104767561052,15.3447188656481,
950.453575295761));
#148197=CARTESIAN_POINT('Ctrl Pts',(-8.07915007496071,16.2251205863895,
948.959457648702));
#148198=CARTESIAN_POINT('Ctrl Pts',(-6.51968959134574,16.8292587962898,
947.465340001643));
#148199=CARTESIAN_POINT('Ctrl Pts',(-4.96022910773078,17.4333970061901,
945.971222354585));
#148200=CARTESIAN_POINT('Ctrl Pts',(-3.31631129755346,17.7406985030951,
944.477104707526));
#148201=CARTESIAN_POINT('Ctrl Pts',(-1.67239348737615,18.048,942.982987060467));
#148202=CARTESIAN_POINT('Ctrl Pts',(-2.21024254310115E-15,18.048,941.488869413408));
#148203=CARTESIAN_POINT('Ctrl Pts',(1.67239348737616,18.048,939.994751766349));
#148204=CARTESIAN_POINT('Ctrl Pts',(3.31631129755346,17.7406985030951,938.50063411929));
#148205=CARTESIAN_POINT('Ctrl Pts',(4.96022910773077,17.4333970061901,937.006516472232));
#148206=CARTESIAN_POINT('Ctrl Pts',(6.51968959134575,16.8292587962898,935.512398825173));
#148207=CARTESIAN_POINT('Ctrl Pts',(8.07915007496071,16.2251205863895,934.018281178114));
#148208=CARTESIAN_POINT('Ctrl Pts',(9.50104767561053,15.3447188656481,932.524163531055));
#148209=CARTESIAN_POINT('Ctrl Pts',(10.9229452762603,14.4643171449067,931.030045883996));
#148210=CARTESIAN_POINT('Ctrl Pts',(12.1588589765331,13.3376329379985,929.535928236937));
#148211=CARTESIAN_POINT('Ctrl Pts',(13.3947726768058,12.2109487310903,928.041810589879));
#148212=CARTESIAN_POINT('Ctrl Pts',(14.4026149179538,10.8763499173728,926.54769294282));
#148213=CARTESIAN_POINT('Ctrl Pts',(15.4104571591017,9.54175110365538,925.053575295761));
#148214=CARTESIAN_POINT('Ctrl Pts',(16.1559070823762,8.04468584505496,923.559457648702));
#148215=CARTESIAN_POINT('Ctrl Pts',(16.9013570056506,6.54762058645456,922.065340001643));
#148216=CARTESIAN_POINT('Ctrl Pts',(17.3590292079831,4.93906964482096,920.571222354584));
#148217=CARTESIAN_POINT('Ctrl Pts',(17.8167014103155,3.33051870318735,919.077104707525));
#148218=CARTESIAN_POINT('Ctrl Pts',(17.9710104137728,1.66525935159367,917.582987060467));
#148219=CARTESIAN_POINT('Ctrl Pts',(18.1253194172301,3.32956716117513E-15,
916.088869413408));
#148220=CARTESIAN_POINT('Ctrl Pts',(17.9710104137728,-1.66525935159367,
914.594751766349));
#148221=CARTESIAN_POINT('Ctrl Pts',(17.8167014103155,-3.33051870318736,
913.10063411929));
#148222=CARTESIAN_POINT('Ctrl Pts',(17.3590292079831,-4.93906964482095,
911.606516472231));
#148223=CARTESIAN_POINT('Ctrl Pts',(16.9013570056506,-6.54762058645456,
910.112398825173));
#148224=CARTESIAN_POINT('Ctrl Pts',(16.1559070823762,-8.04468584505497,
908.618281178114));
#148225=CARTESIAN_POINT('Ctrl Pts',(15.4104571591017,-9.54175110365538,
907.124163531055));
#148226=CARTESIAN_POINT('Ctrl Pts',(14.4026149179538,-10.8763499173728,
905.630045883996));
#148227=CARTESIAN_POINT('Ctrl Pts',(13.3947726768058,-12.2109487310903,
904.135928236937));
#148228=CARTESIAN_POINT('Ctrl Pts',(12.1588589765331,-13.3376329379985,
902.641810589878));
#148229=CARTESIAN_POINT('Ctrl Pts',(10.9229452762603,-14.4643171449067,
901.14769294282));
#148230=CARTESIAN_POINT('Ctrl Pts',(9.50104767561053,-15.3447188656481,
899.653575295761));
#148231=CARTESIAN_POINT('Ctrl Pts',(8.07915007496071,-16.2251205863895,
898.159457648702));
#148232=CARTESIAN_POINT('Ctrl Pts',(6.51968959134574,-16.8292587962898,
896.665340001643));
#148233=CARTESIAN_POINT('Ctrl Pts',(4.96022910773078,-17.4333970061901,
895.171222354584));
#148234=CARTESIAN_POINT('Ctrl Pts',(3.31631129755346,-17.7406985030951,
893.677104707526));
#148235=CARTESIAN_POINT('Ctrl Pts',(1.67239348737615,-18.048,892.182987060467));
#148236=CARTESIAN_POINT('Ctrl Pts',(0.,-18.048,890.688869413408));
#148237=CARTESIAN_POINT('Ctrl Pts',(-1.67239348737615,-18.048,889.194751766349));
#148238=CARTESIAN_POINT('Ctrl Pts',(-3.31631129755346,-17.7406985030951,
887.70063411929));
#148239=CARTESIAN_POINT('Ctrl Pts',(-4.96022910773077,-17.4333970061901,
886.206516472232));
#148240=CARTESIAN_POINT('Ctrl Pts',(-6.51968959134574,-16.8292587962898,
884.712398825172));
#148241=CARTESIAN_POINT('Ctrl Pts',(-8.07915007496071,-16.2251205863895,
883.218281178114));
#148242=CARTESIAN_POINT('Ctrl Pts',(-9.50104767561052,-15.3447188656481,
881.724163531055));
#148243=CARTESIAN_POINT('Ctrl Pts',(-10.9229452762603,-14.4643171449067,
880.230045883996));
#148244=CARTESIAN_POINT('Ctrl Pts',(-12.1588589765331,-13.3376329379985,
878.735928236937));
#148245=CARTESIAN_POINT('Ctrl Pts',(-13.3947726768058,-12.2109487310903,
877.241810589879));
#148246=CARTESIAN_POINT('Ctrl Pts',(-14.4026149179538,-10.8763499173728,
875.74769294282));
#148247=CARTESIAN_POINT('Ctrl Pts',(-15.4104571591017,-9.54175110365538,
874.253575295761));
#148248=CARTESIAN_POINT('Ctrl Pts',(-16.1559070823762,-8.04468584505497,
872.759457648702));
#148249=CARTESIAN_POINT('Ctrl Pts',(-16.9013570056506,-6.54762058645456,
871.265340001643));
#148250=CARTESIAN_POINT('Ctrl Pts',(-17.3590292079831,-4.93906964482095,
869.771222354584));
#148251=CARTESIAN_POINT('Ctrl Pts',(-17.8167014103155,-3.33051870318735,
868.277104707525));
#148252=CARTESIAN_POINT('Ctrl Pts',(-17.9710104137728,-1.66525935159368,
866.782987060467));
#148253=CARTESIAN_POINT('Ctrl Pts',(-18.1253194172301,-1.10985572039171E-15,
865.288869413408));
#148254=CARTESIAN_POINT('Ctrl Pts',(-17.9710104137728,1.66525935159367,
863.794751766349));
#148255=CARTESIAN_POINT('Ctrl Pts',(-17.8167014103155,3.33051870318735,
862.30063411929));
#148256=CARTESIAN_POINT('Ctrl Pts',(-17.3590292079831,4.93906964482096,
860.806516472231));
#148257=CARTESIAN_POINT('Ctrl Pts',(-16.9013570056506,6.54762058645456,
859.312398825173));
#148258=CARTESIAN_POINT('Ctrl Pts',(-16.1559070823762,8.04468584505497,
857.818281178114));
#148259=CARTESIAN_POINT('Ctrl Pts',(-15.4104571591017,9.54175110365538,
856.324163531055));
#148260=CARTESIAN_POINT('Ctrl Pts',(-14.4026149179538,10.8763499173728,
854.830045883996));
#148261=CARTESIAN_POINT('Ctrl Pts',(-13.3947726768058,12.2109487310903,
853.335928236937));
#148262=CARTESIAN_POINT('Ctrl Pts',(-12.1588589765331,13.3376329379985,
851.841810589878));
#148263=CARTESIAN_POINT('Ctrl Pts',(-10.9229452762603,14.4643171449067,
850.34769294282));
#148264=CARTESIAN_POINT('Ctrl Pts',(-9.50104767561052,15.3447188656481,
848.853575295761));
#148265=CARTESIAN_POINT('Ctrl Pts',(-8.07915007496071,16.2251205863895,
847.359457648702));
#148266=CARTESIAN_POINT('Ctrl Pts',(-6.51968959134574,16.8292587962898,
845.865340001643));
#148267=CARTESIAN_POINT('Ctrl Pts',(-4.96022910773078,17.4333970061901,
844.371222354584));
#148268=CARTESIAN_POINT('Ctrl Pts',(-3.31631129755346,17.7406985030951,
842.877104707525));
#148269=CARTESIAN_POINT('Ctrl Pts',(-1.67239348737615,18.048,841.382987060467));
#148270=CARTESIAN_POINT('Ctrl Pts',(-2.21024254310115E-15,18.048,839.888869413408));
#148271=CARTESIAN_POINT('Ctrl Pts',(1.67239348737616,18.048,838.394751766349));
#148272=CARTESIAN_POINT('Ctrl Pts',(3.31631129755346,17.7406985030951,836.90063411929));
#148273=CARTESIAN_POINT('Ctrl Pts',(4.96022910773077,17.4333970061901,835.406516472232));
#148274=CARTESIAN_POINT('Ctrl Pts',(6.51968959134575,16.8292587962898,833.912398825173));
#148275=CARTESIAN_POINT('Ctrl Pts',(8.07915007496071,16.2251205863895,832.418281178114));
#148276=CARTESIAN_POINT('Ctrl Pts',(9.50104767561053,15.3447188656481,830.924163531055));
#148277=CARTESIAN_POINT('Ctrl Pts',(10.9229452762603,14.4643171449067,829.430045883996));
#148278=CARTESIAN_POINT('Ctrl Pts',(12.1588589765331,13.3376329379985,827.935928236937));
#148279=CARTESIAN_POINT('Ctrl Pts',(13.3947726768058,12.2109487310903,826.441810589879));
#148280=CARTESIAN_POINT('Ctrl Pts',(14.4026149179538,10.8763499173728,824.94769294282));
#148281=CARTESIAN_POINT('Ctrl Pts',(15.4104571591017,9.54175110365538,823.453575295761));
#148282=CARTESIAN_POINT('Ctrl Pts',(16.1559070823762,8.04468584505496,821.959457648702));
#148283=CARTESIAN_POINT('Ctrl Pts',(16.9013570056506,6.54762058645456,820.465340001643));
#148284=CARTESIAN_POINT('Ctrl Pts',(17.3590292079831,4.93906964482096,818.971222354584));
#148285=CARTESIAN_POINT('Ctrl Pts',(17.8167014103155,3.33051870318735,817.477104707526));
#148286=CARTESIAN_POINT('Ctrl Pts',(17.9710104137728,1.66525935159367,815.982987060467));
#148287=CARTESIAN_POINT('Ctrl Pts',(18.1253194172301,3.32956716117513E-15,
814.488869413408));
#148288=CARTESIAN_POINT('Ctrl Pts',(17.9710104137728,-1.66525935159367,
812.994751766349));
#148289=CARTESIAN_POINT('Ctrl Pts',(17.8167014103155,-3.33051870318736,
811.50063411929));
#148290=CARTESIAN_POINT('Ctrl Pts',(17.3590292079831,-4.93906964482095,
810.006516472231));
#148291=CARTESIAN_POINT('Ctrl Pts',(16.9013570056506,-6.54762058645456,
808.512398825172));
#148292=CARTESIAN_POINT('Ctrl Pts',(16.1559070823762,-8.04468584505497,
807.018281178114));
#148293=CARTESIAN_POINT('Ctrl Pts',(15.4104571591017,-9.54175110365538,
805.524163531055));
#148294=CARTESIAN_POINT('Ctrl Pts',(14.4026149179538,-10.8763499173728,
804.030045883996));
#148295=CARTESIAN_POINT('Ctrl Pts',(13.3947726768058,-12.2109487310903,
802.535928236937));
#148296=CARTESIAN_POINT('Ctrl Pts',(12.1588589765331,-13.3376329379985,
801.041810589878));
#148297=CARTESIAN_POINT('Ctrl Pts',(10.9229452762603,-14.4643171449067,
799.54769294282));
#148298=CARTESIAN_POINT('Ctrl Pts',(9.50104767561053,-15.3447188656481,
798.053575295761));
#148299=CARTESIAN_POINT('Ctrl Pts',(8.07915007496071,-16.2251205863895,
796.559457648702));
#148300=CARTESIAN_POINT('Ctrl Pts',(6.51968959134574,-16.8292587962898,
795.065340001643));
#148301=CARTESIAN_POINT('Ctrl Pts',(4.96022910773078,-17.4333970061901,
793.571222354584));
#148302=CARTESIAN_POINT('Ctrl Pts',(3.31631129755346,-17.7406985030951,
792.077104707525));
#148303=CARTESIAN_POINT('Ctrl Pts',(1.67239348737615,-18.048,790.582987060467));
#148304=CARTESIAN_POINT('Ctrl Pts',(0.,-18.048,789.088869413408));
#148305=CARTESIAN_POINT('Ctrl Pts',(-1.67239348737615,-18.048,787.594751766349));
#148306=CARTESIAN_POINT('Ctrl Pts',(-3.31631129755346,-17.7406985030951,
786.10063411929));
#148307=CARTESIAN_POINT('Ctrl Pts',(-4.96022910773077,-17.4333970061901,
784.606516472231));
#148308=CARTESIAN_POINT('Ctrl Pts',(-6.51968959134574,-16.8292587962898,
783.112398825173));
#148309=CARTESIAN_POINT('Ctrl Pts',(-8.07915007496071,-16.2251205863895,
781.618281178114));
#148310=CARTESIAN_POINT('Ctrl Pts',(-9.50104767561052,-15.3447188656481,
780.124163531055));
#148311=CARTESIAN_POINT('Ctrl Pts',(-10.9229452762603,-14.4643171449067,
778.630045883996));
#148312=CARTESIAN_POINT('Ctrl Pts',(-12.1588589765331,-13.3376329379985,
777.135928236937));
#148313=CARTESIAN_POINT('Ctrl Pts',(-13.3947726768058,-12.2109487310903,
775.641810589879));
#148314=CARTESIAN_POINT('Ctrl Pts',(-14.4026149179538,-10.8763499173728,
774.14769294282));
#148315=CARTESIAN_POINT('Ctrl Pts',(-15.4104571591017,-9.54175110365538,
772.653575295761));
#148316=CARTESIAN_POINT('Ctrl Pts',(-16.1559070823762,-8.04468584505497,
771.159457648702));
#148317=CARTESIAN_POINT('Ctrl Pts',(-16.9013570056506,-6.54762058645456,
769.665340001643));
#148318=CARTESIAN_POINT('Ctrl Pts',(-17.3590292079831,-4.93906964482095,
768.171222354584));
#148319=CARTESIAN_POINT('Ctrl Pts',(-17.8167014103155,-3.33051870318735,
766.677104707526));
#148320=CARTESIAN_POINT('Ctrl Pts',(-17.9710104137728,-1.66525935159368,
765.182987060467));
#148321=CARTESIAN_POINT('Ctrl Pts',(-18.1253194172301,-1.10985572039171E-15,
763.688869413408));
#148322=CARTESIAN_POINT('Ctrl Pts',(-17.9710104137728,1.66525935159367,
762.194751766349));
#148323=CARTESIAN_POINT('Ctrl Pts',(-17.8167014103155,3.33051870318735,
760.70063411929));
#148324=CARTESIAN_POINT('Ctrl Pts',(-17.3590292079831,4.93906964482096,
759.206516472231));
#148325=CARTESIAN_POINT('Ctrl Pts',(-16.9013570056506,6.54762058645456,
757.712398825172));
#148326=CARTESIAN_POINT('Ctrl Pts',(-16.1559070823762,8.04468584505497,
756.218281178114));
#148327=CARTESIAN_POINT('Ctrl Pts',(-15.4104571591017,9.54175110365538,
754.724163531055));
#148328=CARTESIAN_POINT('Ctrl Pts',(-14.4026149179538,10.8763499173728,
753.230045883996));
#148329=CARTESIAN_POINT('Ctrl Pts',(-13.3947726768058,12.2109487310903,
751.735928236937));
#148330=CARTESIAN_POINT('Ctrl Pts',(-12.1588589765331,13.3376329379985,
750.241810589878));
#148331=CARTESIAN_POINT('Ctrl Pts',(-10.9229452762603,14.4643171449067,
748.74769294282));
#148332=CARTESIAN_POINT('Ctrl Pts',(-9.50104767561052,15.3447188656481,
747.253575295761));
#148333=CARTESIAN_POINT('Ctrl Pts',(-8.07915007496071,16.2251205863895,
745.759457648702));
#148334=CARTESIAN_POINT('Ctrl Pts',(-6.51968959134574,16.8292587962898,
744.265340001643));
#148335=CARTESIAN_POINT('Ctrl Pts',(-4.96022910773078,17.4333970061901,
742.771222354584));
#148336=CARTESIAN_POINT('Ctrl Pts',(-3.31631129755346,17.7406985030951,
741.277104707525));
#148337=CARTESIAN_POINT('Ctrl Pts',(-1.67239348737615,18.048,739.782987060467));
#148338=CARTESIAN_POINT('Ctrl Pts',(-2.21024254310115E-15,18.048,738.288869413408));
#148339=CARTESIAN_POINT('Ctrl Pts',(1.67239348737616,18.048,736.794751766349));
#148340=CARTESIAN_POINT('Ctrl Pts',(3.31631129755346,17.7406985030951,735.30063411929));
#148341=CARTESIAN_POINT('Ctrl Pts',(4.96022910773077,17.4333970061901,733.806516472231));
#148342=CARTESIAN_POINT('Ctrl Pts',(6.51968959134575,16.8292587962898,732.312398825173));
#148343=CARTESIAN_POINT('Ctrl Pts',(8.07915007496071,16.2251205863895,730.818281178114));
#148344=CARTESIAN_POINT('Ctrl Pts',(9.50104767561053,15.3447188656481,729.324163531055));
#148345=CARTESIAN_POINT('Ctrl Pts',(10.9229452762603,14.4643171449067,727.830045883996));
#148346=CARTESIAN_POINT('Ctrl Pts',(12.1588589765331,13.3376329379985,726.335928236937));
#148347=CARTESIAN_POINT('Ctrl Pts',(13.3947726768058,12.2109487310903,724.841810589879));
#148348=CARTESIAN_POINT('Ctrl Pts',(14.4026149179538,10.8763499173728,723.34769294282));
#148349=CARTESIAN_POINT('Ctrl Pts',(15.4104571591017,9.54175110365538,721.853575295761));
#148350=CARTESIAN_POINT('Ctrl Pts',(16.1559070823762,8.04468584505496,720.359457648702));
#148351=CARTESIAN_POINT('Ctrl Pts',(16.9013570056506,6.54762058645456,718.865340001643));
#148352=CARTESIAN_POINT('Ctrl Pts',(17.3590292079831,4.93906964482096,717.371222354584));
#148353=CARTESIAN_POINT('Ctrl Pts',(17.8167014103155,3.33051870318735,715.877104707526));
#148354=CARTESIAN_POINT('Ctrl Pts',(17.9710104137728,1.66525935159367,714.382987060467));
#148355=CARTESIAN_POINT('Ctrl Pts',(18.1253194172301,3.32956716117513E-15,
712.888869413408));
#148356=CARTESIAN_POINT('Ctrl Pts',(17.9710104137728,-1.66525935159367,
711.394751766349));
#148357=CARTESIAN_POINT('Ctrl Pts',(17.8167014103155,-3.33051870318736,
709.90063411929));
#148358=CARTESIAN_POINT('Ctrl Pts',(17.3590292079831,-4.93906964482095,
708.406516472231));
#148359=CARTESIAN_POINT('Ctrl Pts',(16.9013570056506,-6.54762058645456,
706.912398825173));
#148360=CARTESIAN_POINT('Ctrl Pts',(16.1559070823762,-8.04468584505497,
705.418281178114));
#148361=CARTESIAN_POINT('Ctrl Pts',(15.4104571591017,-9.54175110365538,
703.924163531055));
#148362=CARTESIAN_POINT('Ctrl Pts',(14.4026149179538,-10.8763499173728,
702.430045883996));
#148363=CARTESIAN_POINT('Ctrl Pts',(13.3947726768058,-12.2109487310903,
700.935928236937));
#148364=CARTESIAN_POINT('Ctrl Pts',(12.1588589765331,-13.3376329379985,
699.441810589878));
#148365=CARTESIAN_POINT('Ctrl Pts',(10.9229452762603,-14.4643171449067,
697.94769294282));
#148366=CARTESIAN_POINT('Ctrl Pts',(9.50104767561053,-15.3447188656481,
696.453575295761));
#148367=CARTESIAN_POINT('Ctrl Pts',(8.07915007496071,-16.2251205863895,
694.959457648702));
#148368=CARTESIAN_POINT('Ctrl Pts',(6.51968959134574,-16.8292587962898,
693.465340001643));
#148369=CARTESIAN_POINT('Ctrl Pts',(4.96022910773078,-17.4333970061901,
691.971222354584));
#148370=CARTESIAN_POINT('Ctrl Pts',(3.31631129755346,-17.7406985030951,
690.477104707526));
#148371=CARTESIAN_POINT('Ctrl Pts',(1.67239348737615,-18.048,688.982987060467));
#148372=CARTESIAN_POINT('Ctrl Pts',(0.,-18.048,687.488869413408));
#148373=CARTESIAN_POINT('Ctrl Pts',(-1.67239348737615,-18.048,685.994751766349));
#148374=CARTESIAN_POINT('Ctrl Pts',(-3.31631129755346,-17.7406985030951,
684.50063411929));
#148375=CARTESIAN_POINT('Ctrl Pts',(-4.96022910773077,-17.4333970061901,
683.006516472232));
#148376=CARTESIAN_POINT('Ctrl Pts',(-6.51968959134574,-16.8292587962898,
681.512398825172));
#148377=CARTESIAN_POINT('Ctrl Pts',(-8.07915007496071,-16.2251205863895,
680.018281178114));
#148378=CARTESIAN_POINT('Ctrl Pts',(-9.50104767561052,-15.3447188656481,
678.524163531055));
#148379=CARTESIAN_POINT('Ctrl Pts',(-10.9229452762603,-14.4643171449067,
677.030045883996));
#148380=CARTESIAN_POINT('Ctrl Pts',(-12.1588589765331,-13.3376329379985,
675.535928236937));
#148381=CARTESIAN_POINT('Ctrl Pts',(-13.3947726768058,-12.2109487310903,
674.041810589878));
#148382=CARTESIAN_POINT('Ctrl Pts',(-14.4026149179538,-10.8763499173728,
672.54769294282));
#148383=CARTESIAN_POINT('Ctrl Pts',(-15.4104571591017,-9.54175110365538,
671.053575295761));
#148384=CARTESIAN_POINT('Ctrl Pts',(-16.1559070823762,-8.04468584505497,
669.559457648702));
#148385=CARTESIAN_POINT('Ctrl Pts',(-16.9013570056506,-6.54762058645456,
668.065340001643));
#148386=CARTESIAN_POINT('Ctrl Pts',(-17.3590292079831,-4.93906964482095,
666.571222354584));
#148387=CARTESIAN_POINT('Ctrl Pts',(-17.8167014103155,-3.33051870318735,
665.077104707526));
#148388=CARTESIAN_POINT('Ctrl Pts',(-17.9710104137728,-1.66525935159368,
663.582987060467));
#148389=CARTESIAN_POINT('Ctrl Pts',(-18.1253194172301,-1.10985572039171E-15,
662.088869413408));
#148390=CARTESIAN_POINT('Ctrl Pts',(-17.9710104137728,1.66525935159367,
660.594751766349));
#148391=CARTESIAN_POINT('Ctrl Pts',(-17.8167014103155,3.33051870318735,
659.10063411929));
#148392=CARTESIAN_POINT('Ctrl Pts',(-17.3590292079831,4.93906964482096,
657.606516472231));
#148393=CARTESIAN_POINT('Ctrl Pts',(-16.9013570056506,6.54762058645456,
656.112398825172));
#148394=CARTESIAN_POINT('Ctrl Pts',(-16.1559070823762,8.04468584505497,
654.618281178114));
#148395=CARTESIAN_POINT('Ctrl Pts',(-15.4104571591017,9.54175110365538,
653.124163531055));
#148396=CARTESIAN_POINT('Ctrl Pts',(-14.4026149179538,10.8763499173728,
651.630045883996));
#148397=CARTESIAN_POINT('Ctrl Pts',(-13.3947726768058,12.2109487310903,
650.135928236937));
#148398=CARTESIAN_POINT('Ctrl Pts',(-12.1588589765331,13.3376329379985,
648.641810589878));
#148399=CARTESIAN_POINT('Ctrl Pts',(-10.9229452762603,14.4643171449067,
647.14769294282));
#148400=CARTESIAN_POINT('Ctrl Pts',(-9.50104767561052,15.3447188656481,
645.653575295761));
#148401=CARTESIAN_POINT('Ctrl Pts',(-8.07915007496071,16.2251205863895,
644.159457648702));
#148402=CARTESIAN_POINT('Ctrl Pts',(-6.51968959134574,16.8292587962898,
642.665340001643));
#148403=CARTESIAN_POINT('Ctrl Pts',(-4.96022910773078,17.4333970061901,
641.171222354584));
#148404=CARTESIAN_POINT('Ctrl Pts',(-3.31631129755346,17.7406985030951,
639.677104707525));
#148405=CARTESIAN_POINT('Ctrl Pts',(-1.67239348737615,18.048,638.182987060467));
#148406=CARTESIAN_POINT('Ctrl Pts',(-2.21024254310115E-15,18.048,636.688869413408));
#148407=CARTESIAN_POINT('Ctrl Pts',(1.67239348737616,18.048,635.194751766349));
#148408=CARTESIAN_POINT('Ctrl Pts',(3.31631129755346,17.7406985030951,633.70063411929));
#148409=CARTESIAN_POINT('Ctrl Pts',(4.96022910773077,17.4333970061901,632.206516472231));
#148410=CARTESIAN_POINT('Ctrl Pts',(6.51968959134575,16.8292587962898,630.712398825172));
#148411=CARTESIAN_POINT('Ctrl Pts',(8.07915007496071,16.2251205863895,629.218281178114));
#148412=CARTESIAN_POINT('Ctrl Pts',(9.50104767561053,15.3447188656481,627.724163531055));
#148413=CARTESIAN_POINT('Ctrl Pts',(10.9229452762603,14.4643171449067,626.230045883996));
#148414=CARTESIAN_POINT('Ctrl Pts',(12.1588589765331,13.3376329379985,624.735928236937));
#148415=CARTESIAN_POINT('Ctrl Pts',(13.3947726768058,12.2109487310903,623.241810589878));
#148416=CARTESIAN_POINT('Ctrl Pts',(14.4026149179538,10.8763499173728,621.74769294282));
#148417=CARTESIAN_POINT('Ctrl Pts',(15.4104571591017,9.54175110365538,620.253575295761));
#148418=CARTESIAN_POINT('Ctrl Pts',(16.1559070823762,8.04468584505496,618.759457648702));
#148419=CARTESIAN_POINT('Ctrl Pts',(16.9013570056506,6.54762058645456,617.265340001643));
#148420=CARTESIAN_POINT('Ctrl Pts',(17.3590292079831,4.93906964482096,615.771222354584));
#148421=CARTESIAN_POINT('Ctrl Pts',(17.8167014103155,3.33051870318735,614.277104707526));
#148422=CARTESIAN_POINT('Ctrl Pts',(17.9710104137728,1.66525935159367,612.782987060467));
#148423=CARTESIAN_POINT('Ctrl Pts',(18.1253194172301,3.32956716117513E-15,
611.288869413408));
#148424=CARTESIAN_POINT('Ctrl Pts',(17.9710104137728,-1.66525935159367,
609.794751766349));
#148425=CARTESIAN_POINT('Ctrl Pts',(17.8167014103155,-3.33051870318736,
608.30063411929));
#148426=CARTESIAN_POINT('Ctrl Pts',(17.3590292079831,-4.93906964482095,
606.806516472231));
#148427=CARTESIAN_POINT('Ctrl Pts',(16.9013570056506,-6.54762058645456,
605.312398825173));
#148428=CARTESIAN_POINT('Ctrl Pts',(16.1559070823762,-8.04468584505497,
603.818281178114));
#148429=CARTESIAN_POINT('Ctrl Pts',(15.4104571591017,-9.54175110365538,
602.324163531055));
#148430=CARTESIAN_POINT('Ctrl Pts',(14.4026149179538,-10.8763499173728,
600.830045883996));
#148431=CARTESIAN_POINT('Ctrl Pts',(13.3947726768058,-12.2109487310903,
599.335928236937));
#148432=CARTESIAN_POINT('Ctrl Pts',(12.1588589765331,-13.3376329379985,
597.841810589878));
#148433=CARTESIAN_POINT('Ctrl Pts',(10.9229452762603,-14.4643171449067,
596.34769294282));
#148434=CARTESIAN_POINT('Ctrl Pts',(9.50104767561053,-15.3447188656481,
594.853575295761));
#148435=CARTESIAN_POINT('Ctrl Pts',(8.07915007496071,-16.2251205863895,
593.359457648702));
#148436=CARTESIAN_POINT('Ctrl Pts',(6.51968959134574,-16.8292587962898,
591.865340001643));
#148437=CARTESIAN_POINT('Ctrl Pts',(4.96022910773078,-17.4333970061901,
590.371222354584));
#148438=CARTESIAN_POINT('Ctrl Pts',(3.31631129755346,-17.7406985030951,
588.877104707525));
#148439=CARTESIAN_POINT('Ctrl Pts',(1.67239348737615,-18.048,587.382987060467));
#148440=CARTESIAN_POINT('Ctrl Pts',(0.,-18.048,585.888869413408));
#148441=CARTESIAN_POINT('Ctrl Pts',(-1.67239348737615,-18.048,584.394751766349));
#148442=CARTESIAN_POINT('Ctrl Pts',(-3.31631129755346,-17.7406985030951,
582.90063411929));
#148443=CARTESIAN_POINT('Ctrl Pts',(-4.96022910773077,-17.4333970061901,
581.406516472231));
#148444=CARTESIAN_POINT('Ctrl Pts',(-6.51968959134574,-16.8292587962898,
579.912398825173));
#148445=CARTESIAN_POINT('Ctrl Pts',(-8.07915007496071,-16.2251205863895,
578.418281178114));
#148446=CARTESIAN_POINT('Ctrl Pts',(-9.50104767561052,-15.3447188656481,
576.924163531055));
#148447=CARTESIAN_POINT('Ctrl Pts',(-10.9229452762603,-14.4643171449067,
575.430045883996));
#148448=CARTESIAN_POINT('Ctrl Pts',(-12.1588589765331,-13.3376329379985,
573.935928236937));
#148449=CARTESIAN_POINT('Ctrl Pts',(-13.3947726768058,-12.2109487310903,
572.441810589879));
#148450=CARTESIAN_POINT('Ctrl Pts',(-14.4026149179538,-10.8763499173728,
570.94769294282));
#148451=CARTESIAN_POINT('Ctrl Pts',(-15.4104571591017,-9.54175110365538,
569.453575295761));
#148452=CARTESIAN_POINT('Ctrl Pts',(-16.1559070823762,-8.04468584505497,
567.959457648702));
#148453=CARTESIAN_POINT('Ctrl Pts',(-16.9013570056506,-6.54762058645456,
566.465340001643));
#148454=CARTESIAN_POINT('Ctrl Pts',(-17.3590292079831,-4.93906964482095,
564.971222354584));
#148455=CARTESIAN_POINT('Ctrl Pts',(-17.8167014103155,-3.33051870318735,
563.477104707526));
#148456=CARTESIAN_POINT('Ctrl Pts',(-17.9710104137728,-1.66525935159368,
561.982987060467));
#148457=CARTESIAN_POINT('Ctrl Pts',(-18.1253194172301,-1.10985572039171E-15,
560.488869413408));
#148458=CARTESIAN_POINT('Ctrl Pts',(-17.9710104137728,1.66525935159367,
558.994751766349));
#148459=CARTESIAN_POINT('Ctrl Pts',(-17.8167014103155,3.33051870318735,
557.50063411929));
#148460=CARTESIAN_POINT('Ctrl Pts',(-17.3590292079831,4.93906964482096,
556.006516472231));
#148461=CARTESIAN_POINT('Ctrl Pts',(-16.9013570056506,6.54762058645456,
554.512398825173));
#148462=CARTESIAN_POINT('Ctrl Pts',(-16.1559070823762,8.04468584505497,
553.018281178114));
#148463=CARTESIAN_POINT('Ctrl Pts',(-15.4104571591017,9.54175110365538,
551.524163531055));
#148464=CARTESIAN_POINT('Ctrl Pts',(-14.4026149179538,10.8763499173728,
550.030045883996));
#148465=CARTESIAN_POINT('Ctrl Pts',(-13.3947726768058,12.2109487310903,
548.535928236937));
#148466=CARTESIAN_POINT('Ctrl Pts',(-12.1588589765331,13.3376329379985,
547.041810589878));
#148467=CARTESIAN_POINT('Ctrl Pts',(-10.9229452762603,14.4643171449067,
545.54769294282));
#148468=CARTESIAN_POINT('Ctrl Pts',(-9.50104767561052,15.3447188656481,
544.053575295761));
#148469=CARTESIAN_POINT('Ctrl Pts',(-8.07915007496071,16.2251205863895,
542.559457648702));
#148470=CARTESIAN_POINT('Ctrl Pts',(-6.51968959134574,16.8292587962898,
541.065340001643));
#148471=CARTESIAN_POINT('Ctrl Pts',(-4.96022910773078,17.4333970061901,
539.571222354584));
#148472=CARTESIAN_POINT('Ctrl Pts',(-3.31631129755346,17.7406985030951,
538.077104707525));
#148473=CARTESIAN_POINT('Ctrl Pts',(-1.67239348737615,18.048,536.582987060467));
#148474=CARTESIAN_POINT('Ctrl Pts',(-2.21024254310115E-15,18.048,535.088869413408));
#148475=CARTESIAN_POINT('Ctrl Pts',(1.67239348737616,18.048,533.594751766349));
#148476=CARTESIAN_POINT('Ctrl Pts',(3.31631129755346,17.7406985030951,532.10063411929));
#148477=CARTESIAN_POINT('Ctrl Pts',(4.96022910773077,17.4333970061901,530.606516472231));
#148478=CARTESIAN_POINT('Ctrl Pts',(6.51968959134575,16.8292587962898,529.112398825172));
#148479=CARTESIAN_POINT('Ctrl Pts',(8.07915007496071,16.2251205863895,527.618281178114));
#148480=CARTESIAN_POINT('Ctrl Pts',(9.50104767561053,15.3447188656481,526.124163531055));
#148481=CARTESIAN_POINT('Ctrl Pts',(10.9229452762603,14.4643171449067,524.630045883996));
#148482=CARTESIAN_POINT('Ctrl Pts',(12.1588589765331,13.3376329379985,523.135928236937));
#148483=CARTESIAN_POINT('Ctrl Pts',(13.3947726768058,12.2109487310903,521.641810589878));
#148484=CARTESIAN_POINT('Ctrl Pts',(14.4026149179538,10.8763499173728,520.14769294282));
#148485=CARTESIAN_POINT('Ctrl Pts',(15.4104571591017,9.54175110365538,518.653575295761));
#148486=CARTESIAN_POINT('Ctrl Pts',(16.1559070823762,8.04468584505496,517.159457648702));
#148487=CARTESIAN_POINT('Ctrl Pts',(16.9013570056506,6.54762058645456,515.665340001643));
#148488=CARTESIAN_POINT('Ctrl Pts',(17.3590292079831,4.93906964482096,514.171222354584));
#148489=CARTESIAN_POINT('Ctrl Pts',(17.8167014103155,3.33051870318735,512.677104707525));
#148490=CARTESIAN_POINT('Ctrl Pts',(17.9710104137728,1.66525935159367,511.182987060467));
#148491=CARTESIAN_POINT('Ctrl Pts',(18.1253194172301,3.32956716117513E-15,
509.688869413408));
#148492=CARTESIAN_POINT('Ctrl Pts',(17.9710104137728,-1.66525935159367,
508.194751766349));
#148493=CARTESIAN_POINT('Ctrl Pts',(17.8167014103155,-3.33051870318736,
506.70063411929));
#148494=CARTESIAN_POINT('Ctrl Pts',(17.3590292079831,-4.93906964482095,
505.206516472231));
#148495=CARTESIAN_POINT('Ctrl Pts',(16.9013570056506,-6.54762058645456,
503.712398825173));
#148496=CARTESIAN_POINT('Ctrl Pts',(16.1559070823762,-8.04468584505497,
502.218281178114));
#148497=CARTESIAN_POINT('Ctrl Pts',(15.4104571591017,-9.54175110365538,
500.724163531055));
#148498=CARTESIAN_POINT('Ctrl Pts',(14.4026149179538,-10.8763499173728,
499.230045883996));
#148499=CARTESIAN_POINT('Ctrl Pts',(13.3947726768058,-12.2109487310903,
497.735928236937));
#148500=CARTESIAN_POINT('Ctrl Pts',(12.1588589765331,-13.3376329379985,
496.241810589879));
#148501=CARTESIAN_POINT('Ctrl Pts',(10.9229452762603,-14.4643171449067,
494.74769294282));
#148502=CARTESIAN_POINT('Ctrl Pts',(9.50104767561053,-15.3447188656481,
493.253575295761));
#148503=CARTESIAN_POINT('Ctrl Pts',(8.07915007496071,-16.2251205863895,
491.759457648702));
#148504=CARTESIAN_POINT('Ctrl Pts',(6.51968959134574,-16.8292587962898,
490.265340001643));
#148505=CARTESIAN_POINT('Ctrl Pts',(4.96022910773078,-17.4333970061901,
488.771222354584));
#148506=CARTESIAN_POINT('Ctrl Pts',(3.31631129755346,-17.7406985030951,
487.277104707526));
#148507=CARTESIAN_POINT('Ctrl Pts',(1.67239348737615,-18.048,485.782987060467));
#148508=CARTESIAN_POINT('Ctrl Pts',(0.,-18.048,484.288869413408));
#148509=CARTESIAN_POINT('Ctrl Pts',(-1.67239348737615,-18.048,482.794751766349));
#148510=CARTESIAN_POINT('Ctrl Pts',(-3.31631129755346,-17.7406985030951,
481.30063411929));
#148511=CARTESIAN_POINT('Ctrl Pts',(-4.96022910773077,-17.4333970061901,
479.806516472231));
#148512=CARTESIAN_POINT('Ctrl Pts',(-6.51968959134574,-16.8292587962898,
478.312398825173));
#148513=CARTESIAN_POINT('Ctrl Pts',(-8.07915007496071,-16.2251205863895,
476.818281178114));
#148514=CARTESIAN_POINT('Ctrl Pts',(-9.50104767561052,-15.3447188656481,
475.324163531055));
#148515=CARTESIAN_POINT('Ctrl Pts',(-10.9229452762603,-14.4643171449067,
473.830045883996));
#148516=CARTESIAN_POINT('Ctrl Pts',(-12.1588589765331,-13.3376329379985,
472.335928236937));
#148517=CARTESIAN_POINT('Ctrl Pts',(-13.3947726768058,-12.2109487310903,
470.841810589878));
#148518=CARTESIAN_POINT('Ctrl Pts',(-14.4026149179538,-10.8763499173728,
469.34769294282));
#148519=CARTESIAN_POINT('Ctrl Pts',(-15.4104571591017,-9.54175110365538,
467.853575295761));
#148520=CARTESIAN_POINT('Ctrl Pts',(-16.1559070823762,-8.04468584505497,
466.359457648702));
#148521=CARTESIAN_POINT('Ctrl Pts',(-16.9013570056506,-6.54762058645456,
464.865340001643));
#148522=CARTESIAN_POINT('Ctrl Pts',(-17.3590292079831,-4.93906964482095,
463.371222354584));
#148523=CARTESIAN_POINT('Ctrl Pts',(-17.8167014103155,-3.33051870318735,
461.877104707525));
#148524=CARTESIAN_POINT('Ctrl Pts',(-17.9710104137728,-1.66525935159368,
460.382987060467));
#148525=CARTESIAN_POINT('Ctrl Pts',(-18.1253194172301,-1.10985572039171E-15,
458.888869413408));
#148526=CARTESIAN_POINT('Ctrl Pts',(-17.9710104137728,1.66525935159367,
457.394751766349));
#148527=CARTESIAN_POINT('Ctrl Pts',(-17.8167014103155,3.33051870318735,
455.90063411929));
#148528=CARTESIAN_POINT('Ctrl Pts',(-17.3590292079831,4.93906964482096,
454.406516472231));
#148529=CARTESIAN_POINT('Ctrl Pts',(-16.9013570056506,6.54762058645456,
452.912398825173));
#148530=CARTESIAN_POINT('Ctrl Pts',(-16.1559070823762,8.04468584505497,
451.418281178114));
#148531=CARTESIAN_POINT('Ctrl Pts',(-15.4104571591017,9.54175110365538,
449.924163531055));
#148532=CARTESIAN_POINT('Ctrl Pts',(-14.4026149179538,10.8763499173728,
448.430045883996));
#148533=CARTESIAN_POINT('Ctrl Pts',(-13.3947726768058,12.2109487310903,
446.935928236937));
#148534=CARTESIAN_POINT('Ctrl Pts',(-12.1588589765331,13.3376329379985,
445.441810589878));
#148535=CARTESIAN_POINT('Ctrl Pts',(-10.9229452762603,14.4643171449067,
443.94769294282));
#148536=CARTESIAN_POINT('Ctrl Pts',(-9.50104767561052,15.3447188656481,
442.453575295761));
#148537=CARTESIAN_POINT('Ctrl Pts',(-8.07915007496071,16.2251205863895,
440.959457648702));
#148538=CARTESIAN_POINT('Ctrl Pts',(-6.51968959134574,16.8292587962898,
439.465340001643));
#148539=CARTESIAN_POINT('Ctrl Pts',(-4.96022910773078,17.4333970061901,
437.971222354584));
#148540=CARTESIAN_POINT('Ctrl Pts',(-3.31631129755346,17.7406985030951,
436.477104707526));
#148541=CARTESIAN_POINT('Ctrl Pts',(-1.67239348737615,18.048,434.982987060467));
#148542=CARTESIAN_POINT('Ctrl Pts',(-2.21024254310115E-15,18.048,433.488869413408));
#148543=CARTESIAN_POINT('Ctrl Pts',(1.67239348737616,18.048,431.994751766349));
#148544=CARTESIAN_POINT('Ctrl Pts',(3.31631129755346,17.7406985030951,430.50063411929));
#148545=CARTESIAN_POINT('Ctrl Pts',(4.96022910773077,17.4333970061901,429.006516472231));
#148546=CARTESIAN_POINT('Ctrl Pts',(6.51968959134575,16.8292587962898,427.512398825173));
#148547=CARTESIAN_POINT('Ctrl Pts',(8.07915007496071,16.2251205863895,426.018281178114));
#148548=CARTESIAN_POINT('Ctrl Pts',(9.50104767561053,15.3447188656481,424.524163531055));
#148549=CARTESIAN_POINT('Ctrl Pts',(10.9229452762603,14.4643171449067,423.030045883996));
#148550=CARTESIAN_POINT('Ctrl Pts',(12.1588589765331,13.3376329379985,421.535928236937));
#148551=CARTESIAN_POINT('Ctrl Pts',(13.3947726768058,12.2109487310903,420.041810589879));
#148552=CARTESIAN_POINT('Ctrl Pts',(14.4026149179538,10.8763499173728,418.54769294282));
#148553=CARTESIAN_POINT('Ctrl Pts',(15.4104571591017,9.54175110365538,417.053575295761));
#148554=CARTESIAN_POINT('Ctrl Pts',(16.1559070823762,8.04468584505496,415.559457648702));
#148555=CARTESIAN_POINT('Ctrl Pts',(16.9013570056506,6.54762058645456,414.065340001643));
#148556=CARTESIAN_POINT('Ctrl Pts',(17.3590292079831,4.93906964482096,412.571222354584));
#148557=CARTESIAN_POINT('Ctrl Pts',(17.8167014103155,3.33051870318735,411.077104707526));
#148558=CARTESIAN_POINT('Ctrl Pts',(17.9710104137728,1.66525935159367,409.582987060467));
#148559=CARTESIAN_POINT('Ctrl Pts',(18.1253194172301,3.32956716117513E-15,
408.088869413408));
#148560=CARTESIAN_POINT('Ctrl Pts',(17.9710104137728,-1.66525935159367,
406.594751766349));
#148561=CARTESIAN_POINT('Ctrl Pts',(17.8167014103155,-3.33051870318736,
405.10063411929));
#148562=CARTESIAN_POINT('Ctrl Pts',(17.3590292079831,-4.93906964482095,
403.606516472231));
#148563=CARTESIAN_POINT('Ctrl Pts',(16.9013570056506,-6.54762058645456,
402.112398825173));
#148564=CARTESIAN_POINT('Ctrl Pts',(16.1559070823762,-8.04468584505497,
400.618281178114));
#148565=CARTESIAN_POINT('Ctrl Pts',(15.4104571591017,-9.54175110365538,
399.124163531055));
#148566=CARTESIAN_POINT('Ctrl Pts',(14.4026149179538,-10.8763499173728,
397.630045883996));
#148567=CARTESIAN_POINT('Ctrl Pts',(13.3947726768058,-12.2109487310903,
396.135928236937));
#148568=CARTESIAN_POINT('Ctrl Pts',(12.1588589765331,-13.3376329379985,
394.641810589878));
#148569=CARTESIAN_POINT('Ctrl Pts',(10.9229452762603,-14.4643171449067,
393.147692942819));
#148570=CARTESIAN_POINT('Ctrl Pts',(9.50104767561053,-15.3447188656481,
391.653575295761));
#148571=CARTESIAN_POINT('Ctrl Pts',(8.07915007496071,-16.2251205863895,
390.159457648702));
#148572=CARTESIAN_POINT('Ctrl Pts',(6.51968959134574,-16.8292587962898,
388.665340001643));
#148573=CARTESIAN_POINT('Ctrl Pts',(4.96022910773078,-17.4333970061901,
387.171222354584));
#148574=CARTESIAN_POINT('Ctrl Pts',(3.31631129755346,-17.7406985030951,
385.677104707525));
#148575=CARTESIAN_POINT('Ctrl Pts',(1.67239348737615,-18.048,384.182987060467));
#148576=CARTESIAN_POINT('Ctrl Pts',(0.,-18.048,382.688869413408));
#148577=CARTESIAN_POINT('Ctrl Pts',(-1.67239348737615,-18.048,381.194751766349));
#148578=CARTESIAN_POINT('Ctrl Pts',(-3.31631129755346,-17.7406985030951,
379.70063411929));
#148579=CARTESIAN_POINT('Ctrl Pts',(-4.96022910773077,-17.4333970061901,
378.206516472231));
#148580=CARTESIAN_POINT('Ctrl Pts',(-6.51968959134574,-16.8292587962898,
376.712398825173));
#148581=CARTESIAN_POINT('Ctrl Pts',(-8.07915007496071,-16.2251205863895,
375.218281178114));
#148582=CARTESIAN_POINT('Ctrl Pts',(-9.50104767561052,-15.3447188656481,
373.724163531055));
#148583=CARTESIAN_POINT('Ctrl Pts',(-10.9229452762603,-14.4643171449067,
372.230045883996));
#148584=CARTESIAN_POINT('Ctrl Pts',(-12.1588589765331,-13.3376329379985,
370.735928236937));
#148585=CARTESIAN_POINT('Ctrl Pts',(-13.3947726768058,-12.2109487310903,
369.241810589879));
#148586=CARTESIAN_POINT('Ctrl Pts',(-14.4026149179538,-10.8763499173728,
367.74769294282));
#148587=CARTESIAN_POINT('Ctrl Pts',(-15.4104571591017,-9.54175110365538,
366.253575295761));
#148588=CARTESIAN_POINT('Ctrl Pts',(-16.1559070823762,-8.04468584505497,
364.759457648702));
#148589=CARTESIAN_POINT('Ctrl Pts',(-16.9013570056506,-6.54762058645456,
363.265340001643));
#148590=CARTESIAN_POINT('Ctrl Pts',(-17.3590292079831,-4.93906964482095,
361.771222354584));
#148591=CARTESIAN_POINT('Ctrl Pts',(-17.8167014103155,-3.33051870318735,
360.277104707525));
#148592=CARTESIAN_POINT('Ctrl Pts',(-17.9710104137728,-1.66525935159368,
358.782987060467));
#148593=CARTESIAN_POINT('Ctrl Pts',(-18.1253194172301,-1.10985572039171E-15,
357.288869413408));
#148594=CARTESIAN_POINT('Ctrl Pts',(-17.9710104137728,1.66525935159367,
355.794751766349));
#148595=CARTESIAN_POINT('Ctrl Pts',(-17.8167014103155,3.33051870318735,
354.30063411929));
#148596=CARTESIAN_POINT('Ctrl Pts',(-17.3590292079831,4.93906964482096,
352.806516472231));
#148597=CARTESIAN_POINT('Ctrl Pts',(-16.9013570056506,6.54762058645456,
351.312398825173));
#148598=CARTESIAN_POINT('Ctrl Pts',(-16.1559070823762,8.04468584505497,
349.818281178114));
#148599=CARTESIAN_POINT('Ctrl Pts',(-15.4104571591017,9.54175110365538,
348.324163531055));
#148600=CARTESIAN_POINT('Ctrl Pts',(-14.4026149179538,10.8763499173728,
346.830045883996));
#148601=CARTESIAN_POINT('Ctrl Pts',(-13.3947726768058,12.2109487310903,
345.335928236937));
#148602=CARTESIAN_POINT('Ctrl Pts',(-12.1588589765331,13.3376329379985,
343.841810589878));
#148603=CARTESIAN_POINT('Ctrl Pts',(-10.9229452762603,14.4643171449067,
342.34769294282));
#148604=CARTESIAN_POINT('Ctrl Pts',(-9.50104767561052,15.3447188656481,
340.853575295761));
#148605=CARTESIAN_POINT('Ctrl Pts',(-8.07915007496071,16.2251205863895,
339.359457648702));
#148606=CARTESIAN_POINT('Ctrl Pts',(-6.51968959134574,16.8292587962898,
337.865340001643));
#148607=CARTESIAN_POINT('Ctrl Pts',(-4.96022910773078,17.4333970061901,
336.371222354584));
#148608=CARTESIAN_POINT('Ctrl Pts',(-3.31631129755346,17.7406985030951,
334.877104707525));
#148609=CARTESIAN_POINT('Ctrl Pts',(-1.67239348737615,18.048,333.382987060467));
#148610=CARTESIAN_POINT('Ctrl Pts',(-2.21024254310115E-15,18.048,331.888869413408));
#148611=CARTESIAN_POINT('Ctrl Pts',(1.67239348737616,18.048,330.394751766349));
#148612=CARTESIAN_POINT('Ctrl Pts',(3.31631129755346,17.7406985030951,328.90063411929));
#148613=CARTESIAN_POINT('Ctrl Pts',(4.96022910773077,17.4333970061901,327.406516472231));
#148614=CARTESIAN_POINT('Ctrl Pts',(6.51968959134575,16.8292587962898,325.912398825172));
#148615=CARTESIAN_POINT('Ctrl Pts',(8.07915007496071,16.2251205863895,324.418281178114));
#148616=CARTESIAN_POINT('Ctrl Pts',(9.50104767561053,15.3447188656481,322.924163531055));
#148617=CARTESIAN_POINT('Ctrl Pts',(10.9229452762603,14.4643171449067,321.430045883996));
#148618=CARTESIAN_POINT('Ctrl Pts',(12.1588589765331,13.3376329379985,319.935928236937));
#148619=CARTESIAN_POINT('Ctrl Pts',(13.3947726768058,12.2109487310903,318.441810589878));
#148620=CARTESIAN_POINT('Ctrl Pts',(14.4026149179538,10.8763499173728,316.94769294282));
#148621=CARTESIAN_POINT('Ctrl Pts',(15.4104571591017,9.54175110365538,315.453575295761));
#148622=CARTESIAN_POINT('Ctrl Pts',(16.1559070823762,8.04468584505496,313.959457648702));
#148623=CARTESIAN_POINT('Ctrl Pts',(16.9013570056506,6.54762058645456,312.465340001643));
#148624=CARTESIAN_POINT('Ctrl Pts',(17.3590292079831,4.93906964482096,310.971222354584));
#148625=CARTESIAN_POINT('Ctrl Pts',(17.8167014103155,3.33051870318735,309.477104707526));
#148626=CARTESIAN_POINT('Ctrl Pts',(17.9710104137728,1.66525935159367,307.982987060467));
#148627=CARTESIAN_POINT('Ctrl Pts',(18.1253194172301,3.32956716117513E-15,
306.488869413408));
#148628=CARTESIAN_POINT('Ctrl Pts',(17.9710104137728,-1.66525935159367,
304.994751766349));
#148629=CARTESIAN_POINT('Ctrl Pts',(17.8167014103155,-3.33051870318736,
303.50063411929));
#148630=CARTESIAN_POINT('Ctrl Pts',(17.3590292079831,-4.93906964482095,
302.006516472231));
#148631=CARTESIAN_POINT('Ctrl Pts',(16.9013570056506,-6.54762058645456,
300.512398825173));
#148632=CARTESIAN_POINT('Ctrl Pts',(16.1559070823762,-8.04468584505497,
299.018281178114));
#148633=CARTESIAN_POINT('Ctrl Pts',(15.4104571591017,-9.54175110365538,
297.524163531055));
#148634=CARTESIAN_POINT('Ctrl Pts',(14.4026149179538,-10.8763499173728,
296.030045883996));
#148635=CARTESIAN_POINT('Ctrl Pts',(13.3947726768058,-12.2109487310903,
294.535928236937));
#148636=CARTESIAN_POINT('Ctrl Pts',(12.1588589765331,-13.3376329379985,
293.041810589878));
#148637=CARTESIAN_POINT('Ctrl Pts',(10.9229452762603,-14.4643171449067,
291.54769294282));
#148638=CARTESIAN_POINT('Ctrl Pts',(9.50104767561053,-15.3447188656481,
290.053575295761));
#148639=CARTESIAN_POINT('Ctrl Pts',(8.07915007496071,-16.2251205863895,
288.559457648702));
#148640=CARTESIAN_POINT('Ctrl Pts',(6.51968959134574,-16.8292587962898,
287.065340001643));
#148641=CARTESIAN_POINT('Ctrl Pts',(4.96022910773078,-17.4333970061901,
285.571222354584));
#148642=CARTESIAN_POINT('Ctrl Pts',(3.31631129755346,-17.7406985030951,
284.077104707525));
#148643=CARTESIAN_POINT('Ctrl Pts',(1.67239348737615,-18.048,282.582987060467));
#148644=CARTESIAN_POINT('Ctrl Pts',(0.,-18.048,281.088869413408));
#148645=CARTESIAN_POINT('Ctrl Pts',(-1.67239348737615,-18.048,279.594751766349));
#148646=CARTESIAN_POINT('Ctrl Pts',(-3.31631129755346,-17.7406985030951,
278.10063411929));
#148647=CARTESIAN_POINT('Ctrl Pts',(-4.96022910773077,-17.4333970061901,
276.606516472231));
#148648=CARTESIAN_POINT('Ctrl Pts',(-6.51968959134574,-16.8292587962898,
275.112398825172));
#148649=CARTESIAN_POINT('Ctrl Pts',(-8.07915007496071,-16.2251205863895,
273.618281178114));
#148650=CARTESIAN_POINT('Ctrl Pts',(-9.50104767561052,-15.3447188656481,
272.124163531055));
#148651=CARTESIAN_POINT('Ctrl Pts',(-10.9229452762603,-14.4643171449067,
270.630045883996));
#148652=CARTESIAN_POINT('Ctrl Pts',(-12.1588589765331,-13.3376329379985,
269.135928236937));
#148653=CARTESIAN_POINT('Ctrl Pts',(-13.3947726768058,-12.2109487310903,
267.641810589878));
#148654=CARTESIAN_POINT('Ctrl Pts',(-14.4026149179538,-10.8763499173728,
266.14769294282));
#148655=CARTESIAN_POINT('Ctrl Pts',(-15.4104571591017,-9.54175110365538,
264.653575295761));
#148656=CARTESIAN_POINT('Ctrl Pts',(-16.1559070823762,-8.04468584505497,
263.159457648702));
#148657=CARTESIAN_POINT('Ctrl Pts',(-16.9013570056506,-6.54762058645456,
261.665340001643));
#148658=CARTESIAN_POINT('Ctrl Pts',(-17.3590292079831,-4.93906964482095,
260.171222354584));
#148659=CARTESIAN_POINT('Ctrl Pts',(-17.8167014103155,-3.33051870318735,
258.677104707525));
#148660=CARTESIAN_POINT('Ctrl Pts',(-17.9710104137728,-1.66525935159368,
257.182987060467));
#148661=CARTESIAN_POINT('Ctrl Pts',(-18.1253194172301,-1.10985572039171E-15,
255.688869413408));
#148662=CARTESIAN_POINT('Ctrl Pts',(-17.9710104137728,1.66525935159367,
254.194751766349));
#148663=CARTESIAN_POINT('Ctrl Pts',(-17.8167014103155,3.33051870318735,
252.70063411929));
#148664=CARTESIAN_POINT('Ctrl Pts',(-17.3590292079831,4.93906964482096,
251.206516472231));
#148665=CARTESIAN_POINT('Ctrl Pts',(-16.9013570056506,6.54762058645456,
249.712398825173));
#148666=CARTESIAN_POINT('Ctrl Pts',(-16.1559070823762,8.04468584505497,
248.218281178114));
#148667=CARTESIAN_POINT('Ctrl Pts',(-15.4104571591017,9.54175110365538,
246.724163531055));
#148668=CARTESIAN_POINT('Ctrl Pts',(-14.4026149179538,10.8763499173728,
245.230045883996));
#148669=CARTESIAN_POINT('Ctrl Pts',(-13.3947726768058,12.2109487310903,
243.735928236937));
#148670=CARTESIAN_POINT('Ctrl Pts',(-12.1588589765331,13.3376329379985,
242.241810589878));
#148671=CARTESIAN_POINT('Ctrl Pts',(-10.9229452762603,14.4643171449067,
240.74769294282));
#148672=CARTESIAN_POINT('Ctrl Pts',(-9.50104767561052,15.3447188656481,
239.253575295761));
#148673=CARTESIAN_POINT('Ctrl Pts',(-8.07915007496071,16.2251205863895,
237.759457648702));
#148674=CARTESIAN_POINT('Ctrl Pts',(-6.51968959134574,16.8292587962898,
236.265340001643));
#148675=CARTESIAN_POINT('Ctrl Pts',(-4.96022910773078,17.4333970061901,
234.771222354584));
#148676=CARTESIAN_POINT('Ctrl Pts',(-3.31631129755346,17.7406985030951,
233.277104707525));
#148677=CARTESIAN_POINT('Ctrl Pts',(-1.67239348737615,18.048,231.782987060467));
#148678=CARTESIAN_POINT('Ctrl Pts',(-2.21024254310115E-15,18.048,230.288869413408));
#148679=CARTESIAN_POINT('Ctrl Pts',(1.67239348737616,18.048,228.794751766349));
#148680=CARTESIAN_POINT('Ctrl Pts',(3.31631129755346,17.7406985030951,227.30063411929));
#148681=CARTESIAN_POINT('Ctrl Pts',(4.96022910773077,17.4333970061901,225.806516472231));
#148682=CARTESIAN_POINT('Ctrl Pts',(6.51968959134575,16.8292587962898,224.312398825173));
#148683=CARTESIAN_POINT('Ctrl Pts',(8.07915007496071,16.2251205863895,222.818281178114));
#148684=CARTESIAN_POINT('Ctrl Pts',(9.50104767561053,15.3447188656481,221.324163531055));
#148685=CARTESIAN_POINT('Ctrl Pts',(10.9229452762603,14.4643171449067,219.830045883996));
#148686=CARTESIAN_POINT('Ctrl Pts',(12.1588589765331,13.3376329379985,218.335928236937));
#148687=CARTESIAN_POINT('Ctrl Pts',(13.3947726768058,12.2109487310903,216.841810589878));
#148688=CARTESIAN_POINT('Ctrl Pts',(14.4026149179538,10.8763499173728,215.34769294282));
#148689=CARTESIAN_POINT('Ctrl Pts',(15.4104571591017,9.54175110365538,213.853575295761));
#148690=CARTESIAN_POINT('Ctrl Pts',(16.1559070823762,8.04468584505496,212.359457648702));
#148691=CARTESIAN_POINT('Ctrl Pts',(16.9013570056506,6.54762058645456,210.865340001643));
#148692=CARTESIAN_POINT('Ctrl Pts',(17.3590292079831,4.93906964482096,209.371222354584));
#148693=CARTESIAN_POINT('Ctrl Pts',(17.8167014103155,3.33051870318735,207.877104707525));
#148694=CARTESIAN_POINT('Ctrl Pts',(17.9710104137728,1.66525935159367,206.382987060467));
#148695=CARTESIAN_POINT('Ctrl Pts',(18.1253194172301,3.32956716117513E-15,
204.888869413408));
#148696=CARTESIAN_POINT('Ctrl Pts',(17.9710104137728,-1.66525935159367,
203.394751766349));
#148697=CARTESIAN_POINT('Ctrl Pts',(17.8167014103155,-3.33051870318736,
201.90063411929));
#148698=CARTESIAN_POINT('Ctrl Pts',(17.3590292079831,-4.93906964482095,
200.406516472231));
#148699=CARTESIAN_POINT('Ctrl Pts',(16.9013570056506,-6.54762058645456,
198.912398825172));
#148700=CARTESIAN_POINT('Ctrl Pts',(16.1559070823762,-8.04468584505497,
197.418281178114));
#148701=CARTESIAN_POINT('Ctrl Pts',(15.4104571591017,-9.54175110365538,
195.924163531055));
#148702=CARTESIAN_POINT('Ctrl Pts',(14.4026149179538,-10.8763499173728,
194.430045883996));
#148703=CARTESIAN_POINT('Ctrl Pts',(13.3947726768058,-12.2109487310903,
192.935928236937));
#148704=CARTESIAN_POINT('Ctrl Pts',(12.1588589765331,-13.3376329379985,
191.441810589878));
#148705=CARTESIAN_POINT('Ctrl Pts',(10.9229452762603,-14.4643171449067,
189.94769294282));
#148706=CARTESIAN_POINT('Ctrl Pts',(9.50104767561053,-15.3447188656481,
188.453575295761));
#148707=CARTESIAN_POINT('Ctrl Pts',(8.07915007496071,-16.2251205863895,
186.959457648702));
#148708=CARTESIAN_POINT('Ctrl Pts',(6.51968959134574,-16.8292587962898,
185.465340001643));
#148709=CARTESIAN_POINT('Ctrl Pts',(4.96022910773078,-17.4333970061901,
183.971222354584));
#148710=CARTESIAN_POINT('Ctrl Pts',(3.31631129755346,-17.7406985030951,
182.477104707526));
#148711=CARTESIAN_POINT('Ctrl Pts',(1.67239348737615,-18.048,180.982987060467));
#148712=CARTESIAN_POINT('Ctrl Pts',(0.,-18.048,179.488869413408));
#148713=CARTESIAN_POINT('Ctrl Pts',(-1.67239348737615,-18.048,177.994751766349));
#148714=CARTESIAN_POINT('Ctrl Pts',(-3.31631129755346,-17.7406985030951,
176.50063411929));
#148715=CARTESIAN_POINT('Ctrl Pts',(-4.96022910773077,-17.4333970061901,
175.006516472231));
#148716=CARTESIAN_POINT('Ctrl Pts',(-6.51968959134574,-16.8292587962898,
173.512398825173));
#148717=CARTESIAN_POINT('Ctrl Pts',(-8.07915007496071,-16.2251205863895,
172.018281178114));
#148718=CARTESIAN_POINT('Ctrl Pts',(-9.50104767561052,-15.3447188656481,
170.524163531055));
#148719=CARTESIAN_POINT('Ctrl Pts',(-10.9229452762603,-14.4643171449067,
169.030045883996));
#148720=CARTESIAN_POINT('Ctrl Pts',(-12.1588589765331,-13.3376329379985,
167.535928236937));
#148721=CARTESIAN_POINT('Ctrl Pts',(-13.3947726768058,-12.2109487310903,
166.041810589878));
#148722=CARTESIAN_POINT('Ctrl Pts',(-14.4026149179538,-10.8763499173728,
164.54769294282));
#148723=CARTESIAN_POINT('Ctrl Pts',(-15.4104571591017,-9.54175110365538,
163.053575295761));
#148724=CARTESIAN_POINT('Ctrl Pts',(-16.1559070823762,-8.04468584505497,
161.559457648702));
#148725=CARTESIAN_POINT('Ctrl Pts',(-16.9013570056506,-6.54762058645456,
160.065340001643));
#148726=CARTESIAN_POINT('Ctrl Pts',(-17.3590292079831,-4.93906964482095,
158.571222354584));
#148727=CARTESIAN_POINT('Ctrl Pts',(-17.8167014103155,-3.33051870318735,
157.077104707525));
#148728=CARTESIAN_POINT('Ctrl Pts',(-17.9710104137728,-1.66525935159368,
155.582987060467));
#148729=CARTESIAN_POINT('Ctrl Pts',(-18.1253194172301,-1.10985572039171E-15,
154.088869413408));
#148730=CARTESIAN_POINT('Ctrl Pts',(-17.9710104137728,1.66525935159367,
152.594751766349));
#148731=CARTESIAN_POINT('Ctrl Pts',(-17.8167014103155,3.33051870318735,
151.10063411929));
#148732=CARTESIAN_POINT('Ctrl Pts',(-17.3590292079831,4.93906964482096,
149.606516472231));
#148733=CARTESIAN_POINT('Ctrl Pts',(-16.9013570056506,6.54762058645456,
148.112398825172));
#148734=CARTESIAN_POINT('Ctrl Pts',(-16.1559070823762,8.04468584505497,
146.618281178114));
#148735=CARTESIAN_POINT('Ctrl Pts',(-15.4104571591017,9.54175110365538,
145.124163531055));
#148736=CARTESIAN_POINT('Ctrl Pts',(-14.4026149179538,10.8763499173728,
143.630045883996));
#148737=CARTESIAN_POINT('Ctrl Pts',(-13.3947726768058,12.2109487310903,
142.135928236937));
#148738=CARTESIAN_POINT('Ctrl Pts',(-12.1588589765331,13.3376329379985,
140.641810589878));
#148739=CARTESIAN_POINT('Ctrl Pts',(-10.9229452762603,14.4643171449067,
139.147692942819));
#148740=CARTESIAN_POINT('Ctrl Pts',(-9.50104767561052,15.3447188656481,
137.653575295761));
#148741=CARTESIAN_POINT('Ctrl Pts',(-8.07915007496071,16.2251205863895,
136.159457648702));
#148742=CARTESIAN_POINT('Ctrl Pts',(-6.51968959134574,16.8292587962898,
134.665340001643));
#148743=CARTESIAN_POINT('Ctrl Pts',(-4.96022910773078,17.4333970061901,
133.171222354584));
#148744=CARTESIAN_POINT('Ctrl Pts',(-3.31631129755346,17.7406985030951,
131.677104707525));
#148745=CARTESIAN_POINT('Ctrl Pts',(-1.67239348737615,18.048,130.182987060467));
#148746=CARTESIAN_POINT('Ctrl Pts',(-2.21024254310115E-15,18.048,128.688869413408));
#148747=CARTESIAN_POINT('Ctrl Pts',(1.67239348737616,18.048,127.194751766349));
#148748=CARTESIAN_POINT('Ctrl Pts',(3.31631129755346,17.7406985030951,125.70063411929));
#148749=CARTESIAN_POINT('Ctrl Pts',(4.96022910773077,17.4333970061901,124.206516472231));
#148750=CARTESIAN_POINT('Ctrl Pts',(6.51968959134575,16.8292587962898,122.712398825173));
#148751=CARTESIAN_POINT('Ctrl Pts',(8.07915007496071,16.2251205863895,121.218281178114));
#148752=CARTESIAN_POINT('Ctrl Pts',(9.50104767561053,15.3447188656481,119.724163531055));
#148753=CARTESIAN_POINT('Ctrl Pts',(10.9229452762603,14.4643171449067,118.230045883996));
#148754=CARTESIAN_POINT('Ctrl Pts',(12.1588589765331,13.3376329379985,116.735928236937));
#148755=CARTESIAN_POINT('Ctrl Pts',(13.3947726768058,12.2109487310903,115.241810589878));
#148756=CARTESIAN_POINT('Ctrl Pts',(14.4026149179538,10.8763499173728,113.74769294282));
#148757=CARTESIAN_POINT('Ctrl Pts',(15.4104571591017,9.54175110365538,112.253575295761));
#148758=CARTESIAN_POINT('Ctrl Pts',(16.1559070823762,8.04468584505496,110.759457648702));
#148759=CARTESIAN_POINT('Ctrl Pts',(16.9013570056506,6.54762058645456,109.265340001643));
#148760=CARTESIAN_POINT('Ctrl Pts',(17.3590292079831,4.93906964482096,107.771222354584));
#148761=CARTESIAN_POINT('Ctrl Pts',(17.8167014103155,3.33051870318735,106.277104707526));
#148762=CARTESIAN_POINT('Ctrl Pts',(17.9710104137728,1.66525935159367,104.782987060467));
#148763=CARTESIAN_POINT('Ctrl Pts',(18.1253194172301,3.32956716117513E-15,
103.288869413408));
#148764=CARTESIAN_POINT('Ctrl Pts',(17.9710104137728,-1.66525935159367,
101.794751766349));
#148765=CARTESIAN_POINT('Ctrl Pts',(17.8167014103155,-3.33051870318736,
100.30063411929));
#148766=CARTESIAN_POINT('Ctrl Pts',(17.3590292079831,-4.93906964482095,
98.8065164722314));
#148767=CARTESIAN_POINT('Ctrl Pts',(16.9013570056506,-6.54762058645456,
97.3123988251725));
#148768=CARTESIAN_POINT('Ctrl Pts',(16.1559070823762,-8.04468584505497,
95.8182811781136));
#148769=CARTESIAN_POINT('Ctrl Pts',(15.4104571591017,-9.54175110365538,
94.3241635310548));
#148770=CARTESIAN_POINT('Ctrl Pts',(14.4026149179538,-10.8763499173728,
92.8300458839961));
#148771=CARTESIAN_POINT('Ctrl Pts',(13.3947726768058,-12.2109487310903,
91.3359282369372));
#148772=CARTESIAN_POINT('Ctrl Pts',(12.1588589765331,-13.3376329379985,
89.8418105898784));
#148773=CARTESIAN_POINT('Ctrl Pts',(10.9229452762603,-14.4643171449067,
88.3476929428195));
#148774=CARTESIAN_POINT('Ctrl Pts',(9.50104767561053,-15.3447188656481,
86.8535752957606));
#148775=CARTESIAN_POINT('Ctrl Pts',(8.07915007496071,-16.2251205863895,
85.359457648702));
#148776=CARTESIAN_POINT('Ctrl Pts',(6.51968959134574,-16.8292587962898,
83.8653400016432));
#148777=CARTESIAN_POINT('Ctrl Pts',(4.96022910773078,-17.4333970061901,
82.3712223545843));
#148778=CARTESIAN_POINT('Ctrl Pts',(3.31631129755346,-17.7406985030951,
80.8771047075254));
#148779=CARTESIAN_POINT('Ctrl Pts',(1.67239348737615,-18.048,79.3829870604665));
#148780=CARTESIAN_POINT('Ctrl Pts',(0.,-18.048,77.8888694134079));
#148781=CARTESIAN_POINT('Ctrl Pts',(-1.67239348737615,-18.048,76.394751766349));
#148782=CARTESIAN_POINT('Ctrl Pts',(-3.31631129755346,-17.7406985030951,
74.9006341192902));
#148783=CARTESIAN_POINT('Ctrl Pts',(-4.96022910773077,-17.4333970061901,
73.4065164722313));
#148784=CARTESIAN_POINT('Ctrl Pts',(-6.51968959134574,-16.8292587962898,
71.9123988251724));
#148785=CARTESIAN_POINT('Ctrl Pts',(-8.07915007496071,-16.2251205863895,
70.4182811781138));
#148786=CARTESIAN_POINT('Ctrl Pts',(-9.50104767561052,-15.3447188656481,
68.9241635310549));
#148787=CARTESIAN_POINT('Ctrl Pts',(-10.9229452762603,-14.4643171449067,
67.430045883996));
#148788=CARTESIAN_POINT('Ctrl Pts',(-12.1588589765331,-13.3376329379985,
65.9359282369372));
#148789=CARTESIAN_POINT('Ctrl Pts',(-13.3947726768058,-12.2109487310903,
64.4418105898783));
#148790=CARTESIAN_POINT('Ctrl Pts',(-14.4026149179538,-10.8763499173728,
62.9476929428197));
#148791=CARTESIAN_POINT('Ctrl Pts',(-15.4104571591017,-9.54175110365538,
61.4535752957608));
#148792=CARTESIAN_POINT('Ctrl Pts',(-16.1559070823762,-8.04468584505497,
59.9594576487019));
#148793=CARTESIAN_POINT('Ctrl Pts',(-16.9013570056506,-6.54762058645456,
58.4653400016431));
#148794=CARTESIAN_POINT('Ctrl Pts',(-17.3590292079831,-4.93906964482095,
56.9712223545842));
#148795=CARTESIAN_POINT('Ctrl Pts',(-17.8167014103155,-3.33051870318735,
55.4771047075255));
#148796=CARTESIAN_POINT('Ctrl Pts',(-17.9710104137728,-1.66525935159368,
53.9829870604667));
#148797=CARTESIAN_POINT('Ctrl Pts',(-18.1253194172301,-1.10985572039171E-15,
52.4888694134078));
#148798=CARTESIAN_POINT('Ctrl Pts',(-17.9710104137728,1.66525935159367,
50.9947517663489));
#148799=CARTESIAN_POINT('Ctrl Pts',(-17.8167014103155,3.33051870318735,
49.5006341192901));
#148800=CARTESIAN_POINT('Ctrl Pts',(-17.3590292079831,4.93906964482096,
48.0065164722314));
#148801=CARTESIAN_POINT('Ctrl Pts',(-16.9013570056506,6.54762058645456,
46.5123988251726));
#148802=CARTESIAN_POINT('Ctrl Pts',(-16.1559070823762,8.04468584505497,
45.0182811781137));
#148803=CARTESIAN_POINT('Ctrl Pts',(-15.4104571591017,9.54175110365538,
43.5241635310548));
#148804=CARTESIAN_POINT('Ctrl Pts',(-14.4026149179538,10.8763499173728,
42.0300458839959));
#148805=CARTESIAN_POINT('Ctrl Pts',(-13.3947726768058,12.2109487310903,
40.5359282369373));
#148806=CARTESIAN_POINT('Ctrl Pts',(-12.1588589765331,13.3376329379985,
39.0418105898784));
#148807=CARTESIAN_POINT('Ctrl Pts',(-10.9229452762603,14.4643171449067,
37.5476929428196));
#148808=CARTESIAN_POINT('Ctrl Pts',(-9.50104767561052,15.3447188656481,
36.0535752957607));
#148809=CARTESIAN_POINT('Ctrl Pts',(-8.07915007496071,16.2251205863895,
34.5594576487018));
#148810=CARTESIAN_POINT('Ctrl Pts',(-6.51968959134574,16.8292587962898,
33.0653400016432));
#148811=CARTESIAN_POINT('Ctrl Pts',(-4.96022910773078,17.4333970061901,
31.5712223545843));
#148812=CARTESIAN_POINT('Ctrl Pts',(-3.31631129755346,17.7406985030951,
30.0771047075255));
#148813=CARTESIAN_POINT('Ctrl Pts',(-1.67239348737615,18.048,28.5829870604666));
#148814=CARTESIAN_POINT('Ctrl Pts',(-2.21024254310115E-15,18.048,27.0888694134077));
#148815=CARTESIAN_POINT('Ctrl Pts',(1.67239348737616,18.048,25.5947517663491));
#148816=CARTESIAN_POINT('Ctrl Pts',(3.31631129755346,17.7406985030951,24.1006341192902));
#148817=CARTESIAN_POINT('Ctrl Pts',(4.96022910773077,17.4333970061901,22.6065164722313));
#148818=CARTESIAN_POINT('Ctrl Pts',(6.51968959134575,16.8292587962898,21.1123988251725));
#148819=CARTESIAN_POINT('Ctrl Pts',(8.07915007496071,16.2251205863895,19.6182811781136));
#148820=CARTESIAN_POINT('Ctrl Pts',(9.50104767561053,15.3447188656481,18.1241635310549));
#148821=CARTESIAN_POINT('Ctrl Pts',(10.9229452762603,14.4643171449067,16.6300458839961));
#148822=CARTESIAN_POINT('Ctrl Pts',(12.1588589765331,13.3376329379985,15.1359282369372));
#148823=CARTESIAN_POINT('Ctrl Pts',(13.3947726768058,12.2109487310903,13.6418105898783));
#148824=CARTESIAN_POINT('Ctrl Pts',(14.4026149179538,10.8763499173728,12.1476929428195));
#148825=CARTESIAN_POINT('Ctrl Pts',(15.4104571591017,9.54175110365538,10.6535752957608));
#148826=CARTESIAN_POINT('Ctrl Pts',(16.1559070823762,8.04468584505496,9.15945764870196));
#148827=CARTESIAN_POINT('Ctrl Pts',(16.9013570056506,6.54762058645456,7.6653400016431));
#148828=CARTESIAN_POINT('Ctrl Pts',(17.3590292079831,4.93906964482096,6.17122235458423));
#148829=CARTESIAN_POINT('Ctrl Pts',(17.8167014103155,3.33051870318735,4.67710470752536));
#148830=CARTESIAN_POINT('Ctrl Pts',(17.9710104137728,1.66525935159367,3.18298706046671));
#148831=CARTESIAN_POINT('Ctrl Pts',(18.1253194172301,3.32956716117513E-15,
1.68886941340785));
#148832=CARTESIAN_POINT('Ctrl Pts',(17.9710104137728,-1.66525935159367,
0.194751766348977));
#148833=CARTESIAN_POINT('Ctrl Pts',(17.8167014103155,-3.33051870318736,
-1.29936588070989));
#148834=CARTESIAN_POINT('Ctrl Pts',(17.3590292079831,-4.93906964482095,
-2.79348352776876));
#148835=CARTESIAN_POINT('Ctrl Pts',(16.9013570056506,-6.54762058645456,
-4.2876011748274));
#148836=CARTESIAN_POINT('Ctrl Pts',(16.1559070823762,-8.04468584505497,
-5.78171882188627));
#148837=CARTESIAN_POINT('Ctrl Pts',(15.4104571591017,-9.54175110365538,
-7.27583646894514));
#148838=CARTESIAN_POINT('Ctrl Pts',(14.4026149179538,-10.8763499173728,
-8.76995411600401));
#148839=CARTESIAN_POINT('Ctrl Pts',(13.3947726768058,-12.2109487310903,
-10.2640717630629));
#148840=CARTESIAN_POINT('Ctrl Pts',(12.1588589765331,-13.3376329379985,
-11.7581894101215));
#148841=CARTESIAN_POINT('Ctrl Pts',(10.9229452762603,-14.4643171449067,
-13.2523070571804));
#148842=CARTESIAN_POINT('Ctrl Pts',(9.50104767561053,-15.3447188656481,
-14.7464247042393));
#148843=CARTESIAN_POINT('Ctrl Pts',(8.07915007496071,-16.2251205863895,
-16.2405423512981));
#148844=CARTESIAN_POINT('Ctrl Pts',(6.51968959134574,-16.8292587962898,
-17.734659998357));
#148845=CARTESIAN_POINT('Ctrl Pts',(4.96022910773078,-17.4333970061901,
-19.2287776454156));
#148846=CARTESIAN_POINT('Ctrl Pts',(3.31631129755346,-17.7406985030951,
-20.7228952924745));
#148847=CARTESIAN_POINT('Ctrl Pts',(1.67239348737615,-18.048,-22.2170129395334));
#148848=CARTESIAN_POINT('Ctrl Pts',(0.,-18.048,-23.7111305865922));
#148849=CARTESIAN_POINT('Ctrl Pts',(-1.67239348737615,-18.048,-25.2052482336511));
#148850=CARTESIAN_POINT('Ctrl Pts',(-3.31631129755346,-17.7406985030951,
-26.6993658807098));
#148851=CARTESIAN_POINT('Ctrl Pts',(-4.96022910773077,-17.4333970061901,
-28.1934835277686));
#148852=CARTESIAN_POINT('Ctrl Pts',(-6.51968959134574,-16.8292587962898,
-29.6876011748275));
#148853=CARTESIAN_POINT('Ctrl Pts',(-8.07915007496071,-16.2251205863895,
-31.1817188218864));
#148854=CARTESIAN_POINT('Ctrl Pts',(-9.50104767561052,-15.3447188656481,
-32.6758364689452));
#148855=CARTESIAN_POINT('Ctrl Pts',(-10.9229452762603,-14.4643171449067,
-34.1699541160039));
#148856=CARTESIAN_POINT('Ctrl Pts',(-12.1588589765331,-13.3376329379985,
-35.6640717630627));
#148857=CARTESIAN_POINT('Ctrl Pts',(-13.3947726768058,-12.2109487310903,
-37.1581894101216));
#148858=CARTESIAN_POINT('Ctrl Pts',(-14.4026149179538,-10.8763499173728,
-38.6523070571805));
#148859=CARTESIAN_POINT('Ctrl Pts',(-15.4104571591017,-9.54175110365538,
-40.1464247042394));
#148860=CARTESIAN_POINT('Ctrl Pts',(-16.1559070823762,-8.04468584505497,
-41.640542351298));
#148861=CARTESIAN_POINT('Ctrl Pts',(-16.9013570056506,-6.54762058645456,
-43.1346599983569));
#148862=CARTESIAN_POINT('Ctrl Pts',(-17.3590292079831,-4.93906964482095,
-44.6287776454157));
#148863=CARTESIAN_POINT('Ctrl Pts',(-17.8167014103155,-3.33051870318735,
-46.1228952924746));
#148864=CARTESIAN_POINT('Ctrl Pts',(-17.9710104137728,-1.66525935159368,
-47.6170129395335));
#148865=CARTESIAN_POINT('Ctrl Pts',(-18.1253194172301,-1.10985572039171E-15,
-49.1111305865921));
#148866=CARTESIAN_POINT('Ctrl Pts',(-17.9710104137728,1.66525935159367,
-50.605248233651));
#148867=CARTESIAN_POINT('Ctrl Pts',(-17.8167014103155,3.33051870318735,
-52.0993658807098));
#148868=CARTESIAN_POINT('Ctrl Pts',(-17.3590292079831,4.93906964482096,
-53.5934835277687));
#148869=CARTESIAN_POINT('Ctrl Pts',(-16.9013570056506,6.54762058645456,
-55.0876011748276));
#148870=CARTESIAN_POINT('Ctrl Pts',(-16.1559070823762,8.04468584505497,
-56.5817188218862));
#148871=CARTESIAN_POINT('Ctrl Pts',(-15.4104571591017,9.54175110365538,
-58.0758364689451));
#148872=CARTESIAN_POINT('Ctrl Pts',(-14.4026149179538,10.8763499173728,
-59.569954116004));
#148873=CARTESIAN_POINT('Ctrl Pts',(-13.3947726768058,12.2109487310903,
-61.0640717630628));
#148874=CARTESIAN_POINT('Ctrl Pts',(-12.1588589765331,13.3376329379985,
-62.5581894101217));
#148875=CARTESIAN_POINT('Ctrl Pts',(-10.9229452762603,14.4643171449067,
-64.0523070571803));
#148876=CARTESIAN_POINT('Ctrl Pts',(-9.50104767561052,15.3447188656481,
-65.5464247042392));
#148877=CARTESIAN_POINT('Ctrl Pts',(-8.07915007496071,16.2251205863895,
-67.0405423512981));
#148878=CARTESIAN_POINT('Ctrl Pts',(-6.51968959134574,16.8292587962898,
-68.5346599983569));
#148879=CARTESIAN_POINT('Ctrl Pts',(-4.96022910773078,17.4333970061901,
-70.0287776454158));
#148880=CARTESIAN_POINT('Ctrl Pts',(-3.31631129755346,17.7406985030951,
-71.5228952924745));
#148881=CARTESIAN_POINT('Ctrl Pts',(-1.67239348737615,18.048,-73.0170129395333));
#148882=CARTESIAN_POINT('Ctrl Pts',(-2.21024254310115E-15,18.048,-74.5111305865922));
#148883=CARTESIAN_POINT('Ctrl Pts',(1.67239348737616,18.048,-76.0052482336511));
#148884=CARTESIAN_POINT('Ctrl Pts',(3.31631129755346,17.7406985030951,-77.4993658807099));
#148885=CARTESIAN_POINT('Ctrl Pts',(4.96022910773077,17.4333970061901,-78.9934835277686));
#148886=CARTESIAN_POINT('Ctrl Pts',(6.51968959134575,16.8292587962898,-80.4876011748274));
#148887=CARTESIAN_POINT('Ctrl Pts',(8.07915007496071,16.2251205863895,-81.9817188218863));
#148888=CARTESIAN_POINT('Ctrl Pts',(9.50104767561053,15.3447188656481,-83.4758364689452));
#148889=CARTESIAN_POINT('Ctrl Pts',(10.9229452762603,14.4643171449067,-84.9699541160041));
#148890=CARTESIAN_POINT('Ctrl Pts',(12.1588589765331,13.3376329379985,-86.4640717630627));
#148891=CARTESIAN_POINT('Ctrl Pts',(13.3947726768058,12.2109487310903,-87.9581894101216));
#148892=CARTESIAN_POINT('Ctrl Pts',(14.4026149179538,10.8763499173728,-89.4523070571804));
#148893=CARTESIAN_POINT('Ctrl Pts',(15.4104571591017,9.54175110365538,-90.9464247042393));
#148894=CARTESIAN_POINT('Ctrl Pts',(16.1559070823762,8.04468584505496,-92.4405423512982));
#148895=CARTESIAN_POINT('Ctrl Pts',(16.9013570056506,6.54762058645456,-93.9346599983568));
#148896=CARTESIAN_POINT('Ctrl Pts',(17.3590292079831,4.93906964482096,-95.4287776454157));
#148897=CARTESIAN_POINT('Ctrl Pts',(17.8167014103155,3.33051870318735,-96.9228952924745));
#148898=CARTESIAN_POINT('Ctrl Pts',(17.9710104137728,1.66525935159367,-98.4170129395334));
#148899=CARTESIAN_POINT('Ctrl Pts',(18.1253194172301,3.32956716117513E-15,
-99.9111305865923));
#148900=CARTESIAN_POINT('Ctrl Pts',(17.9710104137728,-1.66525935159367,
-101.405248233651));
#148901=CARTESIAN_POINT('Ctrl Pts',(17.8167014103155,-3.33051870318736,
-102.89936588071));
#148902=CARTESIAN_POINT('Ctrl Pts',(17.3590292079831,-4.93906964482095,
-104.393483527769));
#148903=CARTESIAN_POINT('Ctrl Pts',(16.9013570056506,-6.54762058645456,
-105.887601174828));
#148904=CARTESIAN_POINT('Ctrl Pts',(16.1559070823762,-8.04468584505497,
-107.381718821886));
#148905=CARTESIAN_POINT('Ctrl Pts',(15.4104571591017,-9.54175110365538,
-108.875836468945));
#148906=CARTESIAN_POINT('Ctrl Pts',(14.4026149179538,-10.8763499173728,
-110.369954116004));
#148907=CARTESIAN_POINT('Ctrl Pts',(13.3947726768058,-12.2109487310903,
-111.864071763063));
#148908=CARTESIAN_POINT('Ctrl Pts',(12.1588589765331,-13.3376329379985,
-113.358189410122));
#148909=CARTESIAN_POINT('Ctrl Pts',(10.9229452762603,-14.4643171449067,
-114.852307057181));
#148910=CARTESIAN_POINT('Ctrl Pts',(9.50104767561053,-15.3447188656481,
-116.346424704239));
#148911=CARTESIAN_POINT('Ctrl Pts',(8.07915007496071,-16.2251205863895,
-117.840542351298));
#148912=CARTESIAN_POINT('Ctrl Pts',(6.51968959134574,-16.8292587962898,
-119.334659998357));
#148913=CARTESIAN_POINT('Ctrl Pts',(4.96022910773078,-17.4333970061901,
-120.828777645416));
#148914=CARTESIAN_POINT('Ctrl Pts',(3.31631129755346,-17.7406985030951,
-122.322895292475));
#148915=CARTESIAN_POINT('Ctrl Pts',(1.67239348737615,-18.048,-123.817012939533));
#148916=CARTESIAN_POINT('Ctrl Pts',(0.,-18.048,-125.311130586592));
#148917=CARTESIAN_POINT('Ctrl Pts',(-1.67239348737615,-18.048,-126.805248233651));
#148918=CARTESIAN_POINT('Ctrl Pts',(-3.31631129755346,-17.7406985030951,
-128.29936588071));
#148919=CARTESIAN_POINT('Ctrl Pts',(-4.96022910773077,-17.4333970061901,
-129.793483527769));
#148920=CARTESIAN_POINT('Ctrl Pts',(-6.51968959134574,-16.8292587962898,
-131.287601174827));
#148921=CARTESIAN_POINT('Ctrl Pts',(-8.07915007496071,-16.2251205863895,
-132.781718821886));
#148922=CARTESIAN_POINT('Ctrl Pts',(-9.50104767561052,-15.3447188656481,
-134.275836468945));
#148923=CARTESIAN_POINT('Ctrl Pts',(-10.9229452762603,-14.4643171449067,
-135.769954116004));
#148924=CARTESIAN_POINT('Ctrl Pts',(-12.1588589765331,-13.3376329379985,
-137.264071763063));
#148925=CARTESIAN_POINT('Ctrl Pts',(-13.3947726768058,-12.2109487310903,
-138.758189410122));
#148926=CARTESIAN_POINT('Ctrl Pts',(-14.4026149179538,-10.8763499173728,
-140.25230705718));
#148927=CARTESIAN_POINT('Ctrl Pts',(-15.4104571591017,-9.54175110365538,
-141.746424704239));
#148928=CARTESIAN_POINT('Ctrl Pts',(-16.1559070823762,-8.04468584505497,
-143.240542351298));
#148929=CARTESIAN_POINT('Ctrl Pts',(-16.9013570056506,-6.54762058645456,
-144.734659998357));
#148930=CARTESIAN_POINT('Ctrl Pts',(-17.3590292079831,-4.93906964482095,
-146.228777645416));
#148931=CARTESIAN_POINT('Ctrl Pts',(-17.8167014103155,-3.33051870318735,
-147.722895292475));
#148932=CARTESIAN_POINT('Ctrl Pts',(-17.9710104137728,-1.66525935159368,
-149.217012939533));
#148933=CARTESIAN_POINT('Ctrl Pts',(-18.1253194172301,-1.10985572039171E-15,
-150.711130586592));
#148934=CARTESIAN_POINT('Ctrl Pts',(-17.9710104137728,1.66525935159367,
-152.205248233651));
#148935=CARTESIAN_POINT('Ctrl Pts',(-17.8167014103155,3.33051870318735,
-153.69936588071));
#148936=CARTESIAN_POINT('Ctrl Pts',(-17.3590292079831,4.93906964482096,
-155.193483527769));
#148937=CARTESIAN_POINT('Ctrl Pts',(-16.9013570056506,6.54762058645456,
-156.687601174828));
#148938=CARTESIAN_POINT('Ctrl Pts',(-16.1559070823762,8.04468584505497,
-158.181718821886));
#148939=CARTESIAN_POINT('Ctrl Pts',(-15.4104571591017,9.54175110365538,
-159.675836468945));
#148940=CARTESIAN_POINT('Ctrl Pts',(-14.4026149179538,10.8763499173728,
-161.169954116004));
#148941=CARTESIAN_POINT('Ctrl Pts',(-13.3947726768058,12.2109487310903,
-162.664071763063));
#148942=CARTESIAN_POINT('Ctrl Pts',(-12.1588589765331,13.3376329379985,
-164.158189410122));
#148943=CARTESIAN_POINT('Ctrl Pts',(-10.9229452762603,14.4643171449067,
-165.65230705718));
#148944=CARTESIAN_POINT('Ctrl Pts',(-9.50104767561052,15.3447188656481,
-167.146424704239));
#148945=CARTESIAN_POINT('Ctrl Pts',(-8.07915007496071,16.2251205863895,
-168.640542351298));
#148946=CARTESIAN_POINT('Ctrl Pts',(-6.51968959134574,16.8292587962898,
-170.134659998357));
#148947=CARTESIAN_POINT('Ctrl Pts',(-4.96022910773078,17.4333970061901,
-171.628777645416));
#148948=CARTESIAN_POINT('Ctrl Pts',(-3.31631129755346,17.7406985030951,
-173.122895292475));
#148949=CARTESIAN_POINT('Ctrl Pts',(-1.67239348737615,18.048,-174.617012939534));
#148950=CARTESIAN_POINT('Ctrl Pts',(-2.21024254310115E-15,18.048,-176.111130586592));
#148951=CARTESIAN_POINT('Ctrl Pts',(1.67239348737616,18.048,-177.605248233651));
#148952=CARTESIAN_POINT('Ctrl Pts',(3.31631129755346,17.7406985030951,-179.09936588071));
#148953=CARTESIAN_POINT('Ctrl Pts',(4.96022910773077,17.4333970061901,-180.593483527769));
#148954=CARTESIAN_POINT('Ctrl Pts',(6.51968959134575,16.8292587962898,-182.087601174828));
#148955=CARTESIAN_POINT('Ctrl Pts',(8.07915007496071,16.2251205863895,-183.581718821886));
#148956=CARTESIAN_POINT('Ctrl Pts',(9.50104767561053,15.3447188656481,-185.075836468945));
#148957=CARTESIAN_POINT('Ctrl Pts',(10.9229452762603,14.4643171449067,-186.569954116004));
#148958=CARTESIAN_POINT('Ctrl Pts',(12.1588589765331,13.3376329379985,-188.064071763063));
#148959=CARTESIAN_POINT('Ctrl Pts',(13.3947726768058,12.2109487310903,-189.558189410122));
#148960=CARTESIAN_POINT('Ctrl Pts',(14.4026149179538,10.8763499173728,-191.05230705718));
#148961=CARTESIAN_POINT('Ctrl Pts',(15.4104571591017,9.54175110365538,-192.546424704239));
#148962=CARTESIAN_POINT('Ctrl Pts',(16.1559070823762,8.04468584505496,-194.040542351298));
#148963=CARTESIAN_POINT('Ctrl Pts',(16.9013570056506,6.54762058645456,-195.534659998357));
#148964=CARTESIAN_POINT('Ctrl Pts',(17.3590292079831,4.93906964482096,-197.028777645416));
#148965=CARTESIAN_POINT('Ctrl Pts',(17.8167014103155,3.33051870318735,-198.522895292475));
#148966=CARTESIAN_POINT('Ctrl Pts',(17.9710104137728,1.66525935159367,-200.017012939533));
#148967=CARTESIAN_POINT('Ctrl Pts',(18.1253194172301,3.32956716117513E-15,
-201.511130586592));
#148968=CARTESIAN_POINT('Ctrl Pts',(17.9710104137728,-1.66525935159367,
-203.005248233651));
#148969=CARTESIAN_POINT('Ctrl Pts',(17.8167014103155,-3.33051870318736,
-204.49936588071));
#148970=CARTESIAN_POINT('Ctrl Pts',(17.3590292079831,-4.93906964482095,
-205.993483527769));
#148971=CARTESIAN_POINT('Ctrl Pts',(16.9013570056506,-6.54762058645456,
-207.487601174827));
#148972=CARTESIAN_POINT('Ctrl Pts',(16.1559070823762,-8.04468584505497,
-208.981718821886));
#148973=CARTESIAN_POINT('Ctrl Pts',(15.4104571591017,-9.54175110365538,
-210.475836468945));
#148974=CARTESIAN_POINT('Ctrl Pts',(14.4026149179538,-10.8763499173728,
-211.969954116004));
#148975=CARTESIAN_POINT('Ctrl Pts',(13.3947726768058,-12.2109487310903,
-213.464071763063));
#148976=CARTESIAN_POINT('Ctrl Pts',(12.1588589765331,-13.3376329379985,
-214.958189410122));
#148977=CARTESIAN_POINT('Ctrl Pts',(10.9229452762603,-14.4643171449067,
-216.45230705718));
#148978=CARTESIAN_POINT('Ctrl Pts',(9.50104767561053,-15.3447188656481,
-217.946424704239));
#148979=CARTESIAN_POINT('Ctrl Pts',(8.07915007496071,-16.2251205863895,
-219.440542351298));
#148980=CARTESIAN_POINT('Ctrl Pts',(6.51968959134574,-16.8292587962898,
-220.934659998357));
#148981=CARTESIAN_POINT('Ctrl Pts',(4.96022910773078,-17.4333970061901,
-222.428777645416));
#148982=CARTESIAN_POINT('Ctrl Pts',(3.31631129755346,-17.7406985030951,
-223.922895292475));
#148983=CARTESIAN_POINT('Ctrl Pts',(1.67239348737615,-18.048,-225.417012939533));
#148984=CARTESIAN_POINT('Ctrl Pts',(0.,-18.048,-226.911130586592));
#148985=CARTESIAN_POINT('Ctrl Pts',(-1.67239348737615,-18.048,-228.405248233651));
#148986=CARTESIAN_POINT('Ctrl Pts',(-3.31631129755346,-17.7406985030951,
-229.89936588071));
#148987=CARTESIAN_POINT('Ctrl Pts',(-4.96022910773077,-17.4333970061901,
-231.393483527769));
#148988=CARTESIAN_POINT('Ctrl Pts',(-6.51968959134574,-16.8292587962898,
-232.887601174828));
#148989=CARTESIAN_POINT('Ctrl Pts',(-8.07915007496071,-16.2251205863895,
-234.381718821886));
#148990=CARTESIAN_POINT('Ctrl Pts',(-9.50104767561052,-15.3447188656481,
-235.875836468945));
#148991=CARTESIAN_POINT('Ctrl Pts',(-10.9229452762603,-14.4643171449067,
-237.369954116004));
#148992=CARTESIAN_POINT('Ctrl Pts',(-12.1588589765331,-13.3376329379985,
-238.864071763063));
#148993=CARTESIAN_POINT('Ctrl Pts',(-13.3947726768058,-12.2109487310903,
-240.358189410122));
#148994=CARTESIAN_POINT('Ctrl Pts',(-14.4026149179538,-10.8763499173728,
-241.852307057181));
#148995=CARTESIAN_POINT('Ctrl Pts',(-15.4104571591017,-9.54175110365538,
-243.346424704239));
#148996=CARTESIAN_POINT('Ctrl Pts',(-16.1559070823762,-8.04468584505497,
-244.840542351298));
#148997=CARTESIAN_POINT('Ctrl Pts',(-16.9013570056506,-6.54762058645456,
-246.334659998357));
#148998=CARTESIAN_POINT('Ctrl Pts',(-17.3590292079831,-4.93906964482095,
-247.828777645416));
#148999=CARTESIAN_POINT('Ctrl Pts',(-17.8167014103155,-3.33051870318735,
-249.322895292475));
#149000=CARTESIAN_POINT('Ctrl Pts',(-17.9710104137728,-1.66525935159368,
-250.817012939533));
#149001=CARTESIAN_POINT('Ctrl Pts',(-18.1253194172301,-1.10985572039171E-15,
-252.311130586592));
#149002=CARTESIAN_POINT('Ctrl Pts',(-17.9710104137728,1.66525935159367,
-253.805248233651));
#149003=CARTESIAN_POINT('Ctrl Pts',(-17.8167014103155,3.33051870318735,
-255.29936588071));
#149004=CARTESIAN_POINT('Ctrl Pts',(-17.3590292079831,4.93906964482096,
-256.793483527769));
#149005=CARTESIAN_POINT('Ctrl Pts',(-16.9013570056506,6.54762058645456,
-258.287601174827));
#149006=CARTESIAN_POINT('Ctrl Pts',(-16.1559070823762,8.04468584505497,
-259.781718821886));
#149007=CARTESIAN_POINT('Ctrl Pts',(-15.4104571591017,9.54175110365538,
-261.275836468945));
#149008=CARTESIAN_POINT('Ctrl Pts',(-14.4026149179538,10.8763499173728,
-262.769954116004));
#149009=CARTESIAN_POINT('Ctrl Pts',(-13.3947726768058,12.2109487310903,
-264.264071763063));
#149010=CARTESIAN_POINT('Ctrl Pts',(-12.1588589765331,13.3376329379985,
-265.758189410122));
#149011=CARTESIAN_POINT('Ctrl Pts',(-10.9229452762603,14.4643171449067,
-267.25230705718));
#149012=CARTESIAN_POINT('Ctrl Pts',(-9.50104767561052,15.3447188656481,
-268.746424704239));
#149013=CARTESIAN_POINT('Ctrl Pts',(-8.07915007496071,16.2251205863895,
-270.240542351298));
#149014=CARTESIAN_POINT('Ctrl Pts',(-6.51968959134574,16.8292587962898,
-271.734659998357));
#149015=CARTESIAN_POINT('Ctrl Pts',(-4.96022910773078,17.4333970061901,
-273.228777645416));
#149016=CARTESIAN_POINT('Ctrl Pts',(-3.31631129755346,17.7406985030951,
-274.722895292475));
#149017=CARTESIAN_POINT('Ctrl Pts',(-1.67239348737615,18.048,-276.217012939533));
#149018=CARTESIAN_POINT('Ctrl Pts',(-2.21024254310115E-15,18.048,-277.711130586592));
#149019=CARTESIAN_POINT('Ctrl Pts',(1.67239348737616,18.048,-279.205248233651));
#149020=CARTESIAN_POINT('Ctrl Pts',(3.31631129755346,17.7406985030951,-280.69936588071));
#149021=CARTESIAN_POINT('Ctrl Pts',(4.96022910773077,17.4333970061901,-282.193483527769));
#149022=CARTESIAN_POINT('Ctrl Pts',(6.51968959134575,16.8292587962898,-283.687601174827));
#149023=CARTESIAN_POINT('Ctrl Pts',(8.07915007496071,16.2251205863895,-285.181718821886));
#149024=CARTESIAN_POINT('Ctrl Pts',(9.50104767561053,15.3447188656481,-286.675836468945));
#149025=CARTESIAN_POINT('Ctrl Pts',(10.9229452762603,14.4643171449067,-288.169954116004));
#149026=CARTESIAN_POINT('Ctrl Pts',(12.1588589765331,13.3376329379985,-289.664071763063));
#149027=CARTESIAN_POINT('Ctrl Pts',(13.3947726768058,12.2109487310903,-291.158189410122));
#149028=CARTESIAN_POINT('Ctrl Pts',(14.4026149179538,10.8763499173728,-292.652307057181));
#149029=CARTESIAN_POINT('Ctrl Pts',(15.4104571591017,9.54175110365538,-294.146424704239));
#149030=CARTESIAN_POINT('Ctrl Pts',(16.1559070823762,8.04468584505496,-295.640542351298));
#149031=CARTESIAN_POINT('Ctrl Pts',(16.9013570056506,6.54762058645456,-297.134659998357));
#149032=CARTESIAN_POINT('Ctrl Pts',(17.3590292079831,4.93906964482096,-298.628777645416));
#149033=CARTESIAN_POINT('Ctrl Pts',(17.8167014103155,3.33051870318735,-300.122895292475));
#149034=CARTESIAN_POINT('Ctrl Pts',(17.9710104137728,1.66525935159367,-301.617012939533));
#149035=CARTESIAN_POINT('Ctrl Pts',(18.1253194172301,3.32956716117513E-15,
-303.111130586592));
#149036=CARTESIAN_POINT('Ctrl Pts',(17.9710104137728,-1.66525935159367,
-304.605248233651));
#149037=CARTESIAN_POINT('Ctrl Pts',(17.8167014103155,-3.33051870318736,
-306.09936588071));
#149038=CARTESIAN_POINT('Ctrl Pts',(17.3590292079831,-4.93906964482095,
-307.593483527769));
#149039=CARTESIAN_POINT('Ctrl Pts',(16.9013570056506,-6.54762058645456,
-309.087601174828));
#149040=CARTESIAN_POINT('Ctrl Pts',(16.1559070823762,-8.04468584505497,
-310.581718821886));
#149041=CARTESIAN_POINT('Ctrl Pts',(15.4104571591017,-9.54175110365538,
-312.075836468945));
#149042=CARTESIAN_POINT('Ctrl Pts',(14.4026149179538,-10.8763499173728,
-313.569954116004));
#149043=CARTESIAN_POINT('Ctrl Pts',(13.3947726768058,-12.2109487310903,
-315.064071763063));
#149044=CARTESIAN_POINT('Ctrl Pts',(12.1588589765331,-13.3376329379985,
-316.558189410122));
#149045=CARTESIAN_POINT('Ctrl Pts',(10.9229452762603,-14.4643171449067,
-318.05230705718));
#149046=CARTESIAN_POINT('Ctrl Pts',(9.50104767561053,-15.3447188656481,
-319.546424704239));
#149047=CARTESIAN_POINT('Ctrl Pts',(8.07915007496071,-16.2251205863895,
-321.040542351298));
#149048=CARTESIAN_POINT('Ctrl Pts',(6.51968959134574,-16.8292587962898,
-322.534659998357));
#149049=CARTESIAN_POINT('Ctrl Pts',(4.96022910773078,-17.4333970061901,
-324.028777645416));
#149050=CARTESIAN_POINT('Ctrl Pts',(3.31631129755346,-17.7406985030951,
-325.522895292474));
#149051=CARTESIAN_POINT('Ctrl Pts',(1.67239348737615,-18.048,-327.017012939533));
#149052=CARTESIAN_POINT('Ctrl Pts',(0.,-18.048,-328.511130586592));
#149053=CARTESIAN_POINT('Ctrl Pts',(-1.67239348737615,-18.048,-330.005248233651));
#149054=CARTESIAN_POINT('Ctrl Pts',(-3.31631129755346,-17.7406985030951,
-331.49936588071));
#149055=CARTESIAN_POINT('Ctrl Pts',(-4.96022910773077,-17.4333970061901,
-332.993483527769));
#149056=CARTESIAN_POINT('Ctrl Pts',(-6.51968959134574,-16.8292587962898,
-334.487601174827));
#149057=CARTESIAN_POINT('Ctrl Pts',(-8.07915007496071,-16.2251205863895,
-335.981718821886));
#149058=CARTESIAN_POINT('Ctrl Pts',(-9.50104767561052,-15.3447188656481,
-337.475836468945));
#149059=CARTESIAN_POINT('Ctrl Pts',(-10.9229452762603,-14.4643171449067,
-338.969954116004));
#149060=CARTESIAN_POINT('Ctrl Pts',(-12.1588589765331,-13.3376329379985,
-340.464071763063));
#149061=CARTESIAN_POINT('Ctrl Pts',(-13.3947726768058,-12.2109487310903,
-341.958189410122));
#149062=CARTESIAN_POINT('Ctrl Pts',(-14.4026149179538,-10.8763499173728,
-343.45230705718));
#149063=CARTESIAN_POINT('Ctrl Pts',(-15.4104571591017,-9.54175110365538,
-344.946424704239));
#149064=CARTESIAN_POINT('Ctrl Pts',(-16.1559070823762,-8.04468584505497,
-346.440542351298));
#149065=CARTESIAN_POINT('Ctrl Pts',(-16.9013570056506,-6.54762058645456,
-347.934659998357));
#149066=CARTESIAN_POINT('Ctrl Pts',(-17.3590292079831,-4.93906964482095,
-349.428777645416));
#149067=CARTESIAN_POINT('Ctrl Pts',(-17.8167014103155,-3.33051870318735,
-350.922895292475));
#149068=CARTESIAN_POINT('Ctrl Pts',(-17.9710104137728,-1.66525935159368,
-352.417012939533));
#149069=CARTESIAN_POINT('Ctrl Pts',(-18.1253194172301,-1.10985572039171E-15,
-353.911130586592));
#149070=CARTESIAN_POINT('Ctrl Pts',(-17.9710104137728,1.66525935159367,
-355.405248233651));
#149071=CARTESIAN_POINT('Ctrl Pts',(-17.8167014103155,3.33051870318735,
-356.89936588071));
#149072=CARTESIAN_POINT('Ctrl Pts',(-17.3590292079831,4.93906964482096,
-358.393483527769));
#149073=CARTESIAN_POINT('Ctrl Pts',(-16.9013570056506,6.54762058645456,
-359.887601174828));
#149074=CARTESIAN_POINT('Ctrl Pts',(-16.1559070823762,8.04468584505497,
-361.381718821886));
#149075=CARTESIAN_POINT('Ctrl Pts',(-15.4104571591017,9.54175110365538,
-362.875836468945));
#149076=CARTESIAN_POINT('Ctrl Pts',(-14.4026149179538,10.8763499173728,
-364.369954116004));
#149077=CARTESIAN_POINT('Ctrl Pts',(-13.3947726768058,12.2109487310903,
-365.864071763063));
#149078=CARTESIAN_POINT('Ctrl Pts',(-12.1588589765331,13.3376329379985,
-367.358189410122));
#149079=CARTESIAN_POINT('Ctrl Pts',(-10.9229452762603,14.4643171449067,
-368.85230705718));
#149080=CARTESIAN_POINT('Ctrl Pts',(-9.50104767561052,15.3447188656481,
-370.346424704239));
#149081=CARTESIAN_POINT('Ctrl Pts',(-8.07915007496071,16.2251205863895,
-371.840542351298));
#149082=CARTESIAN_POINT('Ctrl Pts',(-6.51968959134574,16.8292587962898,
-373.334659998357));
#149083=CARTESIAN_POINT('Ctrl Pts',(-4.96022910773078,17.4333970061901,
-374.828777645416));
#149084=CARTESIAN_POINT('Ctrl Pts',(-3.31631129755346,17.7406985030951,
-376.322895292475));
#149085=CARTESIAN_POINT('Ctrl Pts',(-1.67239348737615,18.048,-377.817012939533));
#149086=CARTESIAN_POINT('Ctrl Pts',(-2.21024254310115E-15,18.048,-379.311130586592));
#149087=CARTESIAN_POINT('Ctrl Pts',(1.67239348737616,18.048,-380.805248233651));
#149088=CARTESIAN_POINT('Ctrl Pts',(3.31631129755346,17.7406985030951,-382.29936588071));
#149089=CARTESIAN_POINT('Ctrl Pts',(4.96022910773077,17.4333970061901,-383.793483527769));
#149090=CARTESIAN_POINT('Ctrl Pts',(6.51968959134575,16.8292587962898,-385.287601174827));
#149091=CARTESIAN_POINT('Ctrl Pts',(8.07915007496071,16.2251205863895,-386.781718821886));
#149092=CARTESIAN_POINT('Ctrl Pts',(9.50104767561053,15.3447188656481,-388.275836468945));
#149093=CARTESIAN_POINT('Ctrl Pts',(10.9229452762603,14.4643171449067,-389.769954116004));
#149094=CARTESIAN_POINT('Ctrl Pts',(12.1588589765331,13.3376329379985,-391.264071763063));
#149095=CARTESIAN_POINT('Ctrl Pts',(13.3947726768058,12.2109487310903,-392.758189410122));
#149096=CARTESIAN_POINT('Ctrl Pts',(14.4026149179538,10.8763499173728,-394.25230705718));
#149097=CARTESIAN_POINT('Ctrl Pts',(15.4104571591017,9.54175110365538,-395.746424704239));
#149098=CARTESIAN_POINT('Ctrl Pts',(16.1559070823762,8.04468584505496,-397.240542351298));
#149099=CARTESIAN_POINT('Ctrl Pts',(16.9013570056506,6.54762058645456,-398.734659998357));
#149100=CARTESIAN_POINT('Ctrl Pts',(17.3590292079831,4.93906964482096,-400.228777645416));
#149101=CARTESIAN_POINT('Ctrl Pts',(17.8167014103155,3.33051870318735,-401.722895292475));
#149102=CARTESIAN_POINT('Ctrl Pts',(17.9710104137728,1.66525935159367,-403.217012939533));
#149103=CARTESIAN_POINT('Ctrl Pts',(18.1253194172301,3.32956716117513E-15,
-404.711130586592));
#149104=CARTESIAN_POINT('Ctrl Pts',(17.9710104137728,-1.66525935159367,
-406.205248233651));
#149105=CARTESIAN_POINT('Ctrl Pts',(17.8167014103155,-3.33051870318736,
-407.69936588071));
#149106=CARTESIAN_POINT('Ctrl Pts',(17.3590292079831,-4.93906964482095,
-409.193483527769));
#149107=CARTESIAN_POINT('Ctrl Pts',(16.9013570056506,-6.54762058645456,
-410.687601174828));
#149108=CARTESIAN_POINT('Ctrl Pts',(16.1559070823762,-8.04468584505497,
-412.181718821886));
#149109=CARTESIAN_POINT('Ctrl Pts',(15.4104571591017,-9.54175110365538,
-413.675836468945));
#149110=CARTESIAN_POINT('Ctrl Pts',(14.4026149179538,-10.8763499173728,
-415.169954116004));
#149111=CARTESIAN_POINT('Ctrl Pts',(13.3947726768058,-12.2109487310903,
-416.664071763063));
#149112=CARTESIAN_POINT('Ctrl Pts',(12.1588589765331,-13.3376329379985,
-418.158189410122));
#149113=CARTESIAN_POINT('Ctrl Pts',(10.9229452762603,-14.4643171449067,
-419.652307057181));
#149114=CARTESIAN_POINT('Ctrl Pts',(9.50104767561053,-15.3447188656481,
-421.146424704239));
#149115=CARTESIAN_POINT('Ctrl Pts',(8.07915007496071,-16.2251205863895,
-422.640542351298));
#149116=CARTESIAN_POINT('Ctrl Pts',(6.51968959134574,-16.8292587962898,
-424.134659998357));
#149117=CARTESIAN_POINT('Ctrl Pts',(4.96022910773078,-17.4333970061901,
-425.628777645416));
#149118=CARTESIAN_POINT('Ctrl Pts',(3.31631129755346,-17.7406985030951,
-427.122895292475));
#149119=CARTESIAN_POINT('Ctrl Pts',(1.67239348737615,-18.048,-428.617012939534));
#149120=CARTESIAN_POINT('Ctrl Pts',(0.,-18.048,-430.111130586592));
#149121=CARTESIAN_POINT('Ctrl Pts',(-1.67239348737615,-18.048,-431.605248233651));
#149122=CARTESIAN_POINT('Ctrl Pts',(-3.31631129755346,-17.7406985030951,
-433.09936588071));
#149123=CARTESIAN_POINT('Ctrl Pts',(-4.96022910773077,-17.4333970061901,
-434.593483527769));
#149124=CARTESIAN_POINT('Ctrl Pts',(-6.51968959134574,-16.8292587962898,
-436.087601174828));
#149125=CARTESIAN_POINT('Ctrl Pts',(-8.07915007496071,-16.2251205863895,
-437.581718821886));
#149126=CARTESIAN_POINT('Ctrl Pts',(-9.50104767561052,-15.3447188656481,
-439.075836468945));
#149127=CARTESIAN_POINT('Ctrl Pts',(-10.9229452762603,-14.4643171449067,
-440.569954116004));
#149128=CARTESIAN_POINT('Ctrl Pts',(-12.1588589765331,-13.3376329379985,
-442.064071763063));
#149129=CARTESIAN_POINT('Ctrl Pts',(-13.3947726768058,-12.2109487310903,
-443.558189410122));
#149130=CARTESIAN_POINT('Ctrl Pts',(-14.4026149179538,-10.8763499173728,
-445.05230705718));
#149131=CARTESIAN_POINT('Ctrl Pts',(-15.4104571591017,-9.54175110365538,
-446.546424704239));
#149132=CARTESIAN_POINT('Ctrl Pts',(-16.1559070823762,-8.04468584505497,
-448.040542351298));
#149133=CARTESIAN_POINT('Ctrl Pts',(-16.9013570056506,-6.54762058645456,
-449.534659998357));
#149134=CARTESIAN_POINT('Ctrl Pts',(-17.3590292079831,-4.93906964482095,
-451.028777645416));
#149135=CARTESIAN_POINT('Ctrl Pts',(-17.8167014103155,-3.33051870318735,
-452.522895292475));
#149136=CARTESIAN_POINT('Ctrl Pts',(-17.9710104137728,-1.66525935159368,
-454.017012939533));
#149137=CARTESIAN_POINT('Ctrl Pts',(-18.1253194172301,-1.10985572039171E-15,
-455.511130586592));
#149138=CARTESIAN_POINT('Ctrl Pts',(-17.9710104137728,1.66525935159367,
-457.005248233651));
#149139=CARTESIAN_POINT('Ctrl Pts',(-17.8167014103155,3.33051870318735,
-458.49936588071));
#149140=CARTESIAN_POINT('Ctrl Pts',(-17.3590292079831,4.93906964482096,
-459.993483527769));
#149141=CARTESIAN_POINT('Ctrl Pts',(-16.9013570056506,6.54762058645456,
-461.487601174828));
#149142=CARTESIAN_POINT('Ctrl Pts',(-16.1559070823762,8.04468584505497,
-462.981718821886));
#149143=CARTESIAN_POINT('Ctrl Pts',(-15.4104571591017,9.54175110365538,
-464.475836468945));
#149144=CARTESIAN_POINT('Ctrl Pts',(-14.4026149179538,10.8763499173728,
-465.969954116004));
#149145=CARTESIAN_POINT('Ctrl Pts',(-13.3947726768058,12.2109487310903,
-467.464071763063));
#149146=CARTESIAN_POINT('Ctrl Pts',(-12.1588589765331,13.3376329379985,
-468.958189410122));
#149147=CARTESIAN_POINT('Ctrl Pts',(-10.9229452762603,14.4643171449067,
-470.45230705718));
#149148=CARTESIAN_POINT('Ctrl Pts',(-9.50104767561052,15.3447188656481,
-471.946424704239));
#149149=CARTESIAN_POINT('Ctrl Pts',(-8.07915007496071,16.2251205863895,
-473.440542351298));
#149150=CARTESIAN_POINT('Ctrl Pts',(-6.51968959134574,16.8292587962898,
-474.934659998357));
#149151=CARTESIAN_POINT('Ctrl Pts',(-4.96022910773078,17.4333970061901,
-476.428777645416));
#149152=CARTESIAN_POINT('Ctrl Pts',(-3.31631129755346,17.7406985030951,
-477.922895292475));
#149153=CARTESIAN_POINT('Ctrl Pts',(-1.67239348737615,18.048,-479.417012939533));
#149154=CARTESIAN_POINT('Ctrl Pts',(-2.21024254310115E-15,18.048,-480.911130586592));
#149155=CARTESIAN_POINT('Ctrl Pts',(1.67239348737616,18.048,-482.405248233651));
#149156=CARTESIAN_POINT('Ctrl Pts',(3.31631129755346,17.7406985030951,-483.89936588071));
#149157=CARTESIAN_POINT('Ctrl Pts',(4.96022910773077,17.4333970061901,-485.393483527769));
#149158=CARTESIAN_POINT('Ctrl Pts',(6.51968959134575,16.8292587962898,-486.887601174828));
#149159=CARTESIAN_POINT('Ctrl Pts',(8.07915007496071,16.2251205863895,-488.381718821887));
#149160=CARTESIAN_POINT('Ctrl Pts',(9.50104767561053,15.3447188656481,-489.875836468945));
#149161=CARTESIAN_POINT('Ctrl Pts',(10.9229452762603,14.4643171449067,-491.369954116004));
#149162=CARTESIAN_POINT('Ctrl Pts',(12.1588589765331,13.3376329379985,-492.864071763063));
#149163=CARTESIAN_POINT('Ctrl Pts',(13.3947726768058,12.2109487310903,-494.358189410122));
#149164=CARTESIAN_POINT('Ctrl Pts',(14.4026149179538,10.8763499173728,-495.852307057181));
#149165=CARTESIAN_POINT('Ctrl Pts',(15.4104571591017,9.54175110365538,-497.346424704239));
#149166=CARTESIAN_POINT('Ctrl Pts',(16.1559070823762,8.04468584505496,-498.840542351298));
#149167=CARTESIAN_POINT('Ctrl Pts',(16.9013570056506,6.54762058645456,-500.334659998357));
#149168=CARTESIAN_POINT('Ctrl Pts',(17.3590292079831,4.93906964482096,-501.828777645416));
#149169=CARTESIAN_POINT('Ctrl Pts',(17.8167014103155,3.33051870318735,-503.322895292475));
#149170=CARTESIAN_POINT('Ctrl Pts',(17.9710104137728,1.66525935159367,-504.817012939534));
#149171=CARTESIAN_POINT('Ctrl Pts',(18.1253194172301,3.32956716117513E-15,
-506.311130586592));
#149172=CARTESIAN_POINT('Ctrl Pts',(17.9710104137728,-1.66525935159367,
-507.805248233651));
#149173=CARTESIAN_POINT('Ctrl Pts',(17.8167014103155,-3.33051870318736,
-509.29936588071));
#149174=CARTESIAN_POINT('Ctrl Pts',(17.3590292079831,-4.93906964482095,
-510.793483527769));
#149175=CARTESIAN_POINT('Ctrl Pts',(16.9013570056506,-6.54762058645456,
-512.287601174828));
#149176=CARTESIAN_POINT('Ctrl Pts',(16.1559070823762,-8.04468584505497,
-513.781718821886));
#149177=CARTESIAN_POINT('Ctrl Pts',(15.4104571591017,-9.54175110365538,
-515.275836468945));
#149178=CARTESIAN_POINT('Ctrl Pts',(14.4026149179538,-10.8763499173728,
-516.769954116004));
#149179=CARTESIAN_POINT('Ctrl Pts',(13.3947726768058,-12.2109487310903,
-518.264071763063));
#149180=CARTESIAN_POINT('Ctrl Pts',(12.1588589765331,-13.3376329379985,
-519.758189410122));
#149181=CARTESIAN_POINT('Ctrl Pts',(10.9229452762603,-14.4643171449067,
-521.252307057181));
#149182=CARTESIAN_POINT('Ctrl Pts',(9.50104767561053,-15.3447188656481,
-522.746424704239));
#149183=CARTESIAN_POINT('Ctrl Pts',(8.07915007496071,-16.2251205863895,
-524.240542351298));
#149184=CARTESIAN_POINT('Ctrl Pts',(6.51968959134574,-16.8292587962898,
-525.734659998357));
#149185=CARTESIAN_POINT('Ctrl Pts',(4.96022910773078,-17.4333970061901,
-527.228777645416));
#149186=CARTESIAN_POINT('Ctrl Pts',(3.31631129755346,-17.7406985030951,
-528.722895292475));
#149187=CARTESIAN_POINT('Ctrl Pts',(1.67239348737615,-18.048,-530.217012939533));
#149188=CARTESIAN_POINT('Ctrl Pts',(0.,-18.048,-531.711130586592));
#149189=CARTESIAN_POINT('Ctrl Pts',(-1.67239348737615,-18.048,-533.205248233651));
#149190=CARTESIAN_POINT('Ctrl Pts',(-3.31631129755346,-17.7406985030951,
-534.69936588071));
#149191=CARTESIAN_POINT('Ctrl Pts',(-4.96022910773077,-17.4333970061901,
-536.193483527769));
#149192=CARTESIAN_POINT('Ctrl Pts',(-6.51968959134574,-16.8292587962898,
-537.687601174827));
#149193=CARTESIAN_POINT('Ctrl Pts',(-8.07915007496071,-16.2251205863895,
-539.181718821886));
#149194=CARTESIAN_POINT('Ctrl Pts',(-9.50104767561052,-15.3447188656481,
-540.675836468945));
#149195=CARTESIAN_POINT('Ctrl Pts',(-10.9229452762603,-14.4643171449067,
-542.169954116004));
#149196=CARTESIAN_POINT('Ctrl Pts',(-12.1588589765331,-13.3376329379985,
-543.664071763063));
#149197=CARTESIAN_POINT('Ctrl Pts',(-13.3947726768058,-12.2109487310903,
-545.158189410122));
#149198=CARTESIAN_POINT('Ctrl Pts',(-14.4026149179538,-10.8763499173728,
-546.65230705718));
#149199=CARTESIAN_POINT('Ctrl Pts',(-15.4104571591017,-9.54175110365538,
-548.14642470424));
#149200=CARTESIAN_POINT('Ctrl Pts',(-16.1559070823762,-8.04468584505497,
-549.640542351298));
#149201=CARTESIAN_POINT('Ctrl Pts',(-16.9013570056506,-6.54762058645456,
-551.134659998357));
#149202=CARTESIAN_POINT('Ctrl Pts',(-17.3590292079831,-4.93906964482095,
-552.628777645416));
#149203=CARTESIAN_POINT('Ctrl Pts',(-17.8167014103155,-3.33051870318735,
-554.122895292474));
#149204=CARTESIAN_POINT('Ctrl Pts',(-17.9710104137728,-1.66525935159368,
-555.617012939533));
#149205=CARTESIAN_POINT('Ctrl Pts',(-18.1253194172301,-1.10985572039171E-15,
-557.111130586592));
#149206=CARTESIAN_POINT('Ctrl Pts',(-17.9710104137728,1.66525935159367,
-558.605248233651));
#149207=CARTESIAN_POINT('Ctrl Pts',(-17.8167014103155,3.33051870318735,
-560.09936588071));
#149208=CARTESIAN_POINT('Ctrl Pts',(-17.3590292079831,4.93906964482096,
-561.593483527769));
#149209=CARTESIAN_POINT('Ctrl Pts',(-16.9013570056506,6.54762058645456,
-563.087601174828));
#149210=CARTESIAN_POINT('Ctrl Pts',(-16.1559070823762,8.04468584505497,
-564.581718821887));
#149211=CARTESIAN_POINT('Ctrl Pts',(-15.4104571591017,9.54175110365538,
-566.075836468945));
#149212=CARTESIAN_POINT('Ctrl Pts',(-14.4026149179538,10.8763499173728,
-567.569954116004));
#149213=CARTESIAN_POINT('Ctrl Pts',(-13.3947726768058,12.2109487310903,
-569.064071763063));
#149214=CARTESIAN_POINT('Ctrl Pts',(-12.1588589765331,13.3376329379985,
-570.558189410121));
#149215=CARTESIAN_POINT('Ctrl Pts',(-10.9229452762603,14.4643171449067,
-572.05230705718));
#149216=CARTESIAN_POINT('Ctrl Pts',(-9.50104767561052,15.3447188656481,
-573.546424704239));
#149217=CARTESIAN_POINT('Ctrl Pts',(-8.07915007496071,16.2251205863895,
-575.040542351298));
#149218=CARTESIAN_POINT('Ctrl Pts',(-6.51968959134574,16.8292587962898,
-576.534659998357));
#149219=CARTESIAN_POINT('Ctrl Pts',(-4.96022910773078,17.4333970061901,
-578.028777645416));
#149220=CARTESIAN_POINT('Ctrl Pts',(-3.31631129755346,17.7406985030951,
-579.522895292475));
#149221=CARTESIAN_POINT('Ctrl Pts',(-1.67239348737615,18.048,-581.017012939534));
#149222=CARTESIAN_POINT('Ctrl Pts',(-2.21024254310115E-15,18.048,-582.511130586592));
#149223=CARTESIAN_POINT('Ctrl Pts',(1.67239348737616,18.048,-584.005248233651));
#149224=CARTESIAN_POINT('Ctrl Pts',(3.31631129755346,17.7406985030951,-585.49936588071));
#149225=CARTESIAN_POINT('Ctrl Pts',(4.96022910773077,17.4333970061901,-586.993483527769));
#149226=CARTESIAN_POINT('Ctrl Pts',(6.51968959134575,16.8292587962898,-588.487601174827));
#149227=CARTESIAN_POINT('Ctrl Pts',(8.07915007496071,16.2251205863895,-589.981718821886));
#149228=CARTESIAN_POINT('Ctrl Pts',(9.50104767561053,15.3447188656481,-591.475836468945));
#149229=CARTESIAN_POINT('Ctrl Pts',(10.9229452762603,14.4643171449067,-592.969954116004));
#149230=CARTESIAN_POINT('Ctrl Pts',(12.1588589765331,13.3376329379985,-594.464071763063));
#149231=CARTESIAN_POINT('Ctrl Pts',(13.3947726768058,12.2109487310903,-595.958189410122));
#149232=CARTESIAN_POINT('Ctrl Pts',(14.4026149179538,10.8763499173728,-597.45230705718));
#149233=CARTESIAN_POINT('Ctrl Pts',(15.4104571591017,9.54175110365538,-598.946424704239));
#149234=CARTESIAN_POINT('Ctrl Pts',(16.1559070823762,8.04468584505496,-600.440542351298));
#149235=CARTESIAN_POINT('Ctrl Pts',(16.9013570056506,6.54762058645456,-601.934659998357));
#149236=CARTESIAN_POINT('Ctrl Pts',(17.3590292079831,4.93906964482096,-603.428777645416));
#149237=CARTESIAN_POINT('Ctrl Pts',(17.8167014103155,3.33051870318735,-604.922895292475));
#149238=CARTESIAN_POINT('Ctrl Pts',(17.9710104137728,1.66525935159367,-606.417012939533));
#149239=CARTESIAN_POINT('Ctrl Pts',(18.1253194172301,3.32956716117513E-15,
-607.911130586592));
#149240=CARTESIAN_POINT('Ctrl Pts',(17.9710104137728,-1.66525935159367,
-609.405248233651));
#149241=CARTESIAN_POINT('Ctrl Pts',(17.8167014103155,-3.33051870318736,
-610.89936588071));
#149242=CARTESIAN_POINT('Ctrl Pts',(17.3590292079831,-4.93906964482095,
-612.393483527768));
#149243=CARTESIAN_POINT('Ctrl Pts',(16.9013570056506,-6.54762058645456,
-613.887601174828));
#149244=CARTESIAN_POINT('Ctrl Pts',(16.1559070823762,-8.04468584505497,
-615.381718821886));
#149245=CARTESIAN_POINT('Ctrl Pts',(15.4104571591017,-9.54175110365538,
-616.875836468945));
#149246=CARTESIAN_POINT('Ctrl Pts',(14.4026149179538,-10.8763499173728,
-618.369954116004));
#149247=CARTESIAN_POINT('Ctrl Pts',(13.3947726768058,-12.2109487310903,
-619.864071763063));
#149248=CARTESIAN_POINT('Ctrl Pts',(12.1588589765331,-13.3376329379985,
-621.358189410122));
#149249=CARTESIAN_POINT('Ctrl Pts',(10.9229452762603,-14.4643171449067,
-622.852307057181));
#149250=CARTESIAN_POINT('Ctrl Pts',(9.50104767561053,-15.3447188656481,
-624.346424704239));
#149251=CARTESIAN_POINT('Ctrl Pts',(8.07915007496071,-16.2251205863895,
-625.840542351298));
#149252=CARTESIAN_POINT('Ctrl Pts',(6.51968959134574,-16.8292587962898,
-627.334659998357));
#149253=CARTESIAN_POINT('Ctrl Pts',(4.96022910773078,-17.4333970061901,
-628.828777645416));
#149254=CARTESIAN_POINT('Ctrl Pts',(3.31631129755346,-17.7406985030951,
-630.322895292474));
#149255=CARTESIAN_POINT('Ctrl Pts',(1.67239348737615,-18.048,-631.817012939533));
#149256=CARTESIAN_POINT('Ctrl Pts',(0.,-18.048,-633.311130586592));
#149257=CARTESIAN_POINT('Ctrl Pts',(-1.67239348737615,-18.048,-634.805248233651));
#149258=CARTESIAN_POINT('Ctrl Pts',(-3.31631129755346,-17.7406985030951,
-636.29936588071));
#149259=CARTESIAN_POINT('Ctrl Pts',(-4.96022910773077,-17.4333970061901,
-637.793483527769));
#149260=CARTESIAN_POINT('Ctrl Pts',(-6.51968959134574,-16.8292587962898,
-639.287601174828));
#149261=CARTESIAN_POINT('Ctrl Pts',(-8.07915007496071,-16.2251205863895,
-640.781718821886));
#149262=CARTESIAN_POINT('Ctrl Pts',(-9.50104767561052,-15.3447188656481,
-642.275836468945));
#149263=CARTESIAN_POINT('Ctrl Pts',(-10.9229452762603,-14.4643171449067,
-643.769954116004));
#149264=CARTESIAN_POINT('Ctrl Pts',(-12.1588589765331,-13.3376329379985,
-645.264071763063));
#149265=CARTESIAN_POINT('Ctrl Pts',(-13.3947726768058,-12.2109487310903,
-646.758189410122));
#149266=CARTESIAN_POINT('Ctrl Pts',(-14.4026149179538,-10.8763499173728,
-648.25230705718));
#149267=CARTESIAN_POINT('Ctrl Pts',(-15.4104571591017,-9.54175110365538,
-649.746424704239));
#149268=CARTESIAN_POINT('Ctrl Pts',(-16.1559070823762,-8.04468584505497,
-651.240542351298));
#149269=CARTESIAN_POINT('Ctrl Pts',(-16.9013570056506,-6.54762058645456,
-652.734659998357));
#149270=CARTESIAN_POINT('Ctrl Pts',(-17.3590292079831,-4.93906964482095,
-654.228777645416));
#149271=CARTESIAN_POINT('Ctrl Pts',(-17.8167014103155,-3.33051870318735,
-655.722895292475));
#149272=CARTESIAN_POINT('Ctrl Pts',(-17.9710104137728,-1.66525935159368,
-657.217012939533));
#149273=CARTESIAN_POINT('Ctrl Pts',(-18.1253194172301,-1.10985572039171E-15,
-658.711130586592));
#149274=CARTESIAN_POINT('Ctrl Pts',(-17.9710104137728,1.66525935159367,
-660.205248233651));
#149275=CARTESIAN_POINT('Ctrl Pts',(-17.8167014103155,3.33051870318735,
-661.69936588071));
#149276=CARTESIAN_POINT('Ctrl Pts',(-17.3590292079831,4.93906964482096,
-663.193483527769));
#149277=CARTESIAN_POINT('Ctrl Pts',(-16.9013570056506,6.54762058645456,
-664.687601174827));
#149278=CARTESIAN_POINT('Ctrl Pts',(-16.1559070823762,8.04468584505497,
-666.181718821887));
#149279=CARTESIAN_POINT('Ctrl Pts',(-15.4104571591017,9.54175110365538,
-667.675836468945));
#149280=CARTESIAN_POINT('Ctrl Pts',(-14.4026149179538,10.8763499173728,
-669.169954116004));
#149281=CARTESIAN_POINT('Ctrl Pts',(-13.3947726768058,12.2109487310903,
-670.664071763063));
#149282=CARTESIAN_POINT('Ctrl Pts',(-12.1588589765331,13.3376329379985,
-672.158189410121));
#149283=CARTESIAN_POINT('Ctrl Pts',(-10.9229452762603,14.4643171449067,
-673.65230705718));
#149284=CARTESIAN_POINT('Ctrl Pts',(-9.50104767561052,15.3447188656481,
-675.146424704239));
#149285=CARTESIAN_POINT('Ctrl Pts',(-8.07915007496071,16.2251205863895,
-676.640542351298));
#149286=CARTESIAN_POINT('Ctrl Pts',(-6.51968959134574,16.8292587962898,
-678.134659998357));
#149287=CARTESIAN_POINT('Ctrl Pts',(-4.96022910773078,17.4333970061901,
-679.628777645416));
#149288=CARTESIAN_POINT('Ctrl Pts',(-3.31631129755346,17.7406985030951,
-681.122895292475));
#149289=CARTESIAN_POINT('Ctrl Pts',(-1.67239348737615,18.048,-682.617012939534));
#149290=CARTESIAN_POINT('Ctrl Pts',(-2.21024254310115E-15,18.048,-684.111130586592));
#149291=CARTESIAN_POINT('Ctrl Pts',(1.67239348737616,18.048,-685.605248233651));
#149292=CARTESIAN_POINT('Ctrl Pts',(3.31631129755346,17.7406985030951,-687.09936588071));
#149293=CARTESIAN_POINT('Ctrl Pts',(4.96022910773077,17.4333970061901,-688.593483527769));
#149294=CARTESIAN_POINT('Ctrl Pts',(6.51968959134575,16.8292587962898,-690.087601174827));
#149295=CARTESIAN_POINT('Ctrl Pts',(8.07915007496071,16.2251205863895,-691.581718821886));
#149296=CARTESIAN_POINT('Ctrl Pts',(9.50104767561053,15.3447188656481,-693.075836468945));
#149297=CARTESIAN_POINT('Ctrl Pts',(10.9229452762603,14.4643171449067,-694.569954116004));
#149298=CARTESIAN_POINT('Ctrl Pts',(12.1588589765331,13.3376329379985,-696.064071763063));
#149299=CARTESIAN_POINT('Ctrl Pts',(13.3947726768058,12.2109487310903,-697.558189410122));
#149300=CARTESIAN_POINT('Ctrl Pts',(14.4026149179538,10.8763499173728,-699.052307057181));
#149301=CARTESIAN_POINT('Ctrl Pts',(15.4104571591017,9.54175110365538,-700.546424704239));
#149302=CARTESIAN_POINT('Ctrl Pts',(16.1559070823762,8.04468584505496,-702.040542351298));
#149303=CARTESIAN_POINT('Ctrl Pts',(16.9013570056506,6.54762058645456,-703.534659998357));
#149304=CARTESIAN_POINT('Ctrl Pts',(17.3590292079831,4.93906964482096,-705.028777645416));
#149305=CARTESIAN_POINT('Ctrl Pts',(17.8167014103155,3.33051870318735,-706.522895292475));
#149306=CARTESIAN_POINT('Ctrl Pts',(17.9710104137728,1.66525935159367,-708.017012939533));
#149307=CARTESIAN_POINT('Ctrl Pts',(18.1253194172301,3.32956716117513E-15,
-709.511130586592));
#149308=CARTESIAN_POINT('Ctrl Pts',(17.9710104137728,-1.66525935159367,
-711.005248233651));
#149309=CARTESIAN_POINT('Ctrl Pts',(17.8167014103155,-3.33051870318736,
-712.49936588071));
#149310=CARTESIAN_POINT('Ctrl Pts',(17.3590292079831,-4.93906964482095,
-713.993483527769));
#149311=CARTESIAN_POINT('Ctrl Pts',(16.9013570056506,-6.54762058645456,
-715.487601174828));
#149312=CARTESIAN_POINT('Ctrl Pts',(16.1559070823762,-8.04468584505497,
-716.981718821886));
#149313=CARTESIAN_POINT('Ctrl Pts',(15.4104571591017,-9.54175110365538,
-718.475836468945));
#149314=CARTESIAN_POINT('Ctrl Pts',(14.4026149179538,-10.8763499173728,
-719.969954116004));
#149315=CARTESIAN_POINT('Ctrl Pts',(13.3947726768058,-12.2109487310903,
-721.464071763063));
#149316=CARTESIAN_POINT('Ctrl Pts',(12.1588589765331,-13.3376329379985,
-722.958189410122));
#149317=CARTESIAN_POINT('Ctrl Pts',(10.9229452762603,-14.4643171449067,
-724.452307057181));
#149318=CARTESIAN_POINT('Ctrl Pts',(9.50104767561053,-15.3447188656481,
-725.946424704239));
#149319=CARTESIAN_POINT('Ctrl Pts',(8.07915007496071,-16.2251205863895,
-727.440542351298));
#149320=CARTESIAN_POINT('Ctrl Pts',(6.51968959134574,-16.8292587962898,
-728.934659998357));
#149321=CARTESIAN_POINT('Ctrl Pts',(4.96022910773078,-17.4333970061901,
-730.428777645416));
#149322=CARTESIAN_POINT('Ctrl Pts',(3.31631129755346,-17.7406985030951,
-731.922895292474));
#149323=CARTESIAN_POINT('Ctrl Pts',(1.67239348737615,-18.048,-733.417012939533));
#149324=CARTESIAN_POINT('Ctrl Pts',(0.,-18.048,-734.911130586592));
#149325=CARTESIAN_POINT('Ctrl Pts',(-1.67239348737615,-18.048,-736.405248233651));
#149326=CARTESIAN_POINT('Ctrl Pts',(-3.31631129755346,-17.7406985030951,
-737.89936588071));
#149327=CARTESIAN_POINT('Ctrl Pts',(-4.96022910773077,-17.4333970061901,
-739.393483527769));
#149328=CARTESIAN_POINT('Ctrl Pts',(-6.51968959134574,-16.8292587962898,
-740.887601174828));
#149329=CARTESIAN_POINT('Ctrl Pts',(-8.07915007496071,-16.2251205863895,
-742.381718821887));
#149330=CARTESIAN_POINT('Ctrl Pts',(-9.50104767561052,-15.3447188656481,
-743.875836468945));
#149331=CARTESIAN_POINT('Ctrl Pts',(-10.9229452762603,-14.4643171449067,
-745.369954116004));
#149332=CARTESIAN_POINT('Ctrl Pts',(-12.1588589765331,-13.3376329379985,
-746.864071763063));
#149333=CARTESIAN_POINT('Ctrl Pts',(-13.3947726768058,-12.2109487310903,
-748.358189410122));
#149334=CARTESIAN_POINT('Ctrl Pts',(-14.4026149179538,-10.8763499173728,
-749.85230705718));
#149335=CARTESIAN_POINT('Ctrl Pts',(-15.4104571591017,-9.54175110365538,
-751.346424704239));
#149336=CARTESIAN_POINT('Ctrl Pts',(-16.1559070823762,-8.04468584505497,
-752.840542351298));
#149337=CARTESIAN_POINT('Ctrl Pts',(-16.9013570056506,-6.54762058645456,
-754.334659998357));
#149338=CARTESIAN_POINT('Ctrl Pts',(-17.3590292079831,-4.93906964482095,
-755.828777645416));
#149339=CARTESIAN_POINT('Ctrl Pts',(-17.8167014103155,-3.33051870318735,
-757.322895292475));
#149340=CARTESIAN_POINT('Ctrl Pts',(-17.9710104137728,-1.66525935159368,
-758.817012939534));
#149341=CARTESIAN_POINT('Ctrl Pts',(-18.1253194172301,-1.10985572039171E-15,
-760.311130586593));
#149342=CARTESIAN_POINT('Ctrl Pts',(-17.9710104137728,1.66525935159367,
-761.805248233651));
#149343=CARTESIAN_POINT('Ctrl Pts',(-17.8167014103155,3.33051870318735,
-763.29936588071));
#149344=CARTESIAN_POINT('Ctrl Pts',(-17.3590292079831,4.93906964482096,
-764.793483527769));
#149345=CARTESIAN_POINT('Ctrl Pts',(-16.9013570056506,6.54762058645456,
-766.287601174827));
#149346=CARTESIAN_POINT('Ctrl Pts',(-16.1559070823762,8.04468584505497,
-767.781718821886));
#149347=CARTESIAN_POINT('Ctrl Pts',(-15.4104571591017,9.54175110365538,
-769.275836468945));
#149348=CARTESIAN_POINT('Ctrl Pts',(-14.4026149179538,10.8763499173728,
-770.769954116004));
#149349=CARTESIAN_POINT('Ctrl Pts',(-13.3947726768058,12.2109487310903,
-772.264071763063));
#149350=CARTESIAN_POINT('Ctrl Pts',(-12.1588589765331,13.3376329379985,
-773.758189410122));
#149351=CARTESIAN_POINT('Ctrl Pts',(-10.9229452762603,14.4643171449067,
-775.252307057181));
#149352=CARTESIAN_POINT('Ctrl Pts',(-9.50104767561052,15.3447188656481,
-776.746424704239));
#149353=CARTESIAN_POINT('Ctrl Pts',(-8.07915007496071,16.2251205863895,
-778.240542351298));
#149354=CARTESIAN_POINT('Ctrl Pts',(-6.51968959134574,16.8292587962898,
-779.734659998357));
#149355=CARTESIAN_POINT('Ctrl Pts',(-4.96022910773078,17.4333970061901,
-781.228777645416));
#149356=CARTESIAN_POINT('Ctrl Pts',(-3.31631129755346,17.7406985030951,
-782.722895292475));
#149357=CARTESIAN_POINT('Ctrl Pts',(-1.67239348737615,18.048,-784.217012939534));
#149358=CARTESIAN_POINT('Ctrl Pts',(-2.21024254310115E-15,18.048,-785.711130586592));
#149359=CARTESIAN_POINT('Ctrl Pts',(1.67239348737616,18.048,-787.205248233651));
#149360=CARTESIAN_POINT('Ctrl Pts',(3.31631129755346,17.7406985030951,-788.69936588071));
#149361=CARTESIAN_POINT('Ctrl Pts',(4.96022910773077,17.4333970061901,-790.193483527769));
#149362=CARTESIAN_POINT('Ctrl Pts',(6.51968959134575,16.8292587962898,-791.687601174827));
#149363=CARTESIAN_POINT('Ctrl Pts',(8.07915007496071,16.2251205863895,-793.181718821886));
#149364=CARTESIAN_POINT('Ctrl Pts',(9.50104767561053,15.3447188656481,-794.675836468945));
#149365=CARTESIAN_POINT('Ctrl Pts',(10.9229452762603,14.4643171449067,-796.169954116004));
#149366=CARTESIAN_POINT('Ctrl Pts',(12.1588589765331,13.3376329379985,-797.664071763063));
#149367=CARTESIAN_POINT('Ctrl Pts',(13.3947726768058,12.2109487310903,-799.158189410122));
#149368=CARTESIAN_POINT('Ctrl Pts',(14.4026149179538,10.8763499173728,-800.65230705718));
#149369=CARTESIAN_POINT('Ctrl Pts',(15.4104571591017,9.54175110365538,-802.146424704239));
#149370=CARTESIAN_POINT('Ctrl Pts',(16.1559070823762,8.04468584505496,-803.640542351298));
#149371=CARTESIAN_POINT('Ctrl Pts',(16.9013570056506,6.54762058645456,-805.134659998357));
#149372=CARTESIAN_POINT('Ctrl Pts',(17.3590292079831,4.93906964482096,-806.628777645416));
#149373=CARTESIAN_POINT('Ctrl Pts',(17.8167014103155,3.33051870318735,-808.122895292474));
#149374=CARTESIAN_POINT('Ctrl Pts',(17.9710104137728,1.66525935159367,-809.617012939533));
#149375=CARTESIAN_POINT('Ctrl Pts',(18.1253194172301,3.32956716117513E-15,
-811.111130586592));
#149376=CARTESIAN_POINT('Ctrl Pts',(17.9710104137728,-1.66525935159367,
-812.605248233651));
#149377=CARTESIAN_POINT('Ctrl Pts',(17.8167014103155,-3.33051870318736,
-814.09936588071));
#149378=CARTESIAN_POINT('Ctrl Pts',(17.3590292079831,-4.93906964482095,
-815.593483527769));
#149379=CARTESIAN_POINT('Ctrl Pts',(16.9013570056506,-6.54762058645456,
-817.087601174828));
#149380=CARTESIAN_POINT('Ctrl Pts',(16.1559070823762,-8.04468584505497,
-818.581718821887));
#149381=CARTESIAN_POINT('Ctrl Pts',(15.4104571591017,-9.54175110365538,
-820.075836468945));
#149382=CARTESIAN_POINT('Ctrl Pts',(14.4026149179538,-10.8763499173728,
-821.569954116004));
#149383=CARTESIAN_POINT('Ctrl Pts',(13.3947726768058,-12.2109487310903,
-823.064071763063));
#149384=CARTESIAN_POINT('Ctrl Pts',(12.1588589765331,-13.3376329379985,
-824.558189410121));
#149385=CARTESIAN_POINT('Ctrl Pts',(10.9229452762603,-14.4643171449067,
-826.05230705718));
#149386=CARTESIAN_POINT('Ctrl Pts',(9.50104767561053,-15.3447188656481,
-827.546424704239));
#149387=CARTESIAN_POINT('Ctrl Pts',(8.07915007496071,-16.2251205863895,
-829.040542351298));
#149388=CARTESIAN_POINT('Ctrl Pts',(6.51968959134574,-16.8292587962898,
-830.534659998357));
#149389=CARTESIAN_POINT('Ctrl Pts',(4.96022910773078,-17.4333970061901,
-832.028777645416));
#149390=CARTESIAN_POINT('Ctrl Pts',(3.31631129755346,-17.7406985030951,
-833.522895292475));
#149391=CARTESIAN_POINT('Ctrl Pts',(1.67239348737615,-18.048,-835.017012939534));
#149392=CARTESIAN_POINT('Ctrl Pts',(0.,-18.048,-836.511130586592));
#149393=CARTESIAN_POINT('Ctrl Pts',(-1.67239348737615,-18.048,-838.005248233651));
#149394=CARTESIAN_POINT('Ctrl Pts',(-3.31631129755346,-17.7406985030951,
-839.49936588071));
#149395=CARTESIAN_POINT('Ctrl Pts',(-4.96022910773077,-17.4333970061901,
-840.993483527769));
#149396=CARTESIAN_POINT('Ctrl Pts',(-6.51968959134574,-16.8292587962898,
-842.487601174827));
#149397=CARTESIAN_POINT('Ctrl Pts',(-8.07915007496071,-16.2251205863895,
-843.981718821886));
#149398=CARTESIAN_POINT('Ctrl Pts',(-9.50104767561052,-15.3447188656481,
-845.475836468945));
#149399=CARTESIAN_POINT('Ctrl Pts',(-10.9229452762603,-14.4643171449067,
-846.969954116004));
#149400=CARTESIAN_POINT('Ctrl Pts',(-12.1588589765331,-13.3376329379985,
-848.464071763063));
#149401=CARTESIAN_POINT('Ctrl Pts',(-13.3947726768058,-12.2109487310903,
-849.958189410122));
#149402=CARTESIAN_POINT('Ctrl Pts',(-14.4026149179538,-10.8763499173728,
-851.45230705718));
#149403=CARTESIAN_POINT('Ctrl Pts',(-15.4104571591017,-9.54175110365538,
-852.946424704239));
#149404=CARTESIAN_POINT('Ctrl Pts',(-16.1559070823762,-8.04468584505497,
-854.440542351298));
#149405=CARTESIAN_POINT('Ctrl Pts',(-16.9013570056506,-6.54762058645456,
-855.934659998357));
#149406=CARTESIAN_POINT('Ctrl Pts',(-17.3590292079831,-4.93906964482095,
-857.428777645416));
#149407=CARTESIAN_POINT('Ctrl Pts',(-17.8167014103155,-3.33051870318735,
-858.922895292475));
#149408=CARTESIAN_POINT('Ctrl Pts',(-17.9710104137728,-1.66525935159368,
-860.417012939533));
#149409=CARTESIAN_POINT('Ctrl Pts',(-18.1253194172301,-1.10985572039171E-15,
-861.911130586592));
#149410=CARTESIAN_POINT('Ctrl Pts',(-17.9710104137728,1.66525935159367,
-863.405248233651));
#149411=CARTESIAN_POINT('Ctrl Pts',(-17.8167014103155,3.33051870318735,
-864.89936588071));
#149412=CARTESIAN_POINT('Ctrl Pts',(-17.3590292079831,4.93906964482096,
-866.393483527768));
#149413=CARTESIAN_POINT('Ctrl Pts',(-16.9013570056506,6.54762058645456,
-867.887601174827));
#149414=CARTESIAN_POINT('Ctrl Pts',(-16.1559070823762,8.04468584505497,
-869.381718821886));
#149415=CARTESIAN_POINT('Ctrl Pts',(-15.4104571591017,9.54175110365538,
-870.875836468945));
#149416=CARTESIAN_POINT('Ctrl Pts',(-14.4026149179538,10.8763499173728,
-872.369954116004));
#149417=CARTESIAN_POINT('Ctrl Pts',(-13.3947726768058,12.2109487310903,
-873.864071763063));
#149418=CARTESIAN_POINT('Ctrl Pts',(-12.1588589765331,13.3376329379985,
-875.358189410122));
#149419=CARTESIAN_POINT('Ctrl Pts',(-10.9229452762603,14.4643171449067,
-876.85230705718));
#149420=CARTESIAN_POINT('Ctrl Pts',(-9.50104767561052,15.3447188656481,
-878.346424704239));
#149421=CARTESIAN_POINT('Ctrl Pts',(-8.07915007496071,16.2251205863895,
-879.840542351298));
#149422=CARTESIAN_POINT('Ctrl Pts',(-6.51968959134574,16.8292587962898,
-881.334659998357));
#149423=CARTESIAN_POINT('Ctrl Pts',(-4.96022910773078,17.4333970061901,
-882.828777645416));
#149424=CARTESIAN_POINT('Ctrl Pts',(-3.31631129755346,17.7406985030951,
-884.322895292474));
#149425=CARTESIAN_POINT('Ctrl Pts',(-1.67239348737615,18.048,-885.817012939534));
#149426=CARTESIAN_POINT('Ctrl Pts',(-2.21024254310115E-15,18.048,-887.311130586592));
#149427=CARTESIAN_POINT('Ctrl Pts',(1.67239348737616,18.048,-888.805248233651));
#149428=CARTESIAN_POINT('Ctrl Pts',(3.31631129755346,17.7406985030951,-890.29936588071));
#149429=CARTESIAN_POINT('Ctrl Pts',(4.96022910773077,17.4333970061901,-891.793483527769));
#149430=CARTESIAN_POINT('Ctrl Pts',(6.51968959134575,16.8292587962898,-893.287601174828));
#149431=CARTESIAN_POINT('Ctrl Pts',(8.07915007496071,16.2251205863895,-894.781718821887));
#149432=CARTESIAN_POINT('Ctrl Pts',(9.50104767561053,15.3447188656481,-896.275836468945));
#149433=CARTESIAN_POINT('Ctrl Pts',(10.9229452762603,14.4643171449067,-897.769954116004));
#149434=CARTESIAN_POINT('Ctrl Pts',(12.1588589765331,13.3376329379985,-899.264071763063));
#149435=CARTESIAN_POINT('Ctrl Pts',(13.3947726768058,12.2109487310903,-900.758189410122));
#149436=CARTESIAN_POINT('Ctrl Pts',(14.4026149179538,10.8763499173728,-902.25230705718));
#149437=CARTESIAN_POINT('Ctrl Pts',(15.4104571591017,9.54175110365538,-903.746424704239));
#149438=CARTESIAN_POINT('Ctrl Pts',(16.1559070823762,8.04468584505496,-905.240542351298));
#149439=CARTESIAN_POINT('Ctrl Pts',(16.9013570056506,6.54762058645456,-906.734659998357));
#149440=CARTESIAN_POINT('Ctrl Pts',(17.3590292079831,4.93906964482096,-908.228777645416));
#149441=CARTESIAN_POINT('Ctrl Pts',(17.8167014103155,3.33051870318735,-909.722895292475));
#149442=CARTESIAN_POINT('Ctrl Pts',(17.9710104137728,1.66525935159367,-911.217012939533));
#149443=CARTESIAN_POINT('Ctrl Pts',(18.1253194172301,3.32956716117513E-15,
-912.711130586592));
#149444=CARTESIAN_POINT('Ctrl Pts',(17.9710104137728,-1.66525935159367,
-914.205248233651));
#149445=CARTESIAN_POINT('Ctrl Pts',(17.8167014103155,-3.33051870318736,
-915.69936588071));
#149446=CARTESIAN_POINT('Ctrl Pts',(17.3590292079831,-4.93906964482095,
-917.193483527769));
#149447=CARTESIAN_POINT('Ctrl Pts',(16.9013570056506,-6.54762058645456,
-918.687601174827));
#149448=CARTESIAN_POINT('Ctrl Pts',(16.1559070823762,-8.04468584505497,
-920.181718821887));
#149449=CARTESIAN_POINT('Ctrl Pts',(15.4104571591017,-9.54175110365538,
-921.675836468945));
#149450=CARTESIAN_POINT('Ctrl Pts',(14.4026149179538,-10.8763499173728,
-923.169954116004));
#149451=CARTESIAN_POINT('Ctrl Pts',(13.3947726768058,-12.2109487310903,
-924.664071763063));
#149452=CARTESIAN_POINT('Ctrl Pts',(12.1588589765331,-13.3376329379985,
-926.158189410122));
#149453=CARTESIAN_POINT('Ctrl Pts',(10.9229452762603,-14.4643171449067,
-927.65230705718));
#149454=CARTESIAN_POINT('Ctrl Pts',(9.50104767561053,-15.3447188656481,
-929.146424704239));
#149455=CARTESIAN_POINT('Ctrl Pts',(8.07915007496071,-16.2251205863895,
-930.640542351298));
#149456=CARTESIAN_POINT('Ctrl Pts',(6.51968959134574,-16.8292587962898,
-932.134659998357));
#149457=CARTESIAN_POINT('Ctrl Pts',(4.96022910773078,-17.4333970061901,
-933.628777645416));
#149458=CARTESIAN_POINT('Ctrl Pts',(3.31631129755346,-17.7406985030951,
-935.122895292475));
#149459=CARTESIAN_POINT('Ctrl Pts',(1.67239348737615,-18.048,-936.617012939534));
#149460=CARTESIAN_POINT('Ctrl Pts',(0.,-18.048,-938.111130586592));
#149461=CARTESIAN_POINT('Ctrl Pts',(-1.67239348737615,-18.048,-939.605248233651));
#149462=CARTESIAN_POINT('Ctrl Pts',(-3.31631129755346,-17.7406985030951,
-941.09936588071));
#149463=CARTESIAN_POINT('Ctrl Pts',(-4.96022910773077,-17.4333970061901,
-942.593483527769));
#149464=CARTESIAN_POINT('Ctrl Pts',(-6.51968959134574,-16.8292587962898,
-944.087601174827));
#149465=CARTESIAN_POINT('Ctrl Pts',(-8.07915007496071,-16.2251205863895,
-945.581718821886));
#149466=CARTESIAN_POINT('Ctrl Pts',(-9.50104767561052,-15.3447188656481,
-947.075836468945));
#149467=CARTESIAN_POINT('Ctrl Pts',(-10.9229452762603,-14.4643171449067,
-948.569954116004));
#149468=CARTESIAN_POINT('Ctrl Pts',(-12.1588589765331,-13.3376329379985,
-950.064071763063));
#149469=CARTESIAN_POINT('Ctrl Pts',(-13.3947726768058,-12.2109487310903,
-951.558189410122));
#149470=CARTESIAN_POINT('Ctrl Pts',(-14.4026149179538,-10.8763499173728,
-953.052307057181));
#149471=CARTESIAN_POINT('Ctrl Pts',(-15.4104571591017,-9.54175110365538,
-954.54642470424));
#149472=CARTESIAN_POINT('Ctrl Pts',(-16.1559070823762,-8.04468584505497,
-956.040542351298));
#149473=CARTESIAN_POINT('Ctrl Pts',(-16.9013570056506,-6.54762058645456,
-957.534659998357));
#149474=CARTESIAN_POINT('Ctrl Pts',(-17.3590292079831,-4.93906964482095,
-959.028777645416));
#149475=CARTESIAN_POINT('Ctrl Pts',(-17.8167014103155,-3.33051870318735,
-960.522895292475));
#149476=CARTESIAN_POINT('Ctrl Pts',(-17.9710104137728,-1.66525935159368,
-962.017012939533));
#149477=CARTESIAN_POINT('Ctrl Pts',(-18.1253194172301,-1.10985572039171E-15,
-963.511130586592));
#149478=CARTESIAN_POINT('Ctrl Pts',(-17.9710104137728,1.66525935159367,
-965.005248233651));
#149479=CARTESIAN_POINT('Ctrl Pts',(-17.8167014103155,3.33051870318735,
-966.49936588071));
#149480=CARTESIAN_POINT('Ctrl Pts',(-17.3590292079831,4.93906964482096,
-967.993483527769));
#149481=CARTESIAN_POINT('Ctrl Pts',(-16.9013570056506,6.54762058645456,
-969.487601174828));
#149482=CARTESIAN_POINT('Ctrl Pts',(-16.1559070823762,8.04468584505497,
-970.981718821886));
#149483=CARTESIAN_POINT('Ctrl Pts',(-15.4104571591017,9.54175110365538,
-972.475836468945));
#149484=CARTESIAN_POINT('Ctrl Pts',(-14.4026149179538,10.8763499173728,
-973.969954116004));
#149485=CARTESIAN_POINT('Ctrl Pts',(-13.3947726768058,12.2109487310903,
-975.464071763063));
#149486=CARTESIAN_POINT('Ctrl Pts',(-12.1588589765331,13.3376329379985,
-976.958189410122));
#149487=CARTESIAN_POINT('Ctrl Pts',(-10.9229452762603,14.4643171449067,
-978.452307057181));
#149488=CARTESIAN_POINT('Ctrl Pts',(-9.50104767561052,15.3447188656481,
-979.946424704239));
#149489=CARTESIAN_POINT('Ctrl Pts',(-8.07915007496071,16.2251205863895,
-981.440542351298));
#149490=CARTESIAN_POINT('Ctrl Pts',(-6.51968959134574,16.8292587962898,
-982.934659998357));
#149491=CARTESIAN_POINT('Ctrl Pts',(-4.96022910773078,17.4333970061901,
-984.428777645416));
#149492=CARTESIAN_POINT('Ctrl Pts',(-3.31631129755346,17.7406985030951,
-985.922895292474));
#149493=CARTESIAN_POINT('Ctrl Pts',(-1.67239348737615,18.048,-987.417012939533));
#149494=CARTESIAN_POINT('Ctrl Pts',(-2.21024254310115E-15,18.048,-988.911130586592));
#149495=CARTESIAN_POINT('Ctrl Pts',(1.67239348737616,18.048,-990.405248233651));
#149496=CARTESIAN_POINT('Ctrl Pts',(3.31631129755346,17.7406985030951,-991.89936588071));
#149497=CARTESIAN_POINT('Ctrl Pts',(4.96022910773077,17.4333970061901,-993.393483527769));
#149498=CARTESIAN_POINT('Ctrl Pts',(6.51968959134575,16.8292587962898,-994.887601174828));
#149499=CARTESIAN_POINT('Ctrl Pts',(8.07915007496071,16.2251205863895,-996.381718821887));
#149500=CARTESIAN_POINT('Ctrl Pts',(9.50104767561053,15.3447188656481,-997.875836468945));
#149501=CARTESIAN_POINT('Ctrl Pts',(10.9229452762603,14.4643171449067,-999.369954116004));
#149502=CARTESIAN_POINT('Ctrl Pts',(12.1588589765331,13.3376329379985,-1000.86407176306));
#149503=CARTESIAN_POINT('Ctrl Pts',(13.3947726768058,12.2109487310903,-1002.35818941012));
#149504=CARTESIAN_POINT('Ctrl Pts',(14.4026149179538,10.8763499173728,-1003.85230705718));
#149505=CARTESIAN_POINT('Ctrl Pts',(15.4104571591017,9.54175110365538,-1005.34642470424));
#149506=CARTESIAN_POINT('Ctrl Pts',(16.1559070823762,8.04468584505496,-1006.8405423513));
#149507=CARTESIAN_POINT('Ctrl Pts',(16.9013570056506,6.54762058645456,-1008.33465999836));
#149508=CARTESIAN_POINT('Ctrl Pts',(17.3590292079831,4.93906964482096,-1009.82877764542));
#149509=CARTESIAN_POINT('Ctrl Pts',(17.8167014103155,3.33051870318735,-1011.32289529247));
#149510=CARTESIAN_POINT('Ctrl Pts',(17.9710104137728,1.66525935159367,-1012.81701293953));
#149511=CARTESIAN_POINT('Ctrl Pts',(18.1253194172301,3.32956716117513E-15,
-1014.31113058659));
#149512=CARTESIAN_POINT('Ctrl Pts',(17.9710104137728,-1.66525935159367,
-1015.80524823365));
#149513=CARTESIAN_POINT('Ctrl Pts',(17.8167014103155,-3.33051870318736,
-1017.29936588071));
#149514=CARTESIAN_POINT('Ctrl Pts',(17.3590292079831,-4.93906964482095,
-1018.79348352777));
#149515=CARTESIAN_POINT('Ctrl Pts',(16.9013570056506,-6.54762058645456,
-1020.28760117483));
#149516=CARTESIAN_POINT('Ctrl Pts',(16.1559070823762,-8.04468584505497,
-1021.78171882189));
#149517=CARTESIAN_POINT('Ctrl Pts',(15.4104571591017,-9.54175110365538,
-1023.27583646895));
#149518=CARTESIAN_POINT('Ctrl Pts',(14.4026149179538,-10.8763499173728,
-1024.769954116));
#149519=CARTESIAN_POINT('Ctrl Pts',(13.3947726768058,-12.2109487310903,
-1026.26407176306));
#149520=CARTESIAN_POINT('Ctrl Pts',(12.1588589765331,-13.3376329379985,
-1027.75818941012));
#149521=CARTESIAN_POINT('Ctrl Pts',(10.9229452762603,-14.4643171449067,
-1029.25230705718));
#149522=CARTESIAN_POINT('Ctrl Pts',(9.50104767561053,-15.3447188656481,
-1030.74642470424));
#149523=CARTESIAN_POINT('Ctrl Pts',(8.07915007496071,-16.2251205863895,
-1032.2405423513));
#149524=CARTESIAN_POINT('Ctrl Pts',(6.51968959134574,-16.8292587962898,
-1033.73465999836));
#149525=CARTESIAN_POINT('Ctrl Pts',(4.96022910773078,-17.4333970061901,
-1035.22877764542));
#149526=CARTESIAN_POINT('Ctrl Pts',(3.31631129755346,-17.7406985030951,
-1036.72289529247));
#149527=CARTESIAN_POINT('Ctrl Pts',(1.67239348737615,-18.048,-1038.21701293953));
#149528=CARTESIAN_POINT('Ctrl Pts',(0.,-18.048,-1039.71113058659));
#149529=CARTESIAN_POINT('Ctrl Pts',(-1.67239348737615,-18.048,-1041.20524823365));
#149530=CARTESIAN_POINT('Ctrl Pts',(-3.31631129755346,-17.7406985030951,
-1042.69936588071));
#149531=CARTESIAN_POINT('Ctrl Pts',(-4.96022910773077,-17.4333970061901,
-1044.19348352777));
#149532=CARTESIAN_POINT('Ctrl Pts',(-6.51968959134574,-16.8292587962898,
-1045.68760117483));
#149533=CARTESIAN_POINT('Ctrl Pts',(-8.07915007496071,-16.2251205863895,
-1047.18171882189));
#149534=CARTESIAN_POINT('Ctrl Pts',(-9.50104767561052,-15.3447188656481,
-1048.67583646894));
#149535=CARTESIAN_POINT('Ctrl Pts',(-10.9229452762603,-14.4643171449067,
-1050.169954116));
#149536=CARTESIAN_POINT('Ctrl Pts',(-12.1588589765331,-13.3376329379985,
-1051.66407176306));
#149537=CARTESIAN_POINT('Ctrl Pts',(-13.3947726768058,-12.2109487310903,
-1053.15818941012));
#149538=CARTESIAN_POINT('Ctrl Pts',(-14.4026149179538,-10.8763499173728,
-1054.65230705718));
#149539=CARTESIAN_POINT('Ctrl Pts',(-15.4104571591017,-9.54175110365538,
-1056.14642470424));
#149540=CARTESIAN_POINT('Ctrl Pts',(-16.1559070823762,-8.04468584505497,
-1057.6405423513));
#149541=CARTESIAN_POINT('Ctrl Pts',(-16.9013570056506,-6.54762058645456,
-1059.13465999836));
#149542=CARTESIAN_POINT('Ctrl Pts',(-17.3590292079831,-4.93906964482095,
-1060.62877764542));
#149543=CARTESIAN_POINT('Ctrl Pts',(-17.8167014103155,-3.33051870318735,
-1062.12289529247));
#149544=CARTESIAN_POINT('Ctrl Pts',(-17.9710104137728,-1.66525935159368,
-1063.61701293953));
#149545=CARTESIAN_POINT('Ctrl Pts',(-18.1253194172301,-1.10985572039171E-15,
-1065.11113058659));
#149546=CARTESIAN_POINT('Ctrl Pts',(-17.9710104137728,1.66525935159367,
-1066.60524823365));
#149547=CARTESIAN_POINT('Ctrl Pts',(-17.8167014103155,3.33051870318735,
-1068.09936588071));
#149548=CARTESIAN_POINT('Ctrl Pts',(-17.3590292079831,4.93906964482096,
-1069.59348352777));
#149549=CARTESIAN_POINT('Ctrl Pts',(-16.9013570056506,6.54762058645456,
-1071.08760117483));
#149550=CARTESIAN_POINT('Ctrl Pts',(-16.1559070823762,8.04468584505497,
-1072.58171882189));
#149551=CARTESIAN_POINT('Ctrl Pts',(-15.4104571591017,9.54175110365538,
-1074.07583646895));
#149552=CARTESIAN_POINT('Ctrl Pts',(-14.4026149179538,10.8763499173728,
-1075.569954116));
#149553=CARTESIAN_POINT('Ctrl Pts',(-13.3947726768058,12.2109487310903,
-1077.06407176306));
#149554=CARTESIAN_POINT('Ctrl Pts',(-12.1588589765331,13.3376329379985,
-1078.55818941012));
#149555=CARTESIAN_POINT('Ctrl Pts',(-10.9229452762603,14.4643171449067,
-1080.05230705718));
#149556=CARTESIAN_POINT('Ctrl Pts',(-9.50104767561052,15.3447188656481,
-1081.54642470424));
#149557=CARTESIAN_POINT('Ctrl Pts',(-8.07915007496071,16.2251205863895,
-1083.0405423513));
#149558=CARTESIAN_POINT('Ctrl Pts',(-6.51968959134574,16.8292587962898,
-1084.53465999836));
#149559=CARTESIAN_POINT('Ctrl Pts',(-4.96022910773078,17.4333970061901,
-1086.02877764542));
#149560=CARTESIAN_POINT('Ctrl Pts',(-3.31631129755346,17.7406985030951,
-1087.52289529247));
#149561=CARTESIAN_POINT('Ctrl Pts',(-1.67239348737615,18.048,-1089.01701293953));
#149562=CARTESIAN_POINT('Ctrl Pts',(-2.21024254310115E-15,18.048,-1090.51113058659));
#149563=CARTESIAN_POINT('Ctrl Pts',(1.67239348737616,18.048,-1092.00524823365));
#149564=CARTESIAN_POINT('Ctrl Pts',(3.31631129755346,17.7406985030951,-1093.49936588071));
#149565=CARTESIAN_POINT('Ctrl Pts',(4.96022910773077,17.4333970061901,-1094.99348352777));
#149566=CARTESIAN_POINT('Ctrl Pts',(6.51968959134575,16.8292587962898,-1096.48760117483));
#149567=CARTESIAN_POINT('Ctrl Pts',(8.07915007496071,16.2251205863895,-1097.98171882189));
#149568=CARTESIAN_POINT('Ctrl Pts',(9.50104767561053,15.3447188656481,-1099.47583646895));
#149569=CARTESIAN_POINT('Ctrl Pts',(10.9229452762603,14.4643171449067,-1100.969954116));
#149570=CARTESIAN_POINT('Ctrl Pts',(12.1588589765331,13.3376329379985,-1102.46407176306));
#149571=CARTESIAN_POINT('Ctrl Pts',(13.3947726768058,12.2109487310903,-1103.95818941012));
#149572=CARTESIAN_POINT('Ctrl Pts',(14.4026149179538,10.8763499173728,-1105.45230705718));
#149573=CARTESIAN_POINT('Ctrl Pts',(15.4104571591017,9.54175110365538,-1106.94642470424));
#149574=CARTESIAN_POINT('Ctrl Pts',(16.1559070823762,8.04468584505496,-1108.4405423513));
#149575=CARTESIAN_POINT('Ctrl Pts',(16.9013570056506,6.54762058645456,-1109.93465999836));
#149576=CARTESIAN_POINT('Ctrl Pts',(17.3590292079831,4.93906964482096,-1111.42877764542));
#149577=CARTESIAN_POINT('Ctrl Pts',(17.8167014103155,3.33051870318735,-1112.92289529247));
#149578=CARTESIAN_POINT('Ctrl Pts',(17.9710104137728,1.66525935159367,-1114.41701293953));
#149579=CARTESIAN_POINT('Ctrl Pts',(18.1253194172301,3.32956716117513E-15,
-1115.91113058659));
#149580=CARTESIAN_POINT('Ctrl Pts',(17.9710104137728,-1.66525935159367,
-1117.40524823365));
#149581=CARTESIAN_POINT('Ctrl Pts',(17.8167014103155,-3.33051870318736,
-1118.89936588071));
#149582=CARTESIAN_POINT('Ctrl Pts',(17.3590292079831,-4.93906964482095,
-1120.39348352777));
#149583=CARTESIAN_POINT('Ctrl Pts',(16.9013570056506,-6.54762058645456,
-1121.88760117483));
#149584=CARTESIAN_POINT('Ctrl Pts',(16.1559070823762,-8.04468584505497,
-1123.38171882189));
#149585=CARTESIAN_POINT('Ctrl Pts',(15.4104571591017,-9.54175110365538,
-1124.87583646895));
#149586=CARTESIAN_POINT('Ctrl Pts',(14.4026149179538,-10.8763499173728,
-1126.369954116));
#149587=CARTESIAN_POINT('Ctrl Pts',(13.3947726768058,-12.2109487310903,
-1127.86407176306));
#149588=CARTESIAN_POINT('Ctrl Pts',(12.1588589765331,-13.3376329379985,
-1129.35818941012));
#149589=CARTESIAN_POINT('Ctrl Pts',(10.9229452762603,-14.4643171449067,
-1130.85230705718));
#149590=CARTESIAN_POINT('Ctrl Pts',(9.50104767561053,-15.3447188656481,
-1132.34642470424));
#149591=CARTESIAN_POINT('Ctrl Pts',(8.07915007496071,-16.2251205863895,
-1133.8405423513));
#149592=CARTESIAN_POINT('Ctrl Pts',(6.51968959134574,-16.8292587962898,
-1135.33465999836));
#149593=CARTESIAN_POINT('Ctrl Pts',(4.96022910773078,-17.4333970061901,
-1136.82877764542));
#149594=CARTESIAN_POINT('Ctrl Pts',(3.31631129755346,-17.7406985030951,
-1138.32289529247));
#149595=CARTESIAN_POINT('Ctrl Pts',(1.67239348737615,-18.048,-1139.81701293953));
#149596=CARTESIAN_POINT('Ctrl Pts',(0.,-18.048,-1141.31113058659));
#149597=CARTESIAN_POINT('Ctrl Pts',(-1.67239348737615,-18.048,-1142.80524823365));
#149598=CARTESIAN_POINT('Ctrl Pts',(-3.31631129755346,-17.7406985030951,
-1144.29936588071));
#149599=CARTESIAN_POINT('Ctrl Pts',(-4.96022910773077,-17.4333970061901,
-1145.79348352777));
#149600=CARTESIAN_POINT('Ctrl Pts',(-6.51968959134574,-16.8292587962898,
-1147.28760117483));
#149601=CARTESIAN_POINT('Ctrl Pts',(-8.07915007496071,-16.2251205863895,
-1148.78171882189));
#149602=CARTESIAN_POINT('Ctrl Pts',(-9.50104767561052,-15.3447188656481,
-1150.27583646895));
#149603=CARTESIAN_POINT('Ctrl Pts',(-10.9229452762603,-14.4643171449067,
-1151.769954116));
#149604=CARTESIAN_POINT('Ctrl Pts',(-12.1588589765331,-13.3376329379985,
-1153.26407176306));
#149605=CARTESIAN_POINT('Ctrl Pts',(-13.3947726768058,-12.2109487310903,
-1154.75818941012));
#149606=CARTESIAN_POINT('Ctrl Pts',(-14.4026149179538,-10.8763499173728,
-1156.25230705718));
#149607=CARTESIAN_POINT('Ctrl Pts',(-15.4104571591017,-9.54175110365538,
-1157.74642470424));
#149608=CARTESIAN_POINT('Ctrl Pts',(-16.1559070823762,-8.04468584505497,
-1159.2405423513));
#149609=CARTESIAN_POINT('Ctrl Pts',(-16.9013570056506,-6.54762058645456,
-1160.73465999836));
#149610=CARTESIAN_POINT('Ctrl Pts',(-17.3590292079831,-4.93906964482095,
-1162.22877764542));
#149611=CARTESIAN_POINT('Ctrl Pts',(-17.8167014103155,-3.33051870318735,
-1163.72289529247));
#149612=CARTESIAN_POINT('Ctrl Pts',(-17.9710104137728,-1.66525935159368,
-1165.21701293953));
#149613=CARTESIAN_POINT('Ctrl Pts',(-18.1253194172301,-1.10985572039171E-15,
-1166.71113058659));
#149614=CARTESIAN_POINT('Ctrl Pts',(-17.9710104137728,1.66525935159367,
-1168.20524823365));
#149615=CARTESIAN_POINT('Ctrl Pts',(-17.8167014103155,3.33051870318735,
-1169.69936588071));
#149616=CARTESIAN_POINT('Ctrl Pts',(-17.3590292079831,4.93906964482096,
-1171.19348352777));
#149617=CARTESIAN_POINT('Ctrl Pts',(-16.9013570056506,6.54762058645456,
-1172.68760117483));
#149618=CARTESIAN_POINT('Ctrl Pts',(-16.1559070823762,8.04468584505497,
-1174.18171882189));
#149619=CARTESIAN_POINT('Ctrl Pts',(-15.4104571591017,9.54175110365538,
-1175.67583646895));
#149620=CARTESIAN_POINT('Ctrl Pts',(-14.4026149179538,10.8763499173728,
-1177.169954116));
#149621=CARTESIAN_POINT('Ctrl Pts',(-13.3947726768058,12.2109487310903,
-1178.66407176306));
#149622=CARTESIAN_POINT('Ctrl Pts',(-12.1588589765331,13.3376329379985,
-1180.15818941012));
#149623=CARTESIAN_POINT('Ctrl Pts',(-10.9229452762603,14.4643171449067,
-1181.65230705718));
#149624=CARTESIAN_POINT('Ctrl Pts',(-9.50104767561052,15.3447188656481,
-1183.14642470424));
#149625=CARTESIAN_POINT('Ctrl Pts',(-8.07915007496071,16.2251205863895,
-1184.6405423513));
#149626=CARTESIAN_POINT('Ctrl Pts',(-6.51968959134574,16.8292587962898,
-1186.13465999836));
#149627=CARTESIAN_POINT('Ctrl Pts',(-4.96022910773078,17.4333970061901,
-1187.62877764542));
#149628=CARTESIAN_POINT('Ctrl Pts',(-3.31631129755346,17.7406985030951,
-1189.12289529247));
#149629=CARTESIAN_POINT('Ctrl Pts',(-1.67239348737615,18.048,-1190.61701293953));
#149630=CARTESIAN_POINT('Ctrl Pts',(-2.21024254310115E-15,18.048,-1192.11113058659));
#149631=CARTESIAN_POINT('Ctrl Pts',(1.67239348737616,18.048,-1193.60524823365));
#149632=CARTESIAN_POINT('Ctrl Pts',(3.31631129755346,17.7406985030951,-1195.09936588071));
#149633=CARTESIAN_POINT('Ctrl Pts',(4.96022910773077,17.4333970061901,-1196.59348352777));
#149634=CARTESIAN_POINT('Ctrl Pts',(6.51968959134575,16.8292587962898,-1198.08760117483));
#149635=CARTESIAN_POINT('Ctrl Pts',(8.07915007496071,16.2251205863895,-1199.58171882189));
#149636=CARTESIAN_POINT('Ctrl Pts',(9.50104767561053,15.3447188656481,-1201.07583646894));
#149637=CARTESIAN_POINT('Ctrl Pts',(10.9229452762603,14.4643171449067,-1202.569954116));
#149638=CARTESIAN_POINT('Ctrl Pts',(12.1588589765331,13.3376329379985,-1204.06407176306));
#149639=CARTESIAN_POINT('Ctrl Pts',(13.3947726768058,12.2109487310903,-1205.55818941012));
#149640=CARTESIAN_POINT('Ctrl Pts',(14.4026149179538,10.8763499173728,-1207.05230705718));
#149641=CARTESIAN_POINT('Ctrl Pts',(15.4104571591017,9.54175110365538,-1208.54642470424));
#149642=CARTESIAN_POINT('Ctrl Pts',(16.1559070823762,8.04468584505496,-1210.0405423513));
#149643=CARTESIAN_POINT('Ctrl Pts',(16.9013570056506,6.54762058645456,-1211.53465999836));
#149644=CARTESIAN_POINT('Ctrl Pts',(17.3590292079831,4.93906964482096,-1213.02877764542));
#149645=CARTESIAN_POINT('Ctrl Pts',(17.8167014103155,3.33051870318735,-1214.52289529247));
#149646=CARTESIAN_POINT('Ctrl Pts',(17.9710104137728,1.66525935159367,-1216.01701293953));
#149647=CARTESIAN_POINT('Ctrl Pts',(18.1253194172301,3.32956716117513E-15,
-1217.51113058659));
#149648=CARTESIAN_POINT('Ctrl Pts',(17.9710104137728,-1.66525935159367,
-1219.00524823365));
#149649=CARTESIAN_POINT('Ctrl Pts',(17.8167014103155,-3.33051870318736,
-1220.49936588071));
#149650=CARTESIAN_POINT('Ctrl Pts',(17.3590292079831,-4.93906964482095,
-1221.99348352777));
#149651=CARTESIAN_POINT('Ctrl Pts',(16.9013570056506,-6.54762058645456,
-1223.48760117483));
#149652=CARTESIAN_POINT('Ctrl Pts',(16.1559070823762,-8.04468584505497,
-1224.98171882189));
#149653=CARTESIAN_POINT('Ctrl Pts',(15.4104571591017,-9.54175110365538,
-1226.47583646895));
#149654=CARTESIAN_POINT('Ctrl Pts',(14.4026149179538,-10.8763499173728,
-1227.969954116));
#149655=CARTESIAN_POINT('Ctrl Pts',(13.3947726768058,-12.2109487310903,
-1229.46407176306));
#149656=CARTESIAN_POINT('Ctrl Pts',(12.1588589765331,-13.3376329379985,
-1230.95818941012));
#149657=CARTESIAN_POINT('Ctrl Pts',(10.9229452762603,-14.4643171449067,
-1232.45230705718));
#149658=CARTESIAN_POINT('Ctrl Pts',(9.50104767561053,-15.3447188656481,
-1233.94642470424));
#149659=CARTESIAN_POINT('Ctrl Pts',(8.07915007496071,-16.2251205863895,
-1235.4405423513));
#149660=CARTESIAN_POINT('Ctrl Pts',(6.51968959134574,-16.8292587962898,
-1236.93465999836));
#149661=CARTESIAN_POINT('Ctrl Pts',(4.96022910773078,-17.4333970061901,
-1238.42877764542));
#149662=CARTESIAN_POINT('Ctrl Pts',(3.31631129755346,-17.7406985030951,
-1239.92289529247));
#149663=CARTESIAN_POINT('Ctrl Pts',(1.67239348737615,-18.048,-1241.41701293953));
#149664=CARTESIAN_POINT('Ctrl Pts',(0.,-18.048,-1242.91113058659));
#149665=CARTESIAN_POINT('Ctrl Pts',(-1.67239348737615,-18.048,-1244.40524823365));
#149666=CARTESIAN_POINT('Ctrl Pts',(-3.31631129755346,-17.7406985030951,
-1245.89936588071));
#149667=CARTESIAN_POINT('Ctrl Pts',(-4.96022910773077,-17.4333970061901,
-1247.39348352777));
#149668=CARTESIAN_POINT('Ctrl Pts',(-6.51968959134574,-16.8292587962898,
-1248.88760117483));
#149669=CARTESIAN_POINT('Ctrl Pts',(-8.07915007496071,-16.2251205863895,
-1250.38171882189));
#149670=CARTESIAN_POINT('Ctrl Pts',(-9.50104767561052,-15.3447188656481,
-1251.87583646895));
#149671=CARTESIAN_POINT('Ctrl Pts',(-10.9229452762603,-14.4643171449067,
-1253.369954116));
#149672=CARTESIAN_POINT('Ctrl Pts',(-12.1588589765331,-13.3376329379985,
-1254.86407176306));
#149673=CARTESIAN_POINT('Ctrl Pts',(-13.3947726768058,-12.2109487310903,
-1256.35818941012));
#149674=CARTESIAN_POINT('Ctrl Pts',(-14.4026149179538,-10.8763499173728,
-1257.85230705718));
#149675=CARTESIAN_POINT('Ctrl Pts',(-15.4104571591017,-9.54175110365538,
-1259.34642470424));
#149676=CARTESIAN_POINT('Ctrl Pts',(-16.1559070823762,-8.04468584505497,
-1260.8405423513));
#149677=CARTESIAN_POINT('Ctrl Pts',(-16.9013570056506,-6.54762058645456,
-1262.33465999836));
#149678=CARTESIAN_POINT('Ctrl Pts',(-17.3590292079831,-4.93906964482095,
-1263.82877764542));
#149679=CARTESIAN_POINT('Ctrl Pts',(-17.8167014103155,-3.33051870318735,
-1265.32289529247));
#149680=CARTESIAN_POINT('Ctrl Pts',(-17.9710104137728,-1.66525935159368,
-1266.81701293953));
#149681=CARTESIAN_POINT('Ctrl Pts',(-18.1253194172301,-1.10985572039171E-15,
-1268.31113058659));
#149682=CARTESIAN_POINT('Ctrl Pts',(-17.9710104137728,1.66525935159367,
-1269.80524823365));
#149683=CARTESIAN_POINT('Ctrl Pts',(-17.8167014103155,3.33051870318735,
-1271.29936588071));
#149684=CARTESIAN_POINT('Ctrl Pts',(-17.3590292079831,4.93906964482096,
-1272.79348352777));
#149685=CARTESIAN_POINT('Ctrl Pts',(-16.9013570056506,6.54762058645456,
-1274.28760117483));
#149686=CARTESIAN_POINT('Ctrl Pts',(-16.1559070823762,8.04468584505497,
-1275.78171882189));
#149687=CARTESIAN_POINT('Ctrl Pts',(-15.4104571591017,9.54175110365538,
-1277.27583646895));
#149688=CARTESIAN_POINT('Ctrl Pts',(-14.4026149179538,10.8763499173728,
-1278.769954116));
#149689=CARTESIAN_POINT('Ctrl Pts',(-13.3947726768058,12.2109487310903,
-1280.26407176306));
#149690=CARTESIAN_POINT('Ctrl Pts',(-12.1588589765331,13.3376329379985,
-1281.75818941012));
#149691=CARTESIAN_POINT('Ctrl Pts',(-10.9229452762603,14.4643171449067,
-1283.25230705718));
#149692=CARTESIAN_POINT('Ctrl Pts',(-9.50104767561052,15.3447188656481,
-1284.74642470424));
#149693=CARTESIAN_POINT('Ctrl Pts',(-8.07915007496071,16.2251205863895,
-1286.2405423513));
#149694=CARTESIAN_POINT('Ctrl Pts',(-6.51968959134574,16.8292587962898,
-1287.73465999836));
#149695=CARTESIAN_POINT('Ctrl Pts',(-4.96022910773078,17.4333970061901,
-1289.22877764542));
#149696=CARTESIAN_POINT('Ctrl Pts',(-3.31631129755346,17.7406985030951,
-1290.72289529247));
#149697=CARTESIAN_POINT('Ctrl Pts',(-1.67239348737615,18.048,-1292.21701293953));
#149698=CARTESIAN_POINT('Ctrl Pts',(-2.21024254310115E-15,18.048,-1293.71113058659));
#149699=CARTESIAN_POINT('Ctrl Pts',(1.67239348737616,18.048,-1295.20524823365));
#149700=CARTESIAN_POINT('Ctrl Pts',(3.31631129755346,17.7406985030951,-1296.69936588071));
#149701=CARTESIAN_POINT('Ctrl Pts',(4.96022910773077,17.4333970061901,-1298.19348352777));
#149702=CARTESIAN_POINT('Ctrl Pts',(6.51968959134575,16.8292587962898,-1299.68760117483));
#149703=CARTESIAN_POINT('Ctrl Pts',(8.07915007496071,16.2251205863895,-1301.18171882189));
#149704=CARTESIAN_POINT('Ctrl Pts',(9.50104767561053,15.3447188656481,-1302.67583646895));
#149705=CARTESIAN_POINT('Ctrl Pts',(10.9229452762603,14.4643171449067,-1304.169954116));
#149706=CARTESIAN_POINT('Ctrl Pts',(12.1588589765331,13.3376329379985,-1305.66407176306));
#149707=CARTESIAN_POINT('Ctrl Pts',(13.3947726768058,12.2109487310903,-1307.15818941012));
#149708=CARTESIAN_POINT('Ctrl Pts',(14.4026149179538,10.8763499173728,-1308.65230705718));
#149709=CARTESIAN_POINT('Ctrl Pts',(15.4104571591017,9.54175110365538,-1310.14642470424));
#149710=CARTESIAN_POINT('Ctrl Pts',(16.1559070823762,8.04468584505496,-1311.6405423513));
#149711=CARTESIAN_POINT('Ctrl Pts',(16.9013570056506,6.54762058645456,-1313.13465999836));
#149712=CARTESIAN_POINT('Ctrl Pts',(17.3590292079831,4.93906964482096,-1314.62877764542));
#149713=CARTESIAN_POINT('Ctrl Pts',(17.8167014103155,3.33051870318735,-1316.12289529247));
#149714=CARTESIAN_POINT('Ctrl Pts',(17.9710104137728,1.66525935159367,-1317.61701293953));
#149715=CARTESIAN_POINT('Ctrl Pts',(18.1253194172301,3.32956716117513E-15,
-1319.11113058659));
#149716=CARTESIAN_POINT('Ctrl Pts',(17.9710104137728,-1.66525935159367,
-1320.60524823365));
#149717=CARTESIAN_POINT('Ctrl Pts',(17.8167014103155,-3.33051870318736,
-1322.09936588071));
#149718=CARTESIAN_POINT('Ctrl Pts',(17.3590292079831,-4.93906964482095,
-1323.59348352777));
#149719=CARTESIAN_POINT('Ctrl Pts',(16.9013570056506,-6.54762058645456,
-1325.08760117483));
#149720=CARTESIAN_POINT('Ctrl Pts',(16.1559070823762,-8.04468584505497,
-1326.58171882189));
#149721=CARTESIAN_POINT('Ctrl Pts',(15.4104571591017,-9.54175110365538,
-1328.07583646895));
#149722=CARTESIAN_POINT('Ctrl Pts',(14.4026149179538,-10.8763499173728,
-1329.569954116));
#149723=CARTESIAN_POINT('Ctrl Pts',(13.3947726768058,-12.2109487310903,
-1331.06407176306));
#149724=CARTESIAN_POINT('Ctrl Pts',(12.1588589765331,-13.3376329379985,
-1332.55818941012));
#149725=CARTESIAN_POINT('Ctrl Pts',(10.9229452762603,-14.4643171449067,
-1334.05230705718));
#149726=CARTESIAN_POINT('Ctrl Pts',(9.50104767561053,-15.3447188656481,
-1335.54642470424));
#149727=CARTESIAN_POINT('Ctrl Pts',(8.07915007496071,-16.2251205863895,
-1337.0405423513));
#149728=CARTESIAN_POINT('Ctrl Pts',(6.51968959134574,-16.8292587962898,
-1338.53465999836));
#149729=CARTESIAN_POINT('Ctrl Pts',(4.96022910773078,-17.4333970061901,
-1340.02877764542));
#149730=CARTESIAN_POINT('Ctrl Pts',(3.31631129755346,-17.7406985030951,
-1341.52289529247));
#149731=CARTESIAN_POINT('Ctrl Pts',(1.67239348737615,-18.048,-1343.01701293953));
#149732=CARTESIAN_POINT('Ctrl Pts',(0.,-18.048,-1344.51113058659));
#149733=CARTESIAN_POINT('Ctrl Pts',(-1.67239348737615,-18.048,-1346.00524823365));
#149734=CARTESIAN_POINT('Ctrl Pts',(-3.31631129755346,-17.7406985030951,
-1347.49936588071));
#149735=CARTESIAN_POINT('Ctrl Pts',(-4.96022910773077,-17.4333970061901,
-1348.99348352777));
#149736=CARTESIAN_POINT('Ctrl Pts',(-6.51968959134574,-16.8292587962898,
-1350.48760117483));
#149737=CARTESIAN_POINT('Ctrl Pts',(-8.07915007496071,-16.2251205863895,
-1351.98171882189));
#149738=CARTESIAN_POINT('Ctrl Pts',(-9.50104767561052,-15.3447188656481,
-1353.47583646895));
#149739=CARTESIAN_POINT('Ctrl Pts',(-10.9229452762603,-14.4643171449067,
-1354.969954116));
#149740=CARTESIAN_POINT('Ctrl Pts',(-12.1588589765331,-13.3376329379985,
-1356.46407176306));
#149741=CARTESIAN_POINT('Ctrl Pts',(-13.3947726768058,-12.2109487310903,
-1357.95818941012));
#149742=CARTESIAN_POINT('Ctrl Pts',(-14.4026149179538,-10.8763499173728,
-1359.45230705718));
#149743=CARTESIAN_POINT('Ctrl Pts',(-15.4104571591017,-9.54175110365538,
-1360.94642470424));
#149744=CARTESIAN_POINT('Ctrl Pts',(-16.1559070823762,-8.04468584505497,
-1362.4405423513));
#149745=CARTESIAN_POINT('Ctrl Pts',(-16.9013570056506,-6.54762058645456,
-1363.93465999836));
#149746=CARTESIAN_POINT('Ctrl Pts',(-17.3590292079831,-4.93906964482095,
-1365.42877764542));
#149747=CARTESIAN_POINT('Ctrl Pts',(-17.8167014103155,-3.33051870318735,
-1366.92289529248));
#149748=CARTESIAN_POINT('Ctrl Pts',(-17.9710104137728,-1.66525935159368,
-1368.41701293953));
#149749=CARTESIAN_POINT('Ctrl Pts',(-18.1253194172301,-1.10985572039171E-15,
-1369.91113058659));
#149750=CARTESIAN_POINT('Ctrl Pts',(-17.9710104137728,1.66525935159367,
-1371.40524823365));
#149751=CARTESIAN_POINT('Ctrl Pts',(-17.8167014103155,3.33051870318735,
-1372.89936588071));
#149752=CARTESIAN_POINT('Ctrl Pts',(-17.3590292079831,4.93906964482096,
-1374.39348352777));
#149753=CARTESIAN_POINT('Ctrl Pts',(-16.9013570056506,6.54762058645456,
-1375.88760117483));
#149754=CARTESIAN_POINT('Ctrl Pts',(-16.1559070823762,8.04468584505497,
-1377.38171882189));
#149755=CARTESIAN_POINT('Ctrl Pts',(-15.4104571591017,9.54175110365538,
-1378.87583646895));
#149756=CARTESIAN_POINT('Ctrl Pts',(-14.4026149179538,10.8763499173728,
-1380.369954116));
#149757=CARTESIAN_POINT('Ctrl Pts',(-13.3947726768058,12.2109487310903,
-1381.86407176306));
#149758=CARTESIAN_POINT('Ctrl Pts',(-12.1588589765331,13.3376329379985,
-1383.35818941012));
#149759=CARTESIAN_POINT('Ctrl Pts',(-10.9229452762603,14.4643171449067,
-1384.85230705718));
#149760=CARTESIAN_POINT('Ctrl Pts',(-9.50104767561052,15.3447188656481,
-1386.34642470424));
#149761=CARTESIAN_POINT('Ctrl Pts',(-8.07915007496071,16.2251205863895,
-1387.8405423513));
#149762=CARTESIAN_POINT('Ctrl Pts',(-6.51968959134574,16.8292587962898,
-1389.33465999836));
#149763=CARTESIAN_POINT('Ctrl Pts',(-4.96022910773078,17.4333970061901,
-1390.82877764542));
#149764=CARTESIAN_POINT('Ctrl Pts',(-3.31631129755346,17.7406985030951,
-1392.32289529247));
#149765=CARTESIAN_POINT('Ctrl Pts',(-1.67239348737615,18.048,-1393.81701293953));
#149766=CARTESIAN_POINT('Ctrl Pts',(-2.21024254310115E-15,18.048,-1395.31113058659));
#149767=CARTESIAN_POINT('Ctrl Pts',(1.67239348737616,18.048,-1396.80524823365));
#149768=CARTESIAN_POINT('Ctrl Pts',(3.31631129755346,17.7406985030951,-1398.29936588071));
#149769=CARTESIAN_POINT('Ctrl Pts',(4.96022910773077,17.4333970061901,-1399.79348352777));
#149770=CARTESIAN_POINT('Ctrl Pts',(6.51968959134575,16.8292587962898,-1401.28760117483));
#149771=CARTESIAN_POINT('Ctrl Pts',(8.07915007496071,16.2251205863895,-1402.78171882189));
#149772=CARTESIAN_POINT('Ctrl Pts',(9.50104767561053,15.3447188656481,-1404.27583646895));
#149773=CARTESIAN_POINT('Ctrl Pts',(10.9229452762603,14.4643171449067,-1405.769954116));
#149774=CARTESIAN_POINT('Ctrl Pts',(12.1588589765331,13.3376329379985,-1407.26407176306));
#149775=CARTESIAN_POINT('Ctrl Pts',(13.3947726768058,12.2109487310903,-1408.75818941012));
#149776=CARTESIAN_POINT('Ctrl Pts',(14.4026149179538,10.8763499173728,-1410.25230705718));
#149777=CARTESIAN_POINT('Ctrl Pts',(15.4104571591017,9.54175110365538,-1411.74642470424));
#149778=CARTESIAN_POINT('Ctrl Pts',(16.1559070823762,8.04468584505496,-1413.2405423513));
#149779=CARTESIAN_POINT('Ctrl Pts',(16.9013570056506,6.54762058645456,-1414.73465999836));
#149780=CARTESIAN_POINT('Ctrl Pts',(17.3590292079831,4.93906964482096,-1416.22877764542));
#149781=CARTESIAN_POINT('Ctrl Pts',(17.8167014103155,3.33051870318735,-1417.72289529247));
#149782=CARTESIAN_POINT('Ctrl Pts',(17.9710104137728,1.66525935159367,-1419.21701293953));
#149783=CARTESIAN_POINT('Ctrl Pts',(18.1253194172301,3.32956716117513E-15,
-1420.71113058659));
#149784=CARTESIAN_POINT('Ctrl Pts',(17.9710104137728,-1.66525935159367,
-1422.20524823365));
#149785=CARTESIAN_POINT('Ctrl Pts',(17.8167014103155,-3.33051870318736,
-1423.69936588071));
#149786=CARTESIAN_POINT('Ctrl Pts',(17.3590292079831,-4.93906964482095,
-1425.19348352777));
#149787=CARTESIAN_POINT('Ctrl Pts',(16.9013570056506,-6.54762058645456,
-1426.68760117483));
#149788=CARTESIAN_POINT('Ctrl Pts',(16.1559070823762,-8.04468584505497,
-1428.18171882189));
#149789=CARTESIAN_POINT('Ctrl Pts',(15.4104571591017,-9.54175110365538,
-1429.67583646895));
#149790=CARTESIAN_POINT('Ctrl Pts',(14.4026149179538,-10.8763499173728,
-1431.169954116));
#149791=CARTESIAN_POINT('Ctrl Pts',(13.3947726768058,-12.2109487310903,
-1432.66407176306));
#149792=CARTESIAN_POINT('Ctrl Pts',(12.1588589765331,-13.3376329379985,
-1434.15818941012));
#149793=CARTESIAN_POINT('Ctrl Pts',(10.9229452762603,-14.4643171449067,
-1435.65230705718));
#149794=CARTESIAN_POINT('Ctrl Pts',(9.50104767561053,-15.3447188656481,
-1437.14642470424));
#149795=CARTESIAN_POINT('Ctrl Pts',(8.07915007496071,-16.2251205863895,
-1438.6405423513));
#149796=CARTESIAN_POINT('Ctrl Pts',(6.51968959134574,-16.8292587962898,
-1440.13465999836));
#149797=CARTESIAN_POINT('Ctrl Pts',(4.96022910773078,-17.4333970061901,
-1441.62877764542));
#149798=CARTESIAN_POINT('Ctrl Pts',(3.31631129755346,-17.7406985030951,
-1443.12289529247));
#149799=CARTESIAN_POINT('Ctrl Pts',(1.67239348737615,-18.048,-1444.61701293953));
#149800=CARTESIAN_POINT('Ctrl Pts',(0.,-18.048,-1446.11113058659));
#149801=CARTESIAN_POINT('Ctrl Pts',(-1.67239348737615,-18.048,-1447.60524823365));
#149802=CARTESIAN_POINT('Ctrl Pts',(-3.31631129755346,-17.7406985030951,
-1449.09936588071));
#149803=CARTESIAN_POINT('Ctrl Pts',(-4.96022910773077,-17.4333970061901,
-1450.59348352777));
#149804=CARTESIAN_POINT('Ctrl Pts',(-6.51968959134574,-16.8292587962898,
-1452.08760117483));
#149805=CARTESIAN_POINT('Ctrl Pts',(-8.07915007496071,-16.2251205863895,
-1453.58171882189));
#149806=CARTESIAN_POINT('Ctrl Pts',(-9.50104767561052,-15.3447188656481,
-1455.07583646895));
#149807=CARTESIAN_POINT('Ctrl Pts',(-10.9229452762603,-14.4643171449067,
-1456.569954116));
#149808=CARTESIAN_POINT('Ctrl Pts',(-12.1588589765331,-13.3376329379985,
-1458.06407176306));
#149809=CARTESIAN_POINT('Ctrl Pts',(-13.3947726768058,-12.2109487310903,
-1459.55818941012));
#149810=CARTESIAN_POINT('Ctrl Pts',(-14.4026149179538,-10.8763499173728,
-1461.05230705718));
#149811=CARTESIAN_POINT('Ctrl Pts',(-15.4104571591017,-9.54175110365538,
-1462.54642470424));
#149812=CARTESIAN_POINT('Ctrl Pts',(-16.1559070823762,-8.04468584505497,
-1464.0405423513));
#149813=CARTESIAN_POINT('Ctrl Pts',(-16.9013570056506,-6.54762058645456,
-1465.53465999836));
#149814=CARTESIAN_POINT('Ctrl Pts',(-17.3590292079831,-4.93906964482095,
-1467.02877764542));
#149815=CARTESIAN_POINT('Ctrl Pts',(-17.8167014103155,-3.33051870318735,
-1468.52289529247));
#149816=CARTESIAN_POINT('Ctrl Pts',(-17.9710104137728,-1.66525935159368,
-1470.01701293953));
#149817=CARTESIAN_POINT('Ctrl Pts',(-18.1253194172301,-1.10985572039171E-15,
-1471.51113058659));
#149818=CARTESIAN_POINT('Ctrl Pts',(-17.9710104137728,1.66525935159367,
-1473.00524823365));
#149819=CARTESIAN_POINT('Ctrl Pts',(-17.8167014103155,3.33051870318735,
-1474.49936588071));
#149820=CARTESIAN_POINT('Ctrl Pts',(-17.3590292079831,4.93906964482096,
-1475.99348352777));
#149821=CARTESIAN_POINT('Ctrl Pts',(-16.9013570056506,6.54762058645456,
-1477.48760117483));
#149822=CARTESIAN_POINT('Ctrl Pts',(-16.1559070823762,8.04468584505497,
-1478.98171882189));
#149823=CARTESIAN_POINT('Ctrl Pts',(-15.4104571591017,9.54175110365538,
-1480.47583646895));
#149824=CARTESIAN_POINT('Ctrl Pts',(-14.4026149179538,10.8763499173728,
-1481.969954116));
#149825=CARTESIAN_POINT('Ctrl Pts',(-13.3947726768058,12.2109487310903,
-1483.46407176306));
#149826=CARTESIAN_POINT('Ctrl Pts',(-12.1588589765331,13.3376329379985,
-1484.95818941012));
#149827=CARTESIAN_POINT('Ctrl Pts',(-10.9229452762603,14.4643171449067,
-1486.45230705718));
#149828=CARTESIAN_POINT('Ctrl Pts',(-9.50104767561052,15.3447188656481,
-1487.94642470424));
#149829=CARTESIAN_POINT('Ctrl Pts',(-8.07915007496071,16.2251205863895,
-1489.4405423513));
#149830=CARTESIAN_POINT('Ctrl Pts',(-6.51968959134574,16.8292587962898,
-1490.93465999836));
#149831=CARTESIAN_POINT('Ctrl Pts',(-4.96022910773078,17.4333970061901,
-1492.42877764542));
#149832=CARTESIAN_POINT('Ctrl Pts',(-3.31631129755346,17.7406985030951,
-1493.92289529247));
#149833=CARTESIAN_POINT('Ctrl Pts',(-1.67239348737615,18.048,-1495.41701293953));
#149834=CARTESIAN_POINT('Ctrl Pts',(-2.21024254310115E-15,18.048,-1496.91113058659));
#149835=CARTESIAN_POINT('Ctrl Pts',(1.67239348737616,18.048,-1498.40524823365));
#149836=CARTESIAN_POINT('Ctrl Pts',(3.31631129755346,17.7406985030951,-1499.89936588071));
#149837=CARTESIAN_POINT('Ctrl Pts',(4.96022910773077,17.4333970061901,-1501.39348352777));
#149838=CARTESIAN_POINT('Ctrl Pts',(6.51968959134575,16.8292587962898,-1502.88760117483));
#149839=CARTESIAN_POINT('Ctrl Pts',(7.54139510186126,16.4334479728329,-1503.86649627951));
#149840=CARTESIAN_POINT('Ctrl Pts',(8.50771391856893,15.9169440496532,-1504.8491753622));
#149841=CARTESIAN_POINT('',(4.96991138555256,-17.3502243449402,692.));
#149842=CARTESIAN_POINT('Origin',(-231.282509043856,-78.0829325244463,692.000033290347));
#149843=CARTESIAN_POINT('',(0.,-18.048,1500.28886941341));
#149844=CARTESIAN_POINT('Ctrl Pts',(0.,-18.048,1500.28886941341));
#149845=CARTESIAN_POINT('Ctrl Pts',(-1.67239348737611,-18.048,1498.79475176635));
#149846=CARTESIAN_POINT('Ctrl Pts',(-3.31631129755346,-17.7406985030951,
1497.30063411929));
#149847=CARTESIAN_POINT('Ctrl Pts',(-4.96022910773077,-17.4333970061901,
1495.80651647223));
#149848=CARTESIAN_POINT('Ctrl Pts',(-6.51968959134574,-16.8292587962898,
1494.31239882517));
#149849=CARTESIAN_POINT('Ctrl Pts',(-8.07915007496071,-16.2251205863895,
1492.81828117811));
#149850=CARTESIAN_POINT('Ctrl Pts',(-9.50104767561052,-15.3447188656481,
1491.32416353106));
#149851=CARTESIAN_POINT('Ctrl Pts',(-10.9229452762603,-14.4643171449067,
1489.830045884));
#149852=CARTESIAN_POINT('Ctrl Pts',(-12.1588589765331,-13.3376329379985,
1488.33592823694));
#149853=CARTESIAN_POINT('Ctrl Pts',(-13.3947726768058,-12.2109487310903,
1486.84181058988));
#149854=CARTESIAN_POINT('Ctrl Pts',(-14.4026149179538,-10.8763499173728,
1485.34769294282));
#149855=CARTESIAN_POINT('Ctrl Pts',(-15.4104571591017,-9.54175110365538,
1483.85357529576));
#149856=CARTESIAN_POINT('Ctrl Pts',(-16.1559070823762,-8.04468584505497,
1482.3594576487));
#149857=CARTESIAN_POINT('Ctrl Pts',(-16.9013570056506,-6.54762058645456,
1480.86534000164));
#149858=CARTESIAN_POINT('Ctrl Pts',(-17.3590292079831,-4.93906964482095,
1479.37122235458));
#149859=CARTESIAN_POINT('Ctrl Pts',(-17.8167014103155,-3.33051870318735,
1477.87710470753));
#149860=CARTESIAN_POINT('Ctrl Pts',(-17.9710104137728,-1.66525935159368,
1476.38298706047));
#149861=CARTESIAN_POINT('Ctrl Pts',(-18.1253194172301,-1.10985572039171E-15,
1474.88886941341));
#149862=CARTESIAN_POINT('Ctrl Pts',(-17.9710104137728,1.66525935159367,
1473.39475176635));
#149863=CARTESIAN_POINT('Ctrl Pts',(-17.8167014103155,3.33051870318735,
1471.90063411929));
#149864=CARTESIAN_POINT('Ctrl Pts',(-17.3590292079831,4.93906964482096,
1470.40651647223));
#149865=CARTESIAN_POINT('Ctrl Pts',(-16.9013570056506,6.54762058645456,
1468.91239882517));
#149866=CARTESIAN_POINT('Ctrl Pts',(-16.1559070823762,8.04468584505497,
1467.41828117811));
#149867=CARTESIAN_POINT('Ctrl Pts',(-15.4104571591017,9.54175110365538,
1465.92416353106));
#149868=CARTESIAN_POINT('Ctrl Pts',(-14.4026149179538,10.8763499173728,
1464.430045884));
#149869=CARTESIAN_POINT('Ctrl Pts',(-13.3947726768058,12.2109487310903,
1462.93592823694));
#149870=CARTESIAN_POINT('Ctrl Pts',(-12.1588589765331,13.3376329379985,
1461.44181058988));
#149871=CARTESIAN_POINT('Ctrl Pts',(-10.9229452762603,14.4643171449067,
1459.94769294282));
#149872=CARTESIAN_POINT('Ctrl Pts',(-9.50104767561052,15.3447188656481,
1458.45357529576));
#149873=CARTESIAN_POINT('Ctrl Pts',(-8.07915007496071,16.2251205863895,
1456.9594576487));
#149874=CARTESIAN_POINT('Ctrl Pts',(-6.51968959134574,16.8292587962898,
1455.46534000164));
#149875=CARTESIAN_POINT('Ctrl Pts',(-4.96022910773078,17.4333970061901,
1453.97122235458));
#149876=CARTESIAN_POINT('Ctrl Pts',(-3.31631129755346,17.7406985030951,
1452.47710470753));
#149877=CARTESIAN_POINT('Ctrl Pts',(-1.67239348737615,18.048,1450.98298706047));
#149878=CARTESIAN_POINT('Ctrl Pts',(-2.21024254310115E-15,18.048,1449.48886941341));
#149879=CARTESIAN_POINT('Ctrl Pts',(1.67239348737616,18.048,1447.99475176635));
#149880=CARTESIAN_POINT('Ctrl Pts',(3.31631129755346,17.7406985030951,1446.50063411929));
#149881=CARTESIAN_POINT('Ctrl Pts',(4.96022910773077,17.4333970061901,1445.00651647223));
#149882=CARTESIAN_POINT('Ctrl Pts',(6.51968959134575,16.8292587962898,1443.51239882517));
#149883=CARTESIAN_POINT('Ctrl Pts',(8.07915007496071,16.2251205863895,1442.01828117811));
#149884=CARTESIAN_POINT('Ctrl Pts',(9.50104767561053,15.3447188656481,1440.52416353105));
#149885=CARTESIAN_POINT('Ctrl Pts',(10.9229452762603,14.4643171449067,1439.030045884));
#149886=CARTESIAN_POINT('Ctrl Pts',(12.1588589765331,13.3376329379985,1437.53592823694));
#149887=CARTESIAN_POINT('Ctrl Pts',(13.3947726768058,12.2109487310903,1436.04181058988));
#149888=CARTESIAN_POINT('Ctrl Pts',(14.4026149179538,10.8763499173728,1434.54769294282));
#149889=CARTESIAN_POINT('Ctrl Pts',(15.4104571591017,9.54175110365539,1433.05357529576));
#149890=CARTESIAN_POINT('Ctrl Pts',(16.1559070823762,8.04468584505496,1431.5594576487));
#149891=CARTESIAN_POINT('Ctrl Pts',(16.9013570056506,6.54762058645456,1430.06534000164));
#149892=CARTESIAN_POINT('Ctrl Pts',(17.3590292079831,4.93906964482096,1428.57122235458));
#149893=CARTESIAN_POINT('Ctrl Pts',(17.8167014103155,3.33051870318735,1427.07710470753));
#149894=CARTESIAN_POINT('Ctrl Pts',(17.9710104137728,1.66525935159367,1425.58298706047));
#149895=CARTESIAN_POINT('Ctrl Pts',(18.1253194172301,3.32956716117513E-15,
1424.08886941341));
#149896=CARTESIAN_POINT('Ctrl Pts',(17.9710104137728,-1.66525935159367,
1422.59475176635));
#149897=CARTESIAN_POINT('Ctrl Pts',(17.8167014103155,-3.33051870318736,
1421.10063411929));
#149898=CARTESIAN_POINT('Ctrl Pts',(17.3590292079831,-4.93906964482095,
1419.60651647223));
#149899=CARTESIAN_POINT('Ctrl Pts',(16.9013570056506,-6.54762058645456,
1418.11239882517));
#149900=CARTESIAN_POINT('Ctrl Pts',(16.1559070823762,-8.04468584505497,
1416.61828117811));
#149901=CARTESIAN_POINT('Ctrl Pts',(15.4104571591017,-9.54175110365538,
1415.12416353105));
#149902=CARTESIAN_POINT('Ctrl Pts',(14.4026149179538,-10.8763499173728,
1413.630045884));
#149903=CARTESIAN_POINT('Ctrl Pts',(13.3947726768058,-12.2109487310903,
1412.13592823694));
#149904=CARTESIAN_POINT('Ctrl Pts',(12.1588589765331,-13.3376329379985,
1410.64181058988));
#149905=CARTESIAN_POINT('Ctrl Pts',(10.9229452762603,-14.4643171449067,
1409.14769294282));
#149906=CARTESIAN_POINT('Ctrl Pts',(9.50104767561053,-15.3447188656481,
1407.65357529576));
#149907=CARTESIAN_POINT('Ctrl Pts',(8.07915007496071,-16.2251205863895,
1406.1594576487));
#149908=CARTESIAN_POINT('Ctrl Pts',(6.51968959134574,-16.8292587962898,
1404.66534000164));
#149909=CARTESIAN_POINT('Ctrl Pts',(4.96022910773078,-17.4333970061901,
1403.17122235458));
#149910=CARTESIAN_POINT('Ctrl Pts',(3.31631129755346,-17.7406985030951,
1401.67710470753));
#149911=CARTESIAN_POINT('Ctrl Pts',(1.67239348737615,-18.048,1400.18298706047));
#149912=CARTESIAN_POINT('Ctrl Pts',(0.,-18.048,1398.68886941341));
#149913=CARTESIAN_POINT('Ctrl Pts',(-1.67239348737615,-18.048,1397.19475176635));
#149914=CARTESIAN_POINT('Ctrl Pts',(-3.31631129755346,-17.7406985030951,
1395.70063411929));
#149915=CARTESIAN_POINT('Ctrl Pts',(-4.96022910773077,-17.4333970061901,
1394.20651647223));
#149916=CARTESIAN_POINT('Ctrl Pts',(-6.51968959134574,-16.8292587962898,
1392.71239882517));
#149917=CARTESIAN_POINT('Ctrl Pts',(-8.07915007496071,-16.2251205863895,
1391.21828117811));
#149918=CARTESIAN_POINT('Ctrl Pts',(-9.50104767561052,-15.3447188656481,
1389.72416353105));
#149919=CARTESIAN_POINT('Ctrl Pts',(-10.9229452762603,-14.4643171449067,
1388.230045884));
#149920=CARTESIAN_POINT('Ctrl Pts',(-12.1588589765331,-13.3376329379985,
1386.73592823694));
#149921=CARTESIAN_POINT('Ctrl Pts',(-13.3947726768058,-12.2109487310903,
1385.24181058988));
#149922=CARTESIAN_POINT('Ctrl Pts',(-14.4026149179538,-10.8763499173728,
1383.74769294282));
#149923=CARTESIAN_POINT('Ctrl Pts',(-15.4104571591017,-9.54175110365538,
1382.25357529576));
#149924=CARTESIAN_POINT('Ctrl Pts',(-16.1559070823762,-8.04468584505497,
1380.7594576487));
#149925=CARTESIAN_POINT('Ctrl Pts',(-16.9013570056506,-6.54762058645456,
1379.26534000164));
#149926=CARTESIAN_POINT('Ctrl Pts',(-17.3590292079831,-4.93906964482095,
1377.77122235458));
#149927=CARTESIAN_POINT('Ctrl Pts',(-17.8167014103155,-3.33051870318735,
1376.27710470753));
#149928=CARTESIAN_POINT('Ctrl Pts',(-17.9710104137728,-1.66525935159368,
1374.78298706047));
#149929=CARTESIAN_POINT('Ctrl Pts',(-18.1253194172301,-1.10985572039171E-15,
1373.28886941341));
#149930=CARTESIAN_POINT('Ctrl Pts',(-17.9710104137728,1.66525935159367,
1371.79475176635));
#149931=CARTESIAN_POINT('Ctrl Pts',(-17.8167014103155,3.33051870318735,
1370.30063411929));
#149932=CARTESIAN_POINT('Ctrl Pts',(-17.3590292079831,4.93906964482096,
1368.80651647223));
#149933=CARTESIAN_POINT('Ctrl Pts',(-16.9013570056506,6.54762058645456,
1367.31239882517));
#149934=CARTESIAN_POINT('Ctrl Pts',(-16.1559070823762,8.04468584505497,
1365.81828117811));
#149935=CARTESIAN_POINT('Ctrl Pts',(-15.4104571591017,9.54175110365538,
1364.32416353105));
#149936=CARTESIAN_POINT('Ctrl Pts',(-14.4026149179538,10.8763499173728,
1362.830045884));
#149937=CARTESIAN_POINT('Ctrl Pts',(-13.3947726768058,12.2109487310903,
1361.33592823694));
#149938=CARTESIAN_POINT('Ctrl Pts',(-12.1588589765331,13.3376329379985,
1359.84181058988));
#149939=CARTESIAN_POINT('Ctrl Pts',(-10.9229452762603,14.4643171449067,
1358.34769294282));
#149940=CARTESIAN_POINT('Ctrl Pts',(-9.50104767561052,15.3447188656481,
1356.85357529576));
#149941=CARTESIAN_POINT('Ctrl Pts',(-8.07915007496071,16.2251205863895,
1355.3594576487));
#149942=CARTESIAN_POINT('Ctrl Pts',(-6.51968959134574,16.8292587962898,
1353.86534000164));
#149943=CARTESIAN_POINT('Ctrl Pts',(-4.96022910773078,17.4333970061901,
1352.37122235458));
#149944=CARTESIAN_POINT('Ctrl Pts',(-3.31631129755346,17.7406985030951,
1350.87710470753));
#149945=CARTESIAN_POINT('Ctrl Pts',(-1.67239348737615,18.048,1349.38298706047));
#149946=CARTESIAN_POINT('Ctrl Pts',(-2.21024254310115E-15,18.048,1347.88886941341));
#149947=CARTESIAN_POINT('Ctrl Pts',(1.67239348737616,18.048,1346.39475176635));
#149948=CARTESIAN_POINT('Ctrl Pts',(3.31631129755346,17.7406985030951,1344.90063411929));
#149949=CARTESIAN_POINT('Ctrl Pts',(4.96022910773077,17.4333970061901,1343.40651647223));
#149950=CARTESIAN_POINT('Ctrl Pts',(6.51968959134575,16.8292587962898,1341.91239882517));
#149951=CARTESIAN_POINT('Ctrl Pts',(8.07915007496071,16.2251205863895,1340.41828117811));
#149952=CARTESIAN_POINT('Ctrl Pts',(9.50104767561053,15.3447188656481,1338.92416353106));
#149953=CARTESIAN_POINT('Ctrl Pts',(10.9229452762603,14.4643171449067,1337.430045884));
#149954=CARTESIAN_POINT('Ctrl Pts',(12.1588589765331,13.3376329379985,1335.93592823694));
#149955=CARTESIAN_POINT('Ctrl Pts',(13.3947726768058,12.2109487310903,1334.44181058988));
#149956=CARTESIAN_POINT('Ctrl Pts',(14.4026149179538,10.8763499173728,1332.94769294282));
#149957=CARTESIAN_POINT('Ctrl Pts',(15.4104571591017,9.54175110365539,1331.45357529576));
#149958=CARTESIAN_POINT('Ctrl Pts',(16.1559070823762,8.04468584505496,1329.9594576487));
#149959=CARTESIAN_POINT('Ctrl Pts',(16.9013570056506,6.54762058645456,1328.46534000164));
#149960=CARTESIAN_POINT('Ctrl Pts',(17.3590292079831,4.93906964482096,1326.97122235458));
#149961=CARTESIAN_POINT('Ctrl Pts',(17.8167014103155,3.33051870318735,1325.47710470753));
#149962=CARTESIAN_POINT('Ctrl Pts',(17.9710104137728,1.66525935159367,1323.98298706047));
#149963=CARTESIAN_POINT('Ctrl Pts',(18.1253194172301,3.32956716117513E-15,
1322.48886941341));
#149964=CARTESIAN_POINT('Ctrl Pts',(17.9710104137728,-1.66525935159367,
1320.99475176635));
#149965=CARTESIAN_POINT('Ctrl Pts',(17.8167014103155,-3.33051870318736,
1319.50063411929));
#149966=CARTESIAN_POINT('Ctrl Pts',(17.3590292079831,-4.93906964482095,
1318.00651647223));
#149967=CARTESIAN_POINT('Ctrl Pts',(16.9013570056506,-6.54762058645456,
1316.51239882517));
#149968=CARTESIAN_POINT('Ctrl Pts',(16.1559070823762,-8.04468584505497,
1315.01828117811));
#149969=CARTESIAN_POINT('Ctrl Pts',(15.4104571591017,-9.54175110365538,
1313.52416353105));
#149970=CARTESIAN_POINT('Ctrl Pts',(14.4026149179538,-10.8763499173728,
1312.030045884));
#149971=CARTESIAN_POINT('Ctrl Pts',(13.3947726768058,-12.2109487310903,
1310.53592823694));
#149972=CARTESIAN_POINT('Ctrl Pts',(12.1588589765331,-13.3376329379985,
1309.04181058988));
#149973=CARTESIAN_POINT('Ctrl Pts',(10.9229452762603,-14.4643171449067,
1307.54769294282));
#149974=CARTESIAN_POINT('Ctrl Pts',(9.50104767561053,-15.3447188656481,
1306.05357529576));
#149975=CARTESIAN_POINT('Ctrl Pts',(8.07915007496071,-16.2251205863895,
1304.5594576487));
#149976=CARTESIAN_POINT('Ctrl Pts',(6.51968959134574,-16.8292587962898,
1303.06534000164));
#149977=CARTESIAN_POINT('Ctrl Pts',(4.96022910773078,-17.4333970061901,
1301.57122235458));
#149978=CARTESIAN_POINT('Ctrl Pts',(3.31631129755346,-17.7406985030951,
1300.07710470753));
#149979=CARTESIAN_POINT('Ctrl Pts',(1.67239348737615,-18.048,1298.58298706047));
#149980=CARTESIAN_POINT('Ctrl Pts',(0.,-18.048,1297.08886941341));
#149981=CARTESIAN_POINT('Ctrl Pts',(-1.67239348737615,-18.048,1295.59475176635));
#149982=CARTESIAN_POINT('Ctrl Pts',(-3.31631129755346,-17.7406985030951,
1294.10063411929));
#149983=CARTESIAN_POINT('Ctrl Pts',(-4.96022910773077,-17.4333970061901,
1292.60651647223));
#149984=CARTESIAN_POINT('Ctrl Pts',(-6.51968959134574,-16.8292587962898,
1291.11239882517));
#149985=CARTESIAN_POINT('Ctrl Pts',(-8.07915007496071,-16.2251205863895,
1289.61828117811));
#149986=CARTESIAN_POINT('Ctrl Pts',(-9.50104767561052,-15.3447188656481,
1288.12416353105));
#149987=CARTESIAN_POINT('Ctrl Pts',(-10.9229452762603,-14.4643171449067,
1286.630045884));
#149988=CARTESIAN_POINT('Ctrl Pts',(-12.1588589765331,-13.3376329379985,
1285.13592823694));
#149989=CARTESIAN_POINT('Ctrl Pts',(-13.3947726768058,-12.2109487310903,
1283.64181058988));
#149990=CARTESIAN_POINT('Ctrl Pts',(-14.4026149179538,-10.8763499173728,
1282.14769294282));
#149991=CARTESIAN_POINT('Ctrl Pts',(-15.4104571591017,-9.54175110365538,
1280.65357529576));
#149992=CARTESIAN_POINT('Ctrl Pts',(-16.1559070823762,-8.04468584505497,
1279.1594576487));
#149993=CARTESIAN_POINT('Ctrl Pts',(-16.9013570056506,-6.54762058645456,
1277.66534000164));
#149994=CARTESIAN_POINT('Ctrl Pts',(-17.3590292079831,-4.93906964482095,
1276.17122235458));
#149995=CARTESIAN_POINT('Ctrl Pts',(-17.8167014103155,-3.33051870318735,
1274.67710470753));
#149996=CARTESIAN_POINT('Ctrl Pts',(-17.9710104137728,-1.66525935159368,
1273.18298706047));
#149997=CARTESIAN_POINT('Ctrl Pts',(-18.1253194172301,-1.10985572039171E-15,
1271.68886941341));
#149998=CARTESIAN_POINT('Ctrl Pts',(-17.9710104137728,1.66525935159367,
1270.19475176635));
#149999=CARTESIAN_POINT('Ctrl Pts',(-17.8167014103155,3.33051870318735,
1268.70063411929));
#150000=CARTESIAN_POINT('Ctrl Pts',(-17.3590292079831,4.93906964482096,
1267.20651647223));
#150001=CARTESIAN_POINT('Ctrl Pts',(-16.9013570056506,6.54762058645456,
1265.71239882517));
#150002=CARTESIAN_POINT('Ctrl Pts',(-16.1559070823762,8.04468584505497,
1264.21828117811));
#150003=CARTESIAN_POINT('Ctrl Pts',(-15.4104571591017,9.54175110365538,
1262.72416353105));
#150004=CARTESIAN_POINT('Ctrl Pts',(-14.4026149179538,10.8763499173728,
1261.230045884));
#150005=CARTESIAN_POINT('Ctrl Pts',(-13.3947726768058,12.2109487310903,
1259.73592823694));
#150006=CARTESIAN_POINT('Ctrl Pts',(-12.1588589765331,13.3376329379985,
1258.24181058988));
#150007=CARTESIAN_POINT('Ctrl Pts',(-10.9229452762603,14.4643171449067,
1256.74769294282));
#150008=CARTESIAN_POINT('Ctrl Pts',(-9.50104767561052,15.3447188656481,
1255.25357529576));
#150009=CARTESIAN_POINT('Ctrl Pts',(-8.07915007496071,16.2251205863895,
1253.7594576487));
#150010=CARTESIAN_POINT('Ctrl Pts',(-6.51968959134574,16.8292587962898,
1252.26534000164));
#150011=CARTESIAN_POINT('Ctrl Pts',(-4.96022910773078,17.4333970061901,
1250.77122235458));
#150012=CARTESIAN_POINT('Ctrl Pts',(-3.31631129755346,17.7406985030951,
1249.27710470753));
#150013=CARTESIAN_POINT('Ctrl Pts',(-1.67239348737615,18.048,1247.78298706047));
#150014=CARTESIAN_POINT('Ctrl Pts',(-2.21024254310115E-15,18.048,1246.28886941341));
#150015=CARTESIAN_POINT('Ctrl Pts',(1.67239348737616,18.048,1244.79475176635));
#150016=CARTESIAN_POINT('Ctrl Pts',(3.31631129755346,17.7406985030951,1243.30063411929));
#150017=CARTESIAN_POINT('Ctrl Pts',(4.96022910773077,17.4333970061901,1241.80651647223));
#150018=CARTESIAN_POINT('Ctrl Pts',(6.51968959134575,16.8292587962898,1240.31239882517));
#150019=CARTESIAN_POINT('Ctrl Pts',(8.07915007496071,16.2251205863895,1238.81828117811));
#150020=CARTESIAN_POINT('Ctrl Pts',(9.50104767561053,15.3447188656481,1237.32416353105));
#150021=CARTESIAN_POINT('Ctrl Pts',(10.9229452762603,14.4643171449067,1235.830045884));
#150022=CARTESIAN_POINT('Ctrl Pts',(12.1588589765331,13.3376329379985,1234.33592823694));
#150023=CARTESIAN_POINT('Ctrl Pts',(13.3947726768058,12.2109487310903,1232.84181058988));
#150024=CARTESIAN_POINT('Ctrl Pts',(14.4026149179538,10.8763499173728,1231.34769294282));
#150025=CARTESIAN_POINT('Ctrl Pts',(15.4104571591017,9.54175110365539,1229.85357529576));
#150026=CARTESIAN_POINT('Ctrl Pts',(16.1559070823762,8.04468584505496,1228.3594576487));
#150027=CARTESIAN_POINT('Ctrl Pts',(16.9013570056506,6.54762058645456,1226.86534000164));
#150028=CARTESIAN_POINT('Ctrl Pts',(17.3590292079831,4.93906964482096,1225.37122235458));
#150029=CARTESIAN_POINT('Ctrl Pts',(17.8167014103155,3.33051870318735,1223.87710470753));
#150030=CARTESIAN_POINT('Ctrl Pts',(17.9710104137728,1.66525935159367,1222.38298706047));
#150031=CARTESIAN_POINT('Ctrl Pts',(18.1253194172301,3.32956716117513E-15,
1220.88886941341));
#150032=CARTESIAN_POINT('Ctrl Pts',(17.9710104137728,-1.66525935159367,
1219.39475176635));
#150033=CARTESIAN_POINT('Ctrl Pts',(17.8167014103155,-3.33051870318736,
1217.90063411929));
#150034=CARTESIAN_POINT('Ctrl Pts',(17.3590292079831,-4.93906964482095,
1216.40651647223));
#150035=CARTESIAN_POINT('Ctrl Pts',(16.9013570056506,-6.54762058645456,
1214.91239882517));
#150036=CARTESIAN_POINT('Ctrl Pts',(16.1559070823762,-8.04468584505497,
1213.41828117811));
#150037=CARTESIAN_POINT('Ctrl Pts',(15.4104571591017,-9.54175110365538,
1211.92416353106));
#150038=CARTESIAN_POINT('Ctrl Pts',(14.4026149179538,-10.8763499173728,
1210.430045884));
#150039=CARTESIAN_POINT('Ctrl Pts',(13.3947726768058,-12.2109487310903,
1208.93592823694));
#150040=CARTESIAN_POINT('Ctrl Pts',(12.1588589765331,-13.3376329379985,
1207.44181058988));
#150041=CARTESIAN_POINT('Ctrl Pts',(10.9229452762603,-14.4643171449067,
1205.94769294282));
#150042=CARTESIAN_POINT('Ctrl Pts',(9.50104767561053,-15.3447188656481,
1204.45357529576));
#150043=CARTESIAN_POINT('Ctrl Pts',(8.07915007496071,-16.2251205863895,
1202.9594576487));
#150044=CARTESIAN_POINT('Ctrl Pts',(6.51968959134574,-16.8292587962898,
1201.46534000164));
#150045=CARTESIAN_POINT('Ctrl Pts',(4.96022910773078,-17.4333970061901,
1199.97122235458));
#150046=CARTESIAN_POINT('Ctrl Pts',(3.31631129755346,-17.7406985030951,
1198.47710470753));
#150047=CARTESIAN_POINT('Ctrl Pts',(1.67239348737615,-18.048,1196.98298706047));
#150048=CARTESIAN_POINT('Ctrl Pts',(0.,-18.048,1195.48886941341));
#150049=CARTESIAN_POINT('Ctrl Pts',(-1.67239348737615,-18.048,1193.99475176635));
#150050=CARTESIAN_POINT('Ctrl Pts',(-3.31631129755346,-17.7406985030951,
1192.50063411929));
#150051=CARTESIAN_POINT('Ctrl Pts',(-4.96022910773077,-17.4333970061901,
1191.00651647223));
#150052=CARTESIAN_POINT('Ctrl Pts',(-6.51968959134574,-16.8292587962898,
1189.51239882517));
#150053=CARTESIAN_POINT('Ctrl Pts',(-8.07915007496071,-16.2251205863895,
1188.01828117811));
#150054=CARTESIAN_POINT('Ctrl Pts',(-9.50104767561052,-15.3447188656481,
1186.52416353105));
#150055=CARTESIAN_POINT('Ctrl Pts',(-10.9229452762603,-14.4643171449067,
1185.030045884));
#150056=CARTESIAN_POINT('Ctrl Pts',(-12.1588589765331,-13.3376329379985,
1183.53592823694));
#150057=CARTESIAN_POINT('Ctrl Pts',(-13.3947726768058,-12.2109487310903,
1182.04181058988));
#150058=CARTESIAN_POINT('Ctrl Pts',(-14.4026149179538,-10.8763499173728,
1180.54769294282));
#150059=CARTESIAN_POINT('Ctrl Pts',(-15.4104571591017,-9.54175110365538,
1179.05357529576));
#150060=CARTESIAN_POINT('Ctrl Pts',(-16.1559070823762,-8.04468584505497,
1177.5594576487));
#150061=CARTESIAN_POINT('Ctrl Pts',(-16.9013570056506,-6.54762058645456,
1176.06534000164));
#150062=CARTESIAN_POINT('Ctrl Pts',(-17.3590292079831,-4.93906964482095,
1174.57122235458));
#150063=CARTESIAN_POINT('Ctrl Pts',(-17.8167014103155,-3.33051870318735,
1173.07710470753));
#150064=CARTESIAN_POINT('Ctrl Pts',(-17.9710104137728,-1.66525935159368,
1171.58298706047));
#150065=CARTESIAN_POINT('Ctrl Pts',(-18.1253194172301,-1.10985572039171E-15,
1170.08886941341));
#150066=CARTESIAN_POINT('Ctrl Pts',(-17.9710104137728,1.66525935159367,
1168.59475176635));
#150067=CARTESIAN_POINT('Ctrl Pts',(-17.8167014103155,3.33051870318735,
1167.10063411929));
#150068=CARTESIAN_POINT('Ctrl Pts',(-17.3590292079831,4.93906964482096,
1165.60651647223));
#150069=CARTESIAN_POINT('Ctrl Pts',(-16.9013570056506,6.54762058645456,
1164.11239882517));
#150070=CARTESIAN_POINT('Ctrl Pts',(-16.1559070823762,8.04468584505497,
1162.61828117811));
#150071=CARTESIAN_POINT('Ctrl Pts',(-15.4104571591017,9.54175110365538,
1161.12416353106));
#150072=CARTESIAN_POINT('Ctrl Pts',(-14.4026149179538,10.8763499173728,
1159.630045884));
#150073=CARTESIAN_POINT('Ctrl Pts',(-13.3947726768058,12.2109487310903,
1158.13592823694));
#150074=CARTESIAN_POINT('Ctrl Pts',(-12.1588589765331,13.3376329379985,
1156.64181058988));
#150075=CARTESIAN_POINT('Ctrl Pts',(-10.9229452762603,14.4643171449067,
1155.14769294282));
#150076=CARTESIAN_POINT('Ctrl Pts',(-9.50104767561052,15.3447188656481,
1153.65357529576));
#150077=CARTESIAN_POINT('Ctrl Pts',(-8.07915007496071,16.2251205863895,
1152.1594576487));
#150078=CARTESIAN_POINT('Ctrl Pts',(-6.51968959134574,16.8292587962898,
1150.66534000164));
#150079=CARTESIAN_POINT('Ctrl Pts',(-4.96022910773078,17.4333970061901,
1149.17122235458));
#150080=CARTESIAN_POINT('Ctrl Pts',(-3.31631129755346,17.7406985030951,
1147.67710470753));
#150081=CARTESIAN_POINT('Ctrl Pts',(-1.67239348737615,18.048,1146.18298706047));
#150082=CARTESIAN_POINT('Ctrl Pts',(-2.21024254310115E-15,18.048,1144.68886941341));
#150083=CARTESIAN_POINT('Ctrl Pts',(1.67239348737616,18.048,1143.19475176635));
#150084=CARTESIAN_POINT('Ctrl Pts',(3.31631129755346,17.7406985030951,1141.70063411929));
#150085=CARTESIAN_POINT('Ctrl Pts',(4.96022910773077,17.4333970061901,1140.20651647223));
#150086=CARTESIAN_POINT('Ctrl Pts',(6.51968959134575,16.8292587962898,1138.71239882517));
#150087=CARTESIAN_POINT('Ctrl Pts',(8.07915007496071,16.2251205863895,1137.21828117811));
#150088=CARTESIAN_POINT('Ctrl Pts',(9.50104767561053,15.3447188656481,1135.72416353105));
#150089=CARTESIAN_POINT('Ctrl Pts',(10.9229452762603,14.4643171449067,1134.230045884));
#150090=CARTESIAN_POINT('Ctrl Pts',(12.1588589765331,13.3376329379985,1132.73592823694));
#150091=CARTESIAN_POINT('Ctrl Pts',(13.3947726768058,12.2109487310903,1131.24181058988));
#150092=CARTESIAN_POINT('Ctrl Pts',(14.4026149179538,10.8763499173728,1129.74769294282));
#150093=CARTESIAN_POINT('Ctrl Pts',(15.4104571591017,9.54175110365539,1128.25357529576));
#150094=CARTESIAN_POINT('Ctrl Pts',(16.1559070823762,8.04468584505496,1126.7594576487));
#150095=CARTESIAN_POINT('Ctrl Pts',(16.9013570056506,6.54762058645456,1125.26534000164));
#150096=CARTESIAN_POINT('Ctrl Pts',(17.3590292079831,4.93906964482096,1123.77122235458));
#150097=CARTESIAN_POINT('Ctrl Pts',(17.8167014103155,3.33051870318735,1122.27710470753));
#150098=CARTESIAN_POINT('Ctrl Pts',(17.9710104137728,1.66525935159367,1120.78298706047));
#150099=CARTESIAN_POINT('Ctrl Pts',(18.1253194172301,3.32956716117513E-15,
1119.28886941341));
#150100=CARTESIAN_POINT('Ctrl Pts',(17.9710104137728,-1.66525935159367,
1117.79475176635));
#150101=CARTESIAN_POINT('Ctrl Pts',(17.8167014103155,-3.33051870318736,
1116.30063411929));
#150102=CARTESIAN_POINT('Ctrl Pts',(17.3590292079831,-4.93906964482095,
1114.80651647223));
#150103=CARTESIAN_POINT('Ctrl Pts',(16.9013570056506,-6.54762058645456,
1113.31239882517));
#150104=CARTESIAN_POINT('Ctrl Pts',(16.1559070823762,-8.04468584505497,
1111.81828117811));
#150105=CARTESIAN_POINT('Ctrl Pts',(15.4104571591017,-9.54175110365538,
1110.32416353105));
#150106=CARTESIAN_POINT('Ctrl Pts',(14.4026149179538,-10.8763499173728,
1108.830045884));
#150107=CARTESIAN_POINT('Ctrl Pts',(13.3947726768058,-12.2109487310903,
1107.33592823694));
#150108=CARTESIAN_POINT('Ctrl Pts',(12.1588589765331,-13.3376329379985,
1105.84181058988));
#150109=CARTESIAN_POINT('Ctrl Pts',(10.9229452762603,-14.4643171449067,
1104.34769294282));
#150110=CARTESIAN_POINT('Ctrl Pts',(9.50104767561053,-15.3447188656481,
1102.85357529576));
#150111=CARTESIAN_POINT('Ctrl Pts',(8.07915007496071,-16.2251205863895,
1101.3594576487));
#150112=CARTESIAN_POINT('Ctrl Pts',(6.51968959134574,-16.8292587962898,
1099.86534000164));
#150113=CARTESIAN_POINT('Ctrl Pts',(4.96022910773078,-17.4333970061901,
1098.37122235458));
#150114=CARTESIAN_POINT('Ctrl Pts',(3.31631129755346,-17.7406985030951,
1096.87710470753));
#150115=CARTESIAN_POINT('Ctrl Pts',(1.67239348737615,-18.048,1095.38298706047));
#150116=CARTESIAN_POINT('Ctrl Pts',(0.,-18.048,1093.88886941341));
#150117=CARTESIAN_POINT('Ctrl Pts',(-1.67239348737615,-18.048,1092.39475176635));
#150118=CARTESIAN_POINT('Ctrl Pts',(-3.31631129755346,-17.7406985030951,
1090.90063411929));
#150119=CARTESIAN_POINT('Ctrl Pts',(-4.96022910773077,-17.4333970061901,
1089.40651647223));
#150120=CARTESIAN_POINT('Ctrl Pts',(-6.51968959134574,-16.8292587962898,
1087.91239882517));
#150121=CARTESIAN_POINT('Ctrl Pts',(-8.07915007496071,-16.2251205863895,
1086.41828117811));
#150122=CARTESIAN_POINT('Ctrl Pts',(-9.50104767561052,-15.3447188656481,
1084.92416353106));
#150123=CARTESIAN_POINT('Ctrl Pts',(-10.9229452762603,-14.4643171449067,
1083.430045884));
#150124=CARTESIAN_POINT('Ctrl Pts',(-12.1588589765331,-13.3376329379985,
1081.93592823694));
#150125=CARTESIAN_POINT('Ctrl Pts',(-13.3947726768058,-12.2109487310903,
1080.44181058988));
#150126=CARTESIAN_POINT('Ctrl Pts',(-14.4026149179538,-10.8763499173728,
1078.94769294282));
#150127=CARTESIAN_POINT('Ctrl Pts',(-15.4104571591017,-9.54175110365538,
1077.45357529576));
#150128=CARTESIAN_POINT('Ctrl Pts',(-16.1559070823762,-8.04468584505497,
1075.9594576487));
#150129=CARTESIAN_POINT('Ctrl Pts',(-16.9013570056506,-6.54762058645456,
1074.46534000164));
#150130=CARTESIAN_POINT('Ctrl Pts',(-17.3590292079831,-4.93906964482095,
1072.97122235458));
#150131=CARTESIAN_POINT('Ctrl Pts',(-17.8167014103155,-3.33051870318735,
1071.47710470753));
#150132=CARTESIAN_POINT('Ctrl Pts',(-17.9710104137728,-1.66525935159368,
1069.98298706047));
#150133=CARTESIAN_POINT('Ctrl Pts',(-18.1253194172301,-1.10985572039171E-15,
1068.48886941341));
#150134=CARTESIAN_POINT('Ctrl Pts',(-17.9710104137728,1.66525935159367,
1066.99475176635));
#150135=CARTESIAN_POINT('Ctrl Pts',(-17.8167014103155,3.33051870318735,
1065.50063411929));
#150136=CARTESIAN_POINT('Ctrl Pts',(-17.3590292079831,4.93906964482096,
1064.00651647223));
#150137=CARTESIAN_POINT('Ctrl Pts',(-16.9013570056506,6.54762058645456,
1062.51239882517));
#150138=CARTESIAN_POINT('Ctrl Pts',(-16.1559070823762,8.04468584505497,
1061.01828117811));
#150139=CARTESIAN_POINT('Ctrl Pts',(-15.4104571591017,9.54175110365538,
1059.52416353105));
#150140=CARTESIAN_POINT('Ctrl Pts',(-14.4026149179538,10.8763499173728,
1058.030045884));
#150141=CARTESIAN_POINT('Ctrl Pts',(-13.3947726768058,12.2109487310903,
1056.53592823694));
#150142=CARTESIAN_POINT('Ctrl Pts',(-12.1588589765331,13.3376329379985,
1055.04181058988));
#150143=CARTESIAN_POINT('Ctrl Pts',(-10.9229452762603,14.4643171449067,
1053.54769294282));
#150144=CARTESIAN_POINT('Ctrl Pts',(-9.50104767561052,15.3447188656481,
1052.05357529576));
#150145=CARTESIAN_POINT('Ctrl Pts',(-8.07915007496071,16.2251205863895,
1050.5594576487));
#150146=CARTESIAN_POINT('Ctrl Pts',(-6.51968959134574,16.8292587962898,
1049.06534000164));
#150147=CARTESIAN_POINT('Ctrl Pts',(-4.96022910773078,17.4333970061901,
1047.57122235458));
#150148=CARTESIAN_POINT('Ctrl Pts',(-3.31631129755346,17.7406985030951,
1046.07710470753));
#150149=CARTESIAN_POINT('Ctrl Pts',(-1.67239348737615,18.048,1044.58298706047));
#150150=CARTESIAN_POINT('Ctrl Pts',(-2.21024254310115E-15,18.048,1043.08886941341));
#150151=CARTESIAN_POINT('Ctrl Pts',(1.67239348737616,18.048,1041.59475176635));
#150152=CARTESIAN_POINT('Ctrl Pts',(3.31631129755346,17.7406985030951,1040.10063411929));
#150153=CARTESIAN_POINT('Ctrl Pts',(4.96022910773077,17.4333970061901,1038.60651647223));
#150154=CARTESIAN_POINT('Ctrl Pts',(6.51968959134575,16.8292587962898,1037.11239882517));
#150155=CARTESIAN_POINT('Ctrl Pts',(8.07915007496071,16.2251205863895,1035.61828117811));
#150156=CARTESIAN_POINT('Ctrl Pts',(9.50104767561053,15.3447188656481,1034.12416353105));
#150157=CARTESIAN_POINT('Ctrl Pts',(10.9229452762603,14.4643171449067,1032.630045884));
#150158=CARTESIAN_POINT('Ctrl Pts',(12.1588589765331,13.3376329379985,1031.13592823694));
#150159=CARTESIAN_POINT('Ctrl Pts',(13.3947726768058,12.2109487310903,1029.64181058988));
#150160=CARTESIAN_POINT('Ctrl Pts',(14.4026149179538,10.8763499173728,1028.14769294282));
#150161=CARTESIAN_POINT('Ctrl Pts',(15.4104571591017,9.54175110365539,1026.65357529576));
#150162=CARTESIAN_POINT('Ctrl Pts',(16.1559070823762,8.04468584505496,1025.1594576487));
#150163=CARTESIAN_POINT('Ctrl Pts',(16.9013570056506,6.54762058645456,1023.66534000164));
#150164=CARTESIAN_POINT('Ctrl Pts',(17.3590292079831,4.93906964482096,1022.17122235458));
#150165=CARTESIAN_POINT('Ctrl Pts',(17.8167014103155,3.33051870318735,1020.67710470753));
#150166=CARTESIAN_POINT('Ctrl Pts',(17.9710104137728,1.66525935159367,1019.18298706047));
#150167=CARTESIAN_POINT('Ctrl Pts',(18.1253194172301,3.32956716117513E-15,
1017.68886941341));
#150168=CARTESIAN_POINT('Ctrl Pts',(17.9710104137728,-1.66525935159367,
1016.19475176635));
#150169=CARTESIAN_POINT('Ctrl Pts',(17.8167014103155,-3.33051870318736,
1014.70063411929));
#150170=CARTESIAN_POINT('Ctrl Pts',(17.3590292079831,-4.93906964482095,
1013.20651647223));
#150171=CARTESIAN_POINT('Ctrl Pts',(16.9013570056506,-6.54762058645456,
1011.71239882517));
#150172=CARTESIAN_POINT('Ctrl Pts',(16.1559070823762,-8.04468584505497,
1010.21828117811));
#150173=CARTESIAN_POINT('Ctrl Pts',(15.4104571591017,-9.54175110365538,
1008.72416353105));
#150174=CARTESIAN_POINT('Ctrl Pts',(14.4026149179538,-10.8763499173728,
1007.230045884));
#150175=CARTESIAN_POINT('Ctrl Pts',(13.3947726768058,-12.2109487310903,
1005.73592823694));
#150176=CARTESIAN_POINT('Ctrl Pts',(12.1588589765331,-13.3376329379985,
1004.24181058988));
#150177=CARTESIAN_POINT('Ctrl Pts',(10.9229452762603,-14.4643171449067,
1002.74769294282));
#150178=CARTESIAN_POINT('Ctrl Pts',(9.50104767561053,-15.3447188656481,
1001.25357529576));
#150179=CARTESIAN_POINT('Ctrl Pts',(8.07915007496071,-16.2251205863895,
999.759457648702));
#150180=CARTESIAN_POINT('Ctrl Pts',(6.51968959134574,-16.8292587962898,
998.265340001643));
#150181=CARTESIAN_POINT('Ctrl Pts',(4.96022910773078,-17.4333970061901,
996.771222354584));
#150182=CARTESIAN_POINT('Ctrl Pts',(3.31631129755346,-17.7406985030951,
995.277104707525));
#150183=CARTESIAN_POINT('Ctrl Pts',(1.67239348737615,-18.048,993.782987060467));
#150184=CARTESIAN_POINT('Ctrl Pts',(0.,-18.048,992.288869413408));
#150185=CARTESIAN_POINT('Ctrl Pts',(-1.67239348737615,-18.048,990.794751766349));
#150186=CARTESIAN_POINT('Ctrl Pts',(-3.31631129755346,-17.7406985030951,
989.30063411929));
#150187=CARTESIAN_POINT('Ctrl Pts',(-4.96022910773077,-17.4333970061901,
987.806516472231));
#150188=CARTESIAN_POINT('Ctrl Pts',(-6.51968959134574,-16.8292587962898,
986.312398825173));
#150189=CARTESIAN_POINT('Ctrl Pts',(-8.07915007496071,-16.2251205863895,
984.818281178114));
#150190=CARTESIAN_POINT('Ctrl Pts',(-9.50104767561052,-15.3447188656481,
983.324163531055));
#150191=CARTESIAN_POINT('Ctrl Pts',(-10.9229452762603,-14.4643171449067,
981.830045883996));
#150192=CARTESIAN_POINT('Ctrl Pts',(-12.1588589765331,-13.3376329379985,
980.335928236937));
#150193=CARTESIAN_POINT('Ctrl Pts',(-13.3947726768058,-12.2109487310903,
978.841810589878));
#150194=CARTESIAN_POINT('Ctrl Pts',(-14.4026149179538,-10.8763499173728,
977.34769294282));
#150195=CARTESIAN_POINT('Ctrl Pts',(-15.4104571591017,-9.54175110365538,
975.853575295761));
#150196=CARTESIAN_POINT('Ctrl Pts',(-16.1559070823762,-8.04468584505497,
974.359457648702));
#150197=CARTESIAN_POINT('Ctrl Pts',(-16.9013570056506,-6.54762058645456,
972.865340001643));
#150198=CARTESIAN_POINT('Ctrl Pts',(-17.3590292079831,-4.93906964482095,
971.371222354584));
#150199=CARTESIAN_POINT('Ctrl Pts',(-17.8167014103155,-3.33051870318735,
969.877104707525));
#150200=CARTESIAN_POINT('Ctrl Pts',(-17.9710104137728,-1.66525935159368,
968.382987060467));
#150201=CARTESIAN_POINT('Ctrl Pts',(-18.1253194172301,-1.10985572039171E-15,
966.888869413408));
#150202=CARTESIAN_POINT('Ctrl Pts',(-17.9710104137728,1.66525935159367,
965.394751766349));
#150203=CARTESIAN_POINT('Ctrl Pts',(-17.8167014103155,3.33051870318735,
963.90063411929));
#150204=CARTESIAN_POINT('Ctrl Pts',(-17.3590292079831,4.93906964482096,
962.406516472231));
#150205=CARTESIAN_POINT('Ctrl Pts',(-16.9013570056506,6.54762058645456,
960.912398825173));
#150206=CARTESIAN_POINT('Ctrl Pts',(-16.1559070823762,8.04468584505497,
959.418281178114));
#150207=CARTESIAN_POINT('Ctrl Pts',(-15.4104571591017,9.54175110365538,
957.924163531055));
#150208=CARTESIAN_POINT('Ctrl Pts',(-14.4026149179538,10.8763499173728,
956.430045883996));
#150209=CARTESIAN_POINT('Ctrl Pts',(-13.3947726768058,12.2109487310903,
954.935928236937));
#150210=CARTESIAN_POINT('Ctrl Pts',(-12.1588589765331,13.3376329379985,
953.441810589878));
#150211=CARTESIAN_POINT('Ctrl Pts',(-10.9229452762603,14.4643171449067,
951.94769294282));
#150212=CARTESIAN_POINT('Ctrl Pts',(-9.50104767561052,15.3447188656481,
950.453575295761));
#150213=CARTESIAN_POINT('Ctrl Pts',(-8.07915007496071,16.2251205863895,
948.959457648702));
#150214=CARTESIAN_POINT('Ctrl Pts',(-6.51968959134574,16.8292587962898,
947.465340001643));
#150215=CARTESIAN_POINT('Ctrl Pts',(-4.96022910773078,17.4333970061901,
945.971222354584));
#150216=CARTESIAN_POINT('Ctrl Pts',(-3.31631129755346,17.7406985030951,
944.477104707526));
#150217=CARTESIAN_POINT('Ctrl Pts',(-1.67239348737615,18.048,942.982987060467));
#150218=CARTESIAN_POINT('Ctrl Pts',(-2.21024254310115E-15,18.048,941.488869413408));
#150219=CARTESIAN_POINT('Ctrl Pts',(1.67239348737616,18.048,939.994751766349));
#150220=CARTESIAN_POINT('Ctrl Pts',(3.31631129755346,17.7406985030951,938.50063411929));
#150221=CARTESIAN_POINT('Ctrl Pts',(4.96022910773077,17.4333970061901,937.006516472231));
#150222=CARTESIAN_POINT('Ctrl Pts',(6.51968959134575,16.8292587962898,935.512398825173));
#150223=CARTESIAN_POINT('Ctrl Pts',(8.07915007496071,16.2251205863895,934.018281178114));
#150224=CARTESIAN_POINT('Ctrl Pts',(9.50104767561053,15.3447188656481,932.524163531055));
#150225=CARTESIAN_POINT('Ctrl Pts',(10.9229452762603,14.4643171449067,931.030045883996));
#150226=CARTESIAN_POINT('Ctrl Pts',(12.1588589765331,13.3376329379985,929.535928236937));
#150227=CARTESIAN_POINT('Ctrl Pts',(13.3947726768058,12.2109487310903,928.041810589879));
#150228=CARTESIAN_POINT('Ctrl Pts',(14.4026149179538,10.8763499173728,926.54769294282));
#150229=CARTESIAN_POINT('Ctrl Pts',(15.4104571591017,9.54175110365539,925.053575295761));
#150230=CARTESIAN_POINT('Ctrl Pts',(16.1559070823762,8.04468584505496,923.559457648702));
#150231=CARTESIAN_POINT('Ctrl Pts',(16.9013570056506,6.54762058645456,922.065340001643));
#150232=CARTESIAN_POINT('Ctrl Pts',(17.3590292079831,4.93906964482096,920.571222354584));
#150233=CARTESIAN_POINT('Ctrl Pts',(17.8167014103155,3.33051870318735,919.077104707525));
#150234=CARTESIAN_POINT('Ctrl Pts',(17.9710104137728,1.66525935159367,917.582987060467));
#150235=CARTESIAN_POINT('Ctrl Pts',(18.1253194172301,3.32956716117513E-15,
916.088869413408));
#150236=CARTESIAN_POINT('Ctrl Pts',(17.9710104137728,-1.66525935159367,
914.594751766349));
#150237=CARTESIAN_POINT('Ctrl Pts',(17.8167014103155,-3.33051870318736,
913.10063411929));
#150238=CARTESIAN_POINT('Ctrl Pts',(17.3590292079831,-4.93906964482095,
911.606516472231));
#150239=CARTESIAN_POINT('Ctrl Pts',(16.9013570056506,-6.54762058645456,
910.112398825173));
#150240=CARTESIAN_POINT('Ctrl Pts',(16.1559070823762,-8.04468584505497,
908.618281178114));
#150241=CARTESIAN_POINT('Ctrl Pts',(15.4104571591017,-9.54175110365538,
907.124163531055));
#150242=CARTESIAN_POINT('Ctrl Pts',(14.4026149179538,-10.8763499173728,
905.630045883996));
#150243=CARTESIAN_POINT('Ctrl Pts',(13.3947726768058,-12.2109487310903,
904.135928236937));
#150244=CARTESIAN_POINT('Ctrl Pts',(12.1588589765331,-13.3376329379985,
902.641810589878));
#150245=CARTESIAN_POINT('Ctrl Pts',(10.9229452762603,-14.4643171449067,
901.14769294282));
#150246=CARTESIAN_POINT('Ctrl Pts',(9.50104767561053,-15.3447188656481,
899.653575295761));
#150247=CARTESIAN_POINT('Ctrl Pts',(8.07915007496071,-16.2251205863895,
898.159457648702));
#150248=CARTESIAN_POINT('Ctrl Pts',(6.51968959134574,-16.8292587962898,
896.665340001643));
#150249=CARTESIAN_POINT('Ctrl Pts',(4.96022910773078,-17.4333970061901,
895.171222354584));
#150250=CARTESIAN_POINT('Ctrl Pts',(3.31631129755346,-17.7406985030951,
893.677104707526));
#150251=CARTESIAN_POINT('Ctrl Pts',(1.67239348737615,-18.048,892.182987060467));
#150252=CARTESIAN_POINT('Ctrl Pts',(0.,-18.048,890.688869413408));
#150253=CARTESIAN_POINT('Ctrl Pts',(-1.67239348737615,-18.048,889.194751766349));
#150254=CARTESIAN_POINT('Ctrl Pts',(-3.31631129755346,-17.7406985030951,
887.70063411929));
#150255=CARTESIAN_POINT('Ctrl Pts',(-4.96022910773077,-17.4333970061901,
886.206516472232));
#150256=CARTESIAN_POINT('Ctrl Pts',(-6.51968959134574,-16.8292587962898,
884.712398825172));
#150257=CARTESIAN_POINT('Ctrl Pts',(-8.07915007496071,-16.2251205863895,
883.218281178114));
#150258=CARTESIAN_POINT('Ctrl Pts',(-9.50104767561052,-15.3447188656481,
881.724163531055));
#150259=CARTESIAN_POINT('Ctrl Pts',(-10.9229452762603,-14.4643171449067,
880.230045883996));
#150260=CARTESIAN_POINT('Ctrl Pts',(-12.1588589765331,-13.3376329379985,
878.735928236937));
#150261=CARTESIAN_POINT('Ctrl Pts',(-13.3947726768058,-12.2109487310903,
877.241810589878));
#150262=CARTESIAN_POINT('Ctrl Pts',(-14.4026149179538,-10.8763499173728,
875.74769294282));
#150263=CARTESIAN_POINT('Ctrl Pts',(-15.4104571591017,-9.54175110365538,
874.253575295761));
#150264=CARTESIAN_POINT('Ctrl Pts',(-16.1559070823762,-8.04468584505497,
872.759457648702));
#150265=CARTESIAN_POINT('Ctrl Pts',(-16.9013570056506,-6.54762058645456,
871.265340001643));
#150266=CARTESIAN_POINT('Ctrl Pts',(-17.3590292079831,-4.93906964482095,
869.771222354584));
#150267=CARTESIAN_POINT('Ctrl Pts',(-17.8167014103155,-3.33051870318735,
868.277104707525));
#150268=CARTESIAN_POINT('Ctrl Pts',(-17.9710104137728,-1.66525935159368,
866.782987060467));
#150269=CARTESIAN_POINT('Ctrl Pts',(-18.1253194172301,-1.10985572039171E-15,
865.288869413408));
#150270=CARTESIAN_POINT('Ctrl Pts',(-17.9710104137728,1.66525935159367,
863.794751766349));
#150271=CARTESIAN_POINT('Ctrl Pts',(-17.8167014103155,3.33051870318735,
862.30063411929));
#150272=CARTESIAN_POINT('Ctrl Pts',(-17.3590292079831,4.93906964482096,
860.806516472231));
#150273=CARTESIAN_POINT('Ctrl Pts',(-16.9013570056506,6.54762058645456,
859.312398825173));
#150274=CARTESIAN_POINT('Ctrl Pts',(-16.1559070823762,8.04468584505497,
857.818281178114));
#150275=CARTESIAN_POINT('Ctrl Pts',(-15.4104571591017,9.54175110365538,
856.324163531055));
#150276=CARTESIAN_POINT('Ctrl Pts',(-14.4026149179538,10.8763499173728,
854.830045883996));
#150277=CARTESIAN_POINT('Ctrl Pts',(-13.3947726768058,12.2109487310903,
853.335928236937));
#150278=CARTESIAN_POINT('Ctrl Pts',(-12.1588589765331,13.3376329379985,
851.841810589878));
#150279=CARTESIAN_POINT('Ctrl Pts',(-10.9229452762603,14.4643171449067,
850.34769294282));
#150280=CARTESIAN_POINT('Ctrl Pts',(-9.50104767561052,15.3447188656481,
848.853575295761));
#150281=CARTESIAN_POINT('Ctrl Pts',(-8.07915007496071,16.2251205863895,
847.359457648702));
#150282=CARTESIAN_POINT('Ctrl Pts',(-6.51968959134574,16.8292587962898,
845.865340001643));
#150283=CARTESIAN_POINT('Ctrl Pts',(-4.96022910773078,17.4333970061901,
844.371222354584));
#150284=CARTESIAN_POINT('Ctrl Pts',(-3.31631129755346,17.7406985030951,
842.877104707525));
#150285=CARTESIAN_POINT('Ctrl Pts',(-1.67239348737615,18.048,841.382987060467));
#150286=CARTESIAN_POINT('Ctrl Pts',(-2.21024254310115E-15,18.048,839.888869413408));
#150287=CARTESIAN_POINT('Ctrl Pts',(1.67239348737616,18.048,838.394751766349));
#150288=CARTESIAN_POINT('Ctrl Pts',(3.31631129755346,17.7406985030951,836.90063411929));
#150289=CARTESIAN_POINT('Ctrl Pts',(4.96022910773077,17.4333970061901,835.406516472231));
#150290=CARTESIAN_POINT('Ctrl Pts',(6.51968959134575,16.8292587962898,833.912398825173));
#150291=CARTESIAN_POINT('Ctrl Pts',(8.07915007496071,16.2251205863895,832.418281178114));
#150292=CARTESIAN_POINT('Ctrl Pts',(9.50104767561053,15.3447188656481,830.924163531055));
#150293=CARTESIAN_POINT('Ctrl Pts',(10.9229452762603,14.4643171449067,829.430045883996));
#150294=CARTESIAN_POINT('Ctrl Pts',(12.1588589765331,13.3376329379985,827.935928236937));
#150295=CARTESIAN_POINT('Ctrl Pts',(13.3947726768058,12.2109487310903,826.441810589879));
#150296=CARTESIAN_POINT('Ctrl Pts',(14.4026149179538,10.8763499173728,824.94769294282));
#150297=CARTESIAN_POINT('Ctrl Pts',(15.4104571591017,9.54175110365539,823.453575295761));
#150298=CARTESIAN_POINT('Ctrl Pts',(16.1559070823762,8.04468584505496,821.959457648702));
#150299=CARTESIAN_POINT('Ctrl Pts',(16.9013570056506,6.54762058645456,820.465340001643));
#150300=CARTESIAN_POINT('Ctrl Pts',(17.3590292079831,4.93906964482096,818.971222354584));
#150301=CARTESIAN_POINT('Ctrl Pts',(17.8167014103155,3.33051870318735,817.477104707526));
#150302=CARTESIAN_POINT('Ctrl Pts',(17.9710104137728,1.66525935159367,815.982987060467));
#150303=CARTESIAN_POINT('Ctrl Pts',(18.1253194172301,3.32956716117513E-15,
814.488869413408));
#150304=CARTESIAN_POINT('Ctrl Pts',(17.9710104137728,-1.66525935159367,
812.994751766349));
#150305=CARTESIAN_POINT('Ctrl Pts',(17.8167014103155,-3.33051870318736,
811.50063411929));
#150306=CARTESIAN_POINT('Ctrl Pts',(17.3590292079831,-4.93906964482095,
810.006516472231));
#150307=CARTESIAN_POINT('Ctrl Pts',(16.9013570056506,-6.54762058645456,
808.512398825172));
#150308=CARTESIAN_POINT('Ctrl Pts',(16.1559070823762,-8.04468584505497,
807.018281178114));
#150309=CARTESIAN_POINT('Ctrl Pts',(15.4104571591017,-9.54175110365538,
805.524163531055));
#150310=CARTESIAN_POINT('Ctrl Pts',(14.4026149179538,-10.8763499173728,
804.030045883996));
#150311=CARTESIAN_POINT('Ctrl Pts',(13.3947726768058,-12.2109487310903,
802.535928236937));
#150312=CARTESIAN_POINT('Ctrl Pts',(12.1588589765331,-13.3376329379985,
801.041810589878));
#150313=CARTESIAN_POINT('Ctrl Pts',(10.9229452762603,-14.4643171449067,
799.54769294282));
#150314=CARTESIAN_POINT('Ctrl Pts',(9.50104767561053,-15.3447188656481,
798.053575295761));
#150315=CARTESIAN_POINT('Ctrl Pts',(8.07915007496071,-16.2251205863895,
796.559457648702));
#150316=CARTESIAN_POINT('Ctrl Pts',(6.51968959134574,-16.8292587962898,
795.065340001643));
#150317=CARTESIAN_POINT('Ctrl Pts',(4.96022910773078,-17.4333970061901,
793.571222354584));
#150318=CARTESIAN_POINT('Ctrl Pts',(3.31631129755346,-17.7406985030951,
792.077104707525));
#150319=CARTESIAN_POINT('Ctrl Pts',(1.67239348737615,-18.048,790.582987060467));
#150320=CARTESIAN_POINT('Ctrl Pts',(0.,-18.048,789.088869413408));
#150321=CARTESIAN_POINT('Ctrl Pts',(-1.67239348737615,-18.048,787.594751766349));
#150322=CARTESIAN_POINT('Ctrl Pts',(-3.31631129755346,-17.7406985030951,
786.10063411929));
#150323=CARTESIAN_POINT('Ctrl Pts',(-4.96022910773077,-17.4333970061901,
784.606516472231));
#150324=CARTESIAN_POINT('Ctrl Pts',(-6.51968959134574,-16.8292587962898,
783.112398825173));
#150325=CARTESIAN_POINT('Ctrl Pts',(-8.07915007496071,-16.2251205863895,
781.618281178114));
#150326=CARTESIAN_POINT('Ctrl Pts',(-9.50104767561052,-15.3447188656481,
780.124163531055));
#150327=CARTESIAN_POINT('Ctrl Pts',(-10.9229452762603,-14.4643171449067,
778.630045883996));
#150328=CARTESIAN_POINT('Ctrl Pts',(-12.1588589765331,-13.3376329379985,
777.135928236937));
#150329=CARTESIAN_POINT('Ctrl Pts',(-13.3947726768058,-12.2109487310903,
775.641810589879));
#150330=CARTESIAN_POINT('Ctrl Pts',(-14.4026149179538,-10.8763499173728,
774.14769294282));
#150331=CARTESIAN_POINT('Ctrl Pts',(-15.4104571591017,-9.54175110365538,
772.653575295761));
#150332=CARTESIAN_POINT('Ctrl Pts',(-16.1559070823762,-8.04468584505497,
771.159457648702));
#150333=CARTESIAN_POINT('Ctrl Pts',(-16.9013570056506,-6.54762058645456,
769.665340001643));
#150334=CARTESIAN_POINT('Ctrl Pts',(-17.3590292079831,-4.93906964482095,
768.171222354584));
#150335=CARTESIAN_POINT('Ctrl Pts',(-17.8167014103155,-3.33051870318735,
766.677104707526));
#150336=CARTESIAN_POINT('Ctrl Pts',(-17.9710104137728,-1.66525935159368,
765.182987060467));
#150337=CARTESIAN_POINT('Ctrl Pts',(-18.1253194172301,-1.10985572039171E-15,
763.688869413408));
#150338=CARTESIAN_POINT('Ctrl Pts',(-17.9710104137728,1.66525935159367,
762.194751766349));
#150339=CARTESIAN_POINT('Ctrl Pts',(-17.8167014103155,3.33051870318735,
760.70063411929));
#150340=CARTESIAN_POINT('Ctrl Pts',(-17.3590292079831,4.93906964482096,
759.206516472231));
#150341=CARTESIAN_POINT('Ctrl Pts',(-16.9013570056506,6.54762058645456,
757.712398825172));
#150342=CARTESIAN_POINT('Ctrl Pts',(-16.1559070823762,8.04468584505497,
756.218281178114));
#150343=CARTESIAN_POINT('Ctrl Pts',(-15.4104571591017,9.54175110365538,
754.724163531055));
#150344=CARTESIAN_POINT('Ctrl Pts',(-14.4026149179538,10.8763499173728,
753.230045883996));
#150345=CARTESIAN_POINT('Ctrl Pts',(-13.3947726768058,12.2109487310903,
751.735928236937));
#150346=CARTESIAN_POINT('Ctrl Pts',(-12.1588589765331,13.3376329379985,
750.241810589878));
#150347=CARTESIAN_POINT('Ctrl Pts',(-10.9229452762603,14.4643171449067,
748.74769294282));
#150348=CARTESIAN_POINT('Ctrl Pts',(-9.50104767561052,15.3447188656481,
747.253575295761));
#150349=CARTESIAN_POINT('Ctrl Pts',(-8.07915007496071,16.2251205863895,
745.759457648702));
#150350=CARTESIAN_POINT('Ctrl Pts',(-6.51968959134574,16.8292587962898,
744.265340001643));
#150351=CARTESIAN_POINT('Ctrl Pts',(-4.96022910773078,17.4333970061901,
742.771222354584));
#150352=CARTESIAN_POINT('Ctrl Pts',(-3.31631129755346,17.7406985030951,
741.277104707525));
#150353=CARTESIAN_POINT('Ctrl Pts',(-1.67239348737615,18.048,739.782987060467));
#150354=CARTESIAN_POINT('Ctrl Pts',(-2.21024254310115E-15,18.048,738.288869413408));
#150355=CARTESIAN_POINT('Ctrl Pts',(1.67239348737616,18.048,736.794751766349));
#150356=CARTESIAN_POINT('Ctrl Pts',(3.31631129755346,17.7406985030951,735.30063411929));
#150357=CARTESIAN_POINT('Ctrl Pts',(4.96022910773077,17.4333970061901,733.806516472231));
#150358=CARTESIAN_POINT('Ctrl Pts',(6.51968959134575,16.8292587962898,732.312398825173));
#150359=CARTESIAN_POINT('Ctrl Pts',(8.07915007496071,16.2251205863895,730.818281178114));
#150360=CARTESIAN_POINT('Ctrl Pts',(9.50104767561053,15.3447188656481,729.324163531055));
#150361=CARTESIAN_POINT('Ctrl Pts',(10.9229452762603,14.4643171449067,727.830045883996));
#150362=CARTESIAN_POINT('Ctrl Pts',(12.1588589765331,13.3376329379985,726.335928236937));
#150363=CARTESIAN_POINT('Ctrl Pts',(13.3947726768058,12.2109487310903,724.841810589879));
#150364=CARTESIAN_POINT('Ctrl Pts',(14.4026149179538,10.8763499173728,723.34769294282));
#150365=CARTESIAN_POINT('Ctrl Pts',(15.4104571591017,9.54175110365539,721.853575295761));
#150366=CARTESIAN_POINT('Ctrl Pts',(16.1559070823762,8.04468584505496,720.359457648702));
#150367=CARTESIAN_POINT('Ctrl Pts',(16.9013570056506,6.54762058645456,718.865340001643));
#150368=CARTESIAN_POINT('Ctrl Pts',(17.3590292079831,4.93906964482096,717.371222354584));
#150369=CARTESIAN_POINT('Ctrl Pts',(17.8167014103155,3.33051870318735,715.877104707526));
#150370=CARTESIAN_POINT('Ctrl Pts',(17.9710104137728,1.66525935159367,714.382987060467));
#150371=CARTESIAN_POINT('Ctrl Pts',(18.1253194172301,3.32956716117513E-15,
712.888869413408));
#150372=CARTESIAN_POINT('Ctrl Pts',(17.9710104137728,-1.66525935159367,
711.394751766349));
#150373=CARTESIAN_POINT('Ctrl Pts',(17.8167014103155,-3.33051870318736,
709.90063411929));
#150374=CARTESIAN_POINT('Ctrl Pts',(17.3590292079831,-4.93906964482095,
708.406516472231));
#150375=CARTESIAN_POINT('Ctrl Pts',(16.9013570056506,-6.54762058645456,
706.912398825173));
#150376=CARTESIAN_POINT('Ctrl Pts',(16.1559070823762,-8.04468584505497,
705.418281178114));
#150377=CARTESIAN_POINT('Ctrl Pts',(15.4104571591017,-9.54175110365538,
703.924163531055));
#150378=CARTESIAN_POINT('Ctrl Pts',(14.4026149179538,-10.8763499173728,
702.430045883996));
#150379=CARTESIAN_POINT('Ctrl Pts',(13.3947726768058,-12.2109487310903,
700.935928236937));
#150380=CARTESIAN_POINT('Ctrl Pts',(12.1588589765331,-13.3376329379985,
699.441810589878));
#150381=CARTESIAN_POINT('Ctrl Pts',(10.9229452762603,-14.4643171449067,
697.94769294282));
#150382=CARTESIAN_POINT('Ctrl Pts',(9.50104767561053,-15.3447188656481,
696.453575295761));
#150383=CARTESIAN_POINT('Ctrl Pts',(8.07915007496071,-16.2251205863895,
694.959457648702));
#150384=CARTESIAN_POINT('Ctrl Pts',(6.51968959134574,-16.8292587962898,
693.465340001643));
#150385=CARTESIAN_POINT('Ctrl Pts',(5.75661139047343,-17.1248768662138,
692.734235483133));
#150386=CARTESIAN_POINT('Ctrl Pts',(4.96991138555256,-17.3502243449402,
692.));
#150387=CARTESIAN_POINT('',(0.,-39.,1500.98568435754));
#150388=CARTESIAN_POINT('Ctrl Pts',(0.,-18.048,1504.84863058659));
#150389=CARTESIAN_POINT('Ctrl Pts',(-1.67239348737615,-18.048,1503.35451293953));
#150390=CARTESIAN_POINT('Ctrl Pts',(-3.31631129755346,-17.7406985030951,
1501.86039529247));
#150391=CARTESIAN_POINT('Ctrl Pts',(-4.96022910773077,-17.4333970061901,
1500.36627764542));
#150392=CARTESIAN_POINT('Ctrl Pts',(-6.51968959134574,-16.8292587962898,
1498.87215999836));
#150393=CARTESIAN_POINT('Ctrl Pts',(-8.07915007496071,-16.2251205863895,
1497.3780423513));
#150394=CARTESIAN_POINT('Ctrl Pts',(-9.50104767561052,-15.3447188656481,
1495.88392470424));
#150395=CARTESIAN_POINT('Ctrl Pts',(-10.9229452762603,-14.4643171449067,
1494.38980705718));
#150396=CARTESIAN_POINT('Ctrl Pts',(-12.1588589765331,-13.3376329379985,
1492.89568941012));
#150397=CARTESIAN_POINT('Ctrl Pts',(-13.3947726768058,-12.2109487310903,
1491.40157176306));
#150398=CARTESIAN_POINT('Ctrl Pts',(-14.4026149179538,-10.8763499173728,
1489.907454116));
#150399=CARTESIAN_POINT('Ctrl Pts',(-15.4104571591017,-9.54175110365538,
1488.41333646895));
#150400=CARTESIAN_POINT('Ctrl Pts',(-16.1559070823762,-8.04468584505497,
1486.91921882189));
#150401=CARTESIAN_POINT('Ctrl Pts',(-16.9013570056506,-6.54762058645456,
1485.42510117483));
#150402=CARTESIAN_POINT('Ctrl Pts',(-17.3590292079831,-4.93906964482095,
1483.93098352777));
#150403=CARTESIAN_POINT('Ctrl Pts',(-17.8167014103155,-3.33051870318735,
1482.43686588071));
#150404=CARTESIAN_POINT('Ctrl Pts',(-17.9710104137728,-1.66525935159368,
1480.94274823365));
#150405=CARTESIAN_POINT('Ctrl Pts',(-18.1253194172301,-1.10985572039171E-15,
1479.44863058659));
#150406=CARTESIAN_POINT('Ctrl Pts',(-17.9710104137728,1.66525935159367,
1477.95451293953));
#150407=CARTESIAN_POINT('Ctrl Pts',(-17.8167014103155,3.33051870318735,
1476.46039529247));
#150408=CARTESIAN_POINT('Ctrl Pts',(-17.3590292079831,4.93906964482096,
1474.96627764542));
#150409=CARTESIAN_POINT('Ctrl Pts',(-16.9013570056506,6.54762058645456,
1473.47215999836));
#150410=CARTESIAN_POINT('Ctrl Pts',(-16.1559070823762,8.04468584505497,
1471.9780423513));
#150411=CARTESIAN_POINT('Ctrl Pts',(-15.4104571591017,9.54175110365538,
1470.48392470424));
#150412=CARTESIAN_POINT('Ctrl Pts',(-14.4026149179538,10.8763499173728,
1468.98980705718));
#150413=CARTESIAN_POINT('Ctrl Pts',(-13.3947726768058,12.2109487310903,
1467.49568941012));
#150414=CARTESIAN_POINT('Ctrl Pts',(-12.1588589765331,13.3376329379985,
1466.00157176306));
#150415=CARTESIAN_POINT('Ctrl Pts',(-10.9229452762603,14.4643171449067,
1464.507454116));
#150416=CARTESIAN_POINT('Ctrl Pts',(-9.50104767561052,15.3447188656481,
1463.01333646895));
#150417=CARTESIAN_POINT('Ctrl Pts',(-8.07915007496071,16.2251205863895,
1461.51921882189));
#150418=CARTESIAN_POINT('Ctrl Pts',(-6.51968959134574,16.8292587962898,
1460.02510117483));
#150419=CARTESIAN_POINT('Ctrl Pts',(-4.96022910773078,17.4333970061901,
1458.53098352777));
#150420=CARTESIAN_POINT('Ctrl Pts',(-3.31631129755346,17.7406985030951,
1457.03686588071));
#150421=CARTESIAN_POINT('Ctrl Pts',(-1.67239348737615,18.048,1455.54274823365));
#150422=CARTESIAN_POINT('Ctrl Pts',(-2.21024254310115E-15,18.048,1454.04863058659));
#150423=CARTESIAN_POINT('Ctrl Pts',(1.67239348737616,18.048,1452.55451293953));
#150424=CARTESIAN_POINT('Ctrl Pts',(3.31631129755346,17.7406985030951,1451.06039529247));
#150425=CARTESIAN_POINT('Ctrl Pts',(4.96022910773077,17.4333970061901,1449.56627764542));
#150426=CARTESIAN_POINT('Ctrl Pts',(6.51968959134575,16.8292587962898,1448.07215999836));
#150427=CARTESIAN_POINT('Ctrl Pts',(8.07915007496071,16.2251205863895,1446.5780423513));
#150428=CARTESIAN_POINT('Ctrl Pts',(9.50104767561053,15.3447188656481,1445.08392470424));
#150429=CARTESIAN_POINT('Ctrl Pts',(10.9229452762603,14.4643171449067,1443.58980705718));
#150430=CARTESIAN_POINT('Ctrl Pts',(12.1588589765331,13.3376329379985,1442.09568941012));
#150431=CARTESIAN_POINT('Ctrl Pts',(13.3947726768058,12.2109487310903,1440.60157176306));
#150432=CARTESIAN_POINT('Ctrl Pts',(14.4026149179538,10.8763499173728,1439.107454116));
#150433=CARTESIAN_POINT('Ctrl Pts',(15.4104571591017,9.54175110365538,1437.61333646895));
#150434=CARTESIAN_POINT('Ctrl Pts',(16.1559070823762,8.04468584505496,1436.11921882189));
#150435=CARTESIAN_POINT('Ctrl Pts',(16.9013570056506,6.54762058645456,1434.62510117483));
#150436=CARTESIAN_POINT('Ctrl Pts',(17.3590292079831,4.93906964482096,1433.13098352777));
#150437=CARTESIAN_POINT('Ctrl Pts',(17.8167014103155,3.33051870318735,1431.63686588071));
#150438=CARTESIAN_POINT('Ctrl Pts',(17.9710104137728,1.66525935159367,1430.14274823365));
#150439=CARTESIAN_POINT('Ctrl Pts',(18.1253194172301,3.32956716117513E-15,
1428.64863058659));
#150440=CARTESIAN_POINT('Ctrl Pts',(17.9710104137728,-1.66525935159367,
1427.15451293953));
#150441=CARTESIAN_POINT('Ctrl Pts',(17.8167014103155,-3.33051870318736,
1425.66039529247));
#150442=CARTESIAN_POINT('Ctrl Pts',(17.3590292079831,-4.93906964482095,
1424.16627764542));
#150443=CARTESIAN_POINT('Ctrl Pts',(16.9013570056506,-6.54762058645456,
1422.67215999836));
#150444=CARTESIAN_POINT('Ctrl Pts',(16.1559070823762,-8.04468584505497,
1421.1780423513));
#150445=CARTESIAN_POINT('Ctrl Pts',(15.4104571591017,-9.54175110365538,
1419.68392470424));
#150446=CARTESIAN_POINT('Ctrl Pts',(14.4026149179538,-10.8763499173728,
1418.18980705718));
#150447=CARTESIAN_POINT('Ctrl Pts',(13.3947726768058,-12.2109487310903,
1416.69568941012));
#150448=CARTESIAN_POINT('Ctrl Pts',(12.1588589765331,-13.3376329379985,
1415.20157176306));
#150449=CARTESIAN_POINT('Ctrl Pts',(10.9229452762603,-14.4643171449067,
1413.707454116));
#150450=CARTESIAN_POINT('Ctrl Pts',(9.50104767561053,-15.3447188656481,
1412.21333646895));
#150451=CARTESIAN_POINT('Ctrl Pts',(8.07915007496071,-16.2251205863895,
1410.71921882189));
#150452=CARTESIAN_POINT('Ctrl Pts',(6.51968959134574,-16.8292587962898,
1409.22510117483));
#150453=CARTESIAN_POINT('Ctrl Pts',(4.96022910773078,-17.4333970061901,
1407.73098352777));
#150454=CARTESIAN_POINT('Ctrl Pts',(3.31631129755346,-17.7406985030951,
1406.23686588071));
#150455=CARTESIAN_POINT('Ctrl Pts',(1.67239348737615,-18.048,1404.74274823365));
#150456=CARTESIAN_POINT('Ctrl Pts',(0.,-18.048,1403.24863058659));
#150457=CARTESIAN_POINT('Ctrl Pts',(-1.67239348737615,-18.048,1401.75451293953));
#150458=CARTESIAN_POINT('Ctrl Pts',(-3.31631129755346,-17.7406985030951,
1400.26039529247));
#150459=CARTESIAN_POINT('Ctrl Pts',(-4.96022910773077,-17.4333970061901,
1398.76627764542));
#150460=CARTESIAN_POINT('Ctrl Pts',(-6.51968959134574,-16.8292587962898,
1397.27215999836));
#150461=CARTESIAN_POINT('Ctrl Pts',(-8.07915007496071,-16.2251205863895,
1395.7780423513));
#150462=CARTESIAN_POINT('Ctrl Pts',(-9.50104767561052,-15.3447188656481,
1394.28392470424));
#150463=CARTESIAN_POINT('Ctrl Pts',(-10.9229452762603,-14.4643171449067,
1392.78980705718));
#150464=CARTESIAN_POINT('Ctrl Pts',(-12.1588589765331,-13.3376329379985,
1391.29568941012));
#150465=CARTESIAN_POINT('Ctrl Pts',(-13.3947726768058,-12.2109487310903,
1389.80157176306));
#150466=CARTESIAN_POINT('Ctrl Pts',(-14.4026149179538,-10.8763499173728,
1388.307454116));
#150467=CARTESIAN_POINT('Ctrl Pts',(-15.4104571591017,-9.54175110365538,
1386.81333646895));
#150468=CARTESIAN_POINT('Ctrl Pts',(-16.1559070823762,-8.04468584505497,
1385.31921882189));
#150469=CARTESIAN_POINT('Ctrl Pts',(-16.9013570056506,-6.54762058645456,
1383.82510117483));
#150470=CARTESIAN_POINT('Ctrl Pts',(-17.3590292079831,-4.93906964482095,
1382.33098352777));
#150471=CARTESIAN_POINT('Ctrl Pts',(-17.8167014103155,-3.33051870318735,
1380.83686588071));
#150472=CARTESIAN_POINT('Ctrl Pts',(-17.9710104137728,-1.66525935159368,
1379.34274823365));
#150473=CARTESIAN_POINT('Ctrl Pts',(-18.1253194172301,-1.10985572039171E-15,
1377.84863058659));
#150474=CARTESIAN_POINT('Ctrl Pts',(-17.9710104137728,1.66525935159367,
1376.35451293953));
#150475=CARTESIAN_POINT('Ctrl Pts',(-17.8167014103155,3.33051870318735,
1374.86039529247));
#150476=CARTESIAN_POINT('Ctrl Pts',(-17.3590292079831,4.93906964482096,
1373.36627764542));
#150477=CARTESIAN_POINT('Ctrl Pts',(-16.9013570056506,6.54762058645456,
1371.87215999836));
#150478=CARTESIAN_POINT('Ctrl Pts',(-16.1559070823762,8.04468584505497,
1370.3780423513));
#150479=CARTESIAN_POINT('Ctrl Pts',(-15.4104571591017,9.54175110365538,
1368.88392470424));
#150480=CARTESIAN_POINT('Ctrl Pts',(-14.4026149179538,10.8763499173728,
1367.38980705718));
#150481=CARTESIAN_POINT('Ctrl Pts',(-13.3947726768058,12.2109487310903,
1365.89568941012));
#150482=CARTESIAN_POINT('Ctrl Pts',(-12.1588589765331,13.3376329379985,
1364.40157176306));
#150483=CARTESIAN_POINT('Ctrl Pts',(-10.9229452762603,14.4643171449067,
1362.907454116));
#150484=CARTESIAN_POINT('Ctrl Pts',(-9.50104767561052,15.3447188656481,
1361.41333646895));
#150485=CARTESIAN_POINT('Ctrl Pts',(-8.07915007496071,16.2251205863895,
1359.91921882189));
#150486=CARTESIAN_POINT('Ctrl Pts',(-6.51968959134574,16.8292587962898,
1358.42510117483));
#150487=CARTESIAN_POINT('Ctrl Pts',(-4.96022910773078,17.4333970061901,
1356.93098352777));
#150488=CARTESIAN_POINT('Ctrl Pts',(-3.31631129755346,17.7406985030951,
1355.43686588071));
#150489=CARTESIAN_POINT('Ctrl Pts',(-1.67239348737615,18.048,1353.94274823365));
#150490=CARTESIAN_POINT('Ctrl Pts',(-2.21024254310115E-15,18.048,1352.44863058659));
#150491=CARTESIAN_POINT('Ctrl Pts',(1.67239348737616,18.048,1350.95451293953));
#150492=CARTESIAN_POINT('Ctrl Pts',(3.31631129755346,17.7406985030951,1349.46039529247));
#150493=CARTESIAN_POINT('Ctrl Pts',(4.96022910773077,17.4333970061901,1347.96627764542));
#150494=CARTESIAN_POINT('Ctrl Pts',(6.51968959134575,16.8292587962898,1346.47215999836));
#150495=CARTESIAN_POINT('Ctrl Pts',(8.07915007496071,16.2251205863895,1344.9780423513));
#150496=CARTESIAN_POINT('Ctrl Pts',(9.50104767561053,15.3447188656481,1343.48392470424));
#150497=CARTESIAN_POINT('Ctrl Pts',(10.9229452762603,14.4643171449067,1341.98980705718));
#150498=CARTESIAN_POINT('Ctrl Pts',(12.1588589765331,13.3376329379985,1340.49568941012));
#150499=CARTESIAN_POINT('Ctrl Pts',(13.3947726768058,12.2109487310903,1339.00157176306));
#150500=CARTESIAN_POINT('Ctrl Pts',(14.4026149179538,10.8763499173728,1337.507454116));
#150501=CARTESIAN_POINT('Ctrl Pts',(15.4104571591017,9.54175110365538,1336.01333646895));
#150502=CARTESIAN_POINT('Ctrl Pts',(16.1559070823762,8.04468584505496,1334.51921882189));
#150503=CARTESIAN_POINT('Ctrl Pts',(16.9013570056506,6.54762058645456,1333.02510117483));
#150504=CARTESIAN_POINT('Ctrl Pts',(17.3590292079831,4.93906964482096,1331.53098352777));
#150505=CARTESIAN_POINT('Ctrl Pts',(17.8167014103155,3.33051870318735,1330.03686588071));
#150506=CARTESIAN_POINT('Ctrl Pts',(17.9710104137728,1.66525935159367,1328.54274823365));
#150507=CARTESIAN_POINT('Ctrl Pts',(18.1253194172301,3.32956716117513E-15,
1327.04863058659));
#150508=CARTESIAN_POINT('Ctrl Pts',(17.9710104137728,-1.66525935159367,
1325.55451293953));
#150509=CARTESIAN_POINT('Ctrl Pts',(17.8167014103155,-3.33051870318736,
1324.06039529247));
#150510=CARTESIAN_POINT('Ctrl Pts',(17.3590292079831,-4.93906964482095,
1322.56627764542));
#150511=CARTESIAN_POINT('Ctrl Pts',(16.9013570056506,-6.54762058645456,
1321.07215999836));
#150512=CARTESIAN_POINT('Ctrl Pts',(16.1559070823762,-8.04468584505497,
1319.5780423513));
#150513=CARTESIAN_POINT('Ctrl Pts',(15.4104571591017,-9.54175110365538,
1318.08392470424));
#150514=CARTESIAN_POINT('Ctrl Pts',(14.4026149179538,-10.8763499173728,
1316.58980705718));
#150515=CARTESIAN_POINT('Ctrl Pts',(13.3947726768058,-12.2109487310903,
1315.09568941012));
#150516=CARTESIAN_POINT('Ctrl Pts',(12.1588589765331,-13.3376329379985,
1313.60157176306));
#150517=CARTESIAN_POINT('Ctrl Pts',(10.9229452762603,-14.4643171449067,
1312.107454116));
#150518=CARTESIAN_POINT('Ctrl Pts',(9.50104767561053,-15.3447188656481,
1310.61333646895));
#150519=CARTESIAN_POINT('Ctrl Pts',(8.07915007496071,-16.2251205863895,
1309.11921882189));
#150520=CARTESIAN_POINT('Ctrl Pts',(6.51968959134574,-16.8292587962898,
1307.62510117483));
#150521=CARTESIAN_POINT('Ctrl Pts',(4.96022910773078,-17.4333970061901,
1306.13098352777));
#150522=CARTESIAN_POINT('Ctrl Pts',(3.31631129755346,-17.7406985030951,
1304.63686588071));
#150523=CARTESIAN_POINT('Ctrl Pts',(1.67239348737615,-18.048,1303.14274823365));
#150524=CARTESIAN_POINT('Ctrl Pts',(0.,-18.048,1301.64863058659));
#150525=CARTESIAN_POINT('Ctrl Pts',(-1.67239348737615,-18.048,1300.15451293953));
#150526=CARTESIAN_POINT('Ctrl Pts',(-3.31631129755346,-17.7406985030951,
1298.66039529247));
#150527=CARTESIAN_POINT('Ctrl Pts',(-4.96022910773077,-17.4333970061901,
1297.16627764542));
#150528=CARTESIAN_POINT('Ctrl Pts',(-6.51968959134574,-16.8292587962898,
1295.67215999836));
#150529=CARTESIAN_POINT('Ctrl Pts',(-8.07915007496071,-16.2251205863895,
1294.1780423513));
#150530=CARTESIAN_POINT('Ctrl Pts',(-9.50104767561052,-15.3447188656481,
1292.68392470424));
#150531=CARTESIAN_POINT('Ctrl Pts',(-10.9229452762603,-14.4643171449067,
1291.18980705718));
#150532=CARTESIAN_POINT('Ctrl Pts',(-12.1588589765331,-13.3376329379985,
1289.69568941012));
#150533=CARTESIAN_POINT('Ctrl Pts',(-13.3947726768058,-12.2109487310903,
1288.20157176306));
#150534=CARTESIAN_POINT('Ctrl Pts',(-14.4026149179538,-10.8763499173728,
1286.707454116));
#150535=CARTESIAN_POINT('Ctrl Pts',(-15.4104571591017,-9.54175110365538,
1285.21333646895));
#150536=CARTESIAN_POINT('Ctrl Pts',(-16.1559070823762,-8.04468584505497,
1283.71921882189));
#150537=CARTESIAN_POINT('Ctrl Pts',(-16.9013570056506,-6.54762058645456,
1282.22510117483));
#150538=CARTESIAN_POINT('Ctrl Pts',(-17.3590292079831,-4.93906964482095,
1280.73098352777));
#150539=CARTESIAN_POINT('Ctrl Pts',(-17.8167014103155,-3.33051870318735,
1279.23686588071));
#150540=CARTESIAN_POINT('Ctrl Pts',(-17.9710104137728,-1.66525935159368,
1277.74274823365));
#150541=CARTESIAN_POINT('Ctrl Pts',(-18.1253194172301,-1.10985572039171E-15,
1276.24863058659));
#150542=CARTESIAN_POINT('Ctrl Pts',(-17.9710104137728,1.66525935159367,
1274.75451293953));
#150543=CARTESIAN_POINT('Ctrl Pts',(-17.8167014103155,3.33051870318735,
1273.26039529247));
#150544=CARTESIAN_POINT('Ctrl Pts',(-17.3590292079831,4.93906964482096,
1271.76627764542));
#150545=CARTESIAN_POINT('Ctrl Pts',(-16.9013570056506,6.54762058645456,
1270.27215999836));
#150546=CARTESIAN_POINT('Ctrl Pts',(-16.1559070823762,8.04468584505497,
1268.7780423513));
#150547=CARTESIAN_POINT('Ctrl Pts',(-15.4104571591017,9.54175110365538,
1267.28392470424));
#150548=CARTESIAN_POINT('Ctrl Pts',(-14.4026149179538,10.8763499173728,
1265.78980705718));
#150549=CARTESIAN_POINT('Ctrl Pts',(-13.3947726768058,12.2109487310903,
1264.29568941012));
#150550=CARTESIAN_POINT('Ctrl Pts',(-12.1588589765331,13.3376329379985,
1262.80157176306));
#150551=CARTESIAN_POINT('Ctrl Pts',(-10.9229452762603,14.4643171449067,
1261.307454116));
#150552=CARTESIAN_POINT('Ctrl Pts',(-9.50104767561052,15.3447188656481,
1259.81333646895));
#150553=CARTESIAN_POINT('Ctrl Pts',(-8.07915007496071,16.2251205863895,
1258.31921882189));
#150554=CARTESIAN_POINT('Ctrl Pts',(-6.51968959134574,16.8292587962898,
1256.82510117483));
#150555=CARTESIAN_POINT('Ctrl Pts',(-4.96022910773078,17.4333970061901,
1255.33098352777));
#150556=CARTESIAN_POINT('Ctrl Pts',(-3.31631129755346,17.7406985030951,
1253.83686588071));
#150557=CARTESIAN_POINT('Ctrl Pts',(-1.67239348737615,18.048,1252.34274823365));
#150558=CARTESIAN_POINT('Ctrl Pts',(-2.21024254310115E-15,18.048,1250.84863058659));
#150559=CARTESIAN_POINT('Ctrl Pts',(1.67239348737616,18.048,1249.35451293953));
#150560=CARTESIAN_POINT('Ctrl Pts',(3.31631129755346,17.7406985030951,1247.86039529247));
#150561=CARTESIAN_POINT('Ctrl Pts',(4.96022910773077,17.4333970061901,1246.36627764542));
#150562=CARTESIAN_POINT('Ctrl Pts',(6.51968959134575,16.8292587962898,1244.87215999836));
#150563=CARTESIAN_POINT('Ctrl Pts',(8.07915007496071,16.2251205863895,1243.3780423513));
#150564=CARTESIAN_POINT('Ctrl Pts',(9.50104767561053,15.3447188656481,1241.88392470424));
#150565=CARTESIAN_POINT('Ctrl Pts',(10.9229452762603,14.4643171449067,1240.38980705718));
#150566=CARTESIAN_POINT('Ctrl Pts',(12.1588589765331,13.3376329379985,1238.89568941012));
#150567=CARTESIAN_POINT('Ctrl Pts',(13.3947726768058,12.2109487310903,1237.40157176306));
#150568=CARTESIAN_POINT('Ctrl Pts',(14.4026149179538,10.8763499173728,1235.907454116));
#150569=CARTESIAN_POINT('Ctrl Pts',(15.4104571591017,9.54175110365538,1234.41333646895));
#150570=CARTESIAN_POINT('Ctrl Pts',(16.1559070823762,8.04468584505496,1232.91921882189));
#150571=CARTESIAN_POINT('Ctrl Pts',(16.9013570056506,6.54762058645456,1231.42510117483));
#150572=CARTESIAN_POINT('Ctrl Pts',(17.3590292079831,4.93906964482096,1229.93098352777));
#150573=CARTESIAN_POINT('Ctrl Pts',(17.8167014103155,3.33051870318735,1228.43686588071));
#150574=CARTESIAN_POINT('Ctrl Pts',(17.9710104137728,1.66525935159367,1226.94274823365));
#150575=CARTESIAN_POINT('Ctrl Pts',(18.1253194172301,3.32956716117513E-15,
1225.44863058659));
#150576=CARTESIAN_POINT('Ctrl Pts',(17.9710104137728,-1.66525935159367,
1223.95451293953));
#150577=CARTESIAN_POINT('Ctrl Pts',(17.8167014103155,-3.33051870318736,
1222.46039529247));
#150578=CARTESIAN_POINT('Ctrl Pts',(17.3590292079831,-4.93906964482095,
1220.96627764542));
#150579=CARTESIAN_POINT('Ctrl Pts',(16.9013570056506,-6.54762058645456,
1219.47215999836));
#150580=CARTESIAN_POINT('Ctrl Pts',(16.1559070823762,-8.04468584505497,
1217.9780423513));
#150581=CARTESIAN_POINT('Ctrl Pts',(15.4104571591017,-9.54175110365538,
1216.48392470424));
#150582=CARTESIAN_POINT('Ctrl Pts',(14.4026149179538,-10.8763499173728,
1214.98980705718));
#150583=CARTESIAN_POINT('Ctrl Pts',(13.3947726768058,-12.2109487310903,
1213.49568941012));
#150584=CARTESIAN_POINT('Ctrl Pts',(12.1588589765331,-13.3376329379985,
1212.00157176306));
#150585=CARTESIAN_POINT('Ctrl Pts',(10.9229452762603,-14.4643171449067,
1210.507454116));
#150586=CARTESIAN_POINT('Ctrl Pts',(9.50104767561053,-15.3447188656481,
1209.01333646895));
#150587=CARTESIAN_POINT('Ctrl Pts',(8.07915007496071,-16.2251205863895,
1207.51921882189));
#150588=CARTESIAN_POINT('Ctrl Pts',(6.51968959134574,-16.8292587962898,
1206.02510117483));
#150589=CARTESIAN_POINT('Ctrl Pts',(4.96022910773078,-17.4333970061901,
1204.53098352777));
#150590=CARTESIAN_POINT('Ctrl Pts',(3.31631129755346,-17.7406985030951,
1203.03686588071));
#150591=CARTESIAN_POINT('Ctrl Pts',(1.67239348737615,-18.048,1201.54274823365));
#150592=CARTESIAN_POINT('Ctrl Pts',(0.,-18.048,1200.04863058659));
#150593=CARTESIAN_POINT('Ctrl Pts',(-1.67239348737615,-18.048,1198.55451293953));
#150594=CARTESIAN_POINT('Ctrl Pts',(-3.31631129755346,-17.7406985030951,
1197.06039529247));
#150595=CARTESIAN_POINT('Ctrl Pts',(-4.96022910773077,-17.4333970061901,
1195.56627764542));
#150596=CARTESIAN_POINT('Ctrl Pts',(-6.51968959134574,-16.8292587962898,
1194.07215999836));
#150597=CARTESIAN_POINT('Ctrl Pts',(-8.07915007496071,-16.2251205863895,
1192.5780423513));
#150598=CARTESIAN_POINT('Ctrl Pts',(-9.50104767561052,-15.3447188656481,
1191.08392470424));
#150599=CARTESIAN_POINT('Ctrl Pts',(-10.9229452762603,-14.4643171449067,
1189.58980705718));
#150600=CARTESIAN_POINT('Ctrl Pts',(-12.1588589765331,-13.3376329379985,
1188.09568941012));
#150601=CARTESIAN_POINT('Ctrl Pts',(-13.3947726768058,-12.2109487310903,
1186.60157176306));
#150602=CARTESIAN_POINT('Ctrl Pts',(-14.4026149179538,-10.8763499173728,
1185.107454116));
#150603=CARTESIAN_POINT('Ctrl Pts',(-15.4104571591017,-9.54175110365538,
1183.61333646895));
#150604=CARTESIAN_POINT('Ctrl Pts',(-16.1559070823762,-8.04468584505497,
1182.11921882189));
#150605=CARTESIAN_POINT('Ctrl Pts',(-16.9013570056506,-6.54762058645456,
1180.62510117483));
#150606=CARTESIAN_POINT('Ctrl Pts',(-17.3590292079831,-4.93906964482095,
1179.13098352777));
#150607=CARTESIAN_POINT('Ctrl Pts',(-17.8167014103155,-3.33051870318735,
1177.63686588071));
#150608=CARTESIAN_POINT('Ctrl Pts',(-17.9710104137728,-1.66525935159368,
1176.14274823365));
#150609=CARTESIAN_POINT('Ctrl Pts',(-18.1253194172301,-1.10985572039171E-15,
1174.64863058659));
#150610=CARTESIAN_POINT('Ctrl Pts',(-17.9710104137728,1.66525935159367,
1173.15451293953));
#150611=CARTESIAN_POINT('Ctrl Pts',(-17.8167014103155,3.33051870318735,
1171.66039529247));
#150612=CARTESIAN_POINT('Ctrl Pts',(-17.3590292079831,4.93906964482096,
1170.16627764542));
#150613=CARTESIAN_POINT('Ctrl Pts',(-16.9013570056506,6.54762058645456,
1168.67215999836));
#150614=CARTESIAN_POINT('Ctrl Pts',(-16.1559070823762,8.04468584505497,
1167.1780423513));
#150615=CARTESIAN_POINT('Ctrl Pts',(-15.4104571591017,9.54175110365538,
1165.68392470424));
#150616=CARTESIAN_POINT('Ctrl Pts',(-14.4026149179538,10.8763499173728,
1164.18980705718));
#150617=CARTESIAN_POINT('Ctrl Pts',(-13.3947726768058,12.2109487310903,
1162.69568941012));
#150618=CARTESIAN_POINT('Ctrl Pts',(-12.1588589765331,13.3376329379985,
1161.20157176306));
#150619=CARTESIAN_POINT('Ctrl Pts',(-10.9229452762603,14.4643171449067,
1159.707454116));
#150620=CARTESIAN_POINT('Ctrl Pts',(-9.50104767561052,15.3447188656481,
1158.21333646895));
#150621=CARTESIAN_POINT('Ctrl Pts',(-8.07915007496071,16.2251205863895,
1156.71921882189));
#150622=CARTESIAN_POINT('Ctrl Pts',(-6.51968959134574,16.8292587962898,
1155.22510117483));
#150623=CARTESIAN_POINT('Ctrl Pts',(-4.96022910773078,17.4333970061901,
1153.73098352777));
#150624=CARTESIAN_POINT('Ctrl Pts',(-3.31631129755346,17.7406985030951,
1152.23686588071));
#150625=CARTESIAN_POINT('Ctrl Pts',(-1.67239348737615,18.048,1150.74274823365));
#150626=CARTESIAN_POINT('Ctrl Pts',(-2.21024254310115E-15,18.048,1149.24863058659));
#150627=CARTESIAN_POINT('Ctrl Pts',(1.67239348737616,18.048,1147.75451293953));
#150628=CARTESIAN_POINT('Ctrl Pts',(3.31631129755346,17.7406985030951,1146.26039529247));
#150629=CARTESIAN_POINT('Ctrl Pts',(4.96022910773077,17.4333970061901,1144.76627764542));
#150630=CARTESIAN_POINT('Ctrl Pts',(6.51968959134575,16.8292587962898,1143.27215999836));
#150631=CARTESIAN_POINT('Ctrl Pts',(8.07915007496071,16.2251205863895,1141.7780423513));
#150632=CARTESIAN_POINT('Ctrl Pts',(9.50104767561053,15.3447188656481,1140.28392470424));
#150633=CARTESIAN_POINT('Ctrl Pts',(10.9229452762603,14.4643171449067,1138.78980705718));
#150634=CARTESIAN_POINT('Ctrl Pts',(12.1588589765331,13.3376329379985,1137.29568941012));
#150635=CARTESIAN_POINT('Ctrl Pts',(13.3947726768058,12.2109487310903,1135.80157176306));
#150636=CARTESIAN_POINT('Ctrl Pts',(14.4026149179538,10.8763499173728,1134.307454116));
#150637=CARTESIAN_POINT('Ctrl Pts',(15.4104571591017,9.54175110365538,1132.81333646895));
#150638=CARTESIAN_POINT('Ctrl Pts',(16.1559070823762,8.04468584505496,1131.31921882189));
#150639=CARTESIAN_POINT('Ctrl Pts',(16.9013570056506,6.54762058645456,1129.82510117483));
#150640=CARTESIAN_POINT('Ctrl Pts',(17.3590292079831,4.93906964482096,1128.33098352777));
#150641=CARTESIAN_POINT('Ctrl Pts',(17.8167014103155,3.33051870318735,1126.83686588071));
#150642=CARTESIAN_POINT('Ctrl Pts',(17.9710104137728,1.66525935159367,1125.34274823365));
#150643=CARTESIAN_POINT('Ctrl Pts',(18.1253194172301,3.32956716117513E-15,
1123.84863058659));
#150644=CARTESIAN_POINT('Ctrl Pts',(17.9710104137728,-1.66525935159367,
1122.35451293953));
#150645=CARTESIAN_POINT('Ctrl Pts',(17.8167014103155,-3.33051870318736,
1120.86039529247));
#150646=CARTESIAN_POINT('Ctrl Pts',(17.3590292079831,-4.93906964482095,
1119.36627764542));
#150647=CARTESIAN_POINT('Ctrl Pts',(16.9013570056506,-6.54762058645456,
1117.87215999836));
#150648=CARTESIAN_POINT('Ctrl Pts',(16.1559070823762,-8.04468584505497,
1116.3780423513));
#150649=CARTESIAN_POINT('Ctrl Pts',(15.4104571591017,-9.54175110365538,
1114.88392470424));
#150650=CARTESIAN_POINT('Ctrl Pts',(14.4026149179538,-10.8763499173728,
1113.38980705718));
#150651=CARTESIAN_POINT('Ctrl Pts',(13.3947726768058,-12.2109487310903,
1111.89568941012));
#150652=CARTESIAN_POINT('Ctrl Pts',(12.1588589765331,-13.3376329379985,
1110.40157176306));
#150653=CARTESIAN_POINT('Ctrl Pts',(10.9229452762603,-14.4643171449067,
1108.907454116));
#150654=CARTESIAN_POINT('Ctrl Pts',(9.50104767561053,-15.3447188656481,
1107.41333646895));
#150655=CARTESIAN_POINT('Ctrl Pts',(8.07915007496071,-16.2251205863895,
1105.91921882189));
#150656=CARTESIAN_POINT('Ctrl Pts',(6.51968959134574,-16.8292587962898,
1104.42510117483));
#150657=CARTESIAN_POINT('Ctrl Pts',(4.96022910773078,-17.4333970061901,
1102.93098352777));
#150658=CARTESIAN_POINT('Ctrl Pts',(3.31631129755346,-17.7406985030951,
1101.43686588071));
#150659=CARTESIAN_POINT('Ctrl Pts',(1.67239348737615,-18.048,1099.94274823365));
#150660=CARTESIAN_POINT('Ctrl Pts',(0.,-18.048,1098.44863058659));
#150661=CARTESIAN_POINT('Ctrl Pts',(-1.67239348737615,-18.048,1096.95451293953));
#150662=CARTESIAN_POINT('Ctrl Pts',(-3.31631129755346,-17.7406985030951,
1095.46039529247));
#150663=CARTESIAN_POINT('Ctrl Pts',(-4.96022910773077,-17.4333970061901,
1093.96627764542));
#150664=CARTESIAN_POINT('Ctrl Pts',(-6.51968959134574,-16.8292587962898,
1092.47215999836));
#150665=CARTESIAN_POINT('Ctrl Pts',(-8.07915007496071,-16.2251205863895,
1090.9780423513));
#150666=CARTESIAN_POINT('Ctrl Pts',(-9.50104767561052,-15.3447188656481,
1089.48392470424));
#150667=CARTESIAN_POINT('Ctrl Pts',(-10.9229452762603,-14.4643171449067,
1087.98980705718));
#150668=CARTESIAN_POINT('Ctrl Pts',(-12.1588589765331,-13.3376329379985,
1086.49568941012));
#150669=CARTESIAN_POINT('Ctrl Pts',(-13.3947726768058,-12.2109487310903,
1085.00157176306));
#150670=CARTESIAN_POINT('Ctrl Pts',(-14.4026149179538,-10.8763499173728,
1083.507454116));
#150671=CARTESIAN_POINT('Ctrl Pts',(-15.4104571591017,-9.54175110365538,
1082.01333646895));
#150672=CARTESIAN_POINT('Ctrl Pts',(-16.1559070823762,-8.04468584505497,
1080.51921882189));
#150673=CARTESIAN_POINT('Ctrl Pts',(-16.9013570056506,-6.54762058645456,
1079.02510117483));
#150674=CARTESIAN_POINT('Ctrl Pts',(-17.3590292079831,-4.93906964482095,
1077.53098352777));
#150675=CARTESIAN_POINT('Ctrl Pts',(-17.8167014103155,-3.33051870318735,
1076.03686588071));
#150676=CARTESIAN_POINT('Ctrl Pts',(-17.9710104137728,-1.66525935159368,
1074.54274823365));
#150677=CARTESIAN_POINT('Ctrl Pts',(-18.1253194172301,-1.10985572039171E-15,
1073.04863058659));
#150678=CARTESIAN_POINT('Ctrl Pts',(-17.9710104137728,1.66525935159367,
1071.55451293953));
#150679=CARTESIAN_POINT('Ctrl Pts',(-17.8167014103155,3.33051870318735,
1070.06039529247));
#150680=CARTESIAN_POINT('Ctrl Pts',(-17.3590292079831,4.93906964482096,
1068.56627764542));
#150681=CARTESIAN_POINT('Ctrl Pts',(-16.9013570056506,6.54762058645456,
1067.07215999836));
#150682=CARTESIAN_POINT('Ctrl Pts',(-16.1559070823762,8.04468584505497,
1065.5780423513));
#150683=CARTESIAN_POINT('Ctrl Pts',(-15.4104571591017,9.54175110365538,
1064.08392470424));
#150684=CARTESIAN_POINT('Ctrl Pts',(-14.4026149179538,10.8763499173728,
1062.58980705718));
#150685=CARTESIAN_POINT('Ctrl Pts',(-13.3947726768058,12.2109487310903,
1061.09568941012));
#150686=CARTESIAN_POINT('Ctrl Pts',(-12.1588589765331,13.3376329379985,
1059.60157176306));
#150687=CARTESIAN_POINT('Ctrl Pts',(-10.9229452762603,14.4643171449067,
1058.107454116));
#150688=CARTESIAN_POINT('Ctrl Pts',(-9.50104767561052,15.3447188656481,
1056.61333646895));
#150689=CARTESIAN_POINT('Ctrl Pts',(-8.07915007496071,16.2251205863895,
1055.11921882189));
#150690=CARTESIAN_POINT('Ctrl Pts',(-6.51968959134574,16.8292587962898,
1053.62510117483));
#150691=CARTESIAN_POINT('Ctrl Pts',(-4.96022910773078,17.4333970061901,
1052.13098352777));
#150692=CARTESIAN_POINT('Ctrl Pts',(-3.31631129755346,17.7406985030951,
1050.63686588071));
#150693=CARTESIAN_POINT('Ctrl Pts',(-1.67239348737615,18.048,1049.14274823365));
#150694=CARTESIAN_POINT('Ctrl Pts',(-2.21024254310115E-15,18.048,1047.64863058659));
#150695=CARTESIAN_POINT('Ctrl Pts',(1.67239348737616,18.048,1046.15451293953));
#150696=CARTESIAN_POINT('Ctrl Pts',(3.31631129755346,17.7406985030951,1044.66039529247));
#150697=CARTESIAN_POINT('Ctrl Pts',(4.96022910773077,17.4333970061901,1043.16627764542));
#150698=CARTESIAN_POINT('Ctrl Pts',(6.51968959134575,16.8292587962898,1041.67215999836));
#150699=CARTESIAN_POINT('Ctrl Pts',(8.07915007496071,16.2251205863895,1040.1780423513));
#150700=CARTESIAN_POINT('Ctrl Pts',(9.50104767561053,15.3447188656481,1038.68392470424));
#150701=CARTESIAN_POINT('Ctrl Pts',(10.9229452762603,14.4643171449067,1037.18980705718));
#150702=CARTESIAN_POINT('Ctrl Pts',(12.1588589765331,13.3376329379985,1035.69568941012));
#150703=CARTESIAN_POINT('Ctrl Pts',(13.3947726768058,12.2109487310903,1034.20157176306));
#150704=CARTESIAN_POINT('Ctrl Pts',(14.4026149179538,10.8763499173728,1032.707454116));
#150705=CARTESIAN_POINT('Ctrl Pts',(15.4104571591017,9.54175110365538,1031.21333646895));
#150706=CARTESIAN_POINT('Ctrl Pts',(16.1559070823762,8.04468584505496,1029.71921882189));
#150707=CARTESIAN_POINT('Ctrl Pts',(16.9013570056506,6.54762058645456,1028.22510117483));
#150708=CARTESIAN_POINT('Ctrl Pts',(17.3590292079831,4.93906964482096,1026.73098352777));
#150709=CARTESIAN_POINT('Ctrl Pts',(17.8167014103155,3.33051870318735,1025.23686588071));
#150710=CARTESIAN_POINT('Ctrl Pts',(17.9710104137728,1.66525935159367,1023.74274823365));
#150711=CARTESIAN_POINT('Ctrl Pts',(18.1253194172301,3.32956716117513E-15,
1022.24863058659));
#150712=CARTESIAN_POINT('Ctrl Pts',(17.9710104137728,-1.66525935159367,
1020.75451293953));
#150713=CARTESIAN_POINT('Ctrl Pts',(17.8167014103155,-3.33051870318736,
1019.26039529247));
#150714=CARTESIAN_POINT('Ctrl Pts',(17.3590292079831,-4.93906964482095,
1017.76627764542));
#150715=CARTESIAN_POINT('Ctrl Pts',(16.9013570056506,-6.54762058645456,
1016.27215999836));
#150716=CARTESIAN_POINT('Ctrl Pts',(16.1559070823762,-8.04468584505497,
1014.7780423513));
#150717=CARTESIAN_POINT('Ctrl Pts',(15.4104571591017,-9.54175110365538,
1013.28392470424));
#150718=CARTESIAN_POINT('Ctrl Pts',(14.4026149179538,-10.8763499173728,
1011.78980705718));
#150719=CARTESIAN_POINT('Ctrl Pts',(13.3947726768058,-12.2109487310903,
1010.29568941012));
#150720=CARTESIAN_POINT('Ctrl Pts',(12.1588589765331,-13.3376329379985,
1008.80157176306));
#150721=CARTESIAN_POINT('Ctrl Pts',(10.9229452762603,-14.4643171449067,
1007.307454116));
#150722=CARTESIAN_POINT('Ctrl Pts',(9.50104767561053,-15.3447188656481,
1005.81333646895));
#150723=CARTESIAN_POINT('Ctrl Pts',(8.07915007496071,-16.2251205863895,
1004.31921882189));
#150724=CARTESIAN_POINT('Ctrl Pts',(6.51968959134574,-16.8292587962898,
1002.82510117483));
#150725=CARTESIAN_POINT('Ctrl Pts',(4.96022910773078,-17.4333970061901,
1001.33098352777));
#150726=CARTESIAN_POINT('Ctrl Pts',(3.31631129755346,-17.7406985030951,
999.83686588071));
#150727=CARTESIAN_POINT('Ctrl Pts',(1.67239348737615,-18.048,998.342748233651));
#150728=CARTESIAN_POINT('Ctrl Pts',(0.,-18.048,996.848630586592));
#150729=CARTESIAN_POINT('Ctrl Pts',(-1.67239348737615,-18.048,995.354512939534));
#150730=CARTESIAN_POINT('Ctrl Pts',(-3.31631129755346,-17.7406985030951,
993.860395292475));
#150731=CARTESIAN_POINT('Ctrl Pts',(-4.96022910773077,-17.4333970061901,
992.366277645416));
#150732=CARTESIAN_POINT('Ctrl Pts',(-6.51968959134574,-16.8292587962898,
990.872159998357));
#150733=CARTESIAN_POINT('Ctrl Pts',(-8.07915007496071,-16.2251205863895,
989.378042351298));
#150734=CARTESIAN_POINT('Ctrl Pts',(-9.50104767561052,-15.3447188656481,
987.883924704239));
#150735=CARTESIAN_POINT('Ctrl Pts',(-10.9229452762603,-14.4643171449067,
986.38980705718));
#150736=CARTESIAN_POINT('Ctrl Pts',(-12.1588589765331,-13.3376329379985,
984.895689410122));
#150737=CARTESIAN_POINT('Ctrl Pts',(-13.3947726768058,-12.2109487310903,
983.401571763063));
#150738=CARTESIAN_POINT('Ctrl Pts',(-14.4026149179538,-10.8763499173728,
981.907454116004));
#150739=CARTESIAN_POINT('Ctrl Pts',(-15.4104571591017,-9.54175110365538,
980.413336468945));
#150740=CARTESIAN_POINT('Ctrl Pts',(-16.1559070823762,-8.04468584505497,
978.919218821886));
#150741=CARTESIAN_POINT('Ctrl Pts',(-16.9013570056506,-6.54762058645456,
977.425101174828));
#150742=CARTESIAN_POINT('Ctrl Pts',(-17.3590292079831,-4.93906964482095,
975.930983527769));
#150743=CARTESIAN_POINT('Ctrl Pts',(-17.8167014103155,-3.33051870318735,
974.43686588071));
#150744=CARTESIAN_POINT('Ctrl Pts',(-17.9710104137728,-1.66525935159368,
972.942748233651));
#150745=CARTESIAN_POINT('Ctrl Pts',(-18.1253194172301,-1.10985572039171E-15,
971.448630586592));
#150746=CARTESIAN_POINT('Ctrl Pts',(-17.9710104137728,1.66525935159367,
969.954512939534));
#150747=CARTESIAN_POINT('Ctrl Pts',(-17.8167014103155,3.33051870318735,
968.460395292475));
#150748=CARTESIAN_POINT('Ctrl Pts',(-17.3590292079831,4.93906964482096,
966.966277645416));
#150749=CARTESIAN_POINT('Ctrl Pts',(-16.9013570056506,6.54762058645456,
965.472159998357));
#150750=CARTESIAN_POINT('Ctrl Pts',(-16.1559070823762,8.04468584505497,
963.978042351298));
#150751=CARTESIAN_POINT('Ctrl Pts',(-15.4104571591017,9.54175110365538,
962.483924704239));
#150752=CARTESIAN_POINT('Ctrl Pts',(-14.4026149179538,10.8763499173728,
960.989807057181));
#150753=CARTESIAN_POINT('Ctrl Pts',(-13.3947726768058,12.2109487310903,
959.495689410122));
#150754=CARTESIAN_POINT('Ctrl Pts',(-12.1588589765331,13.3376329379985,
958.001571763063));
#150755=CARTESIAN_POINT('Ctrl Pts',(-10.9229452762603,14.4643171449067,
956.507454116004));
#150756=CARTESIAN_POINT('Ctrl Pts',(-9.50104767561052,15.3447188656481,
955.013336468945));
#150757=CARTESIAN_POINT('Ctrl Pts',(-8.07915007496071,16.2251205863895,
953.519218821887));
#150758=CARTESIAN_POINT('Ctrl Pts',(-6.51968959134574,16.8292587962898,
952.025101174828));
#150759=CARTESIAN_POINT('Ctrl Pts',(-4.96022910773078,17.4333970061901,
950.530983527769));
#150760=CARTESIAN_POINT('Ctrl Pts',(-3.31631129755346,17.7406985030951,
949.03686588071));
#150761=CARTESIAN_POINT('Ctrl Pts',(-1.67239348737615,18.048,947.542748233651));
#150762=CARTESIAN_POINT('Ctrl Pts',(-2.21024254310115E-15,18.048,946.048630586592));
#150763=CARTESIAN_POINT('Ctrl Pts',(1.67239348737616,18.048,944.554512939534));
#150764=CARTESIAN_POINT('Ctrl Pts',(3.31631129755346,17.7406985030951,943.060395292475));
#150765=CARTESIAN_POINT('Ctrl Pts',(4.96022910773077,17.4333970061901,941.566277645416));
#150766=CARTESIAN_POINT('Ctrl Pts',(6.51968959134575,16.8292587962898,940.072159998357));
#150767=CARTESIAN_POINT('Ctrl Pts',(8.07915007496071,16.2251205863895,938.578042351298));
#150768=CARTESIAN_POINT('Ctrl Pts',(9.50104767561053,15.3447188656481,937.083924704239));
#150769=CARTESIAN_POINT('Ctrl Pts',(10.9229452762603,14.4643171449067,935.589807057181));
#150770=CARTESIAN_POINT('Ctrl Pts',(12.1588589765331,13.3376329379985,934.095689410122));
#150771=CARTESIAN_POINT('Ctrl Pts',(13.3947726768058,12.2109487310903,932.601571763063));
#150772=CARTESIAN_POINT('Ctrl Pts',(14.4026149179538,10.8763499173728,931.107454116004));
#150773=CARTESIAN_POINT('Ctrl Pts',(15.4104571591017,9.54175110365538,929.613336468945));
#150774=CARTESIAN_POINT('Ctrl Pts',(16.1559070823762,8.04468584505496,928.119218821886));
#150775=CARTESIAN_POINT('Ctrl Pts',(16.9013570056506,6.54762058645456,926.625101174827));
#150776=CARTESIAN_POINT('Ctrl Pts',(17.3590292079831,4.93906964482096,925.130983527769));
#150777=CARTESIAN_POINT('Ctrl Pts',(17.8167014103155,3.33051870318735,923.63686588071));
#150778=CARTESIAN_POINT('Ctrl Pts',(17.9710104137728,1.66525935159367,922.142748233651));
#150779=CARTESIAN_POINT('Ctrl Pts',(18.1253194172301,3.32956716117513E-15,
920.648630586593));
#150780=CARTESIAN_POINT('Ctrl Pts',(17.9710104137728,-1.66525935159367,
919.154512939534));
#150781=CARTESIAN_POINT('Ctrl Pts',(17.8167014103155,-3.33051870318736,
917.660395292475));
#150782=CARTESIAN_POINT('Ctrl Pts',(17.3590292079831,-4.93906964482095,
916.166277645416));
#150783=CARTESIAN_POINT('Ctrl Pts',(16.9013570056506,-6.54762058645456,
914.672159998357));
#150784=CARTESIAN_POINT('Ctrl Pts',(16.1559070823762,-8.04468584505497,
913.178042351298));
#150785=CARTESIAN_POINT('Ctrl Pts',(15.4104571591017,-9.54175110365538,
911.683924704239));
#150786=CARTESIAN_POINT('Ctrl Pts',(14.4026149179538,-10.8763499173728,
910.18980705718));
#150787=CARTESIAN_POINT('Ctrl Pts',(13.3947726768058,-12.2109487310903,
908.695689410122));
#150788=CARTESIAN_POINT('Ctrl Pts',(12.1588589765331,-13.3376329379985,
907.201571763063));
#150789=CARTESIAN_POINT('Ctrl Pts',(10.9229452762603,-14.4643171449067,
905.707454116004));
#150790=CARTESIAN_POINT('Ctrl Pts',(9.50104767561053,-15.3447188656481,
904.213336468945));
#150791=CARTESIAN_POINT('Ctrl Pts',(8.07915007496071,-16.2251205863895,
902.719218821886));
#150792=CARTESIAN_POINT('Ctrl Pts',(6.51968959134574,-16.8292587962898,
901.225101174828));
#150793=CARTESIAN_POINT('Ctrl Pts',(4.96022910773078,-17.4333970061901,
899.730983527769));
#150794=CARTESIAN_POINT('Ctrl Pts',(3.31631129755346,-17.7406985030951,
898.23686588071));
#150795=CARTESIAN_POINT('Ctrl Pts',(1.67239348737615,-18.048,896.742748233651));
#150796=CARTESIAN_POINT('Ctrl Pts',(0.,-18.048,895.248630586592));
#150797=CARTESIAN_POINT('Ctrl Pts',(-1.67239348737615,-18.048,893.754512939534));
#150798=CARTESIAN_POINT('Ctrl Pts',(-3.31631129755346,-17.7406985030951,
892.260395292475));
#150799=CARTESIAN_POINT('Ctrl Pts',(-4.96022910773077,-17.4333970061901,
890.766277645416));
#150800=CARTESIAN_POINT('Ctrl Pts',(-6.51968959134574,-16.8292587962898,
889.272159998357));
#150801=CARTESIAN_POINT('Ctrl Pts',(-8.07915007496071,-16.2251205863895,
887.778042351298));
#150802=CARTESIAN_POINT('Ctrl Pts',(-9.50104767561052,-15.3447188656481,
886.283924704239));
#150803=CARTESIAN_POINT('Ctrl Pts',(-10.9229452762603,-14.4643171449067,
884.789807057181));
#150804=CARTESIAN_POINT('Ctrl Pts',(-12.1588589765331,-13.3376329379985,
883.295689410122));
#150805=CARTESIAN_POINT('Ctrl Pts',(-13.3947726768058,-12.2109487310903,
881.801571763063));
#150806=CARTESIAN_POINT('Ctrl Pts',(-14.4026149179538,-10.8763499173728,
880.307454116004));
#150807=CARTESIAN_POINT('Ctrl Pts',(-15.4104571591017,-9.54175110365538,
878.813336468945));
#150808=CARTESIAN_POINT('Ctrl Pts',(-16.1559070823762,-8.04468584505497,
877.319218821886));
#150809=CARTESIAN_POINT('Ctrl Pts',(-16.9013570056506,-6.54762058645456,
875.825101174828));
#150810=CARTESIAN_POINT('Ctrl Pts',(-17.3590292079831,-4.93906964482095,
874.330983527769));
#150811=CARTESIAN_POINT('Ctrl Pts',(-17.8167014103155,-3.33051870318735,
872.83686588071));
#150812=CARTESIAN_POINT('Ctrl Pts',(-17.9710104137728,-1.66525935159368,
871.342748233651));
#150813=CARTESIAN_POINT('Ctrl Pts',(-18.1253194172301,-1.10985572039171E-15,
869.848630586592));
#150814=CARTESIAN_POINT('Ctrl Pts',(-17.9710104137728,1.66525935159367,
868.354512939534));
#150815=CARTESIAN_POINT('Ctrl Pts',(-17.8167014103155,3.33051870318735,
866.860395292475));
#150816=CARTESIAN_POINT('Ctrl Pts',(-17.3590292079831,4.93906964482096,
865.366277645416));
#150817=CARTESIAN_POINT('Ctrl Pts',(-16.9013570056506,6.54762058645456,
863.872159998357));
#150818=CARTESIAN_POINT('Ctrl Pts',(-16.1559070823762,8.04468584505497,
862.378042351298));
#150819=CARTESIAN_POINT('Ctrl Pts',(-15.4104571591017,9.54175110365538,
860.883924704239));
#150820=CARTESIAN_POINT('Ctrl Pts',(-14.4026149179538,10.8763499173728,
859.389807057181));
#150821=CARTESIAN_POINT('Ctrl Pts',(-13.3947726768058,12.2109487310903,
857.895689410122));
#150822=CARTESIAN_POINT('Ctrl Pts',(-12.1588589765331,13.3376329379985,
856.401571763063));
#150823=CARTESIAN_POINT('Ctrl Pts',(-10.9229452762603,14.4643171449067,
854.907454116004));
#150824=CARTESIAN_POINT('Ctrl Pts',(-9.50104767561052,15.3447188656481,
853.413336468945));
#150825=CARTESIAN_POINT('Ctrl Pts',(-8.07915007496071,16.2251205863895,
851.919218821886));
#150826=CARTESIAN_POINT('Ctrl Pts',(-6.51968959134574,16.8292587962898,
850.425101174828));
#150827=CARTESIAN_POINT('Ctrl Pts',(-4.96022910773078,17.4333970061901,
848.930983527769));
#150828=CARTESIAN_POINT('Ctrl Pts',(-3.31631129755346,17.7406985030951,
847.43686588071));
#150829=CARTESIAN_POINT('Ctrl Pts',(-1.67239348737615,18.048,845.942748233651));
#150830=CARTESIAN_POINT('Ctrl Pts',(-2.21024254310115E-15,18.048,844.448630586592));
#150831=CARTESIAN_POINT('Ctrl Pts',(1.67239348737616,18.048,842.954512939534));
#150832=CARTESIAN_POINT('Ctrl Pts',(3.31631129755346,17.7406985030951,841.460395292475));
#150833=CARTESIAN_POINT('Ctrl Pts',(4.96022910773077,17.4333970061901,839.966277645416));
#150834=CARTESIAN_POINT('Ctrl Pts',(6.51968959134575,16.8292587962898,838.472159998357));
#150835=CARTESIAN_POINT('Ctrl Pts',(8.07915007496071,16.2251205863895,836.978042351298));
#150836=CARTESIAN_POINT('Ctrl Pts',(9.50104767561053,15.3447188656481,835.483924704239));
#150837=CARTESIAN_POINT('Ctrl Pts',(10.9229452762603,14.4643171449067,833.989807057181));
#150838=CARTESIAN_POINT('Ctrl Pts',(12.1588589765331,13.3376329379985,832.495689410122));
#150839=CARTESIAN_POINT('Ctrl Pts',(13.3947726768058,12.2109487310903,831.001571763063));
#150840=CARTESIAN_POINT('Ctrl Pts',(14.4026149179538,10.8763499173728,829.507454116004));
#150841=CARTESIAN_POINT('Ctrl Pts',(15.4104571591017,9.54175110365538,828.013336468945));
#150842=CARTESIAN_POINT('Ctrl Pts',(16.1559070823762,8.04468584505496,826.519218821886));
#150843=CARTESIAN_POINT('Ctrl Pts',(16.9013570056506,6.54762058645456,825.025101174828));
#150844=CARTESIAN_POINT('Ctrl Pts',(17.3590292079831,4.93906964482096,823.530983527769));
#150845=CARTESIAN_POINT('Ctrl Pts',(17.8167014103155,3.33051870318735,822.03686588071));
#150846=CARTESIAN_POINT('Ctrl Pts',(17.9710104137728,1.66525935159367,820.542748233651));
#150847=CARTESIAN_POINT('Ctrl Pts',(18.1253194172301,3.32956716117513E-15,
819.048630586593));
#150848=CARTESIAN_POINT('Ctrl Pts',(17.9710104137728,-1.66525935159367,
817.554512939533));
#150849=CARTESIAN_POINT('Ctrl Pts',(17.8167014103155,-3.33051870318736,
816.060395292475));
#150850=CARTESIAN_POINT('Ctrl Pts',(17.3590292079831,-4.93906964482095,
814.566277645416));
#150851=CARTESIAN_POINT('Ctrl Pts',(16.9013570056506,-6.54762058645456,
813.072159998357));
#150852=CARTESIAN_POINT('Ctrl Pts',(16.1559070823762,-8.04468584505497,
811.578042351298));
#150853=CARTESIAN_POINT('Ctrl Pts',(15.4104571591017,-9.54175110365538,
810.083924704239));
#150854=CARTESIAN_POINT('Ctrl Pts',(14.4026149179538,-10.8763499173728,
808.589807057181));
#150855=CARTESIAN_POINT('Ctrl Pts',(13.3947726768058,-12.2109487310903,
807.095689410122));
#150856=CARTESIAN_POINT('Ctrl Pts',(12.1588589765331,-13.3376329379985,
805.601571763063));
#150857=CARTESIAN_POINT('Ctrl Pts',(10.9229452762603,-14.4643171449067,
804.107454116004));
#150858=CARTESIAN_POINT('Ctrl Pts',(9.50104767561053,-15.3447188656481,
802.613336468945));
#150859=CARTESIAN_POINT('Ctrl Pts',(8.07915007496071,-16.2251205863895,
801.119218821887));
#150860=CARTESIAN_POINT('Ctrl Pts',(6.51968959134574,-16.8292587962898,
799.625101174828));
#150861=CARTESIAN_POINT('Ctrl Pts',(4.96022910773078,-17.4333970061901,
798.130983527769));
#150862=CARTESIAN_POINT('Ctrl Pts',(3.31631129755346,-17.7406985030951,
796.63686588071));
#150863=CARTESIAN_POINT('Ctrl Pts',(1.67239348737615,-18.048,795.142748233651));
#150864=CARTESIAN_POINT('Ctrl Pts',(0.,-18.048,793.648630586592));
#150865=CARTESIAN_POINT('Ctrl Pts',(-1.67239348737615,-18.048,792.154512939534));
#150866=CARTESIAN_POINT('Ctrl Pts',(-3.31631129755346,-17.7406985030951,
790.660395292475));
#150867=CARTESIAN_POINT('Ctrl Pts',(-4.96022910773077,-17.4333970061901,
789.166277645416));
#150868=CARTESIAN_POINT('Ctrl Pts',(-6.51968959134574,-16.8292587962898,
787.672159998357));
#150869=CARTESIAN_POINT('Ctrl Pts',(-8.07915007496071,-16.2251205863895,
786.178042351298));
#150870=CARTESIAN_POINT('Ctrl Pts',(-9.50104767561052,-15.3447188656481,
784.683924704239));
#150871=CARTESIAN_POINT('Ctrl Pts',(-10.9229452762603,-14.4643171449067,
783.189807057181));
#150872=CARTESIAN_POINT('Ctrl Pts',(-12.1588589765331,-13.3376329379985,
781.695689410122));
#150873=CARTESIAN_POINT('Ctrl Pts',(-13.3947726768058,-12.2109487310903,
780.201571763063));
#150874=CARTESIAN_POINT('Ctrl Pts',(-14.4026149179538,-10.8763499173728,
778.707454116004));
#150875=CARTESIAN_POINT('Ctrl Pts',(-15.4104571591017,-9.54175110365538,
777.213336468945));
#150876=CARTESIAN_POINT('Ctrl Pts',(-16.1559070823762,-8.04468584505497,
775.719218821886));
#150877=CARTESIAN_POINT('Ctrl Pts',(-16.9013570056506,-6.54762058645456,
774.225101174828));
#150878=CARTESIAN_POINT('Ctrl Pts',(-17.3590292079831,-4.93906964482095,
772.730983527769));
#150879=CARTESIAN_POINT('Ctrl Pts',(-17.8167014103155,-3.33051870318735,
771.23686588071));
#150880=CARTESIAN_POINT('Ctrl Pts',(-17.9710104137728,-1.66525935159368,
769.742748233651));
#150881=CARTESIAN_POINT('Ctrl Pts',(-18.1253194172301,-1.10985572039171E-15,
768.248630586593));
#150882=CARTESIAN_POINT('Ctrl Pts',(-17.9710104137728,1.66525935159367,
766.754512939533));
#150883=CARTESIAN_POINT('Ctrl Pts',(-17.8167014103155,3.33051870318735,
765.260395292475));
#150884=CARTESIAN_POINT('Ctrl Pts',(-17.3590292079831,4.93906964482096,
763.766277645416));
#150885=CARTESIAN_POINT('Ctrl Pts',(-16.9013570056506,6.54762058645456,
762.272159998357));
#150886=CARTESIAN_POINT('Ctrl Pts',(-16.1559070823762,8.04468584505497,
760.778042351298));
#150887=CARTESIAN_POINT('Ctrl Pts',(-15.4104571591017,9.54175110365538,
759.28392470424));
#150888=CARTESIAN_POINT('Ctrl Pts',(-14.4026149179538,10.8763499173728,
757.78980705718));
#150889=CARTESIAN_POINT('Ctrl Pts',(-13.3947726768058,12.2109487310903,
756.295689410122));
#150890=CARTESIAN_POINT('Ctrl Pts',(-12.1588589765331,13.3376329379985,
754.801571763063));
#150891=CARTESIAN_POINT('Ctrl Pts',(-10.9229452762603,14.4643171449067,
753.307454116004));
#150892=CARTESIAN_POINT('Ctrl Pts',(-9.50104767561052,15.3447188656481,
751.813336468945));
#150893=CARTESIAN_POINT('Ctrl Pts',(-8.07915007496071,16.2251205863895,
750.319218821886));
#150894=CARTESIAN_POINT('Ctrl Pts',(-6.51968959134574,16.8292587962898,
748.825101174828));
#150895=CARTESIAN_POINT('Ctrl Pts',(-4.96022910773078,17.4333970061901,
747.330983527769));
#150896=CARTESIAN_POINT('Ctrl Pts',(-3.31631129755346,17.7406985030951,
745.83686588071));
#150897=CARTESIAN_POINT('Ctrl Pts',(-1.67239348737615,18.048,744.342748233651));
#150898=CARTESIAN_POINT('Ctrl Pts',(-2.21024254310115E-15,18.048,742.848630586592));
#150899=CARTESIAN_POINT('Ctrl Pts',(1.67239348737616,18.048,741.354512939533));
#150900=CARTESIAN_POINT('Ctrl Pts',(3.31631129755346,17.7406985030951,739.860395292475));
#150901=CARTESIAN_POINT('Ctrl Pts',(4.96022910773077,17.4333970061901,738.366277645416));
#150902=CARTESIAN_POINT('Ctrl Pts',(6.51968959134575,16.8292587962898,736.872159998357));
#150903=CARTESIAN_POINT('Ctrl Pts',(8.07915007496071,16.2251205863895,735.378042351298));
#150904=CARTESIAN_POINT('Ctrl Pts',(9.50104767561053,15.3447188656481,733.883924704239));
#150905=CARTESIAN_POINT('Ctrl Pts',(10.9229452762603,14.4643171449067,732.389807057181));
#150906=CARTESIAN_POINT('Ctrl Pts',(12.1588589765331,13.3376329379985,730.895689410122));
#150907=CARTESIAN_POINT('Ctrl Pts',(13.3947726768058,12.2109487310903,729.401571763063));
#150908=CARTESIAN_POINT('Ctrl Pts',(14.4026149179538,10.8763499173728,727.907454116004));
#150909=CARTESIAN_POINT('Ctrl Pts',(15.4104571591017,9.54175110365538,726.413336468945));
#150910=CARTESIAN_POINT('Ctrl Pts',(16.1559070823762,8.04468584505496,724.919218821886));
#150911=CARTESIAN_POINT('Ctrl Pts',(16.9013570056506,6.54762058645456,723.425101174828));
#150912=CARTESIAN_POINT('Ctrl Pts',(17.3590292079831,4.93906964482096,721.930983527769));
#150913=CARTESIAN_POINT('Ctrl Pts',(17.8167014103155,3.33051870318735,720.43686588071));
#150914=CARTESIAN_POINT('Ctrl Pts',(17.9710104137728,1.66525935159367,718.942748233651));
#150915=CARTESIAN_POINT('Ctrl Pts',(18.1253194172301,3.32956716117513E-15,
717.448630586592));
#150916=CARTESIAN_POINT('Ctrl Pts',(17.9710104137728,-1.66525935159367,
715.954512939534));
#150917=CARTESIAN_POINT('Ctrl Pts',(17.8167014103155,-3.33051870318736,
714.460395292475));
#150918=CARTESIAN_POINT('Ctrl Pts',(17.3590292079831,-4.93906964482095,
712.966277645416));
#150919=CARTESIAN_POINT('Ctrl Pts',(16.9013570056506,-6.54762058645456,
711.472159998357));
#150920=CARTESIAN_POINT('Ctrl Pts',(16.1559070823762,-8.04468584505497,
709.978042351298));
#150921=CARTESIAN_POINT('Ctrl Pts',(15.4104571591017,-9.54175110365538,
708.483924704239));
#150922=CARTESIAN_POINT('Ctrl Pts',(14.4026149179538,-10.8763499173728,
706.989807057181));
#150923=CARTESIAN_POINT('Ctrl Pts',(13.3947726768058,-12.2109487310903,
705.495689410122));
#150924=CARTESIAN_POINT('Ctrl Pts',(12.1588589765331,-13.3376329379985,
704.001571763063));
#150925=CARTESIAN_POINT('Ctrl Pts',(10.9229452762603,-14.4643171449067,
702.507454116004));
#150926=CARTESIAN_POINT('Ctrl Pts',(9.50104767561053,-15.3447188656481,
701.013336468945));
#150927=CARTESIAN_POINT('Ctrl Pts',(8.07915007496071,-16.2251205863895,
699.519218821886));
#150928=CARTESIAN_POINT('Ctrl Pts',(6.51968959134574,-16.8292587962898,
698.025101174828));
#150929=CARTESIAN_POINT('Ctrl Pts',(4.96022910773078,-17.4333970061901,
696.530983527769));
#150930=CARTESIAN_POINT('Ctrl Pts',(3.31631129755346,-17.7406985030951,
695.03686588071));
#150931=CARTESIAN_POINT('Ctrl Pts',(1.67239348737615,-18.048,693.542748233651));
#150932=CARTESIAN_POINT('Ctrl Pts',(0.,-18.048,692.048630586592));
#150933=CARTESIAN_POINT('Ctrl Pts',(-1.67239348737615,-18.048,690.554512939533));
#150934=CARTESIAN_POINT('Ctrl Pts',(-3.31631129755346,-17.7406985030951,
689.060395292475));
#150935=CARTESIAN_POINT('Ctrl Pts',(-4.96022910773077,-17.4333970061901,
687.566277645416));
#150936=CARTESIAN_POINT('Ctrl Pts',(-6.51968959134574,-16.8292587962898,
686.072159998357));
#150937=CARTESIAN_POINT('Ctrl Pts',(-8.07915007496071,-16.2251205863895,
684.578042351298));
#150938=CARTESIAN_POINT('Ctrl Pts',(-9.50104767561052,-15.3447188656481,
683.083924704239));
#150939=CARTESIAN_POINT('Ctrl Pts',(-10.9229452762603,-14.4643171449067,
681.589807057181));
#150940=CARTESIAN_POINT('Ctrl Pts',(-12.1588589765331,-13.3376329379985,
680.095689410122));
#150941=CARTESIAN_POINT('Ctrl Pts',(-13.3947726768058,-12.2109487310903,
678.601571763063));
#150942=CARTESIAN_POINT('Ctrl Pts',(-14.4026149179538,-10.8763499173728,
677.107454116004));
#150943=CARTESIAN_POINT('Ctrl Pts',(-15.4104571591017,-9.54175110365538,
675.613336468945));
#150944=CARTESIAN_POINT('Ctrl Pts',(-16.1559070823762,-8.04468584505497,
674.119218821887));
#150945=CARTESIAN_POINT('Ctrl Pts',(-16.9013570056506,-6.54762058645456,
672.625101174828));
#150946=CARTESIAN_POINT('Ctrl Pts',(-17.3590292079831,-4.93906964482095,
671.130983527769));
#150947=CARTESIAN_POINT('Ctrl Pts',(-17.8167014103155,-3.33051870318735,
669.63686588071));
#150948=CARTESIAN_POINT('Ctrl Pts',(-17.9710104137728,-1.66525935159368,
668.142748233651));
#150949=CARTESIAN_POINT('Ctrl Pts',(-18.1253194172301,-1.10985572039171E-15,
666.648630586592));
#150950=CARTESIAN_POINT('Ctrl Pts',(-17.9710104137728,1.66525935159367,
665.154512939533));
#150951=CARTESIAN_POINT('Ctrl Pts',(-17.8167014103155,3.33051870318735,
663.660395292475));
#150952=CARTESIAN_POINT('Ctrl Pts',(-17.3590292079831,4.93906964482096,
662.166277645416));
#150953=CARTESIAN_POINT('Ctrl Pts',(-16.9013570056506,6.54762058645456,
660.672159998357));
#150954=CARTESIAN_POINT('Ctrl Pts',(-16.1559070823762,8.04468584505497,
659.178042351298));
#150955=CARTESIAN_POINT('Ctrl Pts',(-15.4104571591017,9.54175110365538,
657.68392470424));
#150956=CARTESIAN_POINT('Ctrl Pts',(-14.4026149179538,10.8763499173728,
656.18980705718));
#150957=CARTESIAN_POINT('Ctrl Pts',(-13.3947726768058,12.2109487310903,
654.695689410122));
#150958=CARTESIAN_POINT('Ctrl Pts',(-12.1588589765331,13.3376329379985,
653.201571763063));
#150959=CARTESIAN_POINT('Ctrl Pts',(-10.9229452762603,14.4643171449067,
651.707454116004));
#150960=CARTESIAN_POINT('Ctrl Pts',(-9.50104767561052,15.3447188656481,
650.213336468945));
#150961=CARTESIAN_POINT('Ctrl Pts',(-8.07915007496071,16.2251205863895,
648.719218821886));
#150962=CARTESIAN_POINT('Ctrl Pts',(-6.51968959134574,16.8292587962898,
647.225101174828));
#150963=CARTESIAN_POINT('Ctrl Pts',(-4.96022910773078,17.4333970061901,
645.730983527769));
#150964=CARTESIAN_POINT('Ctrl Pts',(-3.31631129755346,17.7406985030951,
644.23686588071));
#150965=CARTESIAN_POINT('Ctrl Pts',(-1.67239348737615,18.048,642.742748233651));
#150966=CARTESIAN_POINT('Ctrl Pts',(-2.21024254310115E-15,18.048,641.248630586592));
#150967=CARTESIAN_POINT('Ctrl Pts',(1.67239348737616,18.048,639.754512939533));
#150968=CARTESIAN_POINT('Ctrl Pts',(3.31631129755346,17.7406985030951,638.260395292475));
#150969=CARTESIAN_POINT('Ctrl Pts',(4.96022910773077,17.4333970061901,636.766277645416));
#150970=CARTESIAN_POINT('Ctrl Pts',(6.51968959134575,16.8292587962898,635.272159998357));
#150971=CARTESIAN_POINT('Ctrl Pts',(8.07915007496071,16.2251205863895,633.778042351298));
#150972=CARTESIAN_POINT('Ctrl Pts',(9.50104767561053,15.3447188656481,632.283924704239));
#150973=CARTESIAN_POINT('Ctrl Pts',(10.9229452762603,14.4643171449067,630.78980705718));
#150974=CARTESIAN_POINT('Ctrl Pts',(12.1588589765331,13.3376329379985,629.295689410122));
#150975=CARTESIAN_POINT('Ctrl Pts',(13.3947726768058,12.2109487310903,627.801571763063));
#150976=CARTESIAN_POINT('Ctrl Pts',(14.4026149179538,10.8763499173728,626.307454116004));
#150977=CARTESIAN_POINT('Ctrl Pts',(15.4104571591017,9.54175110365538,624.813336468945));
#150978=CARTESIAN_POINT('Ctrl Pts',(16.1559070823762,8.04468584505496,623.319218821886));
#150979=CARTESIAN_POINT('Ctrl Pts',(16.9013570056506,6.54762058645456,621.825101174828));
#150980=CARTESIAN_POINT('Ctrl Pts',(17.3590292079831,4.93906964482096,620.330983527769));
#150981=CARTESIAN_POINT('Ctrl Pts',(17.8167014103155,3.33051870318735,618.83686588071));
#150982=CARTESIAN_POINT('Ctrl Pts',(17.9710104137728,1.66525935159367,617.342748233651));
#150983=CARTESIAN_POINT('Ctrl Pts',(18.1253194172301,3.32956716117513E-15,
615.848630586592));
#150984=CARTESIAN_POINT('Ctrl Pts',(17.9710104137728,-1.66525935159367,
614.354512939533));
#150985=CARTESIAN_POINT('Ctrl Pts',(17.8167014103155,-3.33051870318736,
612.860395292475));
#150986=CARTESIAN_POINT('Ctrl Pts',(17.3590292079831,-4.93906964482095,
611.366277645416));
#150987=CARTESIAN_POINT('Ctrl Pts',(16.9013570056506,-6.54762058645456,
609.872159998357));
#150988=CARTESIAN_POINT('Ctrl Pts',(16.1559070823762,-8.04468584505497,
608.378042351298));
#150989=CARTESIAN_POINT('Ctrl Pts',(15.4104571591017,-9.54175110365538,
606.88392470424));
#150990=CARTESIAN_POINT('Ctrl Pts',(14.4026149179538,-10.8763499173728,
605.389807057181));
#150991=CARTESIAN_POINT('Ctrl Pts',(13.3947726768058,-12.2109487310903,
603.895689410122));
#150992=CARTESIAN_POINT('Ctrl Pts',(12.1588589765331,-13.3376329379985,
602.401571763063));
#150993=CARTESIAN_POINT('Ctrl Pts',(10.9229452762603,-14.4643171449067,
600.907454116004));
#150994=CARTESIAN_POINT('Ctrl Pts',(9.50104767561053,-15.3447188656481,
599.413336468945));
#150995=CARTESIAN_POINT('Ctrl Pts',(8.07915007496071,-16.2251205863895,
597.919218821887));
#150996=CARTESIAN_POINT('Ctrl Pts',(6.51968959134574,-16.8292587962898,
596.425101174828));
#150997=CARTESIAN_POINT('Ctrl Pts',(4.96022910773078,-17.4333970061901,
594.930983527769));
#150998=CARTESIAN_POINT('Ctrl Pts',(3.31631129755346,-17.7406985030951,
593.43686588071));
#150999=CARTESIAN_POINT('Ctrl Pts',(1.67239348737615,-18.048,591.942748233651));
#151000=CARTESIAN_POINT('Ctrl Pts',(0.,-18.048,590.448630586592));
#151001=CARTESIAN_POINT('Ctrl Pts',(-1.67239348737615,-18.048,588.954512939533));
#151002=CARTESIAN_POINT('Ctrl Pts',(-3.31631129755346,-17.7406985030951,
587.460395292475));
#151003=CARTESIAN_POINT('Ctrl Pts',(-4.96022910773077,-17.4333970061901,
585.966277645416));
#151004=CARTESIAN_POINT('Ctrl Pts',(-6.51968959134574,-16.8292587962898,
584.472159998357));
#151005=CARTESIAN_POINT('Ctrl Pts',(-8.07915007496071,-16.2251205863895,
582.978042351298));
#151006=CARTESIAN_POINT('Ctrl Pts',(-9.50104767561052,-15.3447188656481,
581.483924704239));
#151007=CARTESIAN_POINT('Ctrl Pts',(-10.9229452762603,-14.4643171449067,
579.989807057181));
#151008=CARTESIAN_POINT('Ctrl Pts',(-12.1588589765331,-13.3376329379985,
578.495689410122));
#151009=CARTESIAN_POINT('Ctrl Pts',(-13.3947726768058,-12.2109487310903,
577.001571763063));
#151010=CARTESIAN_POINT('Ctrl Pts',(-14.4026149179538,-10.8763499173728,
575.507454116004));
#151011=CARTESIAN_POINT('Ctrl Pts',(-15.4104571591017,-9.54175110365538,
574.013336468945));
#151012=CARTESIAN_POINT('Ctrl Pts',(-16.1559070823762,-8.04468584505497,
572.519218821886));
#151013=CARTESIAN_POINT('Ctrl Pts',(-16.9013570056506,-6.54762058645456,
571.025101174828));
#151014=CARTESIAN_POINT('Ctrl Pts',(-17.3590292079831,-4.93906964482095,
569.530983527769));
#151015=CARTESIAN_POINT('Ctrl Pts',(-17.8167014103155,-3.33051870318735,
568.03686588071));
#151016=CARTESIAN_POINT('Ctrl Pts',(-17.9710104137728,-1.66525935159368,
566.542748233651));
#151017=CARTESIAN_POINT('Ctrl Pts',(-18.1253194172301,-1.10985572039171E-15,
565.048630586592));
#151018=CARTESIAN_POINT('Ctrl Pts',(-17.9710104137728,1.66525935159367,
563.554512939533));
#151019=CARTESIAN_POINT('Ctrl Pts',(-17.8167014103155,3.33051870318735,
562.060395292475));
#151020=CARTESIAN_POINT('Ctrl Pts',(-17.3590292079831,4.93906964482096,
560.566277645416));
#151021=CARTESIAN_POINT('Ctrl Pts',(-16.9013570056506,6.54762058645456,
559.072159998357));
#151022=CARTESIAN_POINT('Ctrl Pts',(-16.1559070823762,8.04468584505497,
557.578042351298));
#151023=CARTESIAN_POINT('Ctrl Pts',(-15.4104571591017,9.54175110365538,
556.083924704239));
#151024=CARTESIAN_POINT('Ctrl Pts',(-14.4026149179538,10.8763499173728,
554.589807057181));
#151025=CARTESIAN_POINT('Ctrl Pts',(-13.3947726768058,12.2109487310903,
553.095689410122));
#151026=CARTESIAN_POINT('Ctrl Pts',(-12.1588589765331,13.3376329379985,
551.601571763063));
#151027=CARTESIAN_POINT('Ctrl Pts',(-10.9229452762603,14.4643171449067,
550.107454116004));
#151028=CARTESIAN_POINT('Ctrl Pts',(-9.50104767561052,15.3447188656481,
548.613336468945));
#151029=CARTESIAN_POINT('Ctrl Pts',(-8.07915007496071,16.2251205863895,
547.119218821887));
#151030=CARTESIAN_POINT('Ctrl Pts',(-6.51968959134574,16.8292587962898,
545.625101174828));
#151031=CARTESIAN_POINT('Ctrl Pts',(-4.96022910773078,17.4333970061901,
544.130983527769));
#151032=CARTESIAN_POINT('Ctrl Pts',(-3.31631129755346,17.7406985030951,
542.63686588071));
#151033=CARTESIAN_POINT('Ctrl Pts',(-1.67239348737615,18.048,541.142748233651));
#151034=CARTESIAN_POINT('Ctrl Pts',(-2.21024254310115E-15,18.048,539.648630586592));
#151035=CARTESIAN_POINT('Ctrl Pts',(1.67239348737616,18.048,538.154512939533));
#151036=CARTESIAN_POINT('Ctrl Pts',(3.31631129755346,17.7406985030951,536.660395292475));
#151037=CARTESIAN_POINT('Ctrl Pts',(4.96022910773077,17.4333970061901,535.166277645416));
#151038=CARTESIAN_POINT('Ctrl Pts',(6.51968959134575,16.8292587962898,533.672159998357));
#151039=CARTESIAN_POINT('Ctrl Pts',(8.07915007496071,16.2251205863895,532.178042351298));
#151040=CARTESIAN_POINT('Ctrl Pts',(9.50104767561053,15.3447188656481,530.683924704239));
#151041=CARTESIAN_POINT('Ctrl Pts',(10.9229452762603,14.4643171449067,529.18980705718));
#151042=CARTESIAN_POINT('Ctrl Pts',(12.1588589765331,13.3376329379985,527.695689410122));
#151043=CARTESIAN_POINT('Ctrl Pts',(13.3947726768058,12.2109487310903,526.201571763063));
#151044=CARTESIAN_POINT('Ctrl Pts',(14.4026149179538,10.8763499173728,524.707454116004));
#151045=CARTESIAN_POINT('Ctrl Pts',(15.4104571591017,9.54175110365538,523.213336468945));
#151046=CARTESIAN_POINT('Ctrl Pts',(16.1559070823762,8.04468584505496,521.719218821886));
#151047=CARTESIAN_POINT('Ctrl Pts',(16.9013570056506,6.54762058645456,520.225101174828));
#151048=CARTESIAN_POINT('Ctrl Pts',(17.3590292079831,4.93906964482096,518.730983527769));
#151049=CARTESIAN_POINT('Ctrl Pts',(17.8167014103155,3.33051870318735,517.23686588071));
#151050=CARTESIAN_POINT('Ctrl Pts',(17.9710104137728,1.66525935159367,515.742748233651));
#151051=CARTESIAN_POINT('Ctrl Pts',(18.1253194172301,3.32956716117513E-15,
514.248630586592));
#151052=CARTESIAN_POINT('Ctrl Pts',(17.9710104137728,-1.66525935159367,
512.754512939533));
#151053=CARTESIAN_POINT('Ctrl Pts',(17.8167014103155,-3.33051870318736,
511.260395292475));
#151054=CARTESIAN_POINT('Ctrl Pts',(17.3590292079831,-4.93906964482095,
509.766277645416));
#151055=CARTESIAN_POINT('Ctrl Pts',(16.9013570056506,-6.54762058645456,
508.272159998357));
#151056=CARTESIAN_POINT('Ctrl Pts',(16.1559070823762,-8.04468584505497,
506.778042351298));
#151057=CARTESIAN_POINT('Ctrl Pts',(15.4104571591017,-9.54175110365538,
505.283924704239));
#151058=CARTESIAN_POINT('Ctrl Pts',(14.4026149179538,-10.8763499173728,
503.78980705718));
#151059=CARTESIAN_POINT('Ctrl Pts',(13.3947726768058,-12.2109487310903,
502.295689410122));
#151060=CARTESIAN_POINT('Ctrl Pts',(12.1588589765331,-13.3376329379985,
500.801571763063));
#151061=CARTESIAN_POINT('Ctrl Pts',(10.9229452762603,-14.4643171449067,
499.307454116004));
#151062=CARTESIAN_POINT('Ctrl Pts',(9.50104767561053,-15.3447188656481,
497.813336468945));
#151063=CARTESIAN_POINT('Ctrl Pts',(8.07915007496071,-16.2251205863895,
496.319218821886));
#151064=CARTESIAN_POINT('Ctrl Pts',(6.51968959134574,-16.8292587962898,
494.825101174827));
#151065=CARTESIAN_POINT('Ctrl Pts',(4.96022910773078,-17.4333970061901,
493.330983527769));
#151066=CARTESIAN_POINT('Ctrl Pts',(3.31631129755346,-17.7406985030951,
491.83686588071));
#151067=CARTESIAN_POINT('Ctrl Pts',(1.67239348737615,-18.048,490.342748233651));
#151068=CARTESIAN_POINT('Ctrl Pts',(0.,-18.048,488.848630586592));
#151069=CARTESIAN_POINT('Ctrl Pts',(-1.67239348737615,-18.048,487.354512939533));
#151070=CARTESIAN_POINT('Ctrl Pts',(-3.31631129755346,-17.7406985030951,
485.860395292475));
#151071=CARTESIAN_POINT('Ctrl Pts',(-4.96022910773077,-17.4333970061901,
484.366277645416));
#151072=CARTESIAN_POINT('Ctrl Pts',(-6.51968959134574,-16.8292587962898,
482.872159998357));
#151073=CARTESIAN_POINT('Ctrl Pts',(-8.07915007496071,-16.2251205863895,
481.378042351298));
#151074=CARTESIAN_POINT('Ctrl Pts',(-9.50104767561052,-15.3447188656481,
479.883924704239));
#151075=CARTESIAN_POINT('Ctrl Pts',(-10.9229452762603,-14.4643171449067,
478.389807057181));
#151076=CARTESIAN_POINT('Ctrl Pts',(-12.1588589765331,-13.3376329379985,
476.895689410122));
#151077=CARTESIAN_POINT('Ctrl Pts',(-13.3947726768058,-12.2109487310903,
475.401571763063));
#151078=CARTESIAN_POINT('Ctrl Pts',(-14.4026149179538,-10.8763499173728,
473.907454116004));
#151079=CARTESIAN_POINT('Ctrl Pts',(-15.4104571591017,-9.54175110365538,
472.413336468945));
#151080=CARTESIAN_POINT('Ctrl Pts',(-16.1559070823762,-8.04468584505497,
470.919218821886));
#151081=CARTESIAN_POINT('Ctrl Pts',(-16.9013570056506,-6.54762058645456,
469.425101174828));
#151082=CARTESIAN_POINT('Ctrl Pts',(-17.3590292079831,-4.93906964482095,
467.930983527769));
#151083=CARTESIAN_POINT('Ctrl Pts',(-17.8167014103155,-3.33051870318735,
466.43686588071));
#151084=CARTESIAN_POINT('Ctrl Pts',(-17.9710104137728,-1.66525935159368,
464.942748233651));
#151085=CARTESIAN_POINT('Ctrl Pts',(-18.1253194172301,-1.10985572039171E-15,
463.448630586592));
#151086=CARTESIAN_POINT('Ctrl Pts',(-17.9710104137728,1.66525935159367,
461.954512939534));
#151087=CARTESIAN_POINT('Ctrl Pts',(-17.8167014103155,3.33051870318735,
460.460395292475));
#151088=CARTESIAN_POINT('Ctrl Pts',(-17.3590292079831,4.93906964482096,
458.966277645416));
#151089=CARTESIAN_POINT('Ctrl Pts',(-16.9013570056506,6.54762058645456,
457.472159998357));
#151090=CARTESIAN_POINT('Ctrl Pts',(-16.1559070823762,8.04468584505497,
455.978042351298));
#151091=CARTESIAN_POINT('Ctrl Pts',(-15.4104571591017,9.54175110365538,
454.483924704239));
#151092=CARTESIAN_POINT('Ctrl Pts',(-14.4026149179538,10.8763499173728,
452.989807057181));
#151093=CARTESIAN_POINT('Ctrl Pts',(-13.3947726768058,12.2109487310903,
451.495689410122));
#151094=CARTESIAN_POINT('Ctrl Pts',(-12.1588589765331,13.3376329379985,
450.001571763063));
#151095=CARTESIAN_POINT('Ctrl Pts',(-10.9229452762603,14.4643171449067,
448.507454116004));
#151096=CARTESIAN_POINT('Ctrl Pts',(-9.50104767561052,15.3447188656481,
447.013336468945));
#151097=CARTESIAN_POINT('Ctrl Pts',(-8.07915007496071,16.2251205863895,
445.519218821887));
#151098=CARTESIAN_POINT('Ctrl Pts',(-6.51968959134574,16.8292587962898,
444.025101174828));
#151099=CARTESIAN_POINT('Ctrl Pts',(-4.96022910773078,17.4333970061901,
442.530983527769));
#151100=CARTESIAN_POINT('Ctrl Pts',(-3.31631129755346,17.7406985030951,
441.03686588071));
#151101=CARTESIAN_POINT('Ctrl Pts',(-1.67239348737615,18.048,439.542748233651));
#151102=CARTESIAN_POINT('Ctrl Pts',(-2.21024254310115E-15,18.048,438.048630586592));
#151103=CARTESIAN_POINT('Ctrl Pts',(1.67239348737616,18.048,436.554512939533));
#151104=CARTESIAN_POINT('Ctrl Pts',(3.31631129755346,17.7406985030951,435.060395292475));
#151105=CARTESIAN_POINT('Ctrl Pts',(4.96022910773077,17.4333970061901,433.566277645416));
#151106=CARTESIAN_POINT('Ctrl Pts',(6.51968959134575,16.8292587962898,432.072159998357));
#151107=CARTESIAN_POINT('Ctrl Pts',(8.07915007496071,16.2251205863895,430.578042351298));
#151108=CARTESIAN_POINT('Ctrl Pts',(9.50104767561053,15.3447188656481,429.083924704239));
#151109=CARTESIAN_POINT('Ctrl Pts',(10.9229452762603,14.4643171449067,427.58980705718));
#151110=CARTESIAN_POINT('Ctrl Pts',(12.1588589765331,13.3376329379985,426.095689410122));
#151111=CARTESIAN_POINT('Ctrl Pts',(13.3947726768058,12.2109487310903,424.601571763063));
#151112=CARTESIAN_POINT('Ctrl Pts',(14.4026149179538,10.8763499173728,423.107454116004));
#151113=CARTESIAN_POINT('Ctrl Pts',(15.4104571591017,9.54175110365538,421.613336468945));
#151114=CARTESIAN_POINT('Ctrl Pts',(16.1559070823762,8.04468584505496,420.119218821886));
#151115=CARTESIAN_POINT('Ctrl Pts',(16.9013570056506,6.54762058645456,418.625101174828));
#151116=CARTESIAN_POINT('Ctrl Pts',(17.3590292079831,4.93906964482096,417.130983527769));
#151117=CARTESIAN_POINT('Ctrl Pts',(17.8167014103155,3.33051870318735,415.63686588071));
#151118=CARTESIAN_POINT('Ctrl Pts',(17.9710104137728,1.66525935159367,414.142748233651));
#151119=CARTESIAN_POINT('Ctrl Pts',(18.1253194172301,3.32956716117513E-15,
412.648630586592));
#151120=CARTESIAN_POINT('Ctrl Pts',(17.9710104137728,-1.66525935159367,
411.154512939534));
#151121=CARTESIAN_POINT('Ctrl Pts',(17.8167014103155,-3.33051870318736,
409.660395292475));
#151122=CARTESIAN_POINT('Ctrl Pts',(17.3590292079831,-4.93906964482095,
408.166277645416));
#151123=CARTESIAN_POINT('Ctrl Pts',(16.9013570056506,-6.54762058645456,
406.672159998357));
#151124=CARTESIAN_POINT('Ctrl Pts',(16.1559070823762,-8.04468584505497,
405.178042351298));
#151125=CARTESIAN_POINT('Ctrl Pts',(15.4104571591017,-9.54175110365538,
403.683924704239));
#151126=CARTESIAN_POINT('Ctrl Pts',(14.4026149179538,-10.8763499173728,
402.189807057181));
#151127=CARTESIAN_POINT('Ctrl Pts',(13.3947726768058,-12.2109487310903,
400.695689410122));
#151128=CARTESIAN_POINT('Ctrl Pts',(12.1588589765331,-13.3376329379985,
399.201571763063));
#151129=CARTESIAN_POINT('Ctrl Pts',(10.9229452762603,-14.4643171449067,
397.707454116004));
#151130=CARTESIAN_POINT('Ctrl Pts',(9.50104767561053,-15.3447188656481,
396.213336468945));
#151131=CARTESIAN_POINT('Ctrl Pts',(8.07915007496071,-16.2251205863895,
394.719218821887));
#151132=CARTESIAN_POINT('Ctrl Pts',(6.51968959134574,-16.8292587962898,
393.225101174828));
#151133=CARTESIAN_POINT('Ctrl Pts',(4.96022910773078,-17.4333970061901,
391.730983527769));
#151134=CARTESIAN_POINT('Ctrl Pts',(3.31631129755346,-17.7406985030951,
390.23686588071));
#151135=CARTESIAN_POINT('Ctrl Pts',(1.67239348737615,-18.048,388.742748233651));
#151136=CARTESIAN_POINT('Ctrl Pts',(0.,-18.048,387.248630586592));
#151137=CARTESIAN_POINT('Ctrl Pts',(-1.67239348737615,-18.048,385.754512939533));
#151138=CARTESIAN_POINT('Ctrl Pts',(-3.31631129755346,-17.7406985030951,
384.260395292475));
#151139=CARTESIAN_POINT('Ctrl Pts',(-4.96022910773077,-17.4333970061901,
382.766277645416));
#151140=CARTESIAN_POINT('Ctrl Pts',(-6.51968959134574,-16.8292587962898,
381.272159998357));
#151141=CARTESIAN_POINT('Ctrl Pts',(-8.07915007496071,-16.2251205863895,
379.778042351298));
#151142=CARTESIAN_POINT('Ctrl Pts',(-9.50104767561052,-15.3447188656481,
378.283924704239));
#151143=CARTESIAN_POINT('Ctrl Pts',(-10.9229452762603,-14.4643171449067,
376.789807057181));
#151144=CARTESIAN_POINT('Ctrl Pts',(-12.1588589765331,-13.3376329379985,
375.295689410122));
#151145=CARTESIAN_POINT('Ctrl Pts',(-13.3947726768058,-12.2109487310903,
373.801571763063));
#151146=CARTESIAN_POINT('Ctrl Pts',(-14.4026149179538,-10.8763499173728,
372.307454116004));
#151147=CARTESIAN_POINT('Ctrl Pts',(-15.4104571591017,-9.54175110365538,
370.813336468945));
#151148=CARTESIAN_POINT('Ctrl Pts',(-16.1559070823762,-8.04468584505497,
369.319218821886));
#151149=CARTESIAN_POINT('Ctrl Pts',(-16.9013570056506,-6.54762058645456,
367.825101174827));
#151150=CARTESIAN_POINT('Ctrl Pts',(-17.3590292079831,-4.93906964482095,
366.330983527769));
#151151=CARTESIAN_POINT('Ctrl Pts',(-17.8167014103155,-3.33051870318735,
364.83686588071));
#151152=CARTESIAN_POINT('Ctrl Pts',(-17.9710104137728,-1.66525935159368,
363.342748233651));
#151153=CARTESIAN_POINT('Ctrl Pts',(-18.1253194172301,-1.10985572039171E-15,
361.848630586592));
#151154=CARTESIAN_POINT('Ctrl Pts',(-17.9710104137728,1.66525935159367,
360.354512939533));
#151155=CARTESIAN_POINT('Ctrl Pts',(-17.8167014103155,3.33051870318735,
358.860395292475));
#151156=CARTESIAN_POINT('Ctrl Pts',(-17.3590292079831,4.93906964482096,
357.366277645416));
#151157=CARTESIAN_POINT('Ctrl Pts',(-16.9013570056506,6.54762058645456,
355.872159998357));
#151158=CARTESIAN_POINT('Ctrl Pts',(-16.1559070823762,8.04468584505497,
354.378042351298));
#151159=CARTESIAN_POINT('Ctrl Pts',(-15.4104571591017,9.54175110365538,
352.883924704239));
#151160=CARTESIAN_POINT('Ctrl Pts',(-14.4026149179538,10.8763499173728,
351.389807057181));
#151161=CARTESIAN_POINT('Ctrl Pts',(-13.3947726768058,12.2109487310903,
349.895689410122));
#151162=CARTESIAN_POINT('Ctrl Pts',(-12.1588589765331,13.3376329379985,
348.401571763063));
#151163=CARTESIAN_POINT('Ctrl Pts',(-10.9229452762603,14.4643171449067,
346.907454116004));
#151164=CARTESIAN_POINT('Ctrl Pts',(-9.50104767561052,15.3447188656481,
345.413336468945));
#151165=CARTESIAN_POINT('Ctrl Pts',(-8.07915007496071,16.2251205863895,
343.919218821887));
#151166=CARTESIAN_POINT('Ctrl Pts',(-6.51968959134574,16.8292587962898,
342.425101174828));
#151167=CARTESIAN_POINT('Ctrl Pts',(-4.96022910773078,17.4333970061901,
340.930983527769));
#151168=CARTESIAN_POINT('Ctrl Pts',(-3.31631129755346,17.7406985030951,
339.43686588071));
#151169=CARTESIAN_POINT('Ctrl Pts',(-1.67239348737615,18.048,337.942748233651));
#151170=CARTESIAN_POINT('Ctrl Pts',(-2.21024254310115E-15,18.048,336.448630586592));
#151171=CARTESIAN_POINT('Ctrl Pts',(1.67239348737616,18.048,334.954512939533));
#151172=CARTESIAN_POINT('Ctrl Pts',(3.31631129755346,17.7406985030951,333.460395292475));
#151173=CARTESIAN_POINT('Ctrl Pts',(4.96022910773077,17.4333970061901,331.966277645416));
#151174=CARTESIAN_POINT('Ctrl Pts',(6.51968959134575,16.8292587962898,330.472159998357));
#151175=CARTESIAN_POINT('Ctrl Pts',(8.07915007496071,16.2251205863895,328.978042351298));
#151176=CARTESIAN_POINT('Ctrl Pts',(9.50104767561053,15.3447188656481,327.483924704239));
#151177=CARTESIAN_POINT('Ctrl Pts',(10.9229452762603,14.4643171449067,325.98980705718));
#151178=CARTESIAN_POINT('Ctrl Pts',(12.1588589765331,13.3376329379985,324.495689410122));
#151179=CARTESIAN_POINT('Ctrl Pts',(13.3947726768058,12.2109487310903,323.001571763063));
#151180=CARTESIAN_POINT('Ctrl Pts',(14.4026149179538,10.8763499173728,321.507454116004));
#151181=CARTESIAN_POINT('Ctrl Pts',(15.4104571591017,9.54175110365538,320.013336468945));
#151182=CARTESIAN_POINT('Ctrl Pts',(16.1559070823762,8.04468584505496,318.519218821886));
#151183=CARTESIAN_POINT('Ctrl Pts',(16.9013570056506,6.54762058645456,317.025101174828));
#151184=CARTESIAN_POINT('Ctrl Pts',(17.3590292079831,4.93906964482096,315.530983527769));
#151185=CARTESIAN_POINT('Ctrl Pts',(17.8167014103155,3.33051870318735,314.03686588071));
#151186=CARTESIAN_POINT('Ctrl Pts',(17.9710104137728,1.66525935159367,312.542748233651));
#151187=CARTESIAN_POINT('Ctrl Pts',(18.1253194172301,3.32956716117513E-15,
311.048630586592));
#151188=CARTESIAN_POINT('Ctrl Pts',(17.9710104137728,-1.66525935159367,
309.554512939533));
#151189=CARTESIAN_POINT('Ctrl Pts',(17.8167014103155,-3.33051870318736,
308.060395292475));
#151190=CARTESIAN_POINT('Ctrl Pts',(17.3590292079831,-4.93906964482095,
306.566277645416));
#151191=CARTESIAN_POINT('Ctrl Pts',(16.9013570056506,-6.54762058645456,
305.072159998357));
#151192=CARTESIAN_POINT('Ctrl Pts',(16.1559070823762,-8.04468584505497,
303.578042351298));
#151193=CARTESIAN_POINT('Ctrl Pts',(15.4104571591017,-9.54175110365538,
302.083924704239));
#151194=CARTESIAN_POINT('Ctrl Pts',(14.4026149179538,-10.8763499173728,
300.58980705718));
#151195=CARTESIAN_POINT('Ctrl Pts',(13.3947726768058,-12.2109487310903,
299.095689410122));
#151196=CARTESIAN_POINT('Ctrl Pts',(12.1588589765331,-13.3376329379985,
297.601571763063));
#151197=CARTESIAN_POINT('Ctrl Pts',(10.9229452762603,-14.4643171449067,
296.107454116004));
#151198=CARTESIAN_POINT('Ctrl Pts',(9.50104767561053,-15.3447188656481,
294.613336468945));
#151199=CARTESIAN_POINT('Ctrl Pts',(8.07915007496071,-16.2251205863895,
293.119218821886));
#151200=CARTESIAN_POINT('Ctrl Pts',(6.51968959134574,-16.8292587962898,
291.625101174828));
#151201=CARTESIAN_POINT('Ctrl Pts',(4.96022910773078,-17.4333970061901,
290.130983527769));
#151202=CARTESIAN_POINT('Ctrl Pts',(3.31631129755346,-17.7406985030951,
288.63686588071));
#151203=CARTESIAN_POINT('Ctrl Pts',(1.67239348737615,-18.048,287.142748233651));
#151204=CARTESIAN_POINT('Ctrl Pts',(0.,-18.048,285.648630586592));
#151205=CARTESIAN_POINT('Ctrl Pts',(-1.67239348737615,-18.048,284.154512939534));
#151206=CARTESIAN_POINT('Ctrl Pts',(-3.31631129755346,-17.7406985030951,
282.660395292475));
#151207=CARTESIAN_POINT('Ctrl Pts',(-4.96022910773077,-17.4333970061901,
281.166277645416));
#151208=CARTESIAN_POINT('Ctrl Pts',(-6.51968959134574,-16.8292587962898,
279.672159998357));
#151209=CARTESIAN_POINT('Ctrl Pts',(-8.07915007496071,-16.2251205863895,
278.178042351298));
#151210=CARTESIAN_POINT('Ctrl Pts',(-9.50104767561052,-15.3447188656481,
276.683924704239));
#151211=CARTESIAN_POINT('Ctrl Pts',(-10.9229452762603,-14.4643171449067,
275.189807057181));
#151212=CARTESIAN_POINT('Ctrl Pts',(-12.1588589765331,-13.3376329379985,
273.695689410122));
#151213=CARTESIAN_POINT('Ctrl Pts',(-13.3947726768058,-12.2109487310903,
272.201571763063));
#151214=CARTESIAN_POINT('Ctrl Pts',(-14.4026149179538,-10.8763499173728,
270.707454116004));
#151215=CARTESIAN_POINT('Ctrl Pts',(-15.4104571591017,-9.54175110365538,
269.213336468945));
#151216=CARTESIAN_POINT('Ctrl Pts',(-16.1559070823762,-8.04468584505497,
267.719218821886));
#151217=CARTESIAN_POINT('Ctrl Pts',(-16.9013570056506,-6.54762058645456,
266.225101174828));
#151218=CARTESIAN_POINT('Ctrl Pts',(-17.3590292079831,-4.93906964482095,
264.730983527769));
#151219=CARTESIAN_POINT('Ctrl Pts',(-17.8167014103155,-3.33051870318735,
263.23686588071));
#151220=CARTESIAN_POINT('Ctrl Pts',(-17.9710104137728,-1.66525935159368,
261.742748233651));
#151221=CARTESIAN_POINT('Ctrl Pts',(-18.1253194172301,-1.10985572039171E-15,
260.248630586592));
#151222=CARTESIAN_POINT('Ctrl Pts',(-17.9710104137728,1.66525935159367,
258.754512939533));
#151223=CARTESIAN_POINT('Ctrl Pts',(-17.8167014103155,3.33051870318735,
257.260395292475));
#151224=CARTESIAN_POINT('Ctrl Pts',(-17.3590292079831,4.93906964482096,
255.766277645416));
#151225=CARTESIAN_POINT('Ctrl Pts',(-16.9013570056506,6.54762058645456,
254.272159998357));
#151226=CARTESIAN_POINT('Ctrl Pts',(-16.1559070823762,8.04468584505497,
252.778042351298));
#151227=CARTESIAN_POINT('Ctrl Pts',(-15.4104571591017,9.54175110365538,
251.283924704239));
#151228=CARTESIAN_POINT('Ctrl Pts',(-14.4026149179538,10.8763499173728,
249.78980705718));
#151229=CARTESIAN_POINT('Ctrl Pts',(-13.3947726768058,12.2109487310903,
248.295689410122));
#151230=CARTESIAN_POINT('Ctrl Pts',(-12.1588589765331,13.3376329379985,
246.801571763063));
#151231=CARTESIAN_POINT('Ctrl Pts',(-10.9229452762603,14.4643171449067,
245.307454116004));
#151232=CARTESIAN_POINT('Ctrl Pts',(-9.50104767561052,15.3447188656481,
243.813336468945));
#151233=CARTESIAN_POINT('Ctrl Pts',(-8.07915007496071,16.2251205863895,
242.319218821886));
#151234=CARTESIAN_POINT('Ctrl Pts',(-6.51968959134574,16.8292587962898,
240.825101174827));
#151235=CARTESIAN_POINT('Ctrl Pts',(-4.96022910773078,17.4333970061901,
239.330983527769));
#151236=CARTESIAN_POINT('Ctrl Pts',(-3.31631129755346,17.7406985030951,
237.83686588071));
#151237=CARTESIAN_POINT('Ctrl Pts',(-1.67239348737615,18.048,236.342748233651));
#151238=CARTESIAN_POINT('Ctrl Pts',(-2.21024254310115E-15,18.048,234.848630586592));
#151239=CARTESIAN_POINT('Ctrl Pts',(1.67239348737616,18.048,233.354512939533));
#151240=CARTESIAN_POINT('Ctrl Pts',(3.31631129755346,17.7406985030951,231.860395292475));
#151241=CARTESIAN_POINT('Ctrl Pts',(4.96022910773077,17.4333970061901,230.366277645416));
#151242=CARTESIAN_POINT('Ctrl Pts',(6.51968959134575,16.8292587962898,228.872159998357));
#151243=CARTESIAN_POINT('Ctrl Pts',(8.07915007496071,16.2251205863895,227.378042351298));
#151244=CARTESIAN_POINT('Ctrl Pts',(9.50104767561053,15.3447188656481,225.883924704239));
#151245=CARTESIAN_POINT('Ctrl Pts',(10.9229452762603,14.4643171449067,224.389807057181));
#151246=CARTESIAN_POINT('Ctrl Pts',(12.1588589765331,13.3376329379985,222.895689410122));
#151247=CARTESIAN_POINT('Ctrl Pts',(13.3947726768058,12.2109487310903,221.401571763063));
#151248=CARTESIAN_POINT('Ctrl Pts',(14.4026149179538,10.8763499173728,219.907454116004));
#151249=CARTESIAN_POINT('Ctrl Pts',(15.4104571591017,9.54175110365538,218.413336468945));
#151250=CARTESIAN_POINT('Ctrl Pts',(16.1559070823762,8.04468584505496,216.919218821886));
#151251=CARTESIAN_POINT('Ctrl Pts',(16.9013570056506,6.54762058645456,215.425101174828));
#151252=CARTESIAN_POINT('Ctrl Pts',(17.3590292079831,4.93906964482096,213.930983527769));
#151253=CARTESIAN_POINT('Ctrl Pts',(17.8167014103155,3.33051870318735,212.43686588071));
#151254=CARTESIAN_POINT('Ctrl Pts',(17.9710104137728,1.66525935159367,210.942748233651));
#151255=CARTESIAN_POINT('Ctrl Pts',(18.1253194172301,3.32956716117513E-15,
209.448630586592));
#151256=CARTESIAN_POINT('Ctrl Pts',(17.9710104137728,-1.66525935159367,
207.954512939533));
#151257=CARTESIAN_POINT('Ctrl Pts',(17.8167014103155,-3.33051870318736,
206.460395292475));
#151258=CARTESIAN_POINT('Ctrl Pts',(17.3590292079831,-4.93906964482095,
204.966277645416));
#151259=CARTESIAN_POINT('Ctrl Pts',(16.9013570056506,-6.54762058645456,
203.472159998357));
#151260=CARTESIAN_POINT('Ctrl Pts',(16.1559070823762,-8.04468584505497,
201.978042351298));
#151261=CARTESIAN_POINT('Ctrl Pts',(15.4104571591017,-9.54175110365538,
200.483924704239));
#151262=CARTESIAN_POINT('Ctrl Pts',(14.4026149179538,-10.8763499173728,
198.989807057181));
#151263=CARTESIAN_POINT('Ctrl Pts',(13.3947726768058,-12.2109487310903,
197.495689410122));
#151264=CARTESIAN_POINT('Ctrl Pts',(12.1588589765331,-13.3376329379985,
196.001571763063));
#151265=CARTESIAN_POINT('Ctrl Pts',(10.9229452762603,-14.4643171449067,
194.507454116004));
#151266=CARTESIAN_POINT('Ctrl Pts',(9.50104767561053,-15.3447188656481,
193.013336468945));
#151267=CARTESIAN_POINT('Ctrl Pts',(8.07915007496071,-16.2251205863895,
191.519218821886));
#151268=CARTESIAN_POINT('Ctrl Pts',(6.51968959134574,-16.8292587962898,
190.025101174828));
#151269=CARTESIAN_POINT('Ctrl Pts',(4.96022910773078,-17.4333970061901,
188.530983527769));
#151270=CARTESIAN_POINT('Ctrl Pts',(3.31631129755346,-17.7406985030951,
187.03686588071));
#151271=CARTESIAN_POINT('Ctrl Pts',(1.67239348737615,-18.048,185.542748233651));
#151272=CARTESIAN_POINT('Ctrl Pts',(0.,-18.048,184.048630586592));
#151273=CARTESIAN_POINT('Ctrl Pts',(-1.67239348737615,-18.048,182.554512939533));
#151274=CARTESIAN_POINT('Ctrl Pts',(-3.31631129755346,-17.7406985030951,
181.060395292475));
#151275=CARTESIAN_POINT('Ctrl Pts',(-4.96022910773077,-17.4333970061901,
179.566277645416));
#151276=CARTESIAN_POINT('Ctrl Pts',(-6.51968959134574,-16.8292587962898,
178.072159998357));
#151277=CARTESIAN_POINT('Ctrl Pts',(-8.07915007496071,-16.2251205863895,
176.578042351298));
#151278=CARTESIAN_POINT('Ctrl Pts',(-9.50104767561052,-15.3447188656481,
175.083924704239));
#151279=CARTESIAN_POINT('Ctrl Pts',(-10.9229452762603,-14.4643171449067,
173.58980705718));
#151280=CARTESIAN_POINT('Ctrl Pts',(-12.1588589765331,-13.3376329379985,
172.095689410122));
#151281=CARTESIAN_POINT('Ctrl Pts',(-13.3947726768058,-12.2109487310903,
170.601571763063));
#151282=CARTESIAN_POINT('Ctrl Pts',(-14.4026149179538,-10.8763499173728,
169.107454116004));
#151283=CARTESIAN_POINT('Ctrl Pts',(-15.4104571591017,-9.54175110365538,
167.613336468945));
#151284=CARTESIAN_POINT('Ctrl Pts',(-16.1559070823762,-8.04468584505497,
166.119218821886));
#151285=CARTESIAN_POINT('Ctrl Pts',(-16.9013570056506,-6.54762058645456,
164.625101174828));
#151286=CARTESIAN_POINT('Ctrl Pts',(-17.3590292079831,-4.93906964482095,
163.130983527769));
#151287=CARTESIAN_POINT('Ctrl Pts',(-17.8167014103155,-3.33051870318735,
161.63686588071));
#151288=CARTESIAN_POINT('Ctrl Pts',(-17.9710104137728,-1.66525935159368,
160.142748233651));
#151289=CARTESIAN_POINT('Ctrl Pts',(-18.1253194172301,-1.10985572039171E-15,
158.648630586592));
#151290=CARTESIAN_POINT('Ctrl Pts',(-17.9710104137728,1.66525935159367,
157.154512939534));
#151291=CARTESIAN_POINT('Ctrl Pts',(-17.8167014103155,3.33051870318735,
155.660395292475));
#151292=CARTESIAN_POINT('Ctrl Pts',(-17.3590292079831,4.93906964482096,
154.166277645416));
#151293=CARTESIAN_POINT('Ctrl Pts',(-16.9013570056506,6.54762058645456,
152.672159998357));
#151294=CARTESIAN_POINT('Ctrl Pts',(-16.1559070823762,8.04468584505497,
151.178042351298));
#151295=CARTESIAN_POINT('Ctrl Pts',(-15.4104571591017,9.54175110365538,
149.683924704239));
#151296=CARTESIAN_POINT('Ctrl Pts',(-14.4026149179538,10.8763499173728,
148.189807057181));
#151297=CARTESIAN_POINT('Ctrl Pts',(-13.3947726768058,12.2109487310903,
146.695689410122));
#151298=CARTESIAN_POINT('Ctrl Pts',(-12.1588589765331,13.3376329379985,
145.201571763063));
#151299=CARTESIAN_POINT('Ctrl Pts',(-10.9229452762603,14.4643171449067,
143.707454116004));
#151300=CARTESIAN_POINT('Ctrl Pts',(-9.50104767561052,15.3447188656481,
142.213336468945));
#151301=CARTESIAN_POINT('Ctrl Pts',(-8.07915007496071,16.2251205863895,
140.719218821886));
#151302=CARTESIAN_POINT('Ctrl Pts',(-6.51968959134574,16.8292587962898,
139.225101174828));
#151303=CARTESIAN_POINT('Ctrl Pts',(-4.96022910773078,17.4333970061901,
137.730983527769));
#151304=CARTESIAN_POINT('Ctrl Pts',(-3.31631129755346,17.7406985030951,
136.23686588071));
#151305=CARTESIAN_POINT('Ctrl Pts',(-1.67239348737615,18.048,134.742748233651));
#151306=CARTESIAN_POINT('Ctrl Pts',(-2.21024254310115E-15,18.048,133.248630586592));
#151307=CARTESIAN_POINT('Ctrl Pts',(1.67239348737616,18.048,131.754512939533));
#151308=CARTESIAN_POINT('Ctrl Pts',(3.31631129755346,17.7406985030951,130.260395292475));
#151309=CARTESIAN_POINT('Ctrl Pts',(4.96022910773077,17.4333970061901,128.766277645416));
#151310=CARTESIAN_POINT('Ctrl Pts',(6.51968959134575,16.8292587962898,127.272159998357));
#151311=CARTESIAN_POINT('Ctrl Pts',(8.07915007496071,16.2251205863895,125.778042351298));
#151312=CARTESIAN_POINT('Ctrl Pts',(9.50104767561053,15.3447188656481,124.283924704239));
#151313=CARTESIAN_POINT('Ctrl Pts',(10.9229452762603,14.4643171449067,122.78980705718));
#151314=CARTESIAN_POINT('Ctrl Pts',(12.1588589765331,13.3376329379985,121.295689410122));
#151315=CARTESIAN_POINT('Ctrl Pts',(13.3947726768058,12.2109487310903,119.801571763063));
#151316=CARTESIAN_POINT('Ctrl Pts',(14.4026149179538,10.8763499173728,118.307454116004));
#151317=CARTESIAN_POINT('Ctrl Pts',(15.4104571591017,9.54175110365538,116.813336468945));
#151318=CARTESIAN_POINT('Ctrl Pts',(16.1559070823762,8.04468584505496,115.319218821886));
#151319=CARTESIAN_POINT('Ctrl Pts',(16.9013570056506,6.54762058645456,113.825101174828));
#151320=CARTESIAN_POINT('Ctrl Pts',(17.3590292079831,4.93906964482096,112.330983527769));
#151321=CARTESIAN_POINT('Ctrl Pts',(17.8167014103155,3.33051870318735,110.83686588071));
#151322=CARTESIAN_POINT('Ctrl Pts',(17.9710104137728,1.66525935159367,109.342748233651));
#151323=CARTESIAN_POINT('Ctrl Pts',(18.1253194172301,3.32956716117513E-15,
107.848630586592));
#151324=CARTESIAN_POINT('Ctrl Pts',(17.9710104137728,-1.66525935159367,
106.354512939533));
#151325=CARTESIAN_POINT('Ctrl Pts',(17.8167014103155,-3.33051870318736,
104.860395292475));
#151326=CARTESIAN_POINT('Ctrl Pts',(17.3590292079831,-4.93906964482095,
103.366277645416));
#151327=CARTESIAN_POINT('Ctrl Pts',(16.9013570056506,-6.54762058645456,
101.872159998357));
#151328=CARTESIAN_POINT('Ctrl Pts',(16.1559070823762,-8.04468584505497,
100.378042351298));
#151329=CARTESIAN_POINT('Ctrl Pts',(15.4104571591017,-9.54175110365538,
98.8839247042392));
#151330=CARTESIAN_POINT('Ctrl Pts',(14.4026149179538,-10.8763499173728,
97.3898070571806));
#151331=CARTESIAN_POINT('Ctrl Pts',(13.3947726768058,-12.2109487310903,
95.8956894101217));
#151332=CARTESIAN_POINT('Ctrl Pts',(12.1588589765331,-13.3376329379985,
94.4015717630628));
#151333=CARTESIAN_POINT('Ctrl Pts',(10.9229452762603,-14.4643171449067,
92.907454116004));
#151334=CARTESIAN_POINT('Ctrl Pts',(9.50104767561053,-15.3447188656481,
91.4133364689451));
#151335=CARTESIAN_POINT('Ctrl Pts',(8.07915007496071,-16.2251205863895,
89.9192188218865));
#151336=CARTESIAN_POINT('Ctrl Pts',(6.51968959134574,-16.8292587962898,
88.4251011748276));
#151337=CARTESIAN_POINT('Ctrl Pts',(4.96022910773078,-17.4333970061901,
86.9309835277687));
#151338=CARTESIAN_POINT('Ctrl Pts',(3.31631129755346,-17.7406985030951,
85.4368658807099));
#151339=CARTESIAN_POINT('Ctrl Pts',(1.67239348737615,-18.048,83.942748233651));
#151340=CARTESIAN_POINT('Ctrl Pts',(0.,-18.048,82.4486305865924));
#151341=CARTESIAN_POINT('Ctrl Pts',(-1.67239348737615,-18.048,80.9545129395335));
#151342=CARTESIAN_POINT('Ctrl Pts',(-3.31631129755346,-17.7406985030951,
79.4603952924746));
#151343=CARTESIAN_POINT('Ctrl Pts',(-4.96022910773077,-17.4333970061901,
77.9662776454158));
#151344=CARTESIAN_POINT('Ctrl Pts',(-6.51968959134574,-16.8292587962898,
76.4721599983569));
#151345=CARTESIAN_POINT('Ctrl Pts',(-8.07915007496071,-16.2251205863895,
74.9780423512982));
#151346=CARTESIAN_POINT('Ctrl Pts',(-9.50104767561052,-15.3447188656481,
73.4839247042394));
#151347=CARTESIAN_POINT('Ctrl Pts',(-10.9229452762603,-14.4643171449067,
71.9898070571805));
#151348=CARTESIAN_POINT('Ctrl Pts',(-12.1588589765331,-13.3376329379985,
70.4956894101216));
#151349=CARTESIAN_POINT('Ctrl Pts',(-13.3947726768058,-12.2109487310903,
69.0015717630628));
#151350=CARTESIAN_POINT('Ctrl Pts',(-14.4026149179538,-10.8763499173728,
67.5074541160041));
#151351=CARTESIAN_POINT('Ctrl Pts',(-15.4104571591017,-9.54175110365538,
66.0133364689453));
#151352=CARTESIAN_POINT('Ctrl Pts',(-16.1559070823762,-8.04468584505497,
64.5192188218864));
#151353=CARTESIAN_POINT('Ctrl Pts',(-16.9013570056506,-6.54762058645456,
63.0251011748275));
#151354=CARTESIAN_POINT('Ctrl Pts',(-17.3590292079831,-4.93906964482095,
61.5309835277687));
#151355=CARTESIAN_POINT('Ctrl Pts',(-17.8167014103155,-3.33051870318735,
60.03686588071));
#151356=CARTESIAN_POINT('Ctrl Pts',(-17.9710104137728,-1.66525935159368,
58.5427482336511));
#151357=CARTESIAN_POINT('Ctrl Pts',(-18.1253194172301,-1.10985572039171E-15,
57.0486305865923));
#151358=CARTESIAN_POINT('Ctrl Pts',(-17.9710104137728,1.66525935159367,
55.5545129395334));
#151359=CARTESIAN_POINT('Ctrl Pts',(-17.8167014103155,3.33051870318735,
54.0603952924745));
#151360=CARTESIAN_POINT('Ctrl Pts',(-17.3590292079831,4.93906964482096,
52.5662776454159));
#151361=CARTESIAN_POINT('Ctrl Pts',(-16.9013570056506,6.54762058645456,
51.072159998357));
#151362=CARTESIAN_POINT('Ctrl Pts',(-16.1559070823762,8.04468584505497,
49.5780423512981));
#151363=CARTESIAN_POINT('Ctrl Pts',(-15.4104571591017,9.54175110365538,
48.0839247042393));
#151364=CARTESIAN_POINT('Ctrl Pts',(-14.4026149179538,10.8763499173728,
46.5898070571804));
#151365=CARTESIAN_POINT('Ctrl Pts',(-13.3947726768058,12.2109487310903,
45.0956894101218));
#151366=CARTESIAN_POINT('Ctrl Pts',(-12.1588589765331,13.3376329379985,
43.6015717630629));
#151367=CARTESIAN_POINT('Ctrl Pts',(-10.9229452762603,14.4643171449067,
42.107454116004));
#151368=CARTESIAN_POINT('Ctrl Pts',(-9.50104767561052,15.3447188656481,
40.6133364689452));
#151369=CARTESIAN_POINT('Ctrl Pts',(-8.07915007496071,16.2251205863895,
39.1192188218863));
#151370=CARTESIAN_POINT('Ctrl Pts',(-6.51968959134574,16.8292587962898,
37.6251011748276));
#151371=CARTESIAN_POINT('Ctrl Pts',(-4.96022910773078,17.4333970061901,
36.1309835277688));
#151372=CARTESIAN_POINT('Ctrl Pts',(-3.31631129755346,17.7406985030951,
34.6368658807099));
#151373=CARTESIAN_POINT('Ctrl Pts',(-1.67239348737615,18.048,33.142748233651));
#151374=CARTESIAN_POINT('Ctrl Pts',(-2.21024254310115E-15,18.048,31.6486305865922));
#151375=CARTESIAN_POINT('Ctrl Pts',(1.67239348737616,18.048,30.1545129395335));
#151376=CARTESIAN_POINT('Ctrl Pts',(3.31631129755346,17.7406985030951,28.6603952924747));
#151377=CARTESIAN_POINT('Ctrl Pts',(4.96022910773077,17.4333970061901,27.1662776454158));
#151378=CARTESIAN_POINT('Ctrl Pts',(6.51968959134575,16.8292587962898,25.6721599983569));
#151379=CARTESIAN_POINT('Ctrl Pts',(8.07915007496071,16.2251205863895,24.1780423512981));
#151380=CARTESIAN_POINT('Ctrl Pts',(9.50104767561053,15.3447188656481,22.6839247042394));
#151381=CARTESIAN_POINT('Ctrl Pts',(10.9229452762603,14.4643171449067,21.1898070571805));
#151382=CARTESIAN_POINT('Ctrl Pts',(12.1588589765331,13.3376329379985,19.6956894101217));
#151383=CARTESIAN_POINT('Ctrl Pts',(13.3947726768058,12.2109487310903,18.2015717630628));
#151384=CARTESIAN_POINT('Ctrl Pts',(14.4026149179538,10.8763499173728,16.7074541160039));
#151385=CARTESIAN_POINT('Ctrl Pts',(15.4104571591017,9.54175110365538,15.2133364689453));
#151386=CARTESIAN_POINT('Ctrl Pts',(16.1559070823762,8.04468584505496,13.7192188218864));
#151387=CARTESIAN_POINT('Ctrl Pts',(16.9013570056506,6.54762058645456,12.2251011748276));
#151388=CARTESIAN_POINT('Ctrl Pts',(17.3590292079831,4.93906964482096,10.7309835277687));
#151389=CARTESIAN_POINT('Ctrl Pts',(17.8167014103155,3.33051870318735,9.23686588070982));
#151390=CARTESIAN_POINT('Ctrl Pts',(17.9710104137728,1.66525935159367,7.74274823365118));
#151391=CARTESIAN_POINT('Ctrl Pts',(18.1253194172301,3.32956716117513E-15,
6.24863058659231));
#151392=CARTESIAN_POINT('Ctrl Pts',(17.9710104137728,-1.66525935159367,
4.75451293953344));
#151393=CARTESIAN_POINT('Ctrl Pts',(17.8167014103155,-3.33051870318736,
3.26039529247457));
#151394=CARTESIAN_POINT('Ctrl Pts',(17.3590292079831,-4.93906964482095,
1.7662776454157));
#151395=CARTESIAN_POINT('Ctrl Pts',(16.9013570056506,-6.54762058645456,
0.272159998357058));
#151396=CARTESIAN_POINT('Ctrl Pts',(16.1559070823762,-8.04468584505497,
-1.22195764870181));
#151397=CARTESIAN_POINT('Ctrl Pts',(15.4104571591017,-9.54175110365538,
-2.71607529576068));
#151398=CARTESIAN_POINT('Ctrl Pts',(14.4026149179538,-10.8763499173728,
-4.21019294281955));
#151399=CARTESIAN_POINT('Ctrl Pts',(13.3947726768058,-12.2109487310903,
-5.70431058987841));
#151400=CARTESIAN_POINT('Ctrl Pts',(12.1588589765331,-13.3376329379985,
-7.19842823693706));
#151401=CARTESIAN_POINT('Ctrl Pts',(10.9229452762603,-14.4643171449067,
-8.69254588399593));
#151402=CARTESIAN_POINT('Ctrl Pts',(9.50104767561053,-15.3447188656481,
-10.1866635310548));
#151403=CARTESIAN_POINT('Ctrl Pts',(8.07915007496071,-16.2251205863895,
-11.6807811781137));
#151404=CARTESIAN_POINT('Ctrl Pts',(6.51968959134574,-16.8292587962898,
-13.1748988251725));
#151405=CARTESIAN_POINT('Ctrl Pts',(4.96022910773078,-17.4333970061901,
-14.6690164722312));
#151406=CARTESIAN_POINT('Ctrl Pts',(3.31631129755346,-17.7406985030951,
-16.16313411929));
#151407=CARTESIAN_POINT('Ctrl Pts',(1.67239348737615,-18.048,-17.6572517663489));
#151408=CARTESIAN_POINT('Ctrl Pts',(0.,-18.048,-19.1513694134078));
#151409=CARTESIAN_POINT('Ctrl Pts',(-1.67239348737615,-18.048,-20.6454870604667));
#151410=CARTESIAN_POINT('Ctrl Pts',(-3.31631129755346,-17.7406985030951,
-22.1396047075253));
#151411=CARTESIAN_POINT('Ctrl Pts',(-4.96022910773077,-17.4333970061901,
-23.6337223545842));
#151412=CARTESIAN_POINT('Ctrl Pts',(-6.51968959134574,-16.8292587962898,
-25.127840001643));
#151413=CARTESIAN_POINT('Ctrl Pts',(-8.07915007496071,-16.2251205863895,
-26.6219576487019));
#151414=CARTESIAN_POINT('Ctrl Pts',(-9.50104767561052,-15.3447188656481,
-28.1160752957608));
#151415=CARTESIAN_POINT('Ctrl Pts',(-10.9229452762603,-14.4643171449067,
-29.6101929428194));
#151416=CARTESIAN_POINT('Ctrl Pts',(-12.1588589765331,-13.3376329379985,
-31.1043105898783));
#151417=CARTESIAN_POINT('Ctrl Pts',(-13.3947726768058,-12.2109487310903,
-32.5984282369372));
#151418=CARTESIAN_POINT('Ctrl Pts',(-14.4026149179538,-10.8763499173728,
-34.092545883996));
#151419=CARTESIAN_POINT('Ctrl Pts',(-15.4104571591017,-9.54175110365538,
-35.5866635310549));
#151420=CARTESIAN_POINT('Ctrl Pts',(-16.1559070823762,-8.04468584505497,
-37.0807811781135));
#151421=CARTESIAN_POINT('Ctrl Pts',(-16.9013570056506,-6.54762058645456,
-38.5748988251724));
#151422=CARTESIAN_POINT('Ctrl Pts',(-17.3590292079831,-4.93906964482095,
-40.0690164722313));
#151423=CARTESIAN_POINT('Ctrl Pts',(-17.8167014103155,-3.33051870318735,
-41.5631341192901));
#151424=CARTESIAN_POINT('Ctrl Pts',(-17.9710104137728,-1.66525935159368,
-43.057251766349));
#151425=CARTESIAN_POINT('Ctrl Pts',(-18.1253194172301,-1.10985572039171E-15,
-44.5513694134076));
#151426=CARTESIAN_POINT('Ctrl Pts',(-17.9710104137728,1.66525935159367,
-46.0454870604665));
#151427=CARTESIAN_POINT('Ctrl Pts',(-17.8167014103155,3.33051870318735,
-47.5396047075254));
#151428=CARTESIAN_POINT('Ctrl Pts',(-17.3590292079831,4.93906964482096,
-49.0337223545843));
#151429=CARTESIAN_POINT('Ctrl Pts',(-16.9013570056506,6.54762058645456,
-50.5278400016431));
#151430=CARTESIAN_POINT('Ctrl Pts',(-16.1559070823762,8.04468584505497,
-52.0219576487018));
#151431=CARTESIAN_POINT('Ctrl Pts',(-15.4104571591017,9.54175110365538,
-53.5160752957606));
#151432=CARTESIAN_POINT('Ctrl Pts',(-14.4026149179538,10.8763499173728,
-55.0101929428195));
#151433=CARTESIAN_POINT('Ctrl Pts',(-13.3947726768058,12.2109487310903,
-56.5043105898784));
#151434=CARTESIAN_POINT('Ctrl Pts',(-12.1588589765331,13.3376329379985,
-57.9984282369372));
#151435=CARTESIAN_POINT('Ctrl Pts',(-10.9229452762603,14.4643171449067,
-59.4925458839959));
#151436=CARTESIAN_POINT('Ctrl Pts',(-9.50104767561052,15.3447188656481,
-60.9866635310548));
#151437=CARTESIAN_POINT('Ctrl Pts',(-8.07915007496071,16.2251205863895,
-62.4807811781136));
#151438=CARTESIAN_POINT('Ctrl Pts',(-6.51968959134574,16.8292587962898,
-63.9748988251725));
#151439=CARTESIAN_POINT('Ctrl Pts',(-4.96022910773078,17.4333970061901,
-65.4690164722314));
#151440=CARTESIAN_POINT('Ctrl Pts',(-3.31631129755346,17.7406985030951,
-66.96313411929));
#151441=CARTESIAN_POINT('Ctrl Pts',(-1.67239348737615,18.048,-68.4572517663489));
#151442=CARTESIAN_POINT('Ctrl Pts',(-2.21024254310115E-15,18.048,-69.9513694134077));
#151443=CARTESIAN_POINT('Ctrl Pts',(1.67239348737616,18.048,-71.4454870604666));
#151444=CARTESIAN_POINT('Ctrl Pts',(3.31631129755346,17.7406985030951,-72.9396047075255));
#151445=CARTESIAN_POINT('Ctrl Pts',(4.96022910773077,17.4333970061901,-74.4337223545841));
#151446=CARTESIAN_POINT('Ctrl Pts',(6.51968959134575,16.8292587962898,-75.927840001643));
#151447=CARTESIAN_POINT('Ctrl Pts',(8.07915007496071,16.2251205863895,-77.4219576487019));
#151448=CARTESIAN_POINT('Ctrl Pts',(9.50104767561053,15.3447188656481,-78.9160752957607));
#151449=CARTESIAN_POINT('Ctrl Pts',(10.9229452762603,14.4643171449067,-80.4101929428196));
#151450=CARTESIAN_POINT('Ctrl Pts',(12.1588589765331,13.3376329379985,-81.9043105898782));
#151451=CARTESIAN_POINT('Ctrl Pts',(13.3947726768058,12.2109487310903,-83.3984282369371));
#151452=CARTESIAN_POINT('Ctrl Pts',(14.4026149179538,10.8763499173728,-84.892545883996));
#151453=CARTESIAN_POINT('Ctrl Pts',(15.4104571591017,9.54175110365538,-86.3866635310549));
#151454=CARTESIAN_POINT('Ctrl Pts',(16.1559070823762,8.04468584505496,-87.8807811781137));
#151455=CARTESIAN_POINT('Ctrl Pts',(16.9013570056506,6.54762058645456,-89.3748988251724));
#151456=CARTESIAN_POINT('Ctrl Pts',(17.3590292079831,4.93906964482096,-90.8690164722312));
#151457=CARTESIAN_POINT('Ctrl Pts',(17.8167014103155,3.33051870318735,-92.3631341192901));
#151458=CARTESIAN_POINT('Ctrl Pts',(17.9710104137728,1.66525935159367,-93.857251766349));
#151459=CARTESIAN_POINT('Ctrl Pts',(18.1253194172301,3.32956716117513E-15,
-95.3513694134078));
#151460=CARTESIAN_POINT('Ctrl Pts',(17.9710104137728,-1.66525935159367,
-96.8454870604665));
#151461=CARTESIAN_POINT('Ctrl Pts',(17.8167014103155,-3.33051870318736,
-98.3396047075254));
#151462=CARTESIAN_POINT('Ctrl Pts',(17.3590292079831,-4.93906964482095,
-99.8337223545842));
#151463=CARTESIAN_POINT('Ctrl Pts',(16.9013570056506,-6.54762058645456,
-101.327840001643));
#151464=CARTESIAN_POINT('Ctrl Pts',(16.1559070823762,-8.04468584505497,
-102.821957648702));
#151465=CARTESIAN_POINT('Ctrl Pts',(15.4104571591017,-9.54175110365538,
-104.316075295761));
#151466=CARTESIAN_POINT('Ctrl Pts',(14.4026149179538,-10.8763499173728,
-105.810192942819));
#151467=CARTESIAN_POINT('Ctrl Pts',(13.3947726768058,-12.2109487310903,
-107.304310589878));
#151468=CARTESIAN_POINT('Ctrl Pts',(12.1588589765331,-13.3376329379985,
-108.798428236937));
#151469=CARTESIAN_POINT('Ctrl Pts',(10.9229452762603,-14.4643171449067,
-110.292545883996));
#151470=CARTESIAN_POINT('Ctrl Pts',(9.50104767561053,-15.3447188656481,
-111.786663531055));
#151471=CARTESIAN_POINT('Ctrl Pts',(8.07915007496071,-16.2251205863895,
-113.280781178114));
#151472=CARTESIAN_POINT('Ctrl Pts',(6.51968959134574,-16.8292587962898,
-114.774898825172));
#151473=CARTESIAN_POINT('Ctrl Pts',(4.96022910773078,-17.4333970061901,
-116.269016472231));
#151474=CARTESIAN_POINT('Ctrl Pts',(3.31631129755346,-17.7406985030951,
-117.76313411929));
#151475=CARTESIAN_POINT('Ctrl Pts',(1.67239348737615,-18.048,-119.257251766349));
#151476=CARTESIAN_POINT('Ctrl Pts',(0.,-18.048,-120.751369413408));
#151477=CARTESIAN_POINT('Ctrl Pts',(-1.67239348737615,-18.048,-122.245487060467));
#151478=CARTESIAN_POINT('Ctrl Pts',(-3.31631129755346,-17.7406985030951,
-123.739604707525));
#151479=CARTESIAN_POINT('Ctrl Pts',(-4.96022910773077,-17.4333970061901,
-125.233722354584));
#151480=CARTESIAN_POINT('Ctrl Pts',(-6.51968959134574,-16.8292587962898,
-126.727840001643));
#151481=CARTESIAN_POINT('Ctrl Pts',(-8.07915007496071,-16.2251205863895,
-128.221957648702));
#151482=CARTESIAN_POINT('Ctrl Pts',(-9.50104767561052,-15.3447188656481,
-129.716075295761));
#151483=CARTESIAN_POINT('Ctrl Pts',(-10.9229452762603,-14.4643171449067,
-131.21019294282));
#151484=CARTESIAN_POINT('Ctrl Pts',(-12.1588589765331,-13.3376329379985,
-132.704310589878));
#151485=CARTESIAN_POINT('Ctrl Pts',(-13.3947726768058,-12.2109487310903,
-134.198428236937));
#151486=CARTESIAN_POINT('Ctrl Pts',(-14.4026149179538,-10.8763499173728,
-135.692545883996));
#151487=CARTESIAN_POINT('Ctrl Pts',(-15.4104571591017,-9.54175110365538,
-137.186663531055));
#151488=CARTESIAN_POINT('Ctrl Pts',(-16.1559070823762,-8.04468584505497,
-138.680781178114));
#151489=CARTESIAN_POINT('Ctrl Pts',(-16.9013570056506,-6.54762058645456,
-140.174898825173));
#151490=CARTESIAN_POINT('Ctrl Pts',(-17.3590292079831,-4.93906964482095,
-141.669016472231));
#151491=CARTESIAN_POINT('Ctrl Pts',(-17.8167014103155,-3.33051870318735,
-143.16313411929));
#151492=CARTESIAN_POINT('Ctrl Pts',(-17.9710104137728,-1.66525935159368,
-144.657251766349));
#151493=CARTESIAN_POINT('Ctrl Pts',(-18.1253194172301,-1.10985572039171E-15,
-146.151369413408));
#151494=CARTESIAN_POINT('Ctrl Pts',(-17.9710104137728,1.66525935159367,
-147.645487060467));
#151495=CARTESIAN_POINT('Ctrl Pts',(-17.8167014103155,3.33051870318735,
-149.139604707525));
#151496=CARTESIAN_POINT('Ctrl Pts',(-17.3590292079831,4.93906964482096,
-150.633722354584));
#151497=CARTESIAN_POINT('Ctrl Pts',(-16.9013570056506,6.54762058645456,
-152.127840001643));
#151498=CARTESIAN_POINT('Ctrl Pts',(-16.1559070823762,8.04468584505497,
-153.621957648702));
#151499=CARTESIAN_POINT('Ctrl Pts',(-15.4104571591017,9.54175110365538,
-155.116075295761));
#151500=CARTESIAN_POINT('Ctrl Pts',(-14.4026149179538,10.8763499173728,
-156.610192942819));
#151501=CARTESIAN_POINT('Ctrl Pts',(-13.3947726768058,12.2109487310903,
-158.104310589878));
#151502=CARTESIAN_POINT('Ctrl Pts',(-12.1588589765331,13.3376329379985,
-159.598428236937));
#151503=CARTESIAN_POINT('Ctrl Pts',(-10.9229452762603,14.4643171449067,
-161.092545883996));
#151504=CARTESIAN_POINT('Ctrl Pts',(-9.50104767561052,15.3447188656481,
-162.586663531055));
#151505=CARTESIAN_POINT('Ctrl Pts',(-8.07915007496071,16.2251205863895,
-164.080781178114));
#151506=CARTESIAN_POINT('Ctrl Pts',(-6.51968959134574,16.8292587962898,
-165.574898825172));
#151507=CARTESIAN_POINT('Ctrl Pts',(-4.96022910773078,17.4333970061901,
-167.069016472231));
#151508=CARTESIAN_POINT('Ctrl Pts',(-3.31631129755346,17.7406985030951,
-168.56313411929));
#151509=CARTESIAN_POINT('Ctrl Pts',(-1.67239348737615,18.048,-170.057251766349));
#151510=CARTESIAN_POINT('Ctrl Pts',(-2.21024254310115E-15,18.048,-171.551369413408));
#151511=CARTESIAN_POINT('Ctrl Pts',(1.67239348737616,18.048,-173.045487060467));
#151512=CARTESIAN_POINT('Ctrl Pts',(3.31631129755346,17.7406985030951,-174.539604707525));
#151513=CARTESIAN_POINT('Ctrl Pts',(4.96022910773077,17.4333970061901,-176.033722354584));
#151514=CARTESIAN_POINT('Ctrl Pts',(6.51968959134575,16.8292587962898,-177.527840001643));
#151515=CARTESIAN_POINT('Ctrl Pts',(8.07915007496071,16.2251205863895,-179.021957648702));
#151516=CARTESIAN_POINT('Ctrl Pts',(9.50104767561053,15.3447188656481,-180.516075295761));
#151517=CARTESIAN_POINT('Ctrl Pts',(10.9229452762603,14.4643171449067,-182.01019294282));
#151518=CARTESIAN_POINT('Ctrl Pts',(12.1588589765331,13.3376329379985,-183.504310589878));
#151519=CARTESIAN_POINT('Ctrl Pts',(13.3947726768058,12.2109487310903,-184.998428236937));
#151520=CARTESIAN_POINT('Ctrl Pts',(14.4026149179538,10.8763499173728,-186.492545883996));
#151521=CARTESIAN_POINT('Ctrl Pts',(15.4104571591017,9.54175110365538,-187.986663531055));
#151522=CARTESIAN_POINT('Ctrl Pts',(16.1559070823762,8.04468584505496,-189.480781178114));
#151523=CARTESIAN_POINT('Ctrl Pts',(16.9013570056506,6.54762058645456,-190.974898825173));
#151524=CARTESIAN_POINT('Ctrl Pts',(17.3590292079831,4.93906964482096,-192.469016472231));
#151525=CARTESIAN_POINT('Ctrl Pts',(17.8167014103155,3.33051870318735,-193.96313411929));
#151526=CARTESIAN_POINT('Ctrl Pts',(17.9710104137728,1.66525935159367,-195.457251766349));
#151527=CARTESIAN_POINT('Ctrl Pts',(18.1253194172301,3.32956716117513E-15,
-196.951369413408));
#151528=CARTESIAN_POINT('Ctrl Pts',(17.9710104137728,-1.66525935159367,
-198.445487060467));
#151529=CARTESIAN_POINT('Ctrl Pts',(17.8167014103155,-3.33051870318736,
-199.939604707526));
#151530=CARTESIAN_POINT('Ctrl Pts',(17.3590292079831,-4.93906964482095,
-201.433722354584));
#151531=CARTESIAN_POINT('Ctrl Pts',(16.9013570056506,-6.54762058645456,
-202.927840001643));
#151532=CARTESIAN_POINT('Ctrl Pts',(16.1559070823762,-8.04468584505497,
-204.421957648702));
#151533=CARTESIAN_POINT('Ctrl Pts',(15.4104571591017,-9.54175110365538,
-205.916075295761));
#151534=CARTESIAN_POINT('Ctrl Pts',(14.4026149179538,-10.8763499173728,
-207.41019294282));
#151535=CARTESIAN_POINT('Ctrl Pts',(13.3947726768058,-12.2109487310903,
-208.904310589878));
#151536=CARTESIAN_POINT('Ctrl Pts',(12.1588589765331,-13.3376329379985,
-210.398428236937));
#151537=CARTESIAN_POINT('Ctrl Pts',(10.9229452762603,-14.4643171449067,
-211.892545883996));
#151538=CARTESIAN_POINT('Ctrl Pts',(9.50104767561053,-15.3447188656481,
-213.386663531055));
#151539=CARTESIAN_POINT('Ctrl Pts',(8.07915007496071,-16.2251205863895,
-214.880781178114));
#151540=CARTESIAN_POINT('Ctrl Pts',(6.51968959134574,-16.8292587962898,
-216.374898825172));
#151541=CARTESIAN_POINT('Ctrl Pts',(4.96022910773078,-17.4333970061901,
-217.869016472231));
#151542=CARTESIAN_POINT('Ctrl Pts',(3.31631129755346,-17.7406985030951,
-219.36313411929));
#151543=CARTESIAN_POINT('Ctrl Pts',(1.67239348737615,-18.048,-220.857251766349));
#151544=CARTESIAN_POINT('Ctrl Pts',(0.,-18.048,-222.351369413408));
#151545=CARTESIAN_POINT('Ctrl Pts',(-1.67239348737615,-18.048,-223.845487060466));
#151546=CARTESIAN_POINT('Ctrl Pts',(-3.31631129755346,-17.7406985030951,
-225.339604707525));
#151547=CARTESIAN_POINT('Ctrl Pts',(-4.96022910773077,-17.4333970061901,
-226.833722354584));
#151548=CARTESIAN_POINT('Ctrl Pts',(-6.51968959134574,-16.8292587962898,
-228.327840001643));
#151549=CARTESIAN_POINT('Ctrl Pts',(-8.07915007496071,-16.2251205863895,
-229.821957648702));
#151550=CARTESIAN_POINT('Ctrl Pts',(-9.50104767561052,-15.3447188656481,
-231.316075295761));
#151551=CARTESIAN_POINT('Ctrl Pts',(-10.9229452762603,-14.4643171449067,
-232.810192942819));
#151552=CARTESIAN_POINT('Ctrl Pts',(-12.1588589765331,-13.3376329379985,
-234.304310589878));
#151553=CARTESIAN_POINT('Ctrl Pts',(-13.3947726768058,-12.2109487310903,
-235.798428236937));
#151554=CARTESIAN_POINT('Ctrl Pts',(-14.4026149179538,-10.8763499173728,
-237.292545883996));
#151555=CARTESIAN_POINT('Ctrl Pts',(-15.4104571591017,-9.54175110365538,
-238.786663531055));
#151556=CARTESIAN_POINT('Ctrl Pts',(-16.1559070823762,-8.04468584505497,
-240.280781178114));
#151557=CARTESIAN_POINT('Ctrl Pts',(-16.9013570056506,-6.54762058645456,
-241.774898825172));
#151558=CARTESIAN_POINT('Ctrl Pts',(-17.3590292079831,-4.93906964482095,
-243.269016472231));
#151559=CARTESIAN_POINT('Ctrl Pts',(-17.8167014103155,-3.33051870318735,
-244.76313411929));
#151560=CARTESIAN_POINT('Ctrl Pts',(-17.9710104137728,-1.66525935159368,
-246.257251766349));
#151561=CARTESIAN_POINT('Ctrl Pts',(-18.1253194172301,-1.10985572039171E-15,
-247.751369413408));
#151562=CARTESIAN_POINT('Ctrl Pts',(-17.9710104137728,1.66525935159367,
-249.245487060467));
#151563=CARTESIAN_POINT('Ctrl Pts',(-17.8167014103155,3.33051870318735,
-250.739604707525));
#151564=CARTESIAN_POINT('Ctrl Pts',(-17.3590292079831,4.93906964482096,
-252.233722354584));
#151565=CARTESIAN_POINT('Ctrl Pts',(-16.9013570056506,6.54762058645456,
-253.727840001643));
#151566=CARTESIAN_POINT('Ctrl Pts',(-16.1559070823762,8.04468584505497,
-255.221957648702));
#151567=CARTESIAN_POINT('Ctrl Pts',(-15.4104571591017,9.54175110365538,
-256.716075295761));
#151568=CARTESIAN_POINT('Ctrl Pts',(-14.4026149179538,10.8763499173728,
-258.21019294282));
#151569=CARTESIAN_POINT('Ctrl Pts',(-13.3947726768058,12.2109487310903,
-259.704310589879));
#151570=CARTESIAN_POINT('Ctrl Pts',(-12.1588589765331,13.3376329379985,
-261.198428236937));
#151571=CARTESIAN_POINT('Ctrl Pts',(-10.9229452762603,14.4643171449067,
-262.692545883996));
#151572=CARTESIAN_POINT('Ctrl Pts',(-9.50104767561052,15.3447188656481,
-264.186663531055));
#151573=CARTESIAN_POINT('Ctrl Pts',(-8.07915007496071,16.2251205863895,
-265.680781178114));
#151574=CARTESIAN_POINT('Ctrl Pts',(-6.51968959134574,16.8292587962898,
-267.174898825173));
#151575=CARTESIAN_POINT('Ctrl Pts',(-4.96022910773078,17.4333970061901,
-268.669016472231));
#151576=CARTESIAN_POINT('Ctrl Pts',(-3.31631129755346,17.7406985030951,
-270.16313411929));
#151577=CARTESIAN_POINT('Ctrl Pts',(-1.67239348737615,18.048,-271.657251766349));
#151578=CARTESIAN_POINT('Ctrl Pts',(-2.21024254310115E-15,18.048,-273.151369413408));
#151579=CARTESIAN_POINT('Ctrl Pts',(1.67239348737616,18.048,-274.645487060467));
#151580=CARTESIAN_POINT('Ctrl Pts',(3.31631129755346,17.7406985030951,-276.139604707525));
#151581=CARTESIAN_POINT('Ctrl Pts',(4.96022910773077,17.4333970061901,-277.633722354584));
#151582=CARTESIAN_POINT('Ctrl Pts',(6.51968959134575,16.8292587962898,-279.127840001643));
#151583=CARTESIAN_POINT('Ctrl Pts',(8.07915007496071,16.2251205863895,-280.621957648702));
#151584=CARTESIAN_POINT('Ctrl Pts',(9.50104767561053,15.3447188656481,-282.116075295761));
#151585=CARTESIAN_POINT('Ctrl Pts',(10.9229452762603,14.4643171449067,-283.610192942819));
#151586=CARTESIAN_POINT('Ctrl Pts',(12.1588589765331,13.3376329379985,-285.104310589878));
#151587=CARTESIAN_POINT('Ctrl Pts',(13.3947726768058,12.2109487310903,-286.598428236937));
#151588=CARTESIAN_POINT('Ctrl Pts',(14.4026149179538,10.8763499173728,-288.092545883996));
#151589=CARTESIAN_POINT('Ctrl Pts',(15.4104571591017,9.54175110365538,-289.586663531055));
#151590=CARTESIAN_POINT('Ctrl Pts',(16.1559070823762,8.04468584505496,-291.080781178114));
#151591=CARTESIAN_POINT('Ctrl Pts',(16.9013570056506,6.54762058645456,-292.574898825172));
#151592=CARTESIAN_POINT('Ctrl Pts',(17.3590292079831,4.93906964482096,-294.069016472231));
#151593=CARTESIAN_POINT('Ctrl Pts',(17.8167014103155,3.33051870318735,-295.56313411929));
#151594=CARTESIAN_POINT('Ctrl Pts',(17.9710104137728,1.66525935159367,-297.057251766349));
#151595=CARTESIAN_POINT('Ctrl Pts',(18.1253194172301,3.32956716117513E-15,
-298.551369413408));
#151596=CARTESIAN_POINT('Ctrl Pts',(17.9710104137728,-1.66525935159367,
-300.045487060467));
#151597=CARTESIAN_POINT('Ctrl Pts',(17.8167014103155,-3.33051870318736,
-301.539604707525));
#151598=CARTESIAN_POINT('Ctrl Pts',(17.3590292079831,-4.93906964482095,
-303.033722354584));
#151599=CARTESIAN_POINT('Ctrl Pts',(16.9013570056506,-6.54762058645456,
-304.527840001643));
#151600=CARTESIAN_POINT('Ctrl Pts',(16.1559070823762,-8.04468584505497,
-306.021957648702));
#151601=CARTESIAN_POINT('Ctrl Pts',(15.4104571591017,-9.54175110365538,
-307.516075295761));
#151602=CARTESIAN_POINT('Ctrl Pts',(14.4026149179538,-10.8763499173728,
-309.01019294282));
#151603=CARTESIAN_POINT('Ctrl Pts',(13.3947726768058,-12.2109487310903,
-310.504310589878));
#151604=CARTESIAN_POINT('Ctrl Pts',(12.1588589765331,-13.3376329379985,
-311.998428236937));
#151605=CARTESIAN_POINT('Ctrl Pts',(10.9229452762603,-14.4643171449067,
-313.492545883996));
#151606=CARTESIAN_POINT('Ctrl Pts',(9.50104767561053,-15.3447188656481,
-314.986663531055));
#151607=CARTESIAN_POINT('Ctrl Pts',(8.07915007496071,-16.2251205863895,
-316.480781178114));
#151608=CARTESIAN_POINT('Ctrl Pts',(6.51968959134574,-16.8292587962898,
-317.974898825172));
#151609=CARTESIAN_POINT('Ctrl Pts',(4.96022910773078,-17.4333970061901,
-319.469016472231));
#151610=CARTESIAN_POINT('Ctrl Pts',(3.31631129755346,-17.7406985030951,
-320.96313411929));
#151611=CARTESIAN_POINT('Ctrl Pts',(1.67239348737615,-18.048,-322.457251766349));
#151612=CARTESIAN_POINT('Ctrl Pts',(0.,-18.048,-323.951369413408));
#151613=CARTESIAN_POINT('Ctrl Pts',(-1.67239348737615,-18.048,-325.445487060467));
#151614=CARTESIAN_POINT('Ctrl Pts',(-3.31631129755346,-17.7406985030951,
-326.939604707526));
#151615=CARTESIAN_POINT('Ctrl Pts',(-4.96022910773077,-17.4333970061901,
-328.433722354584));
#151616=CARTESIAN_POINT('Ctrl Pts',(-6.51968959134574,-16.8292587962898,
-329.927840001643));
#151617=CARTESIAN_POINT('Ctrl Pts',(-8.07915007496071,-16.2251205863895,
-331.421957648702));
#151618=CARTESIAN_POINT('Ctrl Pts',(-9.50104767561052,-15.3447188656481,
-332.916075295761));
#151619=CARTESIAN_POINT('Ctrl Pts',(-10.9229452762603,-14.4643171449067,
-334.41019294282));
#151620=CARTESIAN_POINT('Ctrl Pts',(-12.1588589765331,-13.3376329379985,
-335.904310589878));
#151621=CARTESIAN_POINT('Ctrl Pts',(-13.3947726768058,-12.2109487310903,
-337.398428236937));
#151622=CARTESIAN_POINT('Ctrl Pts',(-14.4026149179538,-10.8763499173728,
-338.892545883996));
#151623=CARTESIAN_POINT('Ctrl Pts',(-15.4104571591017,-9.54175110365538,
-340.386663531055));
#151624=CARTESIAN_POINT('Ctrl Pts',(-16.1559070823762,-8.04468584505497,
-341.880781178114));
#151625=CARTESIAN_POINT('Ctrl Pts',(-16.9013570056506,-6.54762058645456,
-343.374898825172));
#151626=CARTESIAN_POINT('Ctrl Pts',(-17.3590292079831,-4.93906964482095,
-344.869016472231));
#151627=CARTESIAN_POINT('Ctrl Pts',(-17.8167014103155,-3.33051870318735,
-346.36313411929));
#151628=CARTESIAN_POINT('Ctrl Pts',(-17.9710104137728,-1.66525935159368,
-347.857251766349));
#151629=CARTESIAN_POINT('Ctrl Pts',(-18.1253194172301,-1.10985572039171E-15,
-349.351369413408));
#151630=CARTESIAN_POINT('Ctrl Pts',(-17.9710104137728,1.66525935159367,
-350.845487060467));
#151631=CARTESIAN_POINT('Ctrl Pts',(-17.8167014103155,3.33051870318735,
-352.339604707525));
#151632=CARTESIAN_POINT('Ctrl Pts',(-17.3590292079831,4.93906964482096,
-353.833722354584));
#151633=CARTESIAN_POINT('Ctrl Pts',(-16.9013570056506,6.54762058645456,
-355.327840001643));
#151634=CARTESIAN_POINT('Ctrl Pts',(-16.1559070823762,8.04468584505497,
-356.821957648702));
#151635=CARTESIAN_POINT('Ctrl Pts',(-15.4104571591017,9.54175110365538,
-358.316075295761));
#151636=CARTESIAN_POINT('Ctrl Pts',(-14.4026149179538,10.8763499173728,
-359.81019294282));
#151637=CARTESIAN_POINT('Ctrl Pts',(-13.3947726768058,12.2109487310903,
-361.304310589878));
#151638=CARTESIAN_POINT('Ctrl Pts',(-12.1588589765331,13.3376329379985,
-362.798428236937));
#151639=CARTESIAN_POINT('Ctrl Pts',(-10.9229452762603,14.4643171449067,
-364.292545883996));
#151640=CARTESIAN_POINT('Ctrl Pts',(-9.50104767561052,15.3447188656481,
-365.786663531055));
#151641=CARTESIAN_POINT('Ctrl Pts',(-8.07915007496071,16.2251205863895,
-367.280781178114));
#151642=CARTESIAN_POINT('Ctrl Pts',(-6.51968959134574,16.8292587962898,
-368.774898825172));
#151643=CARTESIAN_POINT('Ctrl Pts',(-4.96022910773078,17.4333970061901,
-370.269016472231));
#151644=CARTESIAN_POINT('Ctrl Pts',(-3.31631129755346,17.7406985030951,
-371.76313411929));
#151645=CARTESIAN_POINT('Ctrl Pts',(-1.67239348737615,18.048,-373.257251766349));
#151646=CARTESIAN_POINT('Ctrl Pts',(-2.21024254310115E-15,18.048,-374.751369413408));
#151647=CARTESIAN_POINT('Ctrl Pts',(1.67239348737616,18.048,-376.245487060467));
#151648=CARTESIAN_POINT('Ctrl Pts',(3.31631129755346,17.7406985030951,-377.739604707525));
#151649=CARTESIAN_POINT('Ctrl Pts',(4.96022910773077,17.4333970061901,-379.233722354584));
#151650=CARTESIAN_POINT('Ctrl Pts',(6.51968959134575,16.8292587962898,-380.727840001643));
#151651=CARTESIAN_POINT('Ctrl Pts',(8.07915007496071,16.2251205863895,-382.221957648702));
#151652=CARTESIAN_POINT('Ctrl Pts',(9.50104767561053,15.3447188656481,-383.716075295761));
#151653=CARTESIAN_POINT('Ctrl Pts',(10.9229452762603,14.4643171449067,-385.21019294282));
#151654=CARTESIAN_POINT('Ctrl Pts',(12.1588589765331,13.3376329379985,-386.704310589878));
#151655=CARTESIAN_POINT('Ctrl Pts',(13.3947726768058,12.2109487310903,-388.198428236937));
#151656=CARTESIAN_POINT('Ctrl Pts',(14.4026149179538,10.8763499173728,-389.692545883996));
#151657=CARTESIAN_POINT('Ctrl Pts',(15.4104571591017,9.54175110365538,-391.186663531055));
#151658=CARTESIAN_POINT('Ctrl Pts',(16.1559070823762,8.04468584505496,-392.680781178114));
#151659=CARTESIAN_POINT('Ctrl Pts',(16.9013570056506,6.54762058645456,-394.174898825173));
#151660=CARTESIAN_POINT('Ctrl Pts',(17.3590292079831,4.93906964482096,-395.669016472231));
#151661=CARTESIAN_POINT('Ctrl Pts',(17.8167014103155,3.33051870318735,-397.16313411929));
#151662=CARTESIAN_POINT('Ctrl Pts',(17.9710104137728,1.66525935159367,-398.657251766349));
#151663=CARTESIAN_POINT('Ctrl Pts',(18.1253194172301,3.32956716117513E-15,
-400.151369413408));
#151664=CARTESIAN_POINT('Ctrl Pts',(17.9710104137728,-1.66525935159367,
-401.645487060467));
#151665=CARTESIAN_POINT('Ctrl Pts',(17.8167014103155,-3.33051870318736,
-403.139604707525));
#151666=CARTESIAN_POINT('Ctrl Pts',(17.3590292079831,-4.93906964482095,
-404.633722354584));
#151667=CARTESIAN_POINT('Ctrl Pts',(16.9013570056506,-6.54762058645456,
-406.127840001643));
#151668=CARTESIAN_POINT('Ctrl Pts',(16.1559070823762,-8.04468584505497,
-407.621957648702));
#151669=CARTESIAN_POINT('Ctrl Pts',(15.4104571591017,-9.54175110365538,
-409.116075295761));
#151670=CARTESIAN_POINT('Ctrl Pts',(14.4026149179538,-10.8763499173728,
-410.610192942819));
#151671=CARTESIAN_POINT('Ctrl Pts',(13.3947726768058,-12.2109487310903,
-412.104310589878));
#151672=CARTESIAN_POINT('Ctrl Pts',(12.1588589765331,-13.3376329379985,
-413.598428236937));
#151673=CARTESIAN_POINT('Ctrl Pts',(10.9229452762603,-14.4643171449067,
-415.092545883996));
#151674=CARTESIAN_POINT('Ctrl Pts',(9.50104767561053,-15.3447188656481,
-416.586663531055));
#151675=CARTESIAN_POINT('Ctrl Pts',(8.07915007496071,-16.2251205863895,
-418.080781178114));
#151676=CARTESIAN_POINT('Ctrl Pts',(6.51968959134574,-16.8292587962898,
-419.574898825172));
#151677=CARTESIAN_POINT('Ctrl Pts',(4.96022910773078,-17.4333970061901,
-421.069016472231));
#151678=CARTESIAN_POINT('Ctrl Pts',(3.31631129755346,-17.7406985030951,
-422.56313411929));
#151679=CARTESIAN_POINT('Ctrl Pts',(1.67239348737615,-18.048,-424.057251766349));
#151680=CARTESIAN_POINT('Ctrl Pts',(0.,-18.048,-425.551369413408));
#151681=CARTESIAN_POINT('Ctrl Pts',(-1.67239348737615,-18.048,-427.045487060466));
#151682=CARTESIAN_POINT('Ctrl Pts',(-3.31631129755346,-17.7406985030951,
-428.539604707525));
#151683=CARTESIAN_POINT('Ctrl Pts',(-4.96022910773077,-17.4333970061901,
-430.033722354584));
#151684=CARTESIAN_POINT('Ctrl Pts',(-6.51968959134574,-16.8292587962898,
-431.527840001643));
#151685=CARTESIAN_POINT('Ctrl Pts',(-8.07915007496071,-16.2251205863895,
-433.021957648702));
#151686=CARTESIAN_POINT('Ctrl Pts',(-9.50104767561052,-15.3447188656481,
-434.516075295761));
#151687=CARTESIAN_POINT('Ctrl Pts',(-10.9229452762603,-14.4643171449067,
-436.01019294282));
#151688=CARTESIAN_POINT('Ctrl Pts',(-12.1588589765331,-13.3376329379985,
-437.504310589878));
#151689=CARTESIAN_POINT('Ctrl Pts',(-13.3947726768058,-12.2109487310903,
-438.998428236937));
#151690=CARTESIAN_POINT('Ctrl Pts',(-14.4026149179538,-10.8763499173728,
-440.492545883996));
#151691=CARTESIAN_POINT('Ctrl Pts',(-15.4104571591017,-9.54175110365538,
-441.986663531055));
#151692=CARTESIAN_POINT('Ctrl Pts',(-16.1559070823762,-8.04468584505497,
-443.480781178114));
#151693=CARTESIAN_POINT('Ctrl Pts',(-16.9013570056506,-6.54762058645456,
-444.974898825172));
#151694=CARTESIAN_POINT('Ctrl Pts',(-17.3590292079831,-4.93906964482095,
-446.469016472231));
#151695=CARTESIAN_POINT('Ctrl Pts',(-17.8167014103155,-3.33051870318735,
-447.96313411929));
#151696=CARTESIAN_POINT('Ctrl Pts',(-17.9710104137728,-1.66525935159368,
-449.457251766349));
#151697=CARTESIAN_POINT('Ctrl Pts',(-18.1253194172301,-1.10985572039171E-15,
-450.951369413408));
#151698=CARTESIAN_POINT('Ctrl Pts',(-17.9710104137728,1.66525935159367,
-452.445487060467));
#151699=CARTESIAN_POINT('Ctrl Pts',(-17.8167014103155,3.33051870318735,
-453.939604707526));
#151700=CARTESIAN_POINT('Ctrl Pts',(-17.3590292079831,4.93906964482096,
-455.433722354584));
#151701=CARTESIAN_POINT('Ctrl Pts',(-16.9013570056506,6.54762058645456,
-456.927840001643));
#151702=CARTESIAN_POINT('Ctrl Pts',(-16.1559070823762,8.04468584505497,
-458.421957648702));
#151703=CARTESIAN_POINT('Ctrl Pts',(-15.4104571591017,9.54175110365538,
-459.916075295761));
#151704=CARTESIAN_POINT('Ctrl Pts',(-14.4026149179538,10.8763499173728,
-461.41019294282));
#151705=CARTESIAN_POINT('Ctrl Pts',(-13.3947726768058,12.2109487310903,
-462.904310589878));
#151706=CARTESIAN_POINT('Ctrl Pts',(-12.1588589765331,13.3376329379985,
-464.398428236937));
#151707=CARTESIAN_POINT('Ctrl Pts',(-10.9229452762603,14.4643171449067,
-465.892545883996));
#151708=CARTESIAN_POINT('Ctrl Pts',(-9.50104767561052,15.3447188656481,
-467.386663531055));
#151709=CARTESIAN_POINT('Ctrl Pts',(-8.07915007496071,16.2251205863895,
-468.880781178114));
#151710=CARTESIAN_POINT('Ctrl Pts',(-6.51968959134574,16.8292587962898,
-470.374898825172));
#151711=CARTESIAN_POINT('Ctrl Pts',(-4.96022910773078,17.4333970061901,
-471.869016472231));
#151712=CARTESIAN_POINT('Ctrl Pts',(-3.31631129755346,17.7406985030951,
-473.36313411929));
#151713=CARTESIAN_POINT('Ctrl Pts',(-1.67239348737615,18.048,-474.857251766349));
#151714=CARTESIAN_POINT('Ctrl Pts',(-2.21024254310115E-15,18.048,-476.351369413408));
#151715=CARTESIAN_POINT('Ctrl Pts',(1.67239348737616,18.048,-477.845487060466));
#151716=CARTESIAN_POINT('Ctrl Pts',(3.31631129755346,17.7406985030951,-479.339604707525));
#151717=CARTESIAN_POINT('Ctrl Pts',(4.96022910773077,17.4333970061901,-480.833722354584));
#151718=CARTESIAN_POINT('Ctrl Pts',(6.51968959134575,16.8292587962898,-482.327840001643));
#151719=CARTESIAN_POINT('Ctrl Pts',(8.07915007496071,16.2251205863895,-483.821957648702));
#151720=CARTESIAN_POINT('Ctrl Pts',(9.50104767561053,15.3447188656481,-485.316075295761));
#151721=CARTESIAN_POINT('Ctrl Pts',(10.9229452762603,14.4643171449067,-486.81019294282));
#151722=CARTESIAN_POINT('Ctrl Pts',(12.1588589765331,13.3376329379985,-488.304310589878));
#151723=CARTESIAN_POINT('Ctrl Pts',(13.3947726768058,12.2109487310903,-489.798428236937));
#151724=CARTESIAN_POINT('Ctrl Pts',(14.4026149179538,10.8763499173728,-491.292545883996));
#151725=CARTESIAN_POINT('Ctrl Pts',(15.4104571591017,9.54175110365538,-492.786663531055));
#151726=CARTESIAN_POINT('Ctrl Pts',(16.1559070823762,8.04468584505496,-494.280781178114));
#151727=CARTESIAN_POINT('Ctrl Pts',(16.9013570056506,6.54762058645456,-495.774898825173));
#151728=CARTESIAN_POINT('Ctrl Pts',(17.3590292079831,4.93906964482096,-497.269016472231));
#151729=CARTESIAN_POINT('Ctrl Pts',(17.8167014103155,3.33051870318735,-498.76313411929));
#151730=CARTESIAN_POINT('Ctrl Pts',(17.9710104137728,1.66525935159367,-500.257251766349));
#151731=CARTESIAN_POINT('Ctrl Pts',(18.1253194172301,3.32956716117513E-15,
-501.751369413408));
#151732=CARTESIAN_POINT('Ctrl Pts',(17.9710104137728,-1.66525935159367,
-503.245487060466));
#151733=CARTESIAN_POINT('Ctrl Pts',(17.8167014103155,-3.33051870318736,
-504.739604707525));
#151734=CARTESIAN_POINT('Ctrl Pts',(17.3590292079831,-4.93906964482095,
-506.233722354584));
#151735=CARTESIAN_POINT('Ctrl Pts',(16.9013570056506,-6.54762058645456,
-507.727840001643));
#151736=CARTESIAN_POINT('Ctrl Pts',(16.1559070823762,-8.04468584505497,
-509.221957648702));
#151737=CARTESIAN_POINT('Ctrl Pts',(15.4104571591017,-9.54175110365538,
-510.716075295761));
#151738=CARTESIAN_POINT('Ctrl Pts',(14.4026149179538,-10.8763499173728,
-512.21019294282));
#151739=CARTESIAN_POINT('Ctrl Pts',(13.3947726768058,-12.2109487310903,
-513.704310589878));
#151740=CARTESIAN_POINT('Ctrl Pts',(12.1588589765331,-13.3376329379985,
-515.198428236937));
#151741=CARTESIAN_POINT('Ctrl Pts',(10.9229452762603,-14.4643171449067,
-516.692545883996));
#151742=CARTESIAN_POINT('Ctrl Pts',(9.50104767561053,-15.3447188656481,
-518.186663531055));
#151743=CARTESIAN_POINT('Ctrl Pts',(8.07915007496071,-16.2251205863895,
-519.680781178114));
#151744=CARTESIAN_POINT('Ctrl Pts',(6.51968959134574,-16.8292587962898,
-521.174898825172));
#151745=CARTESIAN_POINT('Ctrl Pts',(4.96022910773078,-17.4333970061901,
-522.669016472231));
#151746=CARTESIAN_POINT('Ctrl Pts',(3.31631129755346,-17.7406985030951,
-524.16313411929));
#151747=CARTESIAN_POINT('Ctrl Pts',(1.67239348737615,-18.048,-525.657251766349));
#151748=CARTESIAN_POINT('Ctrl Pts',(0.,-18.048,-527.151369413408));
#151749=CARTESIAN_POINT('Ctrl Pts',(-1.67239348737615,-18.048,-528.645487060467));
#151750=CARTESIAN_POINT('Ctrl Pts',(-3.31631129755346,-17.7406985030951,
-530.139604707526));
#151751=CARTESIAN_POINT('Ctrl Pts',(-4.96022910773077,-17.4333970061901,
-531.633722354584));
#151752=CARTESIAN_POINT('Ctrl Pts',(-6.51968959134574,-16.8292587962898,
-533.127840001643));
#151753=CARTESIAN_POINT('Ctrl Pts',(-8.07915007496071,-16.2251205863895,
-534.621957648702));
#151754=CARTESIAN_POINT('Ctrl Pts',(-9.50104767561052,-15.3447188656481,
-536.116075295761));
#151755=CARTESIAN_POINT('Ctrl Pts',(-10.9229452762603,-14.4643171449067,
-537.610192942819));
#151756=CARTESIAN_POINT('Ctrl Pts',(-12.1588589765331,-13.3376329379985,
-539.104310589878));
#151757=CARTESIAN_POINT('Ctrl Pts',(-13.3947726768058,-12.2109487310903,
-540.598428236937));
#151758=CARTESIAN_POINT('Ctrl Pts',(-14.4026149179538,-10.8763499173728,
-542.092545883996));
#151759=CARTESIAN_POINT('Ctrl Pts',(-15.4104571591017,-9.54175110365538,
-543.586663531055));
#151760=CARTESIAN_POINT('Ctrl Pts',(-16.1559070823762,-8.04468584505497,
-545.080781178114));
#151761=CARTESIAN_POINT('Ctrl Pts',(-16.9013570056506,-6.54762058645456,
-546.574898825173));
#151762=CARTESIAN_POINT('Ctrl Pts',(-17.3590292079831,-4.93906964482095,
-548.069016472231));
#151763=CARTESIAN_POINT('Ctrl Pts',(-17.8167014103155,-3.33051870318735,
-549.56313411929));
#151764=CARTESIAN_POINT('Ctrl Pts',(-17.9710104137728,-1.66525935159368,
-551.057251766349));
#151765=CARTESIAN_POINT('Ctrl Pts',(-18.1253194172301,-1.10985572039171E-15,
-552.551369413408));
#151766=CARTESIAN_POINT('Ctrl Pts',(-17.9710104137728,1.66525935159367,
-554.045487060466));
#151767=CARTESIAN_POINT('Ctrl Pts',(-17.8167014103155,3.33051870318735,
-555.539604707526));
#151768=CARTESIAN_POINT('Ctrl Pts',(-17.3590292079831,4.93906964482096,
-557.033722354584));
#151769=CARTESIAN_POINT('Ctrl Pts',(-16.9013570056506,6.54762058645456,
-558.527840001643));
#151770=CARTESIAN_POINT('Ctrl Pts',(-16.1559070823762,8.04468584505497,
-560.021957648702));
#151771=CARTESIAN_POINT('Ctrl Pts',(-15.4104571591017,9.54175110365538,
-561.516075295761));
#151772=CARTESIAN_POINT('Ctrl Pts',(-14.4026149179538,10.8763499173728,
-563.010192942819));
#151773=CARTESIAN_POINT('Ctrl Pts',(-13.3947726768058,12.2109487310903,
-564.504310589878));
#151774=CARTESIAN_POINT('Ctrl Pts',(-12.1588589765331,13.3376329379985,
-565.998428236937));
#151775=CARTESIAN_POINT('Ctrl Pts',(-10.9229452762603,14.4643171449067,
-567.492545883996));
#151776=CARTESIAN_POINT('Ctrl Pts',(-9.50104767561052,15.3447188656481,
-568.986663531055));
#151777=CARTESIAN_POINT('Ctrl Pts',(-8.07915007496071,16.2251205863895,
-570.480781178114));
#151778=CARTESIAN_POINT('Ctrl Pts',(-6.51968959134574,16.8292587962898,
-571.974898825173));
#151779=CARTESIAN_POINT('Ctrl Pts',(-4.96022910773078,17.4333970061901,
-573.469016472231));
#151780=CARTESIAN_POINT('Ctrl Pts',(-3.31631129755346,17.7406985030951,
-574.96313411929));
#151781=CARTESIAN_POINT('Ctrl Pts',(-1.67239348737615,18.048,-576.457251766349));
#151782=CARTESIAN_POINT('Ctrl Pts',(-2.21024254310115E-15,18.048,-577.951369413408));
#151783=CARTESIAN_POINT('Ctrl Pts',(1.67239348737616,18.048,-579.445487060466));
#151784=CARTESIAN_POINT('Ctrl Pts',(3.31631129755346,17.7406985030951,-580.939604707525));
#151785=CARTESIAN_POINT('Ctrl Pts',(4.96022910773077,17.4333970061901,-582.433722354584));
#151786=CARTESIAN_POINT('Ctrl Pts',(6.51968959134575,16.8292587962898,-583.927840001643));
#151787=CARTESIAN_POINT('Ctrl Pts',(8.07915007496071,16.2251205863895,-585.421957648702));
#151788=CARTESIAN_POINT('Ctrl Pts',(9.50104767561053,15.3447188656481,-586.916075295761));
#151789=CARTESIAN_POINT('Ctrl Pts',(10.9229452762603,14.4643171449067,-588.41019294282));
#151790=CARTESIAN_POINT('Ctrl Pts',(12.1588589765331,13.3376329379985,-589.904310589878));
#151791=CARTESIAN_POINT('Ctrl Pts',(13.3947726768058,12.2109487310903,-591.398428236938));
#151792=CARTESIAN_POINT('Ctrl Pts',(14.4026149179538,10.8763499173728,-592.892545883996));
#151793=CARTESIAN_POINT('Ctrl Pts',(15.4104571591017,9.54175110365538,-594.386663531055));
#151794=CARTESIAN_POINT('Ctrl Pts',(16.1559070823762,8.04468584505496,-595.880781178113));
#151795=CARTESIAN_POINT('Ctrl Pts',(16.9013570056506,6.54762058645456,-597.374898825172));
#151796=CARTESIAN_POINT('Ctrl Pts',(17.3590292079831,4.93906964482096,-598.869016472231));
#151797=CARTESIAN_POINT('Ctrl Pts',(17.8167014103155,3.33051870318735,-600.36313411929));
#151798=CARTESIAN_POINT('Ctrl Pts',(17.9710104137728,1.66525935159367,-601.857251766349));
#151799=CARTESIAN_POINT('Ctrl Pts',(18.1253194172301,3.32956716117513E-15,
-603.351369413408));
#151800=CARTESIAN_POINT('Ctrl Pts',(17.9710104137728,-1.66525935159367,
-604.845487060467));
#151801=CARTESIAN_POINT('Ctrl Pts',(17.8167014103155,-3.33051870318736,
-606.339604707526));
#151802=CARTESIAN_POINT('Ctrl Pts',(17.3590292079831,-4.93906964482095,
-607.833722354584));
#151803=CARTESIAN_POINT('Ctrl Pts',(16.9013570056506,-6.54762058645456,
-609.327840001643));
#151804=CARTESIAN_POINT('Ctrl Pts',(16.1559070823762,-8.04468584505497,
-610.821957648702));
#151805=CARTESIAN_POINT('Ctrl Pts',(15.4104571591017,-9.54175110365538,
-612.316075295761));
#151806=CARTESIAN_POINT('Ctrl Pts',(14.4026149179538,-10.8763499173728,
-613.810192942819));
#151807=CARTESIAN_POINT('Ctrl Pts',(13.3947726768058,-12.2109487310903,
-615.304310589878));
#151808=CARTESIAN_POINT('Ctrl Pts',(12.1588589765331,-13.3376329379985,
-616.798428236937));
#151809=CARTESIAN_POINT('Ctrl Pts',(10.9229452762603,-14.4643171449067,
-618.292545883996));
#151810=CARTESIAN_POINT('Ctrl Pts',(9.50104767561053,-15.3447188656481,
-619.786663531055));
#151811=CARTESIAN_POINT('Ctrl Pts',(8.07915007496071,-16.2251205863895,
-621.280781178114));
#151812=CARTESIAN_POINT('Ctrl Pts',(6.51968959134574,-16.8292587962898,
-622.774898825172));
#151813=CARTESIAN_POINT('Ctrl Pts',(4.96022910773078,-17.4333970061901,
-624.269016472231));
#151814=CARTESIAN_POINT('Ctrl Pts',(3.31631129755346,-17.7406985030951,
-625.76313411929));
#151815=CARTESIAN_POINT('Ctrl Pts',(1.67239348737615,-18.048,-627.257251766349));
#151816=CARTESIAN_POINT('Ctrl Pts',(0.,-18.048,-628.751369413408));
#151817=CARTESIAN_POINT('Ctrl Pts',(-1.67239348737615,-18.048,-630.245487060467));
#151818=CARTESIAN_POINT('Ctrl Pts',(-3.31631129755346,-17.7406985030951,
-631.739604707525));
#151819=CARTESIAN_POINT('Ctrl Pts',(-4.96022910773077,-17.4333970061901,
-633.233722354584));
#151820=CARTESIAN_POINT('Ctrl Pts',(-6.51968959134574,-16.8292587962898,
-634.727840001643));
#151821=CARTESIAN_POINT('Ctrl Pts',(-8.07915007496071,-16.2251205863895,
-636.221957648702));
#151822=CARTESIAN_POINT('Ctrl Pts',(-9.50104767561052,-15.3447188656481,
-637.71607529576));
#151823=CARTESIAN_POINT('Ctrl Pts',(-10.9229452762603,-14.4643171449067,
-639.210192942819));
#151824=CARTESIAN_POINT('Ctrl Pts',(-12.1588589765331,-13.3376329379985,
-640.704310589878));
#151825=CARTESIAN_POINT('Ctrl Pts',(-13.3947726768058,-12.2109487310903,
-642.198428236937));
#151826=CARTESIAN_POINT('Ctrl Pts',(-14.4026149179538,-10.8763499173728,
-643.692545883996));
#151827=CARTESIAN_POINT('Ctrl Pts',(-15.4104571591017,-9.54175110365538,
-645.186663531055));
#151828=CARTESIAN_POINT('Ctrl Pts',(-16.1559070823762,-8.04468584505497,
-646.680781178114));
#151829=CARTESIAN_POINT('Ctrl Pts',(-16.9013570056506,-6.54762058645456,
-648.174898825173));
#151830=CARTESIAN_POINT('Ctrl Pts',(-17.3590292079831,-4.93906964482095,
-649.669016472231));
#151831=CARTESIAN_POINT('Ctrl Pts',(-17.8167014103155,-3.33051870318735,
-651.163134119291));
#151832=CARTESIAN_POINT('Ctrl Pts',(-17.9710104137728,-1.66525935159368,
-652.657251766349));
#151833=CARTESIAN_POINT('Ctrl Pts',(-18.1253194172301,-1.10985572039171E-15,
-654.151369413408));
#151834=CARTESIAN_POINT('Ctrl Pts',(-17.9710104137728,1.66525935159367,
-655.645487060466));
#151835=CARTESIAN_POINT('Ctrl Pts',(-17.8167014103155,3.33051870318735,
-657.139604707525));
#151836=CARTESIAN_POINT('Ctrl Pts',(-17.3590292079831,4.93906964482096,
-658.633722354584));
#151837=CARTESIAN_POINT('Ctrl Pts',(-16.9013570056506,6.54762058645456,
-660.127840001643));
#151838=CARTESIAN_POINT('Ctrl Pts',(-16.1559070823762,8.04468584505497,
-661.621957648702));
#151839=CARTESIAN_POINT('Ctrl Pts',(-15.4104571591017,9.54175110365538,
-663.116075295761));
#151840=CARTESIAN_POINT('Ctrl Pts',(-14.4026149179538,10.8763499173728,
-664.61019294282));
#151841=CARTESIAN_POINT('Ctrl Pts',(-13.3947726768058,12.2109487310903,
-666.104310589879));
#151842=CARTESIAN_POINT('Ctrl Pts',(-12.1588589765331,13.3376329379985,
-667.598428236937));
#151843=CARTESIAN_POINT('Ctrl Pts',(-10.9229452762603,14.4643171449067,
-669.092545883996));
#151844=CARTESIAN_POINT('Ctrl Pts',(-9.50104767561052,15.3447188656481,
-670.586663531055));
#151845=CARTESIAN_POINT('Ctrl Pts',(-8.07915007496071,16.2251205863895,
-672.080781178114));
#151846=CARTESIAN_POINT('Ctrl Pts',(-6.51968959134574,16.8292587962898,
-673.574898825172));
#151847=CARTESIAN_POINT('Ctrl Pts',(-4.96022910773078,17.4333970061901,
-675.069016472231));
#151848=CARTESIAN_POINT('Ctrl Pts',(-3.31631129755346,17.7406985030951,
-676.56313411929));
#151849=CARTESIAN_POINT('Ctrl Pts',(-1.67239348737615,18.048,-678.057251766349));
#151850=CARTESIAN_POINT('Ctrl Pts',(-2.21024254310115E-15,18.048,-679.551369413408));
#151851=CARTESIAN_POINT('Ctrl Pts',(1.67239348737616,18.048,-681.045487060467));
#151852=CARTESIAN_POINT('Ctrl Pts',(3.31631129755346,17.7406985030951,-682.539604707525));
#151853=CARTESIAN_POINT('Ctrl Pts',(4.96022910773077,17.4333970061901,-684.033722354584));
#151854=CARTESIAN_POINT('Ctrl Pts',(6.51968959134575,16.8292587962898,-685.527840001643));
#151855=CARTESIAN_POINT('Ctrl Pts',(8.07915007496071,16.2251205863895,-687.021957648702));
#151856=CARTESIAN_POINT('Ctrl Pts',(9.50104767561053,15.3447188656481,-688.516075295761));
#151857=CARTESIAN_POINT('Ctrl Pts',(10.9229452762603,14.4643171449067,-690.01019294282));
#151858=CARTESIAN_POINT('Ctrl Pts',(12.1588589765331,13.3376329379985,-691.504310589879));
#151859=CARTESIAN_POINT('Ctrl Pts',(13.3947726768058,12.2109487310903,-692.998428236937));
#151860=CARTESIAN_POINT('Ctrl Pts',(14.4026149179538,10.8763499173728,-694.492545883996));
#151861=CARTESIAN_POINT('Ctrl Pts',(15.4104571591017,9.54175110365538,-695.986663531055));
#151862=CARTESIAN_POINT('Ctrl Pts',(16.1559070823762,8.04468584505496,-697.480781178113));
#151863=CARTESIAN_POINT('Ctrl Pts',(16.9013570056506,6.54762058645456,-698.974898825172));
#151864=CARTESIAN_POINT('Ctrl Pts',(17.3590292079831,4.93906964482096,-700.469016472231));
#151865=CARTESIAN_POINT('Ctrl Pts',(17.8167014103155,3.33051870318735,-701.96313411929));
#151866=CARTESIAN_POINT('Ctrl Pts',(17.9710104137728,1.66525935159367,-703.457251766349));
#151867=CARTESIAN_POINT('Ctrl Pts',(18.1253194172301,3.32956716117513E-15,
-704.951369413408));
#151868=CARTESIAN_POINT('Ctrl Pts',(17.9710104137728,-1.66525935159367,
-706.445487060467));
#151869=CARTESIAN_POINT('Ctrl Pts',(17.8167014103155,-3.33051870318736,
-707.939604707526));
#151870=CARTESIAN_POINT('Ctrl Pts',(17.3590292079831,-4.93906964482095,
-709.433722354584));
#151871=CARTESIAN_POINT('Ctrl Pts',(16.9013570056506,-6.54762058645456,
-710.927840001643));
#151872=CARTESIAN_POINT('Ctrl Pts',(16.1559070823762,-8.04468584505497,
-712.421957648702));
#151873=CARTESIAN_POINT('Ctrl Pts',(15.4104571591017,-9.54175110365538,
-713.91607529576));
#151874=CARTESIAN_POINT('Ctrl Pts',(14.4026149179538,-10.8763499173728,
-715.410192942819));
#151875=CARTESIAN_POINT('Ctrl Pts',(13.3947726768058,-12.2109487310903,
-716.904310589879));
#151876=CARTESIAN_POINT('Ctrl Pts',(12.1588589765331,-13.3376329379985,
-718.398428236937));
#151877=CARTESIAN_POINT('Ctrl Pts',(10.9229452762603,-14.4643171449067,
-719.892545883996));
#151878=CARTESIAN_POINT('Ctrl Pts',(9.50104767561053,-15.3447188656481,
-721.386663531055));
#151879=CARTESIAN_POINT('Ctrl Pts',(8.07915007496071,-16.2251205863895,
-722.880781178114));
#151880=CARTESIAN_POINT('Ctrl Pts',(6.51968959134574,-16.8292587962898,
-724.374898825173));
#151881=CARTESIAN_POINT('Ctrl Pts',(4.96022910773078,-17.4333970061901,
-725.869016472232));
#151882=CARTESIAN_POINT('Ctrl Pts',(3.31631129755346,-17.7406985030951,
-727.36313411929));
#151883=CARTESIAN_POINT('Ctrl Pts',(1.67239348737615,-18.048,-728.857251766349));
#151884=CARTESIAN_POINT('Ctrl Pts',(0.,-18.048,-730.351369413408));
#151885=CARTESIAN_POINT('Ctrl Pts',(-1.67239348737615,-18.048,-731.845487060467));
#151886=CARTESIAN_POINT('Ctrl Pts',(-3.31631129755346,-17.7406985030951,
-733.339604707525));
#151887=CARTESIAN_POINT('Ctrl Pts',(-4.96022910773077,-17.4333970061901,
-734.833722354584));
#151888=CARTESIAN_POINT('Ctrl Pts',(-6.51968959134574,-16.8292587962898,
-736.327840001643));
#151889=CARTESIAN_POINT('Ctrl Pts',(-8.07915007496071,-16.2251205863895,
-737.821957648702));
#151890=CARTESIAN_POINT('Ctrl Pts',(-9.50104767561052,-15.3447188656481,
-739.316075295761));
#151891=CARTESIAN_POINT('Ctrl Pts',(-10.9229452762603,-14.4643171449067,
-740.81019294282));
#151892=CARTESIAN_POINT('Ctrl Pts',(-12.1588589765331,-13.3376329379985,
-742.304310589878));
#151893=CARTESIAN_POINT('Ctrl Pts',(-13.3947726768058,-12.2109487310903,
-743.798428236937));
#151894=CARTESIAN_POINT('Ctrl Pts',(-14.4026149179538,-10.8763499173728,
-745.292545883996));
#151895=CARTESIAN_POINT('Ctrl Pts',(-15.4104571591017,-9.54175110365538,
-746.786663531055));
#151896=CARTESIAN_POINT('Ctrl Pts',(-16.1559070823762,-8.04468584505497,
-748.280781178114));
#151897=CARTESIAN_POINT('Ctrl Pts',(-16.9013570056506,-6.54762058645456,
-749.774898825172));
#151898=CARTESIAN_POINT('Ctrl Pts',(-17.3590292079831,-4.93906964482095,
-751.269016472231));
#151899=CARTESIAN_POINT('Ctrl Pts',(-17.8167014103155,-3.33051870318735,
-752.76313411929));
#151900=CARTESIAN_POINT('Ctrl Pts',(-17.9710104137728,-1.66525935159368,
-754.257251766349));
#151901=CARTESIAN_POINT('Ctrl Pts',(-18.1253194172301,-1.10985572039171E-15,
-755.751369413408));
#151902=CARTESIAN_POINT('Ctrl Pts',(-17.9710104137728,1.66525935159367,
-757.245487060466));
#151903=CARTESIAN_POINT('Ctrl Pts',(-17.8167014103155,3.33051870318735,
-758.739604707525));
#151904=CARTESIAN_POINT('Ctrl Pts',(-17.3590292079831,4.93906964482096,
-760.233722354584));
#151905=CARTESIAN_POINT('Ctrl Pts',(-16.9013570056506,6.54762058645456,
-761.727840001643));
#151906=CARTESIAN_POINT('Ctrl Pts',(-16.1559070823762,8.04468584505497,
-763.221957648702));
#151907=CARTESIAN_POINT('Ctrl Pts',(-15.4104571591017,9.54175110365538,
-764.716075295761));
#151908=CARTESIAN_POINT('Ctrl Pts',(-14.4026149179538,10.8763499173728,
-766.21019294282));
#151909=CARTESIAN_POINT('Ctrl Pts',(-13.3947726768058,12.2109487310903,
-767.704310589879));
#151910=CARTESIAN_POINT('Ctrl Pts',(-12.1588589765331,13.3376329379985,
-769.198428236937));
#151911=CARTESIAN_POINT('Ctrl Pts',(-10.9229452762603,14.4643171449067,
-770.692545883996));
#151912=CARTESIAN_POINT('Ctrl Pts',(-9.50104767561052,15.3447188656481,
-772.186663531055));
#151913=CARTESIAN_POINT('Ctrl Pts',(-8.07915007496071,16.2251205863895,
-773.680781178114));
#151914=CARTESIAN_POINT('Ctrl Pts',(-6.51968959134574,16.8292587962898,
-775.174898825172));
#151915=CARTESIAN_POINT('Ctrl Pts',(-4.96022910773078,17.4333970061901,
-776.669016472231));
#151916=CARTESIAN_POINT('Ctrl Pts',(-3.31631129755346,17.7406985030951,
-778.16313411929));
#151917=CARTESIAN_POINT('Ctrl Pts',(-1.67239348737615,18.048,-779.657251766349));
#151918=CARTESIAN_POINT('Ctrl Pts',(-2.21024254310115E-15,18.048,-781.151369413408));
#151919=CARTESIAN_POINT('Ctrl Pts',(1.67239348737616,18.048,-782.645487060467));
#151920=CARTESIAN_POINT('Ctrl Pts',(3.31631129755346,17.7406985030951,-784.139604707526));
#151921=CARTESIAN_POINT('Ctrl Pts',(4.96022910773077,17.4333970061901,-785.633722354585));
#151922=CARTESIAN_POINT('Ctrl Pts',(6.51968959134575,16.8292587962898,-787.127840001643));
#151923=CARTESIAN_POINT('Ctrl Pts',(8.07915007496071,16.2251205863895,-788.621957648702));
#151924=CARTESIAN_POINT('Ctrl Pts',(9.50104767561053,15.3447188656481,-790.116075295761));
#151925=CARTESIAN_POINT('Ctrl Pts',(10.9229452762603,14.4643171449067,-791.61019294282));
#151926=CARTESIAN_POINT('Ctrl Pts',(12.1588589765331,13.3376329379985,-793.104310589878));
#151927=CARTESIAN_POINT('Ctrl Pts',(13.3947726768058,12.2109487310903,-794.598428236937));
#151928=CARTESIAN_POINT('Ctrl Pts',(14.4026149179538,10.8763499173728,-796.092545883996));
#151929=CARTESIAN_POINT('Ctrl Pts',(15.4104571591017,9.54175110365538,-797.586663531055));
#151930=CARTESIAN_POINT('Ctrl Pts',(16.1559070823762,8.04468584505496,-799.080781178114));
#151931=CARTESIAN_POINT('Ctrl Pts',(16.9013570056506,6.54762058645456,-800.574898825173));
#151932=CARTESIAN_POINT('Ctrl Pts',(17.3590292079831,4.93906964482096,-802.069016472231));
#151933=CARTESIAN_POINT('Ctrl Pts',(17.8167014103155,3.33051870318735,-803.56313411929));
#151934=CARTESIAN_POINT('Ctrl Pts',(17.9710104137728,1.66525935159367,-805.057251766349));
#151935=CARTESIAN_POINT('Ctrl Pts',(18.1253194172301,3.32956716117513E-15,
-806.551369413408));
#151936=CARTESIAN_POINT('Ctrl Pts',(17.9710104137728,-1.66525935159367,
-808.045487060467));
#151937=CARTESIAN_POINT('Ctrl Pts',(17.8167014103155,-3.33051870318736,
-809.539604707526));
#151938=CARTESIAN_POINT('Ctrl Pts',(17.3590292079831,-4.93906964482095,
-811.033722354584));
#151939=CARTESIAN_POINT('Ctrl Pts',(16.9013570056506,-6.54762058645456,
-812.527840001643));
#151940=CARTESIAN_POINT('Ctrl Pts',(16.1559070823762,-8.04468584505497,
-814.021957648702));
#151941=CARTESIAN_POINT('Ctrl Pts',(15.4104571591017,-9.54175110365538,
-815.516075295761));
#151942=CARTESIAN_POINT('Ctrl Pts',(14.4026149179538,-10.8763499173728,
-817.010192942819));
#151943=CARTESIAN_POINT('Ctrl Pts',(13.3947726768058,-12.2109487310903,
-818.504310589878));
#151944=CARTESIAN_POINT('Ctrl Pts',(12.1588589765331,-13.3376329379985,
-819.998428236937));
#151945=CARTESIAN_POINT('Ctrl Pts',(10.9229452762603,-14.4643171449067,
-821.492545883996));
#151946=CARTESIAN_POINT('Ctrl Pts',(9.50104767561053,-15.3447188656481,
-822.986663531055));
#151947=CARTESIAN_POINT('Ctrl Pts',(8.07915007496071,-16.2251205863895,
-824.480781178114));
#151948=CARTESIAN_POINT('Ctrl Pts',(6.51968959134574,-16.8292587962898,
-825.974898825173));
#151949=CARTESIAN_POINT('Ctrl Pts',(4.96022910773078,-17.4333970061901,
-827.469016472232));
#151950=CARTESIAN_POINT('Ctrl Pts',(3.31631129755346,-17.7406985030951,
-828.96313411929));
#151951=CARTESIAN_POINT('Ctrl Pts',(1.67239348737615,-18.048,-830.457251766349));
#151952=CARTESIAN_POINT('Ctrl Pts',(0.,-18.048,-831.951369413408));
#151953=CARTESIAN_POINT('Ctrl Pts',(-1.67239348737615,-18.048,-833.445487060467));
#151954=CARTESIAN_POINT('Ctrl Pts',(-3.31631129755346,-17.7406985030951,
-834.939604707525));
#151955=CARTESIAN_POINT('Ctrl Pts',(-4.96022910773077,-17.4333970061901,
-836.433722354584));
#151956=CARTESIAN_POINT('Ctrl Pts',(-6.51968959134574,-16.8292587962898,
-837.927840001643));
#151957=CARTESIAN_POINT('Ctrl Pts',(-8.07915007496071,-16.2251205863895,
-839.421957648702));
#151958=CARTESIAN_POINT('Ctrl Pts',(-9.50104767561052,-15.3447188656481,
-840.916075295761));
#151959=CARTESIAN_POINT('Ctrl Pts',(-10.9229452762603,-14.4643171449067,
-842.41019294282));
#151960=CARTESIAN_POINT('Ctrl Pts',(-12.1588589765331,-13.3376329379985,
-843.904310589879));
#151961=CARTESIAN_POINT('Ctrl Pts',(-13.3947726768058,-12.2109487310903,
-845.398428236937));
#151962=CARTESIAN_POINT('Ctrl Pts',(-14.4026149179538,-10.8763499173728,
-846.892545883996));
#151963=CARTESIAN_POINT('Ctrl Pts',(-15.4104571591017,-9.54175110365538,
-848.386663531055));
#151964=CARTESIAN_POINT('Ctrl Pts',(-16.1559070823762,-8.04468584505497,
-849.880781178114));
#151965=CARTESIAN_POINT('Ctrl Pts',(-16.9013570056506,-6.54762058645456,
-851.374898825173));
#151966=CARTESIAN_POINT('Ctrl Pts',(-17.3590292079831,-4.93906964482095,
-852.869016472231));
#151967=CARTESIAN_POINT('Ctrl Pts',(-17.8167014103155,-3.33051870318735,
-854.36313411929));
#151968=CARTESIAN_POINT('Ctrl Pts',(-17.9710104137728,-1.66525935159368,
-855.857251766349));
#151969=CARTESIAN_POINT('Ctrl Pts',(-18.1253194172301,-1.10985572039171E-15,
-857.351369413408));
#151970=CARTESIAN_POINT('Ctrl Pts',(-17.9710104137728,1.66525935159367,
-858.845487060467));
#151971=CARTESIAN_POINT('Ctrl Pts',(-17.8167014103155,3.33051870318735,
-860.339604707526));
#151972=CARTESIAN_POINT('Ctrl Pts',(-17.3590292079831,4.93906964482096,
-861.833722354584));
#151973=CARTESIAN_POINT('Ctrl Pts',(-16.9013570056506,6.54762058645456,
-863.327840001643));
#151974=CARTESIAN_POINT('Ctrl Pts',(-16.1559070823762,8.04468584505497,
-864.821957648702));
#151975=CARTESIAN_POINT('Ctrl Pts',(-15.4104571591017,9.54175110365538,
-866.316075295761));
#151976=CARTESIAN_POINT('Ctrl Pts',(-14.4026149179538,10.8763499173728,
-867.810192942819));
#151977=CARTESIAN_POINT('Ctrl Pts',(-13.3947726768058,12.2109487310903,
-869.304310589878));
#151978=CARTESIAN_POINT('Ctrl Pts',(-12.1588589765331,13.3376329379985,
-870.798428236937));
#151979=CARTESIAN_POINT('Ctrl Pts',(-10.9229452762603,14.4643171449067,
-872.292545883996));
#151980=CARTESIAN_POINT('Ctrl Pts',(-9.50104767561052,15.3447188656481,
-873.786663531055));
#151981=CARTESIAN_POINT('Ctrl Pts',(-8.07915007496071,16.2251205863895,
-875.280781178114));
#151982=CARTESIAN_POINT('Ctrl Pts',(-6.51968959134574,16.8292587962898,
-876.774898825172));
#151983=CARTESIAN_POINT('Ctrl Pts',(-4.96022910773078,17.4333970061901,
-878.269016472231));
#151984=CARTESIAN_POINT('Ctrl Pts',(-3.31631129755346,17.7406985030951,
-879.76313411929));
#151985=CARTESIAN_POINT('Ctrl Pts',(-1.67239348737615,18.048,-881.257251766349));
#151986=CARTESIAN_POINT('Ctrl Pts',(-2.21024254310115E-15,18.048,-882.751369413408));
#151987=CARTESIAN_POINT('Ctrl Pts',(1.67239348737616,18.048,-884.245487060467));
#151988=CARTESIAN_POINT('Ctrl Pts',(3.31631129755346,17.7406985030951,-885.739604707526));
#151989=CARTESIAN_POINT('Ctrl Pts',(4.96022910773077,17.4333970061901,-887.233722354585));
#151990=CARTESIAN_POINT('Ctrl Pts',(6.51968959134575,16.8292587962898,-888.727840001643));
#151991=CARTESIAN_POINT('Ctrl Pts',(8.07915007496071,16.2251205863895,-890.221957648702));
#151992=CARTESIAN_POINT('Ctrl Pts',(9.50104767561053,15.3447188656481,-891.71607529576));
#151993=CARTESIAN_POINT('Ctrl Pts',(10.9229452762603,14.4643171449067,-893.21019294282));
#151994=CARTESIAN_POINT('Ctrl Pts',(12.1588589765331,13.3376329379985,-894.704310589878));
#151995=CARTESIAN_POINT('Ctrl Pts',(13.3947726768058,12.2109487310903,-896.198428236937));
#151996=CARTESIAN_POINT('Ctrl Pts',(14.4026149179538,10.8763499173728,-897.692545883996));
#151997=CARTESIAN_POINT('Ctrl Pts',(15.4104571591017,9.54175110365538,-899.186663531055));
#151998=CARTESIAN_POINT('Ctrl Pts',(16.1559070823762,8.04468584505496,-900.680781178114));
#151999=CARTESIAN_POINT('Ctrl Pts',(16.9013570056506,6.54762058645456,-902.174898825173));
#152000=CARTESIAN_POINT('Ctrl Pts',(17.3590292079831,4.93906964482096,-903.669016472231));
#152001=CARTESIAN_POINT('Ctrl Pts',(17.8167014103155,3.33051870318735,-905.16313411929));
#152002=CARTESIAN_POINT('Ctrl Pts',(17.9710104137728,1.66525935159367,-906.657251766349));
#152003=CARTESIAN_POINT('Ctrl Pts',(18.1253194172301,3.32956716117513E-15,
-908.151369413408));
#152004=CARTESIAN_POINT('Ctrl Pts',(17.9710104137728,-1.66525935159367,
-909.645487060466));
#152005=CARTESIAN_POINT('Ctrl Pts',(17.8167014103155,-3.33051870318736,
-911.139604707525));
#152006=CARTESIAN_POINT('Ctrl Pts',(17.3590292079831,-4.93906964482095,
-912.633722354584));
#152007=CARTESIAN_POINT('Ctrl Pts',(16.9013570056506,-6.54762058645456,
-914.127840001643));
#152008=CARTESIAN_POINT('Ctrl Pts',(16.1559070823762,-8.04468584505497,
-915.621957648702));
#152009=CARTESIAN_POINT('Ctrl Pts',(15.4104571591017,-9.54175110365538,
-917.116075295761));
#152010=CARTESIAN_POINT('Ctrl Pts',(14.4026149179538,-10.8763499173728,
-918.61019294282));
#152011=CARTESIAN_POINT('Ctrl Pts',(13.3947726768058,-12.2109487310903,
-920.104310589879));
#152012=CARTESIAN_POINT('Ctrl Pts',(12.1588589765331,-13.3376329379985,
-921.598428236937));
#152013=CARTESIAN_POINT('Ctrl Pts',(10.9229452762603,-14.4643171449067,
-923.092545883996));
#152014=CARTESIAN_POINT('Ctrl Pts',(9.50104767561053,-15.3447188656481,
-924.586663531055));
#152015=CARTESIAN_POINT('Ctrl Pts',(8.07915007496071,-16.2251205863895,
-926.080781178114));
#152016=CARTESIAN_POINT('Ctrl Pts',(6.51968959134574,-16.8292587962898,
-927.574898825172));
#152017=CARTESIAN_POINT('Ctrl Pts',(4.96022910773078,-17.4333970061901,
-929.069016472232));
#152018=CARTESIAN_POINT('Ctrl Pts',(3.31631129755346,-17.7406985030951,
-930.56313411929));
#152019=CARTESIAN_POINT('Ctrl Pts',(1.67239348737615,-18.048,-932.057251766349));
#152020=CARTESIAN_POINT('Ctrl Pts',(0.,-18.048,-933.551369413408));
#152021=CARTESIAN_POINT('Ctrl Pts',(-1.67239348737615,-18.048,-935.045487060467));
#152022=CARTESIAN_POINT('Ctrl Pts',(-3.31631129755346,-17.7406985030951,
-936.539604707525));
#152023=CARTESIAN_POINT('Ctrl Pts',(-4.96022910773077,-17.4333970061901,
-938.033722354584));
#152024=CARTESIAN_POINT('Ctrl Pts',(-6.51968959134574,-16.8292587962898,
-939.527840001643));
#152025=CARTESIAN_POINT('Ctrl Pts',(-8.07915007496071,-16.2251205863895,
-941.021957648702));
#152026=CARTESIAN_POINT('Ctrl Pts',(-9.50104767561052,-15.3447188656481,
-942.516075295761));
#152027=CARTESIAN_POINT('Ctrl Pts',(-10.9229452762603,-14.4643171449067,
-944.01019294282));
#152028=CARTESIAN_POINT('Ctrl Pts',(-12.1588589765331,-13.3376329379985,
-945.504310589878));
#152029=CARTESIAN_POINT('Ctrl Pts',(-13.3947726768058,-12.2109487310903,
-946.998428236937));
#152030=CARTESIAN_POINT('Ctrl Pts',(-14.4026149179538,-10.8763499173728,
-948.492545883996));
#152031=CARTESIAN_POINT('Ctrl Pts',(-15.4104571591017,-9.54175110365538,
-949.986663531055));
#152032=CARTESIAN_POINT('Ctrl Pts',(-16.1559070823762,-8.04468584505497,
-951.480781178113));
#152033=CARTESIAN_POINT('Ctrl Pts',(-16.9013570056506,-6.54762058645456,
-952.974898825173));
#152034=CARTESIAN_POINT('Ctrl Pts',(-17.3590292079831,-4.93906964482095,
-954.469016472231));
#152035=CARTESIAN_POINT('Ctrl Pts',(-17.8167014103155,-3.33051870318735,
-955.96313411929));
#152036=CARTESIAN_POINT('Ctrl Pts',(-17.9710104137728,-1.66525935159368,
-957.457251766349));
#152037=CARTESIAN_POINT('Ctrl Pts',(-18.1253194172301,-1.10985572039171E-15,
-958.951369413408));
#152038=CARTESIAN_POINT('Ctrl Pts',(-17.9710104137728,1.66525935159367,
-960.445487060467));
#152039=CARTESIAN_POINT('Ctrl Pts',(-17.8167014103155,3.33051870318735,
-961.939604707526));
#152040=CARTESIAN_POINT('Ctrl Pts',(-17.3590292079831,4.93906964482096,
-963.433722354584));
#152041=CARTESIAN_POINT('Ctrl Pts',(-16.9013570056506,6.54762058645456,
-964.927840001643));
#152042=CARTESIAN_POINT('Ctrl Pts',(-16.1559070823762,8.04468584505497,
-966.421957648702));
#152043=CARTESIAN_POINT('Ctrl Pts',(-15.4104571591017,9.54175110365538,
-967.916075295761));
#152044=CARTESIAN_POINT('Ctrl Pts',(-14.4026149179538,10.8763499173728,
-969.410192942819));
#152045=CARTESIAN_POINT('Ctrl Pts',(-13.3947726768058,12.2109487310903,
-970.904310589878));
#152046=CARTESIAN_POINT('Ctrl Pts',(-12.1588589765331,13.3376329379985,
-972.398428236937));
#152047=CARTESIAN_POINT('Ctrl Pts',(-10.9229452762603,14.4643171449067,
-973.892545883996));
#152048=CARTESIAN_POINT('Ctrl Pts',(-9.50104767561052,15.3447188656481,
-975.386663531055));
#152049=CARTESIAN_POINT('Ctrl Pts',(-8.07915007496071,16.2251205863895,
-976.880781178114));
#152050=CARTESIAN_POINT('Ctrl Pts',(-6.51968959134574,16.8292587962898,
-978.374898825173));
#152051=CARTESIAN_POINT('Ctrl Pts',(-4.96022910773078,17.4333970061901,
-979.869016472231));
#152052=CARTESIAN_POINT('Ctrl Pts',(-3.31631129755346,17.7406985030951,
-981.36313411929));
#152053=CARTESIAN_POINT('Ctrl Pts',(-1.67239348737615,18.048,-982.857251766349));
#152054=CARTESIAN_POINT('Ctrl Pts',(-2.21024254310115E-15,18.048,-984.351369413408));
#152055=CARTESIAN_POINT('Ctrl Pts',(1.67239348737616,18.048,-985.845487060466));
#152056=CARTESIAN_POINT('Ctrl Pts',(3.31631129755346,17.7406985030951,-987.339604707525));
#152057=CARTESIAN_POINT('Ctrl Pts',(4.96022910773077,17.4333970061901,-988.833722354585));
#152058=CARTESIAN_POINT('Ctrl Pts',(6.51968959134575,16.8292587962898,-990.327840001643));
#152059=CARTESIAN_POINT('Ctrl Pts',(8.07915007496071,16.2251205863895,-991.821957648702));
#152060=CARTESIAN_POINT('Ctrl Pts',(9.50104767561053,15.3447188656481,-993.316075295761));
#152061=CARTESIAN_POINT('Ctrl Pts',(10.9229452762603,14.4643171449067,-994.81019294282));
#152062=CARTESIAN_POINT('Ctrl Pts',(12.1588589765331,13.3376329379985,-996.304310589878));
#152063=CARTESIAN_POINT('Ctrl Pts',(13.3947726768058,12.2109487310903,-997.798428236937));
#152064=CARTESIAN_POINT('Ctrl Pts',(14.4026149179538,10.8763499173728,-999.292545883996));
#152065=CARTESIAN_POINT('Ctrl Pts',(15.4104571591017,9.54175110365538,-1000.78666353105));
#152066=CARTESIAN_POINT('Ctrl Pts',(16.1559070823762,8.04468584505496,-1002.28078117811));
#152067=CARTESIAN_POINT('Ctrl Pts',(16.9013570056506,6.54762058645456,-1003.77489882517));
#152068=CARTESIAN_POINT('Ctrl Pts',(17.3590292079831,4.93906964482096,-1005.26901647223));
#152069=CARTESIAN_POINT('Ctrl Pts',(17.8167014103155,3.33051870318735,-1006.76313411929));
#152070=CARTESIAN_POINT('Ctrl Pts',(17.9710104137728,1.66525935159367,-1008.25725176635));
#152071=CARTESIAN_POINT('Ctrl Pts',(18.1253194172301,3.32956716117513E-15,
-1009.75136941341));
#152072=CARTESIAN_POINT('Ctrl Pts',(17.9710104137728,-1.66525935159367,
-1011.24548706047));
#152073=CARTESIAN_POINT('Ctrl Pts',(17.8167014103155,-3.33051870318736,
-1012.73960470753));
#152074=CARTESIAN_POINT('Ctrl Pts',(17.3590292079831,-4.93906964482095,
-1014.23372235458));
#152075=CARTESIAN_POINT('Ctrl Pts',(16.9013570056506,-6.54762058645456,
-1015.72784000164));
#152076=CARTESIAN_POINT('Ctrl Pts',(16.1559070823762,-8.04468584505497,
-1017.2219576487));
#152077=CARTESIAN_POINT('Ctrl Pts',(15.4104571591017,-9.54175110365538,
-1018.71607529576));
#152078=CARTESIAN_POINT('Ctrl Pts',(14.4026149179538,-10.8763499173728,
-1020.21019294282));
#152079=CARTESIAN_POINT('Ctrl Pts',(13.3947726768058,-12.2109487310903,
-1021.70431058988));
#152080=CARTESIAN_POINT('Ctrl Pts',(12.1588589765331,-13.3376329379985,
-1023.19842823694));
#152081=CARTESIAN_POINT('Ctrl Pts',(10.9229452762603,-14.4643171449067,
-1024.692545884));
#152082=CARTESIAN_POINT('Ctrl Pts',(9.50104767561053,-15.3447188656481,
-1026.18666353105));
#152083=CARTESIAN_POINT('Ctrl Pts',(8.07915007496071,-16.2251205863895,
-1027.68078117811));
#152084=CARTESIAN_POINT('Ctrl Pts',(6.51968959134574,-16.8292587962898,
-1029.17489882517));
#152085=CARTESIAN_POINT('Ctrl Pts',(4.96022910773078,-17.4333970061901,
-1030.66901647223));
#152086=CARTESIAN_POINT('Ctrl Pts',(3.31631129755346,-17.7406985030951,
-1032.16313411929));
#152087=CARTESIAN_POINT('Ctrl Pts',(1.67239348737615,-18.048,-1033.65725176635));
#152088=CARTESIAN_POINT('Ctrl Pts',(0.,-18.048,-1035.15136941341));
#152089=CARTESIAN_POINT('Ctrl Pts',(-1.67239348737615,-18.048,-1036.64548706047));
#152090=CARTESIAN_POINT('Ctrl Pts',(-3.31631129755346,-17.7406985030951,
-1038.13960470753));
#152091=CARTESIAN_POINT('Ctrl Pts',(-4.96022910773077,-17.4333970061901,
-1039.63372235458));
#152092=CARTESIAN_POINT('Ctrl Pts',(-6.51968959134574,-16.8292587962898,
-1041.12784000164));
#152093=CARTESIAN_POINT('Ctrl Pts',(-8.07915007496071,-16.2251205863895,
-1042.6219576487));
#152094=CARTESIAN_POINT('Ctrl Pts',(-9.50104767561052,-15.3447188656481,
-1044.11607529576));
#152095=CARTESIAN_POINT('Ctrl Pts',(-10.9229452762603,-14.4643171449067,
-1045.61019294282));
#152096=CARTESIAN_POINT('Ctrl Pts',(-12.1588589765331,-13.3376329379985,
-1047.10431058988));
#152097=CARTESIAN_POINT('Ctrl Pts',(-13.3947726768058,-12.2109487310903,
-1048.59842823694));
#152098=CARTESIAN_POINT('Ctrl Pts',(-14.4026149179538,-10.8763499173728,
-1050.092545884));
#152099=CARTESIAN_POINT('Ctrl Pts',(-15.4104571591017,-9.54175110365538,
-1051.58666353105));
#152100=CARTESIAN_POINT('Ctrl Pts',(-16.1559070823762,-8.04468584505497,
-1053.08078117811));
#152101=CARTESIAN_POINT('Ctrl Pts',(-16.9013570056506,-6.54762058645456,
-1054.57489882517));
#152102=CARTESIAN_POINT('Ctrl Pts',(-17.3590292079831,-4.93906964482095,
-1056.06901647223));
#152103=CARTESIAN_POINT('Ctrl Pts',(-17.8167014103155,-3.33051870318735,
-1057.56313411929));
#152104=CARTESIAN_POINT('Ctrl Pts',(-17.9710104137728,-1.66525935159368,
-1059.05725176635));
#152105=CARTESIAN_POINT('Ctrl Pts',(-18.1253194172301,-1.10985572039171E-15,
-1060.55136941341));
#152106=CARTESIAN_POINT('Ctrl Pts',(-17.9710104137728,1.66525935159367,
-1062.04548706047));
#152107=CARTESIAN_POINT('Ctrl Pts',(-17.8167014103155,3.33051870318735,
-1063.53960470753));
#152108=CARTESIAN_POINT('Ctrl Pts',(-17.3590292079831,4.93906964482096,
-1065.03372235458));
#152109=CARTESIAN_POINT('Ctrl Pts',(-16.9013570056506,6.54762058645456,
-1066.52784000164));
#152110=CARTESIAN_POINT('Ctrl Pts',(-16.1559070823762,8.04468584505497,
-1068.0219576487));
#152111=CARTESIAN_POINT('Ctrl Pts',(-15.4104571591017,9.54175110365538,
-1069.51607529576));
#152112=CARTESIAN_POINT('Ctrl Pts',(-14.4026149179538,10.8763499173728,
-1071.01019294282));
#152113=CARTESIAN_POINT('Ctrl Pts',(-13.3947726768058,12.2109487310903,
-1072.50431058988));
#152114=CARTESIAN_POINT('Ctrl Pts',(-12.1588589765331,13.3376329379985,
-1073.99842823694));
#152115=CARTESIAN_POINT('Ctrl Pts',(-10.9229452762603,14.4643171449067,
-1075.492545884));
#152116=CARTESIAN_POINT('Ctrl Pts',(-9.50104767561052,15.3447188656481,
-1076.98666353105));
#152117=CARTESIAN_POINT('Ctrl Pts',(-8.07915007496071,16.2251205863895,
-1078.48078117811));
#152118=CARTESIAN_POINT('Ctrl Pts',(-6.51968959134574,16.8292587962898,
-1079.97489882517));
#152119=CARTESIAN_POINT('Ctrl Pts',(-4.96022910773078,17.4333970061901,
-1081.46901647223));
#152120=CARTESIAN_POINT('Ctrl Pts',(-3.31631129755346,17.7406985030951,
-1082.96313411929));
#152121=CARTESIAN_POINT('Ctrl Pts',(-1.67239348737615,18.048,-1084.45725176635));
#152122=CARTESIAN_POINT('Ctrl Pts',(-2.21024254310115E-15,18.048,-1085.95136941341));
#152123=CARTESIAN_POINT('Ctrl Pts',(1.67239348737616,18.048,-1087.44548706047));
#152124=CARTESIAN_POINT('Ctrl Pts',(3.31631129755346,17.7406985030951,-1088.93960470753));
#152125=CARTESIAN_POINT('Ctrl Pts',(4.96022910773077,17.4333970061901,-1090.43372235458));
#152126=CARTESIAN_POINT('Ctrl Pts',(6.51968959134575,16.8292587962898,-1091.92784000164));
#152127=CARTESIAN_POINT('Ctrl Pts',(8.07915007496071,16.2251205863895,-1093.4219576487));
#152128=CARTESIAN_POINT('Ctrl Pts',(9.50104767561053,15.3447188656481,-1094.91607529576));
#152129=CARTESIAN_POINT('Ctrl Pts',(10.9229452762603,14.4643171449067,-1096.41019294282));
#152130=CARTESIAN_POINT('Ctrl Pts',(12.1588589765331,13.3376329379985,-1097.90431058988));
#152131=CARTESIAN_POINT('Ctrl Pts',(13.3947726768058,12.2109487310903,-1099.39842823694));
#152132=CARTESIAN_POINT('Ctrl Pts',(14.4026149179538,10.8763499173728,-1100.892545884));
#152133=CARTESIAN_POINT('Ctrl Pts',(15.4104571591017,9.54175110365538,-1102.38666353105));
#152134=CARTESIAN_POINT('Ctrl Pts',(16.1559070823762,8.04468584505496,-1103.88078117811));
#152135=CARTESIAN_POINT('Ctrl Pts',(16.9013570056506,6.54762058645456,-1105.37489882517));
#152136=CARTESIAN_POINT('Ctrl Pts',(17.3590292079831,4.93906964482096,-1106.86901647223));
#152137=CARTESIAN_POINT('Ctrl Pts',(17.8167014103155,3.33051870318735,-1108.36313411929));
#152138=CARTESIAN_POINT('Ctrl Pts',(17.9710104137728,1.66525935159367,-1109.85725176635));
#152139=CARTESIAN_POINT('Ctrl Pts',(18.1253194172301,3.32956716117513E-15,
-1111.35136941341));
#152140=CARTESIAN_POINT('Ctrl Pts',(17.9710104137728,-1.66525935159367,
-1112.84548706047));
#152141=CARTESIAN_POINT('Ctrl Pts',(17.8167014103155,-3.33051870318736,
-1114.33960470753));
#152142=CARTESIAN_POINT('Ctrl Pts',(17.3590292079831,-4.93906964482095,
-1115.83372235458));
#152143=CARTESIAN_POINT('Ctrl Pts',(16.9013570056506,-6.54762058645456,
-1117.32784000164));
#152144=CARTESIAN_POINT('Ctrl Pts',(16.1559070823762,-8.04468584505497,
-1118.8219576487));
#152145=CARTESIAN_POINT('Ctrl Pts',(15.4104571591017,-9.54175110365538,
-1120.31607529576));
#152146=CARTESIAN_POINT('Ctrl Pts',(14.4026149179538,-10.8763499173728,
-1121.81019294282));
#152147=CARTESIAN_POINT('Ctrl Pts',(13.3947726768058,-12.2109487310903,
-1123.30431058988));
#152148=CARTESIAN_POINT('Ctrl Pts',(12.1588589765331,-13.3376329379985,
-1124.79842823694));
#152149=CARTESIAN_POINT('Ctrl Pts',(10.9229452762603,-14.4643171449067,
-1126.292545884));
#152150=CARTESIAN_POINT('Ctrl Pts',(9.50104767561053,-15.3447188656481,
-1127.78666353106));
#152151=CARTESIAN_POINT('Ctrl Pts',(8.07915007496071,-16.2251205863895,
-1129.28078117811));
#152152=CARTESIAN_POINT('Ctrl Pts',(6.51968959134574,-16.8292587962898,
-1130.77489882517));
#152153=CARTESIAN_POINT('Ctrl Pts',(4.96022910773078,-17.4333970061901,
-1132.26901647223));
#152154=CARTESIAN_POINT('Ctrl Pts',(3.31631129755346,-17.7406985030951,
-1133.76313411929));
#152155=CARTESIAN_POINT('Ctrl Pts',(1.67239348737615,-18.048,-1135.25725176635));
#152156=CARTESIAN_POINT('Ctrl Pts',(0.,-18.048,-1136.75136941341));
#152157=CARTESIAN_POINT('Ctrl Pts',(-1.67239348737615,-18.048,-1138.24548706047));
#152158=CARTESIAN_POINT('Ctrl Pts',(-3.31631129755346,-17.7406985030951,
-1139.73960470753));
#152159=CARTESIAN_POINT('Ctrl Pts',(-4.96022910773077,-17.4333970061901,
-1141.23372235458));
#152160=CARTESIAN_POINT('Ctrl Pts',(-6.51968959134574,-16.8292587962898,
-1142.72784000164));
#152161=CARTESIAN_POINT('Ctrl Pts',(-8.07915007496071,-16.2251205863895,
-1144.2219576487));
#152162=CARTESIAN_POINT('Ctrl Pts',(-9.50104767561052,-15.3447188656481,
-1145.71607529576));
#152163=CARTESIAN_POINT('Ctrl Pts',(-10.9229452762603,-14.4643171449067,
-1147.21019294282));
#152164=CARTESIAN_POINT('Ctrl Pts',(-12.1588589765331,-13.3376329379985,
-1148.70431058988));
#152165=CARTESIAN_POINT('Ctrl Pts',(-13.3947726768058,-12.2109487310903,
-1150.19842823694));
#152166=CARTESIAN_POINT('Ctrl Pts',(-14.4026149179538,-10.8763499173728,
-1151.692545884));
#152167=CARTESIAN_POINT('Ctrl Pts',(-15.4104571591017,-9.54175110365538,
-1153.18666353105));
#152168=CARTESIAN_POINT('Ctrl Pts',(-16.1559070823762,-8.04468584505497,
-1154.68078117811));
#152169=CARTESIAN_POINT('Ctrl Pts',(-16.9013570056506,-6.54762058645456,
-1156.17489882517));
#152170=CARTESIAN_POINT('Ctrl Pts',(-17.3590292079831,-4.93906964482095,
-1157.66901647223));
#152171=CARTESIAN_POINT('Ctrl Pts',(-17.8167014103155,-3.33051870318735,
-1159.16313411929));
#152172=CARTESIAN_POINT('Ctrl Pts',(-17.9710104137728,-1.66525935159368,
-1160.65725176635));
#152173=CARTESIAN_POINT('Ctrl Pts',(-18.1253194172301,-1.10985572039171E-15,
-1162.15136941341));
#152174=CARTESIAN_POINT('Ctrl Pts',(-17.9710104137728,1.66525935159367,
-1163.64548706047));
#152175=CARTESIAN_POINT('Ctrl Pts',(-17.8167014103155,3.33051870318735,
-1165.13960470753));
#152176=CARTESIAN_POINT('Ctrl Pts',(-17.3590292079831,4.93906964482096,
-1166.63372235458));
#152177=CARTESIAN_POINT('Ctrl Pts',(-16.9013570056506,6.54762058645456,
-1168.12784000164));
#152178=CARTESIAN_POINT('Ctrl Pts',(-16.1559070823762,8.04468584505497,
-1169.6219576487));
#152179=CARTESIAN_POINT('Ctrl Pts',(-15.4104571591017,9.54175110365538,
-1171.11607529576));
#152180=CARTESIAN_POINT('Ctrl Pts',(-14.4026149179538,10.8763499173728,
-1172.61019294282));
#152181=CARTESIAN_POINT('Ctrl Pts',(-13.3947726768058,12.2109487310903,
-1174.10431058988));
#152182=CARTESIAN_POINT('Ctrl Pts',(-12.1588589765331,13.3376329379985,
-1175.59842823694));
#152183=CARTESIAN_POINT('Ctrl Pts',(-10.9229452762603,14.4643171449067,
-1177.092545884));
#152184=CARTESIAN_POINT('Ctrl Pts',(-9.50104767561052,15.3447188656481,
-1178.58666353105));
#152185=CARTESIAN_POINT('Ctrl Pts',(-8.07915007496071,16.2251205863895,
-1180.08078117811));
#152186=CARTESIAN_POINT('Ctrl Pts',(-6.51968959134574,16.8292587962898,
-1181.57489882517));
#152187=CARTESIAN_POINT('Ctrl Pts',(-4.96022910773078,17.4333970061901,
-1183.06901647223));
#152188=CARTESIAN_POINT('Ctrl Pts',(-3.31631129755346,17.7406985030951,
-1184.56313411929));
#152189=CARTESIAN_POINT('Ctrl Pts',(-1.67239348737615,18.048,-1186.05725176635));
#152190=CARTESIAN_POINT('Ctrl Pts',(-2.21024254310115E-15,18.048,-1187.55136941341));
#152191=CARTESIAN_POINT('Ctrl Pts',(1.67239348737616,18.048,-1189.04548706047));
#152192=CARTESIAN_POINT('Ctrl Pts',(3.31631129755346,17.7406985030951,-1190.53960470753));
#152193=CARTESIAN_POINT('Ctrl Pts',(4.96022910773077,17.4333970061901,-1192.03372235458));
#152194=CARTESIAN_POINT('Ctrl Pts',(6.51968959134575,16.8292587962898,-1193.52784000164));
#152195=CARTESIAN_POINT('Ctrl Pts',(8.07915007496071,16.2251205863895,-1195.0219576487));
#152196=CARTESIAN_POINT('Ctrl Pts',(9.50104767561053,15.3447188656481,-1196.51607529576));
#152197=CARTESIAN_POINT('Ctrl Pts',(10.9229452762603,14.4643171449067,-1198.01019294282));
#152198=CARTESIAN_POINT('Ctrl Pts',(12.1588589765331,13.3376329379985,-1199.50431058988));
#152199=CARTESIAN_POINT('Ctrl Pts',(13.3947726768058,12.2109487310903,-1200.99842823694));
#152200=CARTESIAN_POINT('Ctrl Pts',(14.4026149179538,10.8763499173728,-1202.492545884));
#152201=CARTESIAN_POINT('Ctrl Pts',(15.4104571591017,9.54175110365538,-1203.98666353106));
#152202=CARTESIAN_POINT('Ctrl Pts',(16.1559070823762,8.04468584505496,-1205.48078117811));
#152203=CARTESIAN_POINT('Ctrl Pts',(16.9013570056506,6.54762058645456,-1206.97489882517));
#152204=CARTESIAN_POINT('Ctrl Pts',(17.3590292079831,4.93906964482096,-1208.46901647223));
#152205=CARTESIAN_POINT('Ctrl Pts',(17.8167014103155,3.33051870318735,-1209.96313411929));
#152206=CARTESIAN_POINT('Ctrl Pts',(17.9710104137728,1.66525935159367,-1211.45725176635));
#152207=CARTESIAN_POINT('Ctrl Pts',(18.1253194172301,3.32956716117513E-15,
-1212.95136941341));
#152208=CARTESIAN_POINT('Ctrl Pts',(17.9710104137728,-1.66525935159367,
-1214.44548706047));
#152209=CARTESIAN_POINT('Ctrl Pts',(17.8167014103155,-3.33051870318736,
-1215.93960470753));
#152210=CARTESIAN_POINT('Ctrl Pts',(17.3590292079831,-4.93906964482095,
-1217.43372235458));
#152211=CARTESIAN_POINT('Ctrl Pts',(16.9013570056506,-6.54762058645456,
-1218.92784000164));
#152212=CARTESIAN_POINT('Ctrl Pts',(16.1559070823762,-8.04468584505497,
-1220.4219576487));
#152213=CARTESIAN_POINT('Ctrl Pts',(15.4104571591017,-9.54175110365538,
-1221.91607529576));
#152214=CARTESIAN_POINT('Ctrl Pts',(14.4026149179538,-10.8763499173728,
-1223.41019294282));
#152215=CARTESIAN_POINT('Ctrl Pts',(13.3947726768058,-12.2109487310903,
-1224.90431058988));
#152216=CARTESIAN_POINT('Ctrl Pts',(12.1588589765331,-13.3376329379985,
-1226.39842823694));
#152217=CARTESIAN_POINT('Ctrl Pts',(10.9229452762603,-14.4643171449067,
-1227.892545884));
#152218=CARTESIAN_POINT('Ctrl Pts',(9.50104767561053,-15.3447188656481,
-1229.38666353105));
#152219=CARTESIAN_POINT('Ctrl Pts',(8.07915007496071,-16.2251205863895,
-1230.88078117811));
#152220=CARTESIAN_POINT('Ctrl Pts',(6.51968959134574,-16.8292587962898,
-1232.37489882517));
#152221=CARTESIAN_POINT('Ctrl Pts',(4.96022910773078,-17.4333970061901,
-1233.86901647223));
#152222=CARTESIAN_POINT('Ctrl Pts',(3.31631129755346,-17.7406985030951,
-1235.36313411929));
#152223=CARTESIAN_POINT('Ctrl Pts',(1.67239348737615,-18.048,-1236.85725176635));
#152224=CARTESIAN_POINT('Ctrl Pts',(0.,-18.048,-1238.35136941341));
#152225=CARTESIAN_POINT('Ctrl Pts',(-1.67239348737615,-18.048,-1239.84548706047));
#152226=CARTESIAN_POINT('Ctrl Pts',(-3.31631129755346,-17.7406985030951,
-1241.33960470753));
#152227=CARTESIAN_POINT('Ctrl Pts',(-4.96022910773077,-17.4333970061901,
-1242.83372235458));
#152228=CARTESIAN_POINT('Ctrl Pts',(-6.51968959134574,-16.8292587962898,
-1244.32784000164));
#152229=CARTESIAN_POINT('Ctrl Pts',(-8.07915007496071,-16.2251205863895,
-1245.8219576487));
#152230=CARTESIAN_POINT('Ctrl Pts',(-9.50104767561052,-15.3447188656481,
-1247.31607529576));
#152231=CARTESIAN_POINT('Ctrl Pts',(-10.9229452762603,-14.4643171449067,
-1248.81019294282));
#152232=CARTESIAN_POINT('Ctrl Pts',(-12.1588589765331,-13.3376329379985,
-1250.30431058988));
#152233=CARTESIAN_POINT('Ctrl Pts',(-13.3947726768058,-12.2109487310903,
-1251.79842823694));
#152234=CARTESIAN_POINT('Ctrl Pts',(-14.4026149179538,-10.8763499173728,
-1253.292545884));
#152235=CARTESIAN_POINT('Ctrl Pts',(-15.4104571591017,-9.54175110365538,
-1254.78666353105));
#152236=CARTESIAN_POINT('Ctrl Pts',(-16.1559070823762,-8.04468584505497,
-1256.28078117811));
#152237=CARTESIAN_POINT('Ctrl Pts',(-16.9013570056506,-6.54762058645456,
-1257.77489882517));
#152238=CARTESIAN_POINT('Ctrl Pts',(-17.3590292079831,-4.93906964482095,
-1259.26901647223));
#152239=CARTESIAN_POINT('Ctrl Pts',(-17.8167014103155,-3.33051870318735,
-1260.76313411929));
#152240=CARTESIAN_POINT('Ctrl Pts',(-17.9710104137728,-1.66525935159368,
-1262.25725176635));
#152241=CARTESIAN_POINT('Ctrl Pts',(-18.1253194172301,-1.10985572039171E-15,
-1263.75136941341));
#152242=CARTESIAN_POINT('Ctrl Pts',(-17.9710104137728,1.66525935159367,
-1265.24548706047));
#152243=CARTESIAN_POINT('Ctrl Pts',(-17.8167014103155,3.33051870318735,
-1266.73960470753));
#152244=CARTESIAN_POINT('Ctrl Pts',(-17.3590292079831,4.93906964482096,
-1268.23372235458));
#152245=CARTESIAN_POINT('Ctrl Pts',(-16.9013570056506,6.54762058645456,
-1269.72784000164));
#152246=CARTESIAN_POINT('Ctrl Pts',(-16.1559070823762,8.04468584505497,
-1271.2219576487));
#152247=CARTESIAN_POINT('Ctrl Pts',(-15.4104571591017,9.54175110365538,
-1272.71607529576));
#152248=CARTESIAN_POINT('Ctrl Pts',(-14.4026149179538,10.8763499173728,
-1274.21019294282));
#152249=CARTESIAN_POINT('Ctrl Pts',(-13.3947726768058,12.2109487310903,
-1275.70431058988));
#152250=CARTESIAN_POINT('Ctrl Pts',(-12.1588589765331,13.3376329379985,
-1277.19842823694));
#152251=CARTESIAN_POINT('Ctrl Pts',(-10.9229452762603,14.4643171449067,
-1278.692545884));
#152252=CARTESIAN_POINT('Ctrl Pts',(-9.50104767561052,15.3447188656481,
-1280.18666353105));
#152253=CARTESIAN_POINT('Ctrl Pts',(-8.07915007496071,16.2251205863895,
-1281.68078117811));
#152254=CARTESIAN_POINT('Ctrl Pts',(-6.51968959134574,16.8292587962898,
-1283.17489882517));
#152255=CARTESIAN_POINT('Ctrl Pts',(-4.96022910773078,17.4333970061901,
-1284.66901647223));
#152256=CARTESIAN_POINT('Ctrl Pts',(-3.31631129755346,17.7406985030951,
-1286.16313411929));
#152257=CARTESIAN_POINT('Ctrl Pts',(-1.67239348737615,18.048,-1287.65725176635));
#152258=CARTESIAN_POINT('Ctrl Pts',(-2.21024254310115E-15,18.048,-1289.15136941341));
#152259=CARTESIAN_POINT('Ctrl Pts',(1.67239348737616,18.048,-1290.64548706047));
#152260=CARTESIAN_POINT('Ctrl Pts',(3.31631129755346,17.7406985030951,-1292.13960470753));
#152261=CARTESIAN_POINT('Ctrl Pts',(4.96022910773077,17.4333970061901,-1293.63372235458));
#152262=CARTESIAN_POINT('Ctrl Pts',(6.51968959134575,16.8292587962898,-1295.12784000164));
#152263=CARTESIAN_POINT('Ctrl Pts',(8.07915007496071,16.2251205863895,-1296.6219576487));
#152264=CARTESIAN_POINT('Ctrl Pts',(9.50104767561053,15.3447188656481,-1298.11607529576));
#152265=CARTESIAN_POINT('Ctrl Pts',(10.9229452762603,14.4643171449067,-1299.61019294282));
#152266=CARTESIAN_POINT('Ctrl Pts',(12.1588589765331,13.3376329379985,-1301.10431058988));
#152267=CARTESIAN_POINT('Ctrl Pts',(13.3947726768058,12.2109487310903,-1302.59842823694));
#152268=CARTESIAN_POINT('Ctrl Pts',(14.4026149179538,10.8763499173728,-1304.092545884));
#152269=CARTESIAN_POINT('Ctrl Pts',(15.4104571591017,9.54175110365538,-1305.58666353106));
#152270=CARTESIAN_POINT('Ctrl Pts',(16.1559070823762,8.04468584505496,-1307.08078117811));
#152271=CARTESIAN_POINT('Ctrl Pts',(16.9013570056506,6.54762058645456,-1308.57489882517));
#152272=CARTESIAN_POINT('Ctrl Pts',(17.3590292079831,4.93906964482096,-1310.06901647223));
#152273=CARTESIAN_POINT('Ctrl Pts',(17.8167014103155,3.33051870318735,-1311.56313411929));
#152274=CARTESIAN_POINT('Ctrl Pts',(17.9710104137728,1.66525935159367,-1313.05725176635));
#152275=CARTESIAN_POINT('Ctrl Pts',(18.1253194172301,3.32956716117513E-15,
-1314.55136941341));
#152276=CARTESIAN_POINT('Ctrl Pts',(17.9710104137728,-1.66525935159367,
-1316.04548706047));
#152277=CARTESIAN_POINT('Ctrl Pts',(17.8167014103155,-3.33051870318736,
-1317.53960470753));
#152278=CARTESIAN_POINT('Ctrl Pts',(17.3590292079831,-4.93906964482095,
-1319.03372235458));
#152279=CARTESIAN_POINT('Ctrl Pts',(16.9013570056506,-6.54762058645456,
-1320.52784000164));
#152280=CARTESIAN_POINT('Ctrl Pts',(16.1559070823762,-8.04468584505497,
-1322.0219576487));
#152281=CARTESIAN_POINT('Ctrl Pts',(15.4104571591017,-9.54175110365538,
-1323.51607529576));
#152282=CARTESIAN_POINT('Ctrl Pts',(14.4026149179538,-10.8763499173728,
-1325.01019294282));
#152283=CARTESIAN_POINT('Ctrl Pts',(13.3947726768058,-12.2109487310903,
-1326.50431058988));
#152284=CARTESIAN_POINT('Ctrl Pts',(12.1588589765331,-13.3376329379985,
-1327.99842823694));
#152285=CARTESIAN_POINT('Ctrl Pts',(10.9229452762603,-14.4643171449067,
-1329.492545884));
#152286=CARTESIAN_POINT('Ctrl Pts',(9.50104767561053,-15.3447188656481,
-1330.98666353105));
#152287=CARTESIAN_POINT('Ctrl Pts',(8.07915007496071,-16.2251205863895,
-1332.48078117811));
#152288=CARTESIAN_POINT('Ctrl Pts',(6.51968959134574,-16.8292587962898,
-1333.97489882517));
#152289=CARTESIAN_POINT('Ctrl Pts',(4.96022910773078,-17.4333970061901,
-1335.46901647223));
#152290=CARTESIAN_POINT('Ctrl Pts',(3.31631129755346,-17.7406985030951,
-1336.96313411929));
#152291=CARTESIAN_POINT('Ctrl Pts',(1.67239348737615,-18.048,-1338.45725176635));
#152292=CARTESIAN_POINT('Ctrl Pts',(0.,-18.048,-1339.95136941341));
#152293=CARTESIAN_POINT('Ctrl Pts',(-1.67239348737615,-18.048,-1341.44548706047));
#152294=CARTESIAN_POINT('Ctrl Pts',(-3.31631129755346,-17.7406985030951,
-1342.93960470753));
#152295=CARTESIAN_POINT('Ctrl Pts',(-4.96022910773077,-17.4333970061901,
-1344.43372235458));
#152296=CARTESIAN_POINT('Ctrl Pts',(-6.51968959134574,-16.8292587962898,
-1345.92784000164));
#152297=CARTESIAN_POINT('Ctrl Pts',(-8.07915007496071,-16.2251205863895,
-1347.4219576487));
#152298=CARTESIAN_POINT('Ctrl Pts',(-9.50104767561052,-15.3447188656481,
-1348.91607529576));
#152299=CARTESIAN_POINT('Ctrl Pts',(-10.9229452762603,-14.4643171449067,
-1350.41019294282));
#152300=CARTESIAN_POINT('Ctrl Pts',(-12.1588589765331,-13.3376329379985,
-1351.90431058988));
#152301=CARTESIAN_POINT('Ctrl Pts',(-13.3947726768058,-12.2109487310903,
-1353.39842823694));
#152302=CARTESIAN_POINT('Ctrl Pts',(-14.4026149179538,-10.8763499173728,
-1354.892545884));
#152303=CARTESIAN_POINT('Ctrl Pts',(-15.4104571591017,-9.54175110365538,
-1356.38666353105));
#152304=CARTESIAN_POINT('Ctrl Pts',(-16.1559070823762,-8.04468584505497,
-1357.88078117811));
#152305=CARTESIAN_POINT('Ctrl Pts',(-16.9013570056506,-6.54762058645456,
-1359.37489882517));
#152306=CARTESIAN_POINT('Ctrl Pts',(-17.3590292079831,-4.93906964482095,
-1360.86901647223));
#152307=CARTESIAN_POINT('Ctrl Pts',(-17.8167014103155,-3.33051870318735,
-1362.36313411929));
#152308=CARTESIAN_POINT('Ctrl Pts',(-17.9710104137728,-1.66525935159368,
-1363.85725176635));
#152309=CARTESIAN_POINT('Ctrl Pts',(-18.1253194172301,-1.10985572039171E-15,
-1365.35136941341));
#152310=CARTESIAN_POINT('Ctrl Pts',(-17.9710104137728,1.66525935159367,
-1366.84548706047));
#152311=CARTESIAN_POINT('Ctrl Pts',(-17.8167014103155,3.33051870318735,
-1368.33960470753));
#152312=CARTESIAN_POINT('Ctrl Pts',(-17.3590292079831,4.93906964482096,
-1369.83372235458));
#152313=CARTESIAN_POINT('Ctrl Pts',(-16.9013570056506,6.54762058645456,
-1371.32784000164));
#152314=CARTESIAN_POINT('Ctrl Pts',(-16.1559070823762,8.04468584505497,
-1372.8219576487));
#152315=CARTESIAN_POINT('Ctrl Pts',(-15.4104571591017,9.54175110365538,
-1374.31607529576));
#152316=CARTESIAN_POINT('Ctrl Pts',(-14.4026149179538,10.8763499173728,
-1375.81019294282));
#152317=CARTESIAN_POINT('Ctrl Pts',(-13.3947726768058,12.2109487310903,
-1377.30431058988));
#152318=CARTESIAN_POINT('Ctrl Pts',(-12.1588589765331,13.3376329379985,
-1378.79842823694));
#152319=CARTESIAN_POINT('Ctrl Pts',(-10.9229452762603,14.4643171449067,
-1380.292545884));
#152320=CARTESIAN_POINT('Ctrl Pts',(-9.50104767561052,15.3447188656481,
-1381.78666353106));
#152321=CARTESIAN_POINT('Ctrl Pts',(-8.07915007496071,16.2251205863895,
-1383.28078117811));
#152322=CARTESIAN_POINT('Ctrl Pts',(-6.51968959134574,16.8292587962898,
-1384.77489882517));
#152323=CARTESIAN_POINT('Ctrl Pts',(-4.96022910773078,17.4333970061901,
-1386.26901647223));
#152324=CARTESIAN_POINT('Ctrl Pts',(-3.31631129755346,17.7406985030951,
-1387.76313411929));
#152325=CARTESIAN_POINT('Ctrl Pts',(-1.67239348737615,18.048,-1389.25725176635));
#152326=CARTESIAN_POINT('Ctrl Pts',(-2.21024254310115E-15,18.048,-1390.75136941341));
#152327=CARTESIAN_POINT('Ctrl Pts',(1.67239348737616,18.048,-1392.24548706047));
#152328=CARTESIAN_POINT('Ctrl Pts',(3.31631129755346,17.7406985030951,-1393.73960470753));
#152329=CARTESIAN_POINT('Ctrl Pts',(4.96022910773077,17.4333970061901,-1395.23372235458));
#152330=CARTESIAN_POINT('Ctrl Pts',(6.51968959134575,16.8292587962898,-1396.72784000164));
#152331=CARTESIAN_POINT('Ctrl Pts',(8.07915007496071,16.2251205863895,-1398.2219576487));
#152332=CARTESIAN_POINT('Ctrl Pts',(9.50104767561053,15.3447188656481,-1399.71607529576));
#152333=CARTESIAN_POINT('Ctrl Pts',(10.9229452762603,14.4643171449067,-1401.21019294282));
#152334=CARTESIAN_POINT('Ctrl Pts',(12.1588589765331,13.3376329379985,-1402.70431058988));
#152335=CARTESIAN_POINT('Ctrl Pts',(13.3947726768058,12.2109487310903,-1404.19842823694));
#152336=CARTESIAN_POINT('Ctrl Pts',(14.4026149179538,10.8763499173728,-1405.692545884));
#152337=CARTESIAN_POINT('Ctrl Pts',(15.4104571591017,9.54175110365538,-1407.18666353106));
#152338=CARTESIAN_POINT('Ctrl Pts',(16.1559070823762,8.04468584505496,-1408.68078117811));
#152339=CARTESIAN_POINT('Ctrl Pts',(16.9013570056506,6.54762058645456,-1410.17489882517));
#152340=CARTESIAN_POINT('Ctrl Pts',(17.3590292079831,4.93906964482096,-1411.66901647223));
#152341=CARTESIAN_POINT('Ctrl Pts',(17.8167014103155,3.33051870318735,-1413.16313411929));
#152342=CARTESIAN_POINT('Ctrl Pts',(17.9710104137728,1.66525935159367,-1414.65725176635));
#152343=CARTESIAN_POINT('Ctrl Pts',(18.1253194172301,3.32956716117513E-15,
-1416.15136941341));
#152344=CARTESIAN_POINT('Ctrl Pts',(17.9710104137728,-1.66525935159367,
-1417.64548706047));
#152345=CARTESIAN_POINT('Ctrl Pts',(17.8167014103155,-3.33051870318736,
-1419.13960470753));
#152346=CARTESIAN_POINT('Ctrl Pts',(17.3590292079831,-4.93906964482095,
-1420.63372235458));
#152347=CARTESIAN_POINT('Ctrl Pts',(16.9013570056506,-6.54762058645456,
-1422.12784000164));
#152348=CARTESIAN_POINT('Ctrl Pts',(16.1559070823762,-8.04468584505497,
-1423.6219576487));
#152349=CARTESIAN_POINT('Ctrl Pts',(15.4104571591017,-9.54175110365538,
-1425.11607529576));
#152350=CARTESIAN_POINT('Ctrl Pts',(14.4026149179538,-10.8763499173728,
-1426.61019294282));
#152351=CARTESIAN_POINT('Ctrl Pts',(13.3947726768058,-12.2109487310903,
-1428.10431058988));
#152352=CARTESIAN_POINT('Ctrl Pts',(12.1588589765331,-13.3376329379985,
-1429.59842823694));
#152353=CARTESIAN_POINT('Ctrl Pts',(10.9229452762603,-14.4643171449067,
-1431.092545884));
#152354=CARTESIAN_POINT('Ctrl Pts',(9.50104767561053,-15.3447188656481,
-1432.58666353105));
#152355=CARTESIAN_POINT('Ctrl Pts',(8.07915007496071,-16.2251205863895,
-1434.08078117811));
#152356=CARTESIAN_POINT('Ctrl Pts',(6.51968959134574,-16.8292587962898,
-1435.57489882517));
#152357=CARTESIAN_POINT('Ctrl Pts',(4.96022910773078,-17.4333970061901,
-1437.06901647223));
#152358=CARTESIAN_POINT('Ctrl Pts',(3.31631129755346,-17.7406985030951,
-1438.56313411929));
#152359=CARTESIAN_POINT('Ctrl Pts',(1.67239348737615,-18.048,-1440.05725176635));
#152360=CARTESIAN_POINT('Ctrl Pts',(0.,-18.048,-1441.55136941341));
#152361=CARTESIAN_POINT('Ctrl Pts',(-1.67239348737615,-18.048,-1443.04548706047));
#152362=CARTESIAN_POINT('Ctrl Pts',(-3.31631129755346,-17.7406985030951,
-1444.53960470753));
#152363=CARTESIAN_POINT('Ctrl Pts',(-4.96022910773077,-17.4333970061901,
-1446.03372235458));
#152364=CARTESIAN_POINT('Ctrl Pts',(-6.51968959134574,-16.8292587962898,
-1447.52784000164));
#152365=CARTESIAN_POINT('Ctrl Pts',(-8.07915007496071,-16.2251205863895,
-1449.0219576487));
#152366=CARTESIAN_POINT('Ctrl Pts',(-9.50104767561052,-15.3447188656481,
-1450.51607529576));
#152367=CARTESIAN_POINT('Ctrl Pts',(-10.9229452762603,-14.4643171449067,
-1452.01019294282));
#152368=CARTESIAN_POINT('Ctrl Pts',(-12.1588589765331,-13.3376329379985,
-1453.50431058988));
#152369=CARTESIAN_POINT('Ctrl Pts',(-13.3947726768058,-12.2109487310903,
-1454.99842823694));
#152370=CARTESIAN_POINT('Ctrl Pts',(-14.4026149179538,-10.8763499173728,
-1456.492545884));
#152371=CARTESIAN_POINT('Ctrl Pts',(-15.4104571591017,-9.54175110365538,
-1457.98666353106));
#152372=CARTESIAN_POINT('Ctrl Pts',(-16.1559070823762,-8.04468584505497,
-1459.48078117811));
#152373=CARTESIAN_POINT('Ctrl Pts',(-16.9013570056506,-6.54762058645456,
-1460.97489882517));
#152374=CARTESIAN_POINT('Ctrl Pts',(-17.3590292079831,-4.93906964482095,
-1462.46901647223));
#152375=CARTESIAN_POINT('Ctrl Pts',(-17.8167014103155,-3.33051870318735,
-1463.96313411929));
#152376=CARTESIAN_POINT('Ctrl Pts',(-17.9710104137728,-1.66525935159368,
-1465.45725176635));
#152377=CARTESIAN_POINT('Ctrl Pts',(-18.1253194172301,-1.10985572039171E-15,
-1466.95136941341));
#152378=CARTESIAN_POINT('Ctrl Pts',(-17.9710104137728,1.66525935159367,
-1468.44548706047));
#152379=CARTESIAN_POINT('Ctrl Pts',(-17.8167014103155,3.33051870318735,
-1469.93960470753));
#152380=CARTESIAN_POINT('Ctrl Pts',(-17.3590292079831,4.93906964482096,
-1471.43372235458));
#152381=CARTESIAN_POINT('Ctrl Pts',(-16.9013570056506,6.54762058645456,
-1472.92784000164));
#152382=CARTESIAN_POINT('Ctrl Pts',(-16.1559070823762,8.04468584505497,
-1474.4219576487));
#152383=CARTESIAN_POINT('Ctrl Pts',(-15.4104571591017,9.54175110365538,
-1475.91607529576));
#152384=CARTESIAN_POINT('Ctrl Pts',(-14.4026149179538,10.8763499173728,
-1477.41019294282));
#152385=CARTESIAN_POINT('Ctrl Pts',(-13.3947726768058,12.2109487310903,
-1478.90431058988));
#152386=CARTESIAN_POINT('Ctrl Pts',(-12.1588589765331,13.3376329379985,
-1480.39842823694));
#152387=CARTESIAN_POINT('Ctrl Pts',(-10.9229452762603,14.4643171449067,
-1481.892545884));
#152388=CARTESIAN_POINT('Ctrl Pts',(-9.50104767561052,15.3447188656481,
-1483.38666353105));
#152389=CARTESIAN_POINT('Ctrl Pts',(-8.07915007496071,16.2251205863895,
-1484.88078117811));
#152390=CARTESIAN_POINT('Ctrl Pts',(-6.51968959134574,16.8292587962898,
-1486.37489882517));
#152391=CARTESIAN_POINT('Ctrl Pts',(-4.96022910773078,17.4333970061901,
-1487.86901647223));
#152392=CARTESIAN_POINT('Ctrl Pts',(-3.31631129755346,17.7406985030951,
-1489.36313411929));
#152393=CARTESIAN_POINT('Ctrl Pts',(-1.67239348737615,18.048,-1490.85725176635));
#152394=CARTESIAN_POINT('Ctrl Pts',(-2.21024254310115E-15,18.048,-1492.35136941341));
#152395=CARTESIAN_POINT('Ctrl Pts',(1.67239348737616,18.048,-1493.84548706047));
#152396=CARTESIAN_POINT('Ctrl Pts',(3.31631129755346,17.7406985030951,-1495.33960470753));
#152397=CARTESIAN_POINT('Ctrl Pts',(4.96022910773077,17.4333970061901,-1496.83372235458));
#152398=CARTESIAN_POINT('Ctrl Pts',(6.51968959134575,16.8292587962898,-1498.32784000164));
#152399=CARTESIAN_POINT('Ctrl Pts',(7.54128438222279,16.4334908658494,-1499.30662902594));
#152400=CARTESIAN_POINT('Ctrl Pts',(8.50750525179214,15.9170555816938,-1500.28920199011));
#152401=CARTESIAN_POINT('Ctrl Pts',(0.,-50.8,1503.759375));
#152402=CARTESIAN_POINT('Ctrl Pts',(-4.70731322909511,-50.8,1502.26525735294));
#152403=CARTESIAN_POINT('Ctrl Pts',(-9.33447550508177,-49.9350334639422,
1500.77113970588));
#152404=CARTESIAN_POINT('Ctrl Pts',(-13.9616377810684,-49.0700669278844,
1499.27702205882));
#152405=CARTESIAN_POINT('Ctrl Pts',(-18.3510766423074,-47.3695892537413,
1497.78290441177));
#152406=CARTESIAN_POINT('Ctrl Pts',(-22.7405155035463,-45.6691115795981,
1496.28878676471));
#152407=CARTESIAN_POINT('Ctrl Pts',(-26.7427538741697,-43.1910304950644,
1494.79466911765));
#152408=CARTESIAN_POINT('Ctrl Pts',(-30.744992244793,-40.7129494105307,
1493.30055147059));
#152409=CARTESIAN_POINT('Ctrl Pts',(-34.2237386972451,-37.5416529948095,
1491.80643382353));
#152410=CARTESIAN_POINT('Ctrl Pts',(-37.7024851496972,-34.3703565790883,
1490.31231617647));
#152411=CARTESIAN_POINT('Ctrl Pts',(-40.5392751458362,-30.6138395280662,
1488.81819852941));
#152412=CARTESIAN_POINT('Ctrl Pts',(-43.3760651419751,-26.8573224770441,
1487.32408088235));
#152413=CARTESIAN_POINT('Ctrl Pts',(-45.4742952008371,-22.6435084734481,
1485.82996323529));
#152414=CARTESIAN_POINT('Ctrl Pts',(-47.5725252596992,-18.4296944698521,
1484.33584558824));
#152415=CARTESIAN_POINT('Ctrl Pts',(-48.8607426731792,-13.9020798956618,
1482.84172794118));
#152416=CARTESIAN_POINT('Ctrl Pts',(-50.1489600866593,-9.37446532147148,
1481.34761029412));
#152417=CARTESIAN_POINT('Ctrl Pts',(-50.5832961557877,-4.68723266073574,
1479.85349264706));
#152418=CARTESIAN_POINT('Ctrl Pts',(-51.0176322249162,-3.12392900021603E-15,
1478.359375));
#152419=CARTESIAN_POINT('Ctrl Pts',(-50.5832961557877,4.68723266073573,
1476.86525735294));
#152420=CARTESIAN_POINT('Ctrl Pts',(-50.1489600866593,9.37446532147149,
1475.37113970588));
#152421=CARTESIAN_POINT('Ctrl Pts',(-48.8607426731792,13.9020798956618,
1473.87702205882));
#152422=CARTESIAN_POINT('Ctrl Pts',(-47.5725252596992,18.4296944698521,
1472.38290441176));
#152423=CARTESIAN_POINT('Ctrl Pts',(-45.4742952008371,22.6435084734481,
1470.88878676471));
#152424=CARTESIAN_POINT('Ctrl Pts',(-43.3760651419751,26.8573224770442,
1469.39466911765));
#152425=CARTESIAN_POINT('Ctrl Pts',(-40.5392751458362,30.6138395280662,
1467.90055147059));
#152426=CARTESIAN_POINT('Ctrl Pts',(-37.7024851496972,34.3703565790883,
1466.40643382353));
#152427=CARTESIAN_POINT('Ctrl Pts',(-34.2237386972451,37.5416529948095,
1464.91231617647));
#152428=CARTESIAN_POINT('Ctrl Pts',(-30.744992244793,40.7129494105307,1463.41819852941));
#152429=CARTESIAN_POINT('Ctrl Pts',(-26.7427538741697,43.1910304950644,
1461.92408088235));
#152430=CARTESIAN_POINT('Ctrl Pts',(-22.7405155035463,45.6691115795981,
1460.42996323529));
#152431=CARTESIAN_POINT('Ctrl Pts',(-18.3510766423074,47.3695892537413,
1458.93584558824));
#152432=CARTESIAN_POINT('Ctrl Pts',(-13.9616377810684,49.0700669278844,
1457.44172794118));
#152433=CARTESIAN_POINT('Ctrl Pts',(-9.33447550508177,49.9350334639422,
1455.94761029412));
#152434=CARTESIAN_POINT('Ctrl Pts',(-4.7073132290951,50.8,1454.45349264706));
#152435=CARTESIAN_POINT('Ctrl Pts',(-6.22120573966855E-15,50.8,1452.959375));
#152436=CARTESIAN_POINT('Ctrl Pts',(4.70731322909511,50.8,1451.46525735294));
#152437=CARTESIAN_POINT('Ctrl Pts',(9.33447550508176,49.9350334639422,1449.97113970588));
#152438=CARTESIAN_POINT('Ctrl Pts',(13.9616377810684,49.0700669278844,1448.47702205882));
#152439=CARTESIAN_POINT('Ctrl Pts',(18.3510766423074,47.3695892537413,1446.98290441176));
#152440=CARTESIAN_POINT('Ctrl Pts',(22.7405155035463,45.6691115795981,1445.48878676471));
#152441=CARTESIAN_POINT('Ctrl Pts',(26.7427538741697,43.1910304950644,1443.99466911765));
#152442=CARTESIAN_POINT('Ctrl Pts',(30.744992244793,40.7129494105307,1442.50055147059));
#152443=CARTESIAN_POINT('Ctrl Pts',(34.2237386972451,37.5416529948095,1441.00643382353));
#152444=CARTESIAN_POINT('Ctrl Pts',(37.7024851496972,34.3703565790883,1439.51231617647));
#152445=CARTESIAN_POINT('Ctrl Pts',(40.5392751458362,30.6138395280662,1438.01819852941));
#152446=CARTESIAN_POINT('Ctrl Pts',(43.3760651419751,26.8573224770442,1436.52408088235));
#152447=CARTESIAN_POINT('Ctrl Pts',(45.4742952008372,22.6435084734481,1435.02996323529));
#152448=CARTESIAN_POINT('Ctrl Pts',(47.5725252596992,18.4296944698521,1433.53584558824));
#152449=CARTESIAN_POINT('Ctrl Pts',(48.8607426731792,13.9020798956618,1432.04172794118));
#152450=CARTESIAN_POINT('Ctrl Pts',(50.1489600866593,9.37446532147146,1430.54761029412));
#152451=CARTESIAN_POINT('Ctrl Pts',(50.5832961557877,4.68723266073574,1429.05349264706));
#152452=CARTESIAN_POINT('Ctrl Pts',(51.0176322249162,9.37178700064808E-15,
1427.559375));
#152453=CARTESIAN_POINT('Ctrl Pts',(50.5832961557877,-4.68723266073572,
1426.06525735294));
#152454=CARTESIAN_POINT('Ctrl Pts',(50.1489600866593,-9.37446532147149,
1424.57113970588));
#152455=CARTESIAN_POINT('Ctrl Pts',(48.8607426731792,-13.9020798956618,
1423.07702205882));
#152456=CARTESIAN_POINT('Ctrl Pts',(47.5725252596992,-18.4296944698521,
1421.58290441176));
#152457=CARTESIAN_POINT('Ctrl Pts',(45.4742952008371,-22.6435084734482,
1420.08878676471));
#152458=CARTESIAN_POINT('Ctrl Pts',(43.3760651419751,-26.8573224770441,
1418.59466911765));
#152459=CARTESIAN_POINT('Ctrl Pts',(40.5392751458362,-30.6138395280662,
1417.10055147059));
#152460=CARTESIAN_POINT('Ctrl Pts',(37.7024851496972,-34.3703565790883,
1415.60643382353));
#152461=CARTESIAN_POINT('Ctrl Pts',(34.2237386972451,-37.5416529948095,
1414.11231617647));
#152462=CARTESIAN_POINT('Ctrl Pts',(30.744992244793,-40.7129494105307,1412.61819852941));
#152463=CARTESIAN_POINT('Ctrl Pts',(26.7427538741697,-43.1910304950644,
1411.12408088235));
#152464=CARTESIAN_POINT('Ctrl Pts',(22.7405155035463,-45.6691115795981,
1409.62996323529));
#152465=CARTESIAN_POINT('Ctrl Pts',(18.3510766423074,-47.3695892537413,
1408.13584558824));
#152466=CARTESIAN_POINT('Ctrl Pts',(13.9616377810684,-49.0700669278844,
1406.64172794118));
#152467=CARTESIAN_POINT('Ctrl Pts',(9.33447550508176,-49.9350334639422,
1405.14761029412));
#152468=CARTESIAN_POINT('Ctrl Pts',(4.70731322909511,-50.8,1403.65349264706));
#152469=CARTESIAN_POINT('Ctrl Pts',(0.,-50.8,1402.159375));
#152470=CARTESIAN_POINT('Ctrl Pts',(-4.70731322909511,-50.8,1400.66525735294));
#152471=CARTESIAN_POINT('Ctrl Pts',(-9.33447550508177,-49.9350334639422,
1399.17113970588));
#152472=CARTESIAN_POINT('Ctrl Pts',(-13.9616377810684,-49.0700669278844,
1397.67702205882));
#152473=CARTESIAN_POINT('Ctrl Pts',(-18.3510766423074,-47.3695892537413,
1396.18290441176));
#152474=CARTESIAN_POINT('Ctrl Pts',(-22.7405155035463,-45.6691115795981,
1394.68878676471));
#152475=CARTESIAN_POINT('Ctrl Pts',(-26.7427538741697,-43.1910304950644,
1393.19466911765));
#152476=CARTESIAN_POINT('Ctrl Pts',(-30.744992244793,-40.7129494105307,
1391.70055147059));
#152477=CARTESIAN_POINT('Ctrl Pts',(-34.2237386972451,-37.5416529948095,
1390.20643382353));
#152478=CARTESIAN_POINT('Ctrl Pts',(-37.7024851496972,-34.3703565790883,
1388.71231617647));
#152479=CARTESIAN_POINT('Ctrl Pts',(-40.5392751458362,-30.6138395280662,
1387.21819852941));
#152480=CARTESIAN_POINT('Ctrl Pts',(-43.3760651419751,-26.8573224770441,
1385.72408088235));
#152481=CARTESIAN_POINT('Ctrl Pts',(-45.4742952008371,-22.6435084734481,
1384.22996323529));
#152482=CARTESIAN_POINT('Ctrl Pts',(-47.5725252596992,-18.4296944698521,
1382.73584558824));
#152483=CARTESIAN_POINT('Ctrl Pts',(-48.8607426731792,-13.9020798956618,
1381.24172794118));
#152484=CARTESIAN_POINT('Ctrl Pts',(-50.1489600866593,-9.37446532147148,
1379.74761029412));
#152485=CARTESIAN_POINT('Ctrl Pts',(-50.5832961557877,-4.68723266073574,
1378.25349264706));
#152486=CARTESIAN_POINT('Ctrl Pts',(-51.0176322249162,-3.12392900021603E-15,
1376.759375));
#152487=CARTESIAN_POINT('Ctrl Pts',(-50.5832961557877,4.68723266073573,
1375.26525735294));
#152488=CARTESIAN_POINT('Ctrl Pts',(-50.1489600866593,9.37446532147149,
1373.77113970588));
#152489=CARTESIAN_POINT('Ctrl Pts',(-48.8607426731792,13.9020798956618,
1372.27702205882));
#152490=CARTESIAN_POINT('Ctrl Pts',(-47.5725252596992,18.4296944698521,
1370.78290441177));
#152491=CARTESIAN_POINT('Ctrl Pts',(-45.4742952008371,22.6435084734481,
1369.28878676471));
#152492=CARTESIAN_POINT('Ctrl Pts',(-43.3760651419751,26.8573224770442,
1367.79466911765));
#152493=CARTESIAN_POINT('Ctrl Pts',(-40.5392751458362,30.6138395280662,
1366.30055147059));
#152494=CARTESIAN_POINT('Ctrl Pts',(-37.7024851496972,34.3703565790883,
1364.80643382353));
#152495=CARTESIAN_POINT('Ctrl Pts',(-34.2237386972451,37.5416529948095,
1363.31231617647));
#152496=CARTESIAN_POINT('Ctrl Pts',(-30.744992244793,40.7129494105307,1361.81819852941));
#152497=CARTESIAN_POINT('Ctrl Pts',(-26.7427538741697,43.1910304950644,
1360.32408088235));
#152498=CARTESIAN_POINT('Ctrl Pts',(-22.7405155035463,45.6691115795981,
1358.82996323529));
#152499=CARTESIAN_POINT('Ctrl Pts',(-18.3510766423074,47.3695892537413,
1357.33584558824));
#152500=CARTESIAN_POINT('Ctrl Pts',(-13.9616377810684,49.0700669278844,
1355.84172794118));
#152501=CARTESIAN_POINT('Ctrl Pts',(-9.33447550508177,49.9350334639422,
1354.34761029412));
#152502=CARTESIAN_POINT('Ctrl Pts',(-4.7073132290951,50.8,1352.85349264706));
#152503=CARTESIAN_POINT('Ctrl Pts',(-6.22120573966855E-15,50.8,1351.359375));
#152504=CARTESIAN_POINT('Ctrl Pts',(4.70731322909511,50.8,1349.86525735294));
#152505=CARTESIAN_POINT('Ctrl Pts',(9.33447550508176,49.9350334639422,1348.37113970588));
#152506=CARTESIAN_POINT('Ctrl Pts',(13.9616377810684,49.0700669278844,1346.87702205882));
#152507=CARTESIAN_POINT('Ctrl Pts',(18.3510766423074,47.3695892537413,1345.38290441176));
#152508=CARTESIAN_POINT('Ctrl Pts',(22.7405155035463,45.6691115795981,1343.88878676471));
#152509=CARTESIAN_POINT('Ctrl Pts',(26.7427538741697,43.1910304950644,1342.39466911765));
#152510=CARTESIAN_POINT('Ctrl Pts',(30.744992244793,40.7129494105307,1340.90055147059));
#152511=CARTESIAN_POINT('Ctrl Pts',(34.2237386972451,37.5416529948095,1339.40643382353));
#152512=CARTESIAN_POINT('Ctrl Pts',(37.7024851496972,34.3703565790883,1337.91231617647));
#152513=CARTESIAN_POINT('Ctrl Pts',(40.5392751458362,30.6138395280662,1336.41819852941));
#152514=CARTESIAN_POINT('Ctrl Pts',(43.3760651419751,26.8573224770442,1334.92408088235));
#152515=CARTESIAN_POINT('Ctrl Pts',(45.4742952008372,22.6435084734481,1333.42996323529));
#152516=CARTESIAN_POINT('Ctrl Pts',(47.5725252596992,18.4296944698521,1331.93584558824));
#152517=CARTESIAN_POINT('Ctrl Pts',(48.8607426731792,13.9020798956618,1330.44172794118));
#152518=CARTESIAN_POINT('Ctrl Pts',(50.1489600866593,9.37446532147146,1328.94761029412));
#152519=CARTESIAN_POINT('Ctrl Pts',(50.5832961557877,4.68723266073574,1327.45349264706));
#152520=CARTESIAN_POINT('Ctrl Pts',(51.0176322249162,9.37178700064808E-15,
1325.959375));
#152521=CARTESIAN_POINT('Ctrl Pts',(50.5832961557877,-4.68723266073572,
1324.46525735294));
#152522=CARTESIAN_POINT('Ctrl Pts',(50.1489600866593,-9.37446532147149,
1322.97113970588));
#152523=CARTESIAN_POINT('Ctrl Pts',(48.8607426731792,-13.9020798956618,
1321.47702205882));
#152524=CARTESIAN_POINT('Ctrl Pts',(47.5725252596992,-18.4296944698521,
1319.98290441177));
#152525=CARTESIAN_POINT('Ctrl Pts',(45.4742952008371,-22.6435084734482,
1318.48878676471));
#152526=CARTESIAN_POINT('Ctrl Pts',(43.3760651419751,-26.8573224770441,
1316.99466911765));
#152527=CARTESIAN_POINT('Ctrl Pts',(40.5392751458362,-30.6138395280662,
1315.50055147059));
#152528=CARTESIAN_POINT('Ctrl Pts',(37.7024851496972,-34.3703565790883,
1314.00643382353));
#152529=CARTESIAN_POINT('Ctrl Pts',(34.2237386972451,-37.5416529948095,
1312.51231617647));
#152530=CARTESIAN_POINT('Ctrl Pts',(30.744992244793,-40.7129494105307,1311.01819852941));
#152531=CARTESIAN_POINT('Ctrl Pts',(26.7427538741697,-43.1910304950644,
1309.52408088235));
#152532=CARTESIAN_POINT('Ctrl Pts',(22.7405155035463,-45.6691115795981,
1308.02996323529));
#152533=CARTESIAN_POINT('Ctrl Pts',(18.3510766423074,-47.3695892537413,
1306.53584558824));
#152534=CARTESIAN_POINT('Ctrl Pts',(13.9616377810684,-49.0700669278844,
1305.04172794118));
#152535=CARTESIAN_POINT('Ctrl Pts',(9.33447550508176,-49.9350334639422,
1303.54761029412));
#152536=CARTESIAN_POINT('Ctrl Pts',(4.70731322909511,-50.8,1302.05349264706));
#152537=CARTESIAN_POINT('Ctrl Pts',(0.,-50.8,1300.559375));
#152538=CARTESIAN_POINT('Ctrl Pts',(-4.70731322909511,-50.8,1299.06525735294));
#152539=CARTESIAN_POINT('Ctrl Pts',(-9.33447550508177,-49.9350334639422,
1297.57113970588));
#152540=CARTESIAN_POINT('Ctrl Pts',(-13.9616377810684,-49.0700669278844,
1296.07702205882));
#152541=CARTESIAN_POINT('Ctrl Pts',(-18.3510766423074,-47.3695892537413,
1294.58290441176));
#152542=CARTESIAN_POINT('Ctrl Pts',(-22.7405155035463,-45.6691115795981,
1293.08878676471));
#152543=CARTESIAN_POINT('Ctrl Pts',(-26.7427538741697,-43.1910304950644,
1291.59466911765));
#152544=CARTESIAN_POINT('Ctrl Pts',(-30.744992244793,-40.7129494105307,
1290.10055147059));
#152545=CARTESIAN_POINT('Ctrl Pts',(-34.2237386972451,-37.5416529948095,
1288.60643382353));
#152546=CARTESIAN_POINT('Ctrl Pts',(-37.7024851496972,-34.3703565790883,
1287.11231617647));
#152547=CARTESIAN_POINT('Ctrl Pts',(-40.5392751458362,-30.6138395280662,
1285.61819852941));
#152548=CARTESIAN_POINT('Ctrl Pts',(-43.3760651419751,-26.8573224770441,
1284.12408088235));
#152549=CARTESIAN_POINT('Ctrl Pts',(-45.4742952008371,-22.6435084734481,
1282.62996323529));
#152550=CARTESIAN_POINT('Ctrl Pts',(-47.5725252596992,-18.4296944698521,
1281.13584558824));
#152551=CARTESIAN_POINT('Ctrl Pts',(-48.8607426731792,-13.9020798956618,
1279.64172794118));
#152552=CARTESIAN_POINT('Ctrl Pts',(-50.1489600866593,-9.37446532147148,
1278.14761029412));
#152553=CARTESIAN_POINT('Ctrl Pts',(-50.5832961557877,-4.68723266073574,
1276.65349264706));
#152554=CARTESIAN_POINT('Ctrl Pts',(-51.0176322249162,-3.12392900021603E-15,
1275.159375));
#152555=CARTESIAN_POINT('Ctrl Pts',(-50.5832961557877,4.68723266073573,
1273.66525735294));
#152556=CARTESIAN_POINT('Ctrl Pts',(-50.1489600866593,9.37446532147149,
1272.17113970588));
#152557=CARTESIAN_POINT('Ctrl Pts',(-48.8607426731792,13.9020798956618,
1270.67702205882));
#152558=CARTESIAN_POINT('Ctrl Pts',(-47.5725252596992,18.4296944698521,
1269.18290441176));
#152559=CARTESIAN_POINT('Ctrl Pts',(-45.4742952008371,22.6435084734481,
1267.68878676471));
#152560=CARTESIAN_POINT('Ctrl Pts',(-43.3760651419751,26.8573224770442,
1266.19466911765));
#152561=CARTESIAN_POINT('Ctrl Pts',(-40.5392751458362,30.6138395280662,
1264.70055147059));
#152562=CARTESIAN_POINT('Ctrl Pts',(-37.7024851496972,34.3703565790883,
1263.20643382353));
#152563=CARTESIAN_POINT('Ctrl Pts',(-34.2237386972451,37.5416529948095,
1261.71231617647));
#152564=CARTESIAN_POINT('Ctrl Pts',(-30.744992244793,40.7129494105307,1260.21819852941));
#152565=CARTESIAN_POINT('Ctrl Pts',(-26.7427538741697,43.1910304950644,
1258.72408088235));
#152566=CARTESIAN_POINT('Ctrl Pts',(-22.7405155035463,45.6691115795981,
1257.22996323529));
#152567=CARTESIAN_POINT('Ctrl Pts',(-18.3510766423074,47.3695892537413,
1255.73584558824));
#152568=CARTESIAN_POINT('Ctrl Pts',(-13.9616377810684,49.0700669278844,
1254.24172794118));
#152569=CARTESIAN_POINT('Ctrl Pts',(-9.33447550508177,49.9350334639422,
1252.74761029412));
#152570=CARTESIAN_POINT('Ctrl Pts',(-4.7073132290951,50.8,1251.25349264706));
#152571=CARTESIAN_POINT('Ctrl Pts',(-6.22120573966855E-15,50.8,1249.759375));
#152572=CARTESIAN_POINT('Ctrl Pts',(4.70731322909511,50.8,1248.26525735294));
#152573=CARTESIAN_POINT('Ctrl Pts',(9.33447550508176,49.9350334639422,1246.77113970588));
#152574=CARTESIAN_POINT('Ctrl Pts',(13.9616377810684,49.0700669278844,1245.27702205882));
#152575=CARTESIAN_POINT('Ctrl Pts',(18.3510766423074,47.3695892537413,1243.78290441176));
#152576=CARTESIAN_POINT('Ctrl Pts',(22.7405155035463,45.6691115795981,1242.28878676471));
#152577=CARTESIAN_POINT('Ctrl Pts',(26.7427538741697,43.1910304950644,1240.79466911765));
#152578=CARTESIAN_POINT('Ctrl Pts',(30.744992244793,40.7129494105307,1239.30055147059));
#152579=CARTESIAN_POINT('Ctrl Pts',(34.2237386972451,37.5416529948095,1237.80643382353));
#152580=CARTESIAN_POINT('Ctrl Pts',(37.7024851496972,34.3703565790883,1236.31231617647));
#152581=CARTESIAN_POINT('Ctrl Pts',(40.5392751458362,30.6138395280662,1234.81819852941));
#152582=CARTESIAN_POINT('Ctrl Pts',(43.3760651419751,26.8573224770442,1233.32408088235));
#152583=CARTESIAN_POINT('Ctrl Pts',(45.4742952008372,22.6435084734481,1231.82996323529));
#152584=CARTESIAN_POINT('Ctrl Pts',(47.5725252596992,18.4296944698521,1230.33584558824));
#152585=CARTESIAN_POINT('Ctrl Pts',(48.8607426731792,13.9020798956618,1228.84172794118));
#152586=CARTESIAN_POINT('Ctrl Pts',(50.1489600866593,9.37446532147146,1227.34761029412));
#152587=CARTESIAN_POINT('Ctrl Pts',(50.5832961557877,4.68723266073574,1225.85349264706));
#152588=CARTESIAN_POINT('Ctrl Pts',(51.0176322249162,9.37178700064808E-15,
1224.359375));
#152589=CARTESIAN_POINT('Ctrl Pts',(50.5832961557877,-4.68723266073572,
1222.86525735294));
#152590=CARTESIAN_POINT('Ctrl Pts',(50.1489600866593,-9.37446532147149,
1221.37113970588));
#152591=CARTESIAN_POINT('Ctrl Pts',(48.8607426731792,-13.9020798956618,
1219.87702205882));
#152592=CARTESIAN_POINT('Ctrl Pts',(47.5725252596992,-18.4296944698521,
1218.38290441176));
#152593=CARTESIAN_POINT('Ctrl Pts',(45.4742952008371,-22.6435084734482,
1216.88878676471));
#152594=CARTESIAN_POINT('Ctrl Pts',(43.3760651419751,-26.8573224770441,
1215.39466911765));
#152595=CARTESIAN_POINT('Ctrl Pts',(40.5392751458362,-30.6138395280662,
1213.90055147059));
#152596=CARTESIAN_POINT('Ctrl Pts',(37.7024851496972,-34.3703565790883,
1212.40643382353));
#152597=CARTESIAN_POINT('Ctrl Pts',(34.2237386972451,-37.5416529948095,
1210.91231617647));
#152598=CARTESIAN_POINT('Ctrl Pts',(30.744992244793,-40.7129494105307,1209.41819852941));
#152599=CARTESIAN_POINT('Ctrl Pts',(26.7427538741697,-43.1910304950644,
1207.92408088235));
#152600=CARTESIAN_POINT('Ctrl Pts',(22.7405155035463,-45.6691115795981,
1206.42996323529));
#152601=CARTESIAN_POINT('Ctrl Pts',(18.3510766423074,-47.3695892537413,
1204.93584558824));
#152602=CARTESIAN_POINT('Ctrl Pts',(13.9616377810684,-49.0700669278844,
1203.44172794118));
#152603=CARTESIAN_POINT('Ctrl Pts',(9.33447550508176,-49.9350334639422,
1201.94761029412));
#152604=CARTESIAN_POINT('Ctrl Pts',(4.70731322909511,-50.8,1200.45349264706));
#152605=CARTESIAN_POINT('Ctrl Pts',(0.,-50.8,1198.959375));
#152606=CARTESIAN_POINT('Ctrl Pts',(-4.70731322909511,-50.8,1197.46525735294));
#152607=CARTESIAN_POINT('Ctrl Pts',(-9.33447550508177,-49.9350334639422,
1195.97113970588));
#152608=CARTESIAN_POINT('Ctrl Pts',(-13.9616377810684,-49.0700669278844,
1194.47702205882));
#152609=CARTESIAN_POINT('Ctrl Pts',(-18.3510766423074,-47.3695892537413,
1192.98290441176));
#152610=CARTESIAN_POINT('Ctrl Pts',(-22.7405155035463,-45.6691115795981,
1191.48878676471));
#152611=CARTESIAN_POINT('Ctrl Pts',(-26.7427538741697,-43.1910304950644,
1189.99466911765));
#152612=CARTESIAN_POINT('Ctrl Pts',(-30.744992244793,-40.7129494105307,
1188.50055147059));
#152613=CARTESIAN_POINT('Ctrl Pts',(-34.2237386972451,-37.5416529948095,
1187.00643382353));
#152614=CARTESIAN_POINT('Ctrl Pts',(-37.7024851496972,-34.3703565790883,
1185.51231617647));
#152615=CARTESIAN_POINT('Ctrl Pts',(-40.5392751458362,-30.6138395280662,
1184.01819852941));
#152616=CARTESIAN_POINT('Ctrl Pts',(-43.3760651419751,-26.8573224770441,
1182.52408088235));
#152617=CARTESIAN_POINT('Ctrl Pts',(-45.4742952008371,-22.6435084734481,
1181.02996323529));
#152618=CARTESIAN_POINT('Ctrl Pts',(-47.5725252596992,-18.4296944698521,
1179.53584558824));
#152619=CARTESIAN_POINT('Ctrl Pts',(-48.8607426731792,-13.9020798956618,
1178.04172794118));
#152620=CARTESIAN_POINT('Ctrl Pts',(-50.1489600866593,-9.37446532147148,
1176.54761029412));
#152621=CARTESIAN_POINT('Ctrl Pts',(-50.5832961557877,-4.68723266073574,
1175.05349264706));
#152622=CARTESIAN_POINT('Ctrl Pts',(-51.0176322249162,-3.12392900021603E-15,
1173.559375));
#152623=CARTESIAN_POINT('Ctrl Pts',(-50.5832961557877,4.68723266073573,
1172.06525735294));
#152624=CARTESIAN_POINT('Ctrl Pts',(-50.1489600866593,9.37446532147149,
1170.57113970588));
#152625=CARTESIAN_POINT('Ctrl Pts',(-48.8607426731792,13.9020798956618,
1169.07702205882));
#152626=CARTESIAN_POINT('Ctrl Pts',(-47.5725252596992,18.4296944698521,
1167.58290441176));
#152627=CARTESIAN_POINT('Ctrl Pts',(-45.4742952008371,22.6435084734481,
1166.08878676471));
#152628=CARTESIAN_POINT('Ctrl Pts',(-43.3760651419751,26.8573224770442,
1164.59466911765));
#152629=CARTESIAN_POINT('Ctrl Pts',(-40.5392751458362,30.6138395280662,
1163.10055147059));
#152630=CARTESIAN_POINT('Ctrl Pts',(-37.7024851496972,34.3703565790883,
1161.60643382353));
#152631=CARTESIAN_POINT('Ctrl Pts',(-34.2237386972451,37.5416529948095,
1160.11231617647));
#152632=CARTESIAN_POINT('Ctrl Pts',(-30.744992244793,40.7129494105307,1158.61819852941));
#152633=CARTESIAN_POINT('Ctrl Pts',(-26.7427538741697,43.1910304950644,
1157.12408088235));
#152634=CARTESIAN_POINT('Ctrl Pts',(-22.7405155035463,45.6691115795981,
1155.62996323529));
#152635=CARTESIAN_POINT('Ctrl Pts',(-18.3510766423074,47.3695892537413,
1154.13584558824));
#152636=CARTESIAN_POINT('Ctrl Pts',(-13.9616377810684,49.0700669278844,
1152.64172794118));
#152637=CARTESIAN_POINT('Ctrl Pts',(-9.33447550508177,49.9350334639422,
1151.14761029412));
#152638=CARTESIAN_POINT('Ctrl Pts',(-4.7073132290951,50.8,1149.65349264706));
#152639=CARTESIAN_POINT('Ctrl Pts',(-6.22120573966855E-15,50.8,1148.159375));
#152640=CARTESIAN_POINT('Ctrl Pts',(4.70731322909511,50.8,1146.66525735294));
#152641=CARTESIAN_POINT('Ctrl Pts',(9.33447550508176,49.9350334639422,1145.17113970588));
#152642=CARTESIAN_POINT('Ctrl Pts',(13.9616377810684,49.0700669278844,1143.67702205882));
#152643=CARTESIAN_POINT('Ctrl Pts',(18.3510766423074,47.3695892537413,1142.18290441176));
#152644=CARTESIAN_POINT('Ctrl Pts',(22.7405155035463,45.6691115795981,1140.68878676471));
#152645=CARTESIAN_POINT('Ctrl Pts',(26.7427538741697,43.1910304950644,1139.19466911765));
#152646=CARTESIAN_POINT('Ctrl Pts',(30.744992244793,40.7129494105307,1137.70055147059));
#152647=CARTESIAN_POINT('Ctrl Pts',(34.2237386972451,37.5416529948095,1136.20643382353));
#152648=CARTESIAN_POINT('Ctrl Pts',(37.7024851496972,34.3703565790883,1134.71231617647));
#152649=CARTESIAN_POINT('Ctrl Pts',(40.5392751458362,30.6138395280662,1133.21819852941));
#152650=CARTESIAN_POINT('Ctrl Pts',(43.3760651419751,26.8573224770442,1131.72408088235));
#152651=CARTESIAN_POINT('Ctrl Pts',(45.4742952008372,22.6435084734481,1130.22996323529));
#152652=CARTESIAN_POINT('Ctrl Pts',(47.5725252596992,18.4296944698521,1128.73584558824));
#152653=CARTESIAN_POINT('Ctrl Pts',(48.8607426731792,13.9020798956618,1127.24172794118));
#152654=CARTESIAN_POINT('Ctrl Pts',(50.1489600866593,9.37446532147146,1125.74761029412));
#152655=CARTESIAN_POINT('Ctrl Pts',(50.5832961557877,4.68723266073574,1124.25349264706));
#152656=CARTESIAN_POINT('Ctrl Pts',(51.0176322249162,9.37178700064808E-15,
1122.759375));
#152657=CARTESIAN_POINT('Ctrl Pts',(50.5832961557877,-4.68723266073572,
1121.26525735294));
#152658=CARTESIAN_POINT('Ctrl Pts',(50.1489600866593,-9.37446532147149,
1119.77113970588));
#152659=CARTESIAN_POINT('Ctrl Pts',(48.8607426731792,-13.9020798956618,
1118.27702205882));
#152660=CARTESIAN_POINT('Ctrl Pts',(47.5725252596992,-18.4296944698521,
1116.78290441177));
#152661=CARTESIAN_POINT('Ctrl Pts',(45.4742952008371,-22.6435084734482,
1115.28878676471));
#152662=CARTESIAN_POINT('Ctrl Pts',(43.3760651419751,-26.8573224770441,
1113.79466911765));
#152663=CARTESIAN_POINT('Ctrl Pts',(40.5392751458362,-30.6138395280662,
1112.30055147059));
#152664=CARTESIAN_POINT('Ctrl Pts',(37.7024851496972,-34.3703565790883,
1110.80643382353));
#152665=CARTESIAN_POINT('Ctrl Pts',(34.2237386972451,-37.5416529948095,
1109.31231617647));
#152666=CARTESIAN_POINT('Ctrl Pts',(30.744992244793,-40.7129494105307,1107.81819852941));
#152667=CARTESIAN_POINT('Ctrl Pts',(26.7427538741697,-43.1910304950644,
1106.32408088235));
#152668=CARTESIAN_POINT('Ctrl Pts',(22.7405155035463,-45.6691115795981,
1104.82996323529));
#152669=CARTESIAN_POINT('Ctrl Pts',(18.3510766423074,-47.3695892537413,
1103.33584558824));
#152670=CARTESIAN_POINT('Ctrl Pts',(13.9616377810684,-49.0700669278844,
1101.84172794118));
#152671=CARTESIAN_POINT('Ctrl Pts',(9.33447550508176,-49.9350334639422,
1100.34761029412));
#152672=CARTESIAN_POINT('Ctrl Pts',(4.70731322909511,-50.8,1098.85349264706));
#152673=CARTESIAN_POINT('Ctrl Pts',(0.,-50.8,1097.359375));
#152674=CARTESIAN_POINT('Ctrl Pts',(-4.70731322909511,-50.8,1095.86525735294));
#152675=CARTESIAN_POINT('Ctrl Pts',(-9.33447550508177,-49.9350334639422,
1094.37113970588));
#152676=CARTESIAN_POINT('Ctrl Pts',(-13.9616377810684,-49.0700669278844,
1092.87702205882));
#152677=CARTESIAN_POINT('Ctrl Pts',(-18.3510766423074,-47.3695892537413,
1091.38290441176));
#152678=CARTESIAN_POINT('Ctrl Pts',(-22.7405155035463,-45.6691115795981,
1089.88878676471));
#152679=CARTESIAN_POINT('Ctrl Pts',(-26.7427538741697,-43.1910304950644,
1088.39466911765));
#152680=CARTESIAN_POINT('Ctrl Pts',(-30.744992244793,-40.7129494105307,
1086.90055147059));
#152681=CARTESIAN_POINT('Ctrl Pts',(-34.2237386972451,-37.5416529948095,
1085.40643382353));
#152682=CARTESIAN_POINT('Ctrl Pts',(-37.7024851496972,-34.3703565790883,
1083.91231617647));
#152683=CARTESIAN_POINT('Ctrl Pts',(-40.5392751458362,-30.6138395280662,
1082.41819852941));
#152684=CARTESIAN_POINT('Ctrl Pts',(-43.3760651419751,-26.8573224770441,
1080.92408088235));
#152685=CARTESIAN_POINT('Ctrl Pts',(-45.4742952008371,-22.6435084734481,
1079.42996323529));
#152686=CARTESIAN_POINT('Ctrl Pts',(-47.5725252596992,-18.4296944698521,
1077.93584558824));
#152687=CARTESIAN_POINT('Ctrl Pts',(-48.8607426731792,-13.9020798956618,
1076.44172794118));
#152688=CARTESIAN_POINT('Ctrl Pts',(-50.1489600866593,-9.37446532147148,
1074.94761029412));
#152689=CARTESIAN_POINT('Ctrl Pts',(-50.5832961557877,-4.68723266073574,
1073.45349264706));
#152690=CARTESIAN_POINT('Ctrl Pts',(-51.0176322249162,-3.12392900021603E-15,
1071.959375));
#152691=CARTESIAN_POINT('Ctrl Pts',(-50.5832961557877,4.68723266073573,
1070.46525735294));
#152692=CARTESIAN_POINT('Ctrl Pts',(-50.1489600866593,9.37446532147149,
1068.97113970588));
#152693=CARTESIAN_POINT('Ctrl Pts',(-48.8607426731792,13.9020798956618,
1067.47702205882));
#152694=CARTESIAN_POINT('Ctrl Pts',(-47.5725252596992,18.4296944698521,
1065.98290441176));
#152695=CARTESIAN_POINT('Ctrl Pts',(-45.4742952008371,22.6435084734481,
1064.48878676471));
#152696=CARTESIAN_POINT('Ctrl Pts',(-43.3760651419751,26.8573224770442,
1062.99466911765));
#152697=CARTESIAN_POINT('Ctrl Pts',(-40.5392751458362,30.6138395280662,
1061.50055147059));
#152698=CARTESIAN_POINT('Ctrl Pts',(-37.7024851496972,34.3703565790883,
1060.00643382353));
#152699=CARTESIAN_POINT('Ctrl Pts',(-34.2237386972451,37.5416529948095,
1058.51231617647));
#152700=CARTESIAN_POINT('Ctrl Pts',(-30.744992244793,40.7129494105307,1057.01819852941));
#152701=CARTESIAN_POINT('Ctrl Pts',(-26.7427538741697,43.1910304950644,
1055.52408088235));
#152702=CARTESIAN_POINT('Ctrl Pts',(-22.7405155035463,45.6691115795981,
1054.02996323529));
#152703=CARTESIAN_POINT('Ctrl Pts',(-18.3510766423074,47.3695892537413,
1052.53584558824));
#152704=CARTESIAN_POINT('Ctrl Pts',(-13.9616377810684,49.0700669278844,
1051.04172794118));
#152705=CARTESIAN_POINT('Ctrl Pts',(-9.33447550508177,49.9350334639422,
1049.54761029412));
#152706=CARTESIAN_POINT('Ctrl Pts',(-4.7073132290951,50.8,1048.05349264706));
#152707=CARTESIAN_POINT('Ctrl Pts',(-6.22120573966855E-15,50.8,1046.559375));
#152708=CARTESIAN_POINT('Ctrl Pts',(4.70731322909511,50.8,1045.06525735294));
#152709=CARTESIAN_POINT('Ctrl Pts',(9.33447550508176,49.9350334639422,1043.57113970588));
#152710=CARTESIAN_POINT('Ctrl Pts',(13.9616377810684,49.0700669278844,1042.07702205882));
#152711=CARTESIAN_POINT('Ctrl Pts',(18.3510766423074,47.3695892537413,1040.58290441176));
#152712=CARTESIAN_POINT('Ctrl Pts',(22.7405155035463,45.6691115795981,1039.08878676471));
#152713=CARTESIAN_POINT('Ctrl Pts',(26.7427538741697,43.1910304950644,1037.59466911765));
#152714=CARTESIAN_POINT('Ctrl Pts',(30.744992244793,40.7129494105307,1036.10055147059));
#152715=CARTESIAN_POINT('Ctrl Pts',(34.2237386972451,37.5416529948095,1034.60643382353));
#152716=CARTESIAN_POINT('Ctrl Pts',(37.7024851496972,34.3703565790883,1033.11231617647));
#152717=CARTESIAN_POINT('Ctrl Pts',(40.5392751458362,30.6138395280662,1031.61819852941));
#152718=CARTESIAN_POINT('Ctrl Pts',(43.3760651419751,26.8573224770442,1030.12408088235));
#152719=CARTESIAN_POINT('Ctrl Pts',(45.4742952008372,22.6435084734481,1028.62996323529));
#152720=CARTESIAN_POINT('Ctrl Pts',(47.5725252596992,18.4296944698521,1027.13584558824));
#152721=CARTESIAN_POINT('Ctrl Pts',(48.8607426731792,13.9020798956618,1025.64172794118));
#152722=CARTESIAN_POINT('Ctrl Pts',(50.1489600866593,9.37446532147146,1024.14761029412));
#152723=CARTESIAN_POINT('Ctrl Pts',(50.5832961557877,4.68723266073574,1022.65349264706));
#152724=CARTESIAN_POINT('Ctrl Pts',(51.0176322249162,9.37178700064808E-15,
1021.159375));
#152725=CARTESIAN_POINT('Ctrl Pts',(50.5832961557877,-4.68723266073572,
1019.66525735294));
#152726=CARTESIAN_POINT('Ctrl Pts',(50.1489600866593,-9.37446532147149,
1018.17113970588));
#152727=CARTESIAN_POINT('Ctrl Pts',(48.8607426731792,-13.9020798956618,
1016.67702205882));
#152728=CARTESIAN_POINT('Ctrl Pts',(47.5725252596992,-18.4296944698521,
1015.18290441177));
#152729=CARTESIAN_POINT('Ctrl Pts',(45.4742952008371,-22.6435084734482,
1013.68878676471));
#152730=CARTESIAN_POINT('Ctrl Pts',(43.3760651419751,-26.8573224770441,
1012.19466911765));
#152731=CARTESIAN_POINT('Ctrl Pts',(40.5392751458362,-30.6138395280662,
1010.70055147059));
#152732=CARTESIAN_POINT('Ctrl Pts',(37.7024851496972,-34.3703565790883,
1009.20643382353));
#152733=CARTESIAN_POINT('Ctrl Pts',(34.2237386972451,-37.5416529948095,
1007.71231617647));
#152734=CARTESIAN_POINT('Ctrl Pts',(30.744992244793,-40.7129494105307,1006.21819852941));
#152735=CARTESIAN_POINT('Ctrl Pts',(26.7427538741697,-43.1910304950644,
1004.72408088235));
#152736=CARTESIAN_POINT('Ctrl Pts',(22.7405155035463,-45.6691115795981,
1003.22996323529));
#152737=CARTESIAN_POINT('Ctrl Pts',(18.3510766423074,-47.3695892537413,
1001.73584558824));
#152738=CARTESIAN_POINT('Ctrl Pts',(13.9616377810684,-49.0700669278844,
1000.24172794118));
#152739=CARTESIAN_POINT('Ctrl Pts',(9.33447550508176,-49.9350334639422,
998.747610294118));
#152740=CARTESIAN_POINT('Ctrl Pts',(4.70731322909511,-50.8,997.253492647059));
#152741=CARTESIAN_POINT('Ctrl Pts',(0.,-50.8,995.759375));
#152742=CARTESIAN_POINT('Ctrl Pts',(-4.70731322909511,-50.8,994.265257352941));
#152743=CARTESIAN_POINT('Ctrl Pts',(-9.33447550508177,-49.9350334639422,
992.771139705882));
#152744=CARTESIAN_POINT('Ctrl Pts',(-13.9616377810684,-49.0700669278844,
991.277022058824));
#152745=CARTESIAN_POINT('Ctrl Pts',(-18.3510766423074,-47.3695892537413,
989.782904411765));
#152746=CARTESIAN_POINT('Ctrl Pts',(-22.7405155035463,-45.6691115795981,
988.288786764706));
#152747=CARTESIAN_POINT('Ctrl Pts',(-26.7427538741697,-43.1910304950644,
986.794669117647));
#152748=CARTESIAN_POINT('Ctrl Pts',(-30.744992244793,-40.7129494105307,
985.300551470589));
#152749=CARTESIAN_POINT('Ctrl Pts',(-34.2237386972451,-37.5416529948095,
983.806433823529));
#152750=CARTESIAN_POINT('Ctrl Pts',(-37.7024851496972,-34.3703565790883,
982.312316176471));
#152751=CARTESIAN_POINT('Ctrl Pts',(-40.5392751458362,-30.6138395280662,
980.818198529412));
#152752=CARTESIAN_POINT('Ctrl Pts',(-43.3760651419751,-26.8573224770441,
979.324080882353));
#152753=CARTESIAN_POINT('Ctrl Pts',(-45.4742952008371,-22.6435084734481,
977.829963235294));
#152754=CARTESIAN_POINT('Ctrl Pts',(-47.5725252596992,-18.4296944698521,
976.335845588235));
#152755=CARTESIAN_POINT('Ctrl Pts',(-48.8607426731792,-13.9020798956618,
974.841727941176));
#152756=CARTESIAN_POINT('Ctrl Pts',(-50.1489600866593,-9.37446532147148,
973.347610294118));
#152757=CARTESIAN_POINT('Ctrl Pts',(-50.5832961557877,-4.68723266073574,
971.853492647059));
#152758=CARTESIAN_POINT('Ctrl Pts',(-51.0176322249162,-3.12392900021603E-15,
970.359375));
#152759=CARTESIAN_POINT('Ctrl Pts',(-50.5832961557877,4.68723266073573,
968.865257352941));
#152760=CARTESIAN_POINT('Ctrl Pts',(-50.1489600866593,9.37446532147149,
967.371139705883));
#152761=CARTESIAN_POINT('Ctrl Pts',(-48.8607426731792,13.9020798956618,
965.877022058824));
#152762=CARTESIAN_POINT('Ctrl Pts',(-47.5725252596992,18.4296944698521,
964.382904411765));
#152763=CARTESIAN_POINT('Ctrl Pts',(-45.4742952008371,22.6435084734481,
962.888786764706));
#152764=CARTESIAN_POINT('Ctrl Pts',(-43.3760651419751,26.8573224770442,
961.394669117647));
#152765=CARTESIAN_POINT('Ctrl Pts',(-40.5392751458362,30.6138395280662,
959.900551470588));
#152766=CARTESIAN_POINT('Ctrl Pts',(-37.7024851496972,34.3703565790883,
958.40643382353));
#152767=CARTESIAN_POINT('Ctrl Pts',(-34.2237386972451,37.5416529948095,
956.912316176471));
#152768=CARTESIAN_POINT('Ctrl Pts',(-30.744992244793,40.7129494105307,955.418198529412));
#152769=CARTESIAN_POINT('Ctrl Pts',(-26.7427538741697,43.1910304950644,
953.924080882353));
#152770=CARTESIAN_POINT('Ctrl Pts',(-22.7405155035463,45.6691115795981,
952.429963235294));
#152771=CARTESIAN_POINT('Ctrl Pts',(-18.3510766423074,47.3695892537413,
950.935845588235));
#152772=CARTESIAN_POINT('Ctrl Pts',(-13.9616377810684,49.0700669278844,
949.441727941177));
#152773=CARTESIAN_POINT('Ctrl Pts',(-9.33447550508177,49.9350334639422,
947.947610294118));
#152774=CARTESIAN_POINT('Ctrl Pts',(-4.7073132290951,50.8,946.453492647059));
#152775=CARTESIAN_POINT('Ctrl Pts',(-6.22120573966855E-15,50.8,944.959375));
#152776=CARTESIAN_POINT('Ctrl Pts',(4.70731322909511,50.8,943.465257352941));
#152777=CARTESIAN_POINT('Ctrl Pts',(9.33447550508176,49.9350334639422,941.971139705882));
#152778=CARTESIAN_POINT('Ctrl Pts',(13.9616377810684,49.0700669278844,940.477022058824));
#152779=CARTESIAN_POINT('Ctrl Pts',(18.3510766423074,47.3695892537413,938.982904411765));
#152780=CARTESIAN_POINT('Ctrl Pts',(22.7405155035463,45.6691115795981,937.488786764706));
#152781=CARTESIAN_POINT('Ctrl Pts',(26.7427538741697,43.1910304950644,935.994669117647));
#152782=CARTESIAN_POINT('Ctrl Pts',(30.744992244793,40.7129494105307,934.500551470588));
#152783=CARTESIAN_POINT('Ctrl Pts',(34.2237386972451,37.5416529948095,933.00643382353));
#152784=CARTESIAN_POINT('Ctrl Pts',(37.7024851496972,34.3703565790883,931.512316176471));
#152785=CARTESIAN_POINT('Ctrl Pts',(40.5392751458362,30.6138395280662,930.018198529412));
#152786=CARTESIAN_POINT('Ctrl Pts',(43.3760651419751,26.8573224770442,928.524080882353));
#152787=CARTESIAN_POINT('Ctrl Pts',(45.4742952008372,22.6435084734481,927.029963235294));
#152788=CARTESIAN_POINT('Ctrl Pts',(47.5725252596992,18.4296944698521,925.535845588235));
#152789=CARTESIAN_POINT('Ctrl Pts',(48.8607426731792,13.9020798956618,924.041727941176));
#152790=CARTESIAN_POINT('Ctrl Pts',(50.1489600866593,9.37446532147146,922.547610294118));
#152791=CARTESIAN_POINT('Ctrl Pts',(50.5832961557877,4.68723266073574,921.053492647059));
#152792=CARTESIAN_POINT('Ctrl Pts',(51.0176322249162,9.37178700064808E-15,
919.559375));
#152793=CARTESIAN_POINT('Ctrl Pts',(50.5832961557877,-4.68723266073572,
918.065257352941));
#152794=CARTESIAN_POINT('Ctrl Pts',(50.1489600866593,-9.37446532147149,
916.571139705882));
#152795=CARTESIAN_POINT('Ctrl Pts',(48.8607426731792,-13.9020798956618,
915.077022058824));
#152796=CARTESIAN_POINT('Ctrl Pts',(47.5725252596992,-18.4296944698521,
913.582904411765));
#152797=CARTESIAN_POINT('Ctrl Pts',(45.4742952008371,-22.6435084734482,
912.088786764706));
#152798=CARTESIAN_POINT('Ctrl Pts',(43.3760651419751,-26.8573224770441,
910.594669117647));
#152799=CARTESIAN_POINT('Ctrl Pts',(40.5392751458362,-30.6138395280662,
909.100551470588));
#152800=CARTESIAN_POINT('Ctrl Pts',(37.7024851496972,-34.3703565790883,
907.60643382353));
#152801=CARTESIAN_POINT('Ctrl Pts',(34.2237386972451,-37.5416529948095,
906.112316176471));
#152802=CARTESIAN_POINT('Ctrl Pts',(30.744992244793,-40.7129494105307,904.618198529412));
#152803=CARTESIAN_POINT('Ctrl Pts',(26.7427538741697,-43.1910304950644,
903.124080882353));
#152804=CARTESIAN_POINT('Ctrl Pts',(22.7405155035463,-45.6691115795981,
901.629963235294));
#152805=CARTESIAN_POINT('Ctrl Pts',(18.3510766423074,-47.3695892537413,
900.135845588235));
#152806=CARTESIAN_POINT('Ctrl Pts',(13.9616377810684,-49.0700669278844,
898.641727941177));
#152807=CARTESIAN_POINT('Ctrl Pts',(9.33447550508176,-49.9350334639422,
897.147610294118));
#152808=CARTESIAN_POINT('Ctrl Pts',(4.70731322909511,-50.8,895.653492647059));
#152809=CARTESIAN_POINT('Ctrl Pts',(0.,-50.8,894.159375));
#152810=CARTESIAN_POINT('Ctrl Pts',(-4.70731322909511,-50.8,892.665257352941));
#152811=CARTESIAN_POINT('Ctrl Pts',(-9.33447550508177,-49.9350334639422,
891.171139705882));
#152812=CARTESIAN_POINT('Ctrl Pts',(-13.9616377810684,-49.0700669278844,
889.677022058824));
#152813=CARTESIAN_POINT('Ctrl Pts',(-18.3510766423074,-47.3695892537413,
888.182904411765));
#152814=CARTESIAN_POINT('Ctrl Pts',(-22.7405155035463,-45.6691115795981,
886.688786764706));
#152815=CARTESIAN_POINT('Ctrl Pts',(-26.7427538741697,-43.1910304950644,
885.194669117647));
#152816=CARTESIAN_POINT('Ctrl Pts',(-30.744992244793,-40.7129494105307,
883.700551470588));
#152817=CARTESIAN_POINT('Ctrl Pts',(-34.2237386972451,-37.5416529948095,
882.206433823529));
#152818=CARTESIAN_POINT('Ctrl Pts',(-37.7024851496972,-34.3703565790883,
880.712316176471));
#152819=CARTESIAN_POINT('Ctrl Pts',(-40.5392751458362,-30.6138395280662,
879.218198529412));
#152820=CARTESIAN_POINT('Ctrl Pts',(-43.3760651419751,-26.8573224770441,
877.724080882353));
#152821=CARTESIAN_POINT('Ctrl Pts',(-45.4742952008371,-22.6435084734481,
876.229963235294));
#152822=CARTESIAN_POINT('Ctrl Pts',(-47.5725252596992,-18.4296944698521,
874.735845588236));
#152823=CARTESIAN_POINT('Ctrl Pts',(-48.8607426731792,-13.9020798956618,
873.241727941177));
#152824=CARTESIAN_POINT('Ctrl Pts',(-50.1489600866593,-9.37446532147148,
871.747610294118));
#152825=CARTESIAN_POINT('Ctrl Pts',(-50.5832961557877,-4.68723266073574,
870.253492647059));
#152826=CARTESIAN_POINT('Ctrl Pts',(-51.0176322249162,-3.12392900021603E-15,
868.759375));
#152827=CARTESIAN_POINT('Ctrl Pts',(-50.5832961557877,4.68723266073573,
867.265257352941));
#152828=CARTESIAN_POINT('Ctrl Pts',(-50.1489600866593,9.37446532147149,
865.771139705882));
#152829=CARTESIAN_POINT('Ctrl Pts',(-48.8607426731792,13.9020798956618,
864.277022058824));
#152830=CARTESIAN_POINT('Ctrl Pts',(-47.5725252596992,18.4296944698521,
862.782904411765));
#152831=CARTESIAN_POINT('Ctrl Pts',(-45.4742952008371,22.6435084734481,
861.288786764706));
#152832=CARTESIAN_POINT('Ctrl Pts',(-43.3760651419751,26.8573224770442,
859.794669117647));
#152833=CARTESIAN_POINT('Ctrl Pts',(-40.5392751458362,30.6138395280662,
858.300551470588));
#152834=CARTESIAN_POINT('Ctrl Pts',(-37.7024851496972,34.3703565790883,
856.80643382353));
#152835=CARTESIAN_POINT('Ctrl Pts',(-34.2237386972451,37.5416529948095,
855.312316176471));
#152836=CARTESIAN_POINT('Ctrl Pts',(-30.744992244793,40.7129494105307,853.818198529412));
#152837=CARTESIAN_POINT('Ctrl Pts',(-26.7427538741697,43.1910304950644,
852.324080882353));
#152838=CARTESIAN_POINT('Ctrl Pts',(-22.7405155035463,45.6691115795981,
850.829963235294));
#152839=CARTESIAN_POINT('Ctrl Pts',(-18.3510766423074,47.3695892537413,
849.335845588235));
#152840=CARTESIAN_POINT('Ctrl Pts',(-13.9616377810684,49.0700669278844,
847.841727941177));
#152841=CARTESIAN_POINT('Ctrl Pts',(-9.33447550508177,49.9350334639422,
846.347610294118));
#152842=CARTESIAN_POINT('Ctrl Pts',(-4.7073132290951,50.8,844.853492647059));
#152843=CARTESIAN_POINT('Ctrl Pts',(-6.22120573966855E-15,50.8,843.359375));
#152844=CARTESIAN_POINT('Ctrl Pts',(4.70731322909511,50.8,841.865257352941));
#152845=CARTESIAN_POINT('Ctrl Pts',(9.33447550508176,49.9350334639422,840.371139705882));
#152846=CARTESIAN_POINT('Ctrl Pts',(13.9616377810684,49.0700669278844,838.877022058824));
#152847=CARTESIAN_POINT('Ctrl Pts',(18.3510766423074,47.3695892537413,837.382904411765));
#152848=CARTESIAN_POINT('Ctrl Pts',(22.7405155035463,45.6691115795981,835.888786764706));
#152849=CARTESIAN_POINT('Ctrl Pts',(26.7427538741697,43.1910304950644,834.394669117647));
#152850=CARTESIAN_POINT('Ctrl Pts',(30.744992244793,40.7129494105307,832.900551470589));
#152851=CARTESIAN_POINT('Ctrl Pts',(34.2237386972451,37.5416529948095,831.406433823529));
#152852=CARTESIAN_POINT('Ctrl Pts',(37.7024851496972,34.3703565790883,829.912316176471));
#152853=CARTESIAN_POINT('Ctrl Pts',(40.5392751458362,30.6138395280662,828.418198529412));
#152854=CARTESIAN_POINT('Ctrl Pts',(43.3760651419751,26.8573224770442,826.924080882353));
#152855=CARTESIAN_POINT('Ctrl Pts',(45.4742952008372,22.6435084734481,825.429963235294));
#152856=CARTESIAN_POINT('Ctrl Pts',(47.5725252596992,18.4296944698521,823.935845588235));
#152857=CARTESIAN_POINT('Ctrl Pts',(48.8607426731792,13.9020798956618,822.441727941177));
#152858=CARTESIAN_POINT('Ctrl Pts',(50.1489600866593,9.37446532147146,820.947610294118));
#152859=CARTESIAN_POINT('Ctrl Pts',(50.5832961557877,4.68723266073574,819.453492647059));
#152860=CARTESIAN_POINT('Ctrl Pts',(51.0176322249162,9.37178700064808E-15,
817.959375));
#152861=CARTESIAN_POINT('Ctrl Pts',(50.5832961557877,-4.68723266073572,
816.465257352941));
#152862=CARTESIAN_POINT('Ctrl Pts',(50.1489600866593,-9.37446532147149,
814.971139705883));
#152863=CARTESIAN_POINT('Ctrl Pts',(48.8607426731792,-13.9020798956618,
813.477022058824));
#152864=CARTESIAN_POINT('Ctrl Pts',(47.5725252596992,-18.4296944698521,
811.982904411765));
#152865=CARTESIAN_POINT('Ctrl Pts',(45.4742952008371,-22.6435084734482,
810.488786764706));
#152866=CARTESIAN_POINT('Ctrl Pts',(43.3760651419751,-26.8573224770441,
808.994669117647));
#152867=CARTESIAN_POINT('Ctrl Pts',(40.5392751458362,-30.6138395280662,
807.500551470588));
#152868=CARTESIAN_POINT('Ctrl Pts',(37.7024851496972,-34.3703565790883,
806.00643382353));
#152869=CARTESIAN_POINT('Ctrl Pts',(34.2237386972451,-37.5416529948095,
804.512316176471));
#152870=CARTESIAN_POINT('Ctrl Pts',(30.744992244793,-40.7129494105307,803.018198529412));
#152871=CARTESIAN_POINT('Ctrl Pts',(26.7427538741697,-43.1910304950644,
801.524080882353));
#152872=CARTESIAN_POINT('Ctrl Pts',(22.7405155035463,-45.6691115795981,
800.029963235294));
#152873=CARTESIAN_POINT('Ctrl Pts',(18.3510766423074,-47.3695892537413,
798.535845588235));
#152874=CARTESIAN_POINT('Ctrl Pts',(13.9616377810684,-49.0700669278844,
797.041727941177));
#152875=CARTESIAN_POINT('Ctrl Pts',(9.33447550508176,-49.9350334639422,
795.547610294118));
#152876=CARTESIAN_POINT('Ctrl Pts',(4.70731322909511,-50.8,794.053492647059));
#152877=CARTESIAN_POINT('Ctrl Pts',(0.,-50.8,792.559375));
#152878=CARTESIAN_POINT('Ctrl Pts',(-4.70731322909511,-50.8,791.065257352941));
#152879=CARTESIAN_POINT('Ctrl Pts',(-9.33447550508177,-49.9350334639422,
789.571139705882));
#152880=CARTESIAN_POINT('Ctrl Pts',(-13.9616377810684,-49.0700669278844,
788.077022058824));
#152881=CARTESIAN_POINT('Ctrl Pts',(-18.3510766423074,-47.3695892537413,
786.582904411765));
#152882=CARTESIAN_POINT('Ctrl Pts',(-22.7405155035463,-45.6691115795981,
785.088786764706));
#152883=CARTESIAN_POINT('Ctrl Pts',(-26.7427538741697,-43.1910304950644,
783.594669117647));
#152884=CARTESIAN_POINT('Ctrl Pts',(-30.744992244793,-40.7129494105307,
782.100551470588));
#152885=CARTESIAN_POINT('Ctrl Pts',(-34.2237386972451,-37.5416529948095,
780.60643382353));
#152886=CARTESIAN_POINT('Ctrl Pts',(-37.7024851496972,-34.3703565790883,
779.112316176471));
#152887=CARTESIAN_POINT('Ctrl Pts',(-40.5392751458362,-30.6138395280662,
777.618198529412));
#152888=CARTESIAN_POINT('Ctrl Pts',(-43.3760651419751,-26.8573224770441,
776.124080882353));
#152889=CARTESIAN_POINT('Ctrl Pts',(-45.4742952008371,-22.6435084734481,
774.629963235294));
#152890=CARTESIAN_POINT('Ctrl Pts',(-47.5725252596992,-18.4296944698521,
773.135845588235));
#152891=CARTESIAN_POINT('Ctrl Pts',(-48.8607426731792,-13.9020798956618,
771.641727941176));
#152892=CARTESIAN_POINT('Ctrl Pts',(-50.1489600866593,-9.37446532147148,
770.147610294118));
#152893=CARTESIAN_POINT('Ctrl Pts',(-50.5832961557877,-4.68723266073574,
768.653492647059));
#152894=CARTESIAN_POINT('Ctrl Pts',(-51.0176322249162,-3.12392900021603E-15,
767.159375));
#152895=CARTESIAN_POINT('Ctrl Pts',(-50.5832961557877,4.68723266073573,
765.665257352941));
#152896=CARTESIAN_POINT('Ctrl Pts',(-50.1489600866593,9.37446532147149,
764.171139705882));
#152897=CARTESIAN_POINT('Ctrl Pts',(-48.8607426731792,13.9020798956618,
762.677022058824));
#152898=CARTESIAN_POINT('Ctrl Pts',(-47.5725252596992,18.4296944698521,
761.182904411765));
#152899=CARTESIAN_POINT('Ctrl Pts',(-45.4742952008371,22.6435084734481,
759.688786764706));
#152900=CARTESIAN_POINT('Ctrl Pts',(-43.3760651419751,26.8573224770442,
758.194669117647));
#152901=CARTESIAN_POINT('Ctrl Pts',(-40.5392751458362,30.6138395280662,
756.700551470588));
#152902=CARTESIAN_POINT('Ctrl Pts',(-37.7024851496972,34.3703565790883,
755.206433823529));
#152903=CARTESIAN_POINT('Ctrl Pts',(-34.2237386972451,37.5416529948095,
753.712316176471));
#152904=CARTESIAN_POINT('Ctrl Pts',(-30.744992244793,40.7129494105307,752.218198529412));
#152905=CARTESIAN_POINT('Ctrl Pts',(-26.7427538741697,43.1910304950644,
750.724080882353));
#152906=CARTESIAN_POINT('Ctrl Pts',(-22.7405155035463,45.6691115795981,
749.229963235294));
#152907=CARTESIAN_POINT('Ctrl Pts',(-18.3510766423074,47.3695892537413,
747.735845588235));
#152908=CARTESIAN_POINT('Ctrl Pts',(-13.9616377810684,49.0700669278844,
746.241727941177));
#152909=CARTESIAN_POINT('Ctrl Pts',(-9.33447550508177,49.9350334639422,
744.747610294118));
#152910=CARTESIAN_POINT('Ctrl Pts',(-4.7073132290951,50.8,743.253492647059));
#152911=CARTESIAN_POINT('Ctrl Pts',(-6.22120573966855E-15,50.8,741.759375));
#152912=CARTESIAN_POINT('Ctrl Pts',(4.70731322909511,50.8,740.265257352941));
#152913=CARTESIAN_POINT('Ctrl Pts',(9.33447550508176,49.9350334639422,738.771139705882));
#152914=CARTESIAN_POINT('Ctrl Pts',(13.9616377810684,49.0700669278844,737.277022058824));
#152915=CARTESIAN_POINT('Ctrl Pts',(18.3510766423074,47.3695892537413,735.782904411765));
#152916=CARTESIAN_POINT('Ctrl Pts',(22.7405155035463,45.6691115795981,734.288786764706));
#152917=CARTESIAN_POINT('Ctrl Pts',(26.7427538741697,43.1910304950644,732.794669117647));
#152918=CARTESIAN_POINT('Ctrl Pts',(30.744992244793,40.7129494105307,731.300551470588));
#152919=CARTESIAN_POINT('Ctrl Pts',(34.2237386972451,37.5416529948095,729.806433823529));
#152920=CARTESIAN_POINT('Ctrl Pts',(37.7024851496972,34.3703565790883,728.312316176471));
#152921=CARTESIAN_POINT('Ctrl Pts',(40.5392751458362,30.6138395280662,726.818198529412));
#152922=CARTESIAN_POINT('Ctrl Pts',(43.3760651419751,26.8573224770442,725.324080882353));
#152923=CARTESIAN_POINT('Ctrl Pts',(45.4742952008372,22.6435084734481,723.829963235294));
#152924=CARTESIAN_POINT('Ctrl Pts',(47.5725252596992,18.4296944698521,722.335845588235));
#152925=CARTESIAN_POINT('Ctrl Pts',(48.8607426731792,13.9020798956618,720.841727941176));
#152926=CARTESIAN_POINT('Ctrl Pts',(50.1489600866593,9.37446532147146,719.347610294118));
#152927=CARTESIAN_POINT('Ctrl Pts',(50.5832961557877,4.68723266073574,717.853492647059));
#152928=CARTESIAN_POINT('Ctrl Pts',(51.0176322249162,9.37178700064808E-15,
716.359375));
#152929=CARTESIAN_POINT('Ctrl Pts',(50.5832961557877,-4.68723266073572,
714.865257352941));
#152930=CARTESIAN_POINT('Ctrl Pts',(50.1489600866593,-9.37446532147149,
713.371139705882));
#152931=CARTESIAN_POINT('Ctrl Pts',(48.8607426731792,-13.9020798956618,
711.877022058824));
#152932=CARTESIAN_POINT('Ctrl Pts',(47.5725252596992,-18.4296944698521,
710.382904411765));
#152933=CARTESIAN_POINT('Ctrl Pts',(45.4742952008371,-22.6435084734482,
708.888786764706));
#152934=CARTESIAN_POINT('Ctrl Pts',(43.3760651419751,-26.8573224770441,
707.394669117647));
#152935=CARTESIAN_POINT('Ctrl Pts',(40.5392751458362,-30.6138395280662,
705.900551470588));
#152936=CARTESIAN_POINT('Ctrl Pts',(37.7024851496972,-34.3703565790883,
704.406433823529));
#152937=CARTESIAN_POINT('Ctrl Pts',(34.2237386972451,-37.5416529948095,
702.912316176471));
#152938=CARTESIAN_POINT('Ctrl Pts',(30.744992244793,-40.7129494105307,701.418198529412));
#152939=CARTESIAN_POINT('Ctrl Pts',(26.7427538741697,-43.1910304950644,
699.924080882353));
#152940=CARTESIAN_POINT('Ctrl Pts',(22.7405155035463,-45.6691115795981,
698.429963235294));
#152941=CARTESIAN_POINT('Ctrl Pts',(18.3510766423074,-47.3695892537413,
696.935845588235));
#152942=CARTESIAN_POINT('Ctrl Pts',(13.9616377810684,-49.0700669278844,
695.441727941177));
#152943=CARTESIAN_POINT('Ctrl Pts',(9.33447550508176,-49.9350334639422,
693.947610294118));
#152944=CARTESIAN_POINT('Ctrl Pts',(4.70731322909511,-50.8,692.453492647059));
#152945=CARTESIAN_POINT('Ctrl Pts',(0.,-50.8,690.959375));
#152946=CARTESIAN_POINT('Ctrl Pts',(-4.70731322909511,-50.8,689.465257352941));
#152947=CARTESIAN_POINT('Ctrl Pts',(-9.33447550508177,-49.9350334639422,
687.971139705882));
#152948=CARTESIAN_POINT('Ctrl Pts',(-13.9616377810684,-49.0700669278844,
686.477022058824));
#152949=CARTESIAN_POINT('Ctrl Pts',(-18.3510766423074,-47.3695892537413,
684.982904411765));
#152950=CARTESIAN_POINT('Ctrl Pts',(-22.7405155035463,-45.6691115795981,
683.488786764706));
#152951=CARTESIAN_POINT('Ctrl Pts',(-26.7427538741697,-43.1910304950644,
681.994669117647));
#152952=CARTESIAN_POINT('Ctrl Pts',(-30.744992244793,-40.7129494105307,
680.500551470588));
#152953=CARTESIAN_POINT('Ctrl Pts',(-34.2237386972451,-37.5416529948095,
679.006433823529));
#152954=CARTESIAN_POINT('Ctrl Pts',(-37.7024851496972,-34.3703565790883,
677.512316176471));
#152955=CARTESIAN_POINT('Ctrl Pts',(-40.5392751458362,-30.6138395280662,
676.018198529412));
#152956=CARTESIAN_POINT('Ctrl Pts',(-43.3760651419751,-26.8573224770441,
674.524080882353));
#152957=CARTESIAN_POINT('Ctrl Pts',(-45.4742952008371,-22.6435084734481,
673.029963235294));
#152958=CARTESIAN_POINT('Ctrl Pts',(-47.5725252596992,-18.4296944698521,
671.535845588235));
#152959=CARTESIAN_POINT('Ctrl Pts',(-48.8607426731792,-13.9020798956618,
670.041727941177));
#152960=CARTESIAN_POINT('Ctrl Pts',(-50.1489600866593,-9.37446532147148,
668.547610294118));
#152961=CARTESIAN_POINT('Ctrl Pts',(-50.5832961557877,-4.68723266073574,
667.053492647059));
#152962=CARTESIAN_POINT('Ctrl Pts',(-51.0176322249162,-3.12392900021603E-15,
665.559375));
#152963=CARTESIAN_POINT('Ctrl Pts',(-50.5832961557877,4.68723266073573,
664.065257352941));
#152964=CARTESIAN_POINT('Ctrl Pts',(-50.1489600866593,9.37446532147149,
662.571139705882));
#152965=CARTESIAN_POINT('Ctrl Pts',(-48.8607426731792,13.9020798956618,
661.077022058824));
#152966=CARTESIAN_POINT('Ctrl Pts',(-47.5725252596992,18.4296944698521,
659.582904411765));
#152967=CARTESIAN_POINT('Ctrl Pts',(-45.4742952008371,22.6435084734481,
658.088786764706));
#152968=CARTESIAN_POINT('Ctrl Pts',(-43.3760651419751,26.8573224770442,
656.594669117647));
#152969=CARTESIAN_POINT('Ctrl Pts',(-40.5392751458362,30.6138395280662,
655.100551470588));
#152970=CARTESIAN_POINT('Ctrl Pts',(-37.7024851496972,34.3703565790883,
653.606433823529));
#152971=CARTESIAN_POINT('Ctrl Pts',(-34.2237386972451,37.5416529948095,
652.112316176471));
#152972=CARTESIAN_POINT('Ctrl Pts',(-30.744992244793,40.7129494105307,650.618198529412));
#152973=CARTESIAN_POINT('Ctrl Pts',(-26.7427538741697,43.1910304950644,
649.124080882353));
#152974=CARTESIAN_POINT('Ctrl Pts',(-22.7405155035463,45.6691115795981,
647.629963235294));
#152975=CARTESIAN_POINT('Ctrl Pts',(-18.3510766423074,47.3695892537413,
646.135845588235));
#152976=CARTESIAN_POINT('Ctrl Pts',(-13.9616377810684,49.0700669278844,
644.641727941176));
#152977=CARTESIAN_POINT('Ctrl Pts',(-9.33447550508177,49.9350334639422,
643.147610294118));
#152978=CARTESIAN_POINT('Ctrl Pts',(-4.7073132290951,50.8,641.653492647059));
#152979=CARTESIAN_POINT('Ctrl Pts',(-6.22120573966855E-15,50.8,640.159375));
#152980=CARTESIAN_POINT('Ctrl Pts',(4.70731322909511,50.8,638.665257352941));
#152981=CARTESIAN_POINT('Ctrl Pts',(9.33447550508176,49.9350334639422,637.171139705882));
#152982=CARTESIAN_POINT('Ctrl Pts',(13.9616377810684,49.0700669278844,635.677022058824));
#152983=CARTESIAN_POINT('Ctrl Pts',(18.3510766423074,47.3695892537413,634.182904411765));
#152984=CARTESIAN_POINT('Ctrl Pts',(22.7405155035463,45.6691115795981,632.688786764706));
#152985=CARTESIAN_POINT('Ctrl Pts',(26.7427538741697,43.1910304950644,631.194669117647));
#152986=CARTESIAN_POINT('Ctrl Pts',(30.744992244793,40.7129494105307,629.700551470588));
#152987=CARTESIAN_POINT('Ctrl Pts',(34.2237386972451,37.5416529948095,628.206433823529));
#152988=CARTESIAN_POINT('Ctrl Pts',(37.7024851496972,34.3703565790883,626.712316176471));
#152989=CARTESIAN_POINT('Ctrl Pts',(40.5392751458362,30.6138395280662,625.218198529412));
#152990=CARTESIAN_POINT('Ctrl Pts',(43.3760651419751,26.8573224770442,623.724080882353));
#152991=CARTESIAN_POINT('Ctrl Pts',(45.4742952008372,22.6435084734481,622.229963235294));
#152992=CARTESIAN_POINT('Ctrl Pts',(47.5725252596992,18.4296944698521,620.735845588235));
#152993=CARTESIAN_POINT('Ctrl Pts',(48.8607426731792,13.9020798956618,619.241727941177));
#152994=CARTESIAN_POINT('Ctrl Pts',(50.1489600866593,9.37446532147146,617.747610294118));
#152995=CARTESIAN_POINT('Ctrl Pts',(50.5832961557877,4.68723266073574,616.253492647059));
#152996=CARTESIAN_POINT('Ctrl Pts',(51.0176322249162,9.37178700064808E-15,
614.759375));
#152997=CARTESIAN_POINT('Ctrl Pts',(50.5832961557877,-4.68723266073572,
613.265257352941));
#152998=CARTESIAN_POINT('Ctrl Pts',(50.1489600866593,-9.37446532147149,
611.771139705882));
#152999=CARTESIAN_POINT('Ctrl Pts',(48.8607426731792,-13.9020798956618,
610.277022058823));
#153000=CARTESIAN_POINT('Ctrl Pts',(47.5725252596992,-18.4296944698521,
608.782904411765));
#153001=CARTESIAN_POINT('Ctrl Pts',(45.4742952008371,-22.6435084734482,
607.288786764706));
#153002=CARTESIAN_POINT('Ctrl Pts',(43.3760651419751,-26.8573224770441,
605.794669117647));
#153003=CARTESIAN_POINT('Ctrl Pts',(40.5392751458362,-30.6138395280662,
604.300551470588));
#153004=CARTESIAN_POINT('Ctrl Pts',(37.7024851496972,-34.3703565790883,
602.806433823529));
#153005=CARTESIAN_POINT('Ctrl Pts',(34.2237386972451,-37.5416529948095,
601.312316176471));
#153006=CARTESIAN_POINT('Ctrl Pts',(30.744992244793,-40.7129494105307,599.818198529412));
#153007=CARTESIAN_POINT('Ctrl Pts',(26.7427538741697,-43.1910304950644,
598.324080882353));
#153008=CARTESIAN_POINT('Ctrl Pts',(22.7405155035463,-45.6691115795981,
596.829963235294));
#153009=CARTESIAN_POINT('Ctrl Pts',(18.3510766423074,-47.3695892537413,
595.335845588235));
#153010=CARTESIAN_POINT('Ctrl Pts',(13.9616377810684,-49.0700669278844,
593.841727941176));
#153011=CARTESIAN_POINT('Ctrl Pts',(9.33447550508176,-49.9350334639422,
592.347610294118));
#153012=CARTESIAN_POINT('Ctrl Pts',(4.70731322909511,-50.8,590.853492647059));
#153013=CARTESIAN_POINT('Ctrl Pts',(0.,-50.8,589.359375));
#153014=CARTESIAN_POINT('Ctrl Pts',(-4.70731322909511,-50.8,587.865257352941));
#153015=CARTESIAN_POINT('Ctrl Pts',(-9.33447550508177,-49.9350334639422,
586.371139705882));
#153016=CARTESIAN_POINT('Ctrl Pts',(-13.9616377810684,-49.0700669278844,
584.877022058824));
#153017=CARTESIAN_POINT('Ctrl Pts',(-18.3510766423074,-47.3695892537413,
583.382904411765));
#153018=CARTESIAN_POINT('Ctrl Pts',(-22.7405155035463,-45.6691115795981,
581.888786764706));
#153019=CARTESIAN_POINT('Ctrl Pts',(-26.7427538741697,-43.1910304950644,
580.394669117647));
#153020=CARTESIAN_POINT('Ctrl Pts',(-30.744992244793,-40.7129494105307,
578.900551470588));
#153021=CARTESIAN_POINT('Ctrl Pts',(-34.2237386972451,-37.5416529948095,
577.406433823529));
#153022=CARTESIAN_POINT('Ctrl Pts',(-37.7024851496972,-34.3703565790883,
575.912316176471));
#153023=CARTESIAN_POINT('Ctrl Pts',(-40.5392751458362,-30.6138395280662,
574.418198529412));
#153024=CARTESIAN_POINT('Ctrl Pts',(-43.3760651419751,-26.8573224770441,
572.924080882353));
#153025=CARTESIAN_POINT('Ctrl Pts',(-45.4742952008371,-22.6435084734481,
571.429963235294));
#153026=CARTESIAN_POINT('Ctrl Pts',(-47.5725252596992,-18.4296944698521,
569.935845588235));
#153027=CARTESIAN_POINT('Ctrl Pts',(-48.8607426731792,-13.9020798956618,
568.441727941177));
#153028=CARTESIAN_POINT('Ctrl Pts',(-50.1489600866593,-9.37446532147148,
566.947610294118));
#153029=CARTESIAN_POINT('Ctrl Pts',(-50.5832961557877,-4.68723266073574,
565.453492647059));
#153030=CARTESIAN_POINT('Ctrl Pts',(-51.0176322249162,-3.12392900021603E-15,
563.959375));
#153031=CARTESIAN_POINT('Ctrl Pts',(-50.5832961557877,4.68723266073573,
562.465257352941));
#153032=CARTESIAN_POINT('Ctrl Pts',(-50.1489600866593,9.37446532147149,
560.971139705882));
#153033=CARTESIAN_POINT('Ctrl Pts',(-48.8607426731792,13.9020798956618,
559.477022058824));
#153034=CARTESIAN_POINT('Ctrl Pts',(-47.5725252596992,18.4296944698521,
557.982904411765));
#153035=CARTESIAN_POINT('Ctrl Pts',(-45.4742952008371,22.6435084734481,
556.488786764706));
#153036=CARTESIAN_POINT('Ctrl Pts',(-43.3760651419751,26.8573224770442,
554.994669117647));
#153037=CARTESIAN_POINT('Ctrl Pts',(-40.5392751458362,30.6138395280662,
553.500551470588));
#153038=CARTESIAN_POINT('Ctrl Pts',(-37.7024851496972,34.3703565790883,
552.00643382353));
#153039=CARTESIAN_POINT('Ctrl Pts',(-34.2237386972451,37.5416529948095,
550.512316176471));
#153040=CARTESIAN_POINT('Ctrl Pts',(-30.744992244793,40.7129494105307,549.018198529412));
#153041=CARTESIAN_POINT('Ctrl Pts',(-26.7427538741697,43.1910304950644,
547.524080882353));
#153042=CARTESIAN_POINT('Ctrl Pts',(-22.7405155035463,45.6691115795981,
546.029963235294));
#153043=CARTESIAN_POINT('Ctrl Pts',(-18.3510766423074,47.3695892537413,
544.535845588235));
#153044=CARTESIAN_POINT('Ctrl Pts',(-13.9616377810684,49.0700669278844,
543.041727941176));
#153045=CARTESIAN_POINT('Ctrl Pts',(-9.33447550508177,49.9350334639422,
541.547610294118));
#153046=CARTESIAN_POINT('Ctrl Pts',(-4.7073132290951,50.8,540.053492647059));
#153047=CARTESIAN_POINT('Ctrl Pts',(-6.22120573966855E-15,50.8,538.559375));
#153048=CARTESIAN_POINT('Ctrl Pts',(4.70731322909511,50.8,537.065257352941));
#153049=CARTESIAN_POINT('Ctrl Pts',(9.33447550508176,49.9350334639422,535.571139705882));
#153050=CARTESIAN_POINT('Ctrl Pts',(13.9616377810684,49.0700669278844,534.077022058824));
#153051=CARTESIAN_POINT('Ctrl Pts',(18.3510766423074,47.3695892537413,532.582904411765));
#153052=CARTESIAN_POINT('Ctrl Pts',(22.7405155035463,45.6691115795981,531.088786764706));
#153053=CARTESIAN_POINT('Ctrl Pts',(26.7427538741697,43.1910304950644,529.594669117647));
#153054=CARTESIAN_POINT('Ctrl Pts',(30.744992244793,40.7129494105307,528.100551470588));
#153055=CARTESIAN_POINT('Ctrl Pts',(34.2237386972451,37.5416529948095,526.606433823529));
#153056=CARTESIAN_POINT('Ctrl Pts',(37.7024851496972,34.3703565790883,525.112316176471));
#153057=CARTESIAN_POINT('Ctrl Pts',(40.5392751458362,30.6138395280662,523.618198529412));
#153058=CARTESIAN_POINT('Ctrl Pts',(43.3760651419751,26.8573224770442,522.124080882353));
#153059=CARTESIAN_POINT('Ctrl Pts',(45.4742952008372,22.6435084734481,520.629963235294));
#153060=CARTESIAN_POINT('Ctrl Pts',(47.5725252596992,18.4296944698521,519.135845588235));
#153061=CARTESIAN_POINT('Ctrl Pts',(48.8607426731792,13.9020798956618,517.641727941176));
#153062=CARTESIAN_POINT('Ctrl Pts',(50.1489600866593,9.37446532147146,516.147610294118));
#153063=CARTESIAN_POINT('Ctrl Pts',(50.5832961557877,4.68723266073574,514.653492647059));
#153064=CARTESIAN_POINT('Ctrl Pts',(51.0176322249162,9.37178700064808E-15,
513.159375));
#153065=CARTESIAN_POINT('Ctrl Pts',(50.5832961557877,-4.68723266073572,
511.665257352941));
#153066=CARTESIAN_POINT('Ctrl Pts',(50.1489600866593,-9.37446532147149,
510.171139705882));
#153067=CARTESIAN_POINT('Ctrl Pts',(48.8607426731792,-13.9020798956618,
508.677022058824));
#153068=CARTESIAN_POINT('Ctrl Pts',(47.5725252596992,-18.4296944698521,
507.182904411765));
#153069=CARTESIAN_POINT('Ctrl Pts',(45.4742952008371,-22.6435084734482,
505.688786764706));
#153070=CARTESIAN_POINT('Ctrl Pts',(43.3760651419751,-26.8573224770441,
504.194669117647));
#153071=CARTESIAN_POINT('Ctrl Pts',(40.5392751458362,-30.6138395280662,
502.700551470588));
#153072=CARTESIAN_POINT('Ctrl Pts',(37.7024851496972,-34.3703565790883,
501.206433823529));
#153073=CARTESIAN_POINT('Ctrl Pts',(34.2237386972451,-37.5416529948095,
499.712316176471));
#153074=CARTESIAN_POINT('Ctrl Pts',(30.744992244793,-40.7129494105307,498.218198529412));
#153075=CARTESIAN_POINT('Ctrl Pts',(26.7427538741697,-43.1910304950644,
496.724080882353));
#153076=CARTESIAN_POINT('Ctrl Pts',(22.7405155035463,-45.6691115795981,
495.229963235294));
#153077=CARTESIAN_POINT('Ctrl Pts',(18.3510766423074,-47.3695892537413,
493.735845588235));
#153078=CARTESIAN_POINT('Ctrl Pts',(13.9616377810684,-49.0700669278844,
492.241727941177));
#153079=CARTESIAN_POINT('Ctrl Pts',(9.33447550508176,-49.9350334639422,
490.747610294118));
#153080=CARTESIAN_POINT('Ctrl Pts',(4.70731322909511,-50.8,489.253492647059));
#153081=CARTESIAN_POINT('Ctrl Pts',(0.,-50.8,487.759375));
#153082=CARTESIAN_POINT('Ctrl Pts',(-4.70731322909511,-50.8,486.265257352941));
#153083=CARTESIAN_POINT('Ctrl Pts',(-9.33447550508177,-49.9350334639422,
484.771139705882));
#153084=CARTESIAN_POINT('Ctrl Pts',(-13.9616377810684,-49.0700669278844,
483.277022058824));
#153085=CARTESIAN_POINT('Ctrl Pts',(-18.3510766423074,-47.3695892537413,
481.782904411765));
#153086=CARTESIAN_POINT('Ctrl Pts',(-22.7405155035463,-45.6691115795981,
480.288786764706));
#153087=CARTESIAN_POINT('Ctrl Pts',(-26.7427538741697,-43.1910304950644,
478.794669117647));
#153088=CARTESIAN_POINT('Ctrl Pts',(-30.744992244793,-40.7129494105307,
477.300551470589));
#153089=CARTESIAN_POINT('Ctrl Pts',(-34.2237386972451,-37.5416529948095,
475.80643382353));
#153090=CARTESIAN_POINT('Ctrl Pts',(-37.7024851496972,-34.3703565790883,
474.312316176471));
#153091=CARTESIAN_POINT('Ctrl Pts',(-40.5392751458362,-30.6138395280662,
472.818198529412));
#153092=CARTESIAN_POINT('Ctrl Pts',(-43.3760651419751,-26.8573224770441,
471.324080882353));
#153093=CARTESIAN_POINT('Ctrl Pts',(-45.4742952008371,-22.6435084734481,
469.829963235294));
#153094=CARTESIAN_POINT('Ctrl Pts',(-47.5725252596992,-18.4296944698521,
468.335845588235));
#153095=CARTESIAN_POINT('Ctrl Pts',(-48.8607426731792,-13.9020798956618,
466.841727941176));
#153096=CARTESIAN_POINT('Ctrl Pts',(-50.1489600866593,-9.37446532147148,
465.347610294118));
#153097=CARTESIAN_POINT('Ctrl Pts',(-50.5832961557877,-4.68723266073574,
463.853492647059));
#153098=CARTESIAN_POINT('Ctrl Pts',(-51.0176322249162,-3.12392900021603E-15,
462.359375));
#153099=CARTESIAN_POINT('Ctrl Pts',(-50.5832961557877,4.68723266073573,
460.865257352941));
#153100=CARTESIAN_POINT('Ctrl Pts',(-50.1489600866593,9.37446532147149,
459.371139705883));
#153101=CARTESIAN_POINT('Ctrl Pts',(-48.8607426731792,13.9020798956618,
457.877022058824));
#153102=CARTESIAN_POINT('Ctrl Pts',(-47.5725252596992,18.4296944698521,
456.382904411765));
#153103=CARTESIAN_POINT('Ctrl Pts',(-45.4742952008371,22.6435084734481,
454.888786764706));
#153104=CARTESIAN_POINT('Ctrl Pts',(-43.3760651419751,26.8573224770442,
453.394669117647));
#153105=CARTESIAN_POINT('Ctrl Pts',(-40.5392751458362,30.6138395280662,
451.900551470588));
#153106=CARTESIAN_POINT('Ctrl Pts',(-37.7024851496972,34.3703565790883,
450.406433823529));
#153107=CARTESIAN_POINT('Ctrl Pts',(-34.2237386972451,37.5416529948095,
448.912316176471));
#153108=CARTESIAN_POINT('Ctrl Pts',(-30.744992244793,40.7129494105307,447.418198529412));
#153109=CARTESIAN_POINT('Ctrl Pts',(-26.7427538741697,43.1910304950644,
445.924080882353));
#153110=CARTESIAN_POINT('Ctrl Pts',(-22.7405155035463,45.6691115795981,
444.429963235294));
#153111=CARTESIAN_POINT('Ctrl Pts',(-18.3510766423074,47.3695892537413,
442.935845588235));
#153112=CARTESIAN_POINT('Ctrl Pts',(-13.9616377810684,49.0700669278844,
441.441727941177));
#153113=CARTESIAN_POINT('Ctrl Pts',(-9.33447550508177,49.9350334639422,
439.947610294118));
#153114=CARTESIAN_POINT('Ctrl Pts',(-4.7073132290951,50.8,438.453492647059));
#153115=CARTESIAN_POINT('Ctrl Pts',(-6.22120573966855E-15,50.8,436.959375));
#153116=CARTESIAN_POINT('Ctrl Pts',(4.70731322909511,50.8,435.465257352941));
#153117=CARTESIAN_POINT('Ctrl Pts',(9.33447550508176,49.9350334639422,433.971139705882));
#153118=CARTESIAN_POINT('Ctrl Pts',(13.9616377810684,49.0700669278844,432.477022058824));
#153119=CARTESIAN_POINT('Ctrl Pts',(18.3510766423074,47.3695892537413,430.982904411765));
#153120=CARTESIAN_POINT('Ctrl Pts',(22.7405155035463,45.6691115795981,429.488786764706));
#153121=CARTESIAN_POINT('Ctrl Pts',(26.7427538741697,43.1910304950644,427.994669117647));
#153122=CARTESIAN_POINT('Ctrl Pts',(30.744992244793,40.7129494105307,426.500551470588));
#153123=CARTESIAN_POINT('Ctrl Pts',(34.2237386972451,37.5416529948095,425.00643382353));
#153124=CARTESIAN_POINT('Ctrl Pts',(37.7024851496972,34.3703565790883,423.512316176471));
#153125=CARTESIAN_POINT('Ctrl Pts',(40.5392751458362,30.6138395280662,422.018198529412));
#153126=CARTESIAN_POINT('Ctrl Pts',(43.3760651419751,26.8573224770442,420.524080882353));
#153127=CARTESIAN_POINT('Ctrl Pts',(45.4742952008372,22.6435084734481,419.029963235294));
#153128=CARTESIAN_POINT('Ctrl Pts',(47.5725252596992,18.4296944698521,417.535845588235));
#153129=CARTESIAN_POINT('Ctrl Pts',(48.8607426731792,13.9020798956618,416.041727941177));
#153130=CARTESIAN_POINT('Ctrl Pts',(50.1489600866593,9.37446532147146,414.547610294118));
#153131=CARTESIAN_POINT('Ctrl Pts',(50.5832961557877,4.68723266073574,413.053492647059));
#153132=CARTESIAN_POINT('Ctrl Pts',(51.0176322249162,9.37178700064808E-15,
411.559375));
#153133=CARTESIAN_POINT('Ctrl Pts',(50.5832961557877,-4.68723266073572,
410.065257352941));
#153134=CARTESIAN_POINT('Ctrl Pts',(50.1489600866593,-9.37446532147149,
408.571139705882));
#153135=CARTESIAN_POINT('Ctrl Pts',(48.8607426731792,-13.9020798956618,
407.077022058824));
#153136=CARTESIAN_POINT('Ctrl Pts',(47.5725252596992,-18.4296944698521,
405.582904411765));
#153137=CARTESIAN_POINT('Ctrl Pts',(45.4742952008371,-22.6435084734482,
404.088786764706));
#153138=CARTESIAN_POINT('Ctrl Pts',(43.3760651419751,-26.8573224770441,
402.594669117647));
#153139=CARTESIAN_POINT('Ctrl Pts',(40.5392751458362,-30.6138395280662,
401.100551470588));
#153140=CARTESIAN_POINT('Ctrl Pts',(37.7024851496972,-34.3703565790883,
399.60643382353));
#153141=CARTESIAN_POINT('Ctrl Pts',(34.2237386972451,-37.5416529948095,
398.112316176471));
#153142=CARTESIAN_POINT('Ctrl Pts',(30.744992244793,-40.7129494105307,396.618198529412));
#153143=CARTESIAN_POINT('Ctrl Pts',(26.7427538741697,-43.1910304950644,
395.124080882353));
#153144=CARTESIAN_POINT('Ctrl Pts',(22.7405155035463,-45.6691115795981,
393.629963235294));
#153145=CARTESIAN_POINT('Ctrl Pts',(18.3510766423074,-47.3695892537413,
392.135845588235));
#153146=CARTESIAN_POINT('Ctrl Pts',(13.9616377810684,-49.0700669278844,
390.641727941176));
#153147=CARTESIAN_POINT('Ctrl Pts',(9.33447550508176,-49.9350334639422,
389.147610294118));
#153148=CARTESIAN_POINT('Ctrl Pts',(4.70731322909511,-50.8,387.653492647059));
#153149=CARTESIAN_POINT('Ctrl Pts',(0.,-50.8,386.159375));
#153150=CARTESIAN_POINT('Ctrl Pts',(-4.70731322909511,-50.8,384.665257352941));
#153151=CARTESIAN_POINT('Ctrl Pts',(-9.33447550508177,-49.9350334639422,
383.171139705882));
#153152=CARTESIAN_POINT('Ctrl Pts',(-13.9616377810684,-49.0700669278844,
381.677022058824));
#153153=CARTESIAN_POINT('Ctrl Pts',(-18.3510766423074,-47.3695892537413,
380.182904411765));
#153154=CARTESIAN_POINT('Ctrl Pts',(-22.7405155035463,-45.6691115795981,
378.688786764706));
#153155=CARTESIAN_POINT('Ctrl Pts',(-26.7427538741697,-43.1910304950644,
377.194669117647));
#153156=CARTESIAN_POINT('Ctrl Pts',(-30.744992244793,-40.7129494105307,
375.700551470588));
#153157=CARTESIAN_POINT('Ctrl Pts',(-34.2237386972451,-37.5416529948095,
374.206433823529));
#153158=CARTESIAN_POINT('Ctrl Pts',(-37.7024851496972,-34.3703565790883,
372.712316176471));
#153159=CARTESIAN_POINT('Ctrl Pts',(-40.5392751458362,-30.6138395280662,
371.218198529412));
#153160=CARTESIAN_POINT('Ctrl Pts',(-43.3760651419751,-26.8573224770441,
369.724080882353));
#153161=CARTESIAN_POINT('Ctrl Pts',(-45.4742952008371,-22.6435084734481,
368.229963235294));
#153162=CARTESIAN_POINT('Ctrl Pts',(-47.5725252596992,-18.4296944698521,
366.735845588235));
#153163=CARTESIAN_POINT('Ctrl Pts',(-48.8607426731792,-13.9020798956618,
365.241727941177));
#153164=CARTESIAN_POINT('Ctrl Pts',(-50.1489600866593,-9.37446532147148,
363.747610294118));
#153165=CARTESIAN_POINT('Ctrl Pts',(-50.5832961557877,-4.68723266073574,
362.253492647059));
#153166=CARTESIAN_POINT('Ctrl Pts',(-51.0176322249162,-3.12392900021603E-15,
360.759375));
#153167=CARTESIAN_POINT('Ctrl Pts',(-50.5832961557877,4.68723266073573,
359.265257352941));
#153168=CARTESIAN_POINT('Ctrl Pts',(-50.1489600866593,9.37446532147149,
357.771139705883));
#153169=CARTESIAN_POINT('Ctrl Pts',(-48.8607426731792,13.9020798956618,
356.277022058824));
#153170=CARTESIAN_POINT('Ctrl Pts',(-47.5725252596992,18.4296944698521,
354.782904411765));
#153171=CARTESIAN_POINT('Ctrl Pts',(-45.4742952008371,22.6435084734481,
353.288786764706));
#153172=CARTESIAN_POINT('Ctrl Pts',(-43.3760651419751,26.8573224770442,
351.794669117647));
#153173=CARTESIAN_POINT('Ctrl Pts',(-40.5392751458362,30.6138395280662,
350.300551470588));
#153174=CARTESIAN_POINT('Ctrl Pts',(-37.7024851496972,34.3703565790883,
348.80643382353));
#153175=CARTESIAN_POINT('Ctrl Pts',(-34.2237386972451,37.5416529948095,
347.312316176471));
#153176=CARTESIAN_POINT('Ctrl Pts',(-30.744992244793,40.7129494105307,345.818198529412));
#153177=CARTESIAN_POINT('Ctrl Pts',(-26.7427538741697,43.1910304950644,
344.324080882353));
#153178=CARTESIAN_POINT('Ctrl Pts',(-22.7405155035463,45.6691115795981,
342.829963235294));
#153179=CARTESIAN_POINT('Ctrl Pts',(-18.3510766423074,47.3695892537413,
341.335845588235));
#153180=CARTESIAN_POINT('Ctrl Pts',(-13.9616377810684,49.0700669278844,
339.841727941176));
#153181=CARTESIAN_POINT('Ctrl Pts',(-9.33447550508177,49.9350334639422,
338.347610294118));
#153182=CARTESIAN_POINT('Ctrl Pts',(-4.7073132290951,50.8,336.853492647059));
#153183=CARTESIAN_POINT('Ctrl Pts',(-6.22120573966855E-15,50.8,335.359375));
#153184=CARTESIAN_POINT('Ctrl Pts',(4.70731322909511,50.8,333.865257352941));
#153185=CARTESIAN_POINT('Ctrl Pts',(9.33447550508176,49.9350334639422,332.371139705882));
#153186=CARTESIAN_POINT('Ctrl Pts',(13.9616377810684,49.0700669278844,330.877022058824));
#153187=CARTESIAN_POINT('Ctrl Pts',(18.3510766423074,47.3695892537413,329.382904411765));
#153188=CARTESIAN_POINT('Ctrl Pts',(22.7405155035463,45.6691115795981,327.888786764706));
#153189=CARTESIAN_POINT('Ctrl Pts',(26.7427538741697,43.1910304950644,326.394669117647));
#153190=CARTESIAN_POINT('Ctrl Pts',(30.744992244793,40.7129494105307,324.900551470588));
#153191=CARTESIAN_POINT('Ctrl Pts',(34.2237386972451,37.5416529948095,323.406433823529));
#153192=CARTESIAN_POINT('Ctrl Pts',(37.7024851496972,34.3703565790883,321.912316176471));
#153193=CARTESIAN_POINT('Ctrl Pts',(40.5392751458362,30.6138395280662,320.418198529412));
#153194=CARTESIAN_POINT('Ctrl Pts',(43.3760651419751,26.8573224770442,318.924080882353));
#153195=CARTESIAN_POINT('Ctrl Pts',(45.4742952008372,22.6435084734481,317.429963235294));
#153196=CARTESIAN_POINT('Ctrl Pts',(47.5725252596992,18.4296944698521,315.935845588235));
#153197=CARTESIAN_POINT('Ctrl Pts',(48.8607426731792,13.9020798956618,314.441727941176));
#153198=CARTESIAN_POINT('Ctrl Pts',(50.1489600866593,9.37446532147146,312.947610294118));
#153199=CARTESIAN_POINT('Ctrl Pts',(50.5832961557877,4.68723266073574,311.453492647059));
#153200=CARTESIAN_POINT('Ctrl Pts',(51.0176322249162,9.37178700064808E-15,
309.959375));
#153201=CARTESIAN_POINT('Ctrl Pts',(50.5832961557877,-4.68723266073572,
308.465257352941));
#153202=CARTESIAN_POINT('Ctrl Pts',(50.1489600866593,-9.37446532147149,
306.971139705882));
#153203=CARTESIAN_POINT('Ctrl Pts',(48.8607426731792,-13.9020798956618,
305.477022058824));
#153204=CARTESIAN_POINT('Ctrl Pts',(47.5725252596992,-18.4296944698521,
303.982904411765));
#153205=CARTESIAN_POINT('Ctrl Pts',(45.4742952008371,-22.6435084734482,
302.488786764706));
#153206=CARTESIAN_POINT('Ctrl Pts',(43.3760651419751,-26.8573224770441,
300.994669117647));
#153207=CARTESIAN_POINT('Ctrl Pts',(40.5392751458362,-30.6138395280662,
299.500551470588));
#153208=CARTESIAN_POINT('Ctrl Pts',(37.7024851496972,-34.3703565790883,
298.00643382353));
#153209=CARTESIAN_POINT('Ctrl Pts',(34.2237386972451,-37.5416529948095,
296.512316176471));
#153210=CARTESIAN_POINT('Ctrl Pts',(30.744992244793,-40.7129494105307,295.018198529412));
#153211=CARTESIAN_POINT('Ctrl Pts',(26.7427538741697,-43.1910304950644,
293.524080882353));
#153212=CARTESIAN_POINT('Ctrl Pts',(22.7405155035463,-45.6691115795981,
292.029963235294));
#153213=CARTESIAN_POINT('Ctrl Pts',(18.3510766423074,-47.3695892537413,
290.535845588235));
#153214=CARTESIAN_POINT('Ctrl Pts',(13.9616377810684,-49.0700669278844,
289.041727941177));
#153215=CARTESIAN_POINT('Ctrl Pts',(9.33447550508176,-49.9350334639422,
287.547610294118));
#153216=CARTESIAN_POINT('Ctrl Pts',(4.70731322909511,-50.8,286.053492647059));
#153217=CARTESIAN_POINT('Ctrl Pts',(0.,-50.8,284.559375));
#153218=CARTESIAN_POINT('Ctrl Pts',(-4.70731322909511,-50.8,283.065257352941));
#153219=CARTESIAN_POINT('Ctrl Pts',(-9.33447550508177,-49.9350334639422,
281.571139705882));
#153220=CARTESIAN_POINT('Ctrl Pts',(-13.9616377810684,-49.0700669278844,
280.077022058824));
#153221=CARTESIAN_POINT('Ctrl Pts',(-18.3510766423074,-47.3695892537413,
278.582904411765));
#153222=CARTESIAN_POINT('Ctrl Pts',(-22.7405155035463,-45.6691115795981,
277.088786764706));
#153223=CARTESIAN_POINT('Ctrl Pts',(-26.7427538741697,-43.1910304950644,
275.594669117647));
#153224=CARTESIAN_POINT('Ctrl Pts',(-30.744992244793,-40.7129494105307,
274.100551470588));
#153225=CARTESIAN_POINT('Ctrl Pts',(-34.2237386972451,-37.5416529948095,
272.606433823529));
#153226=CARTESIAN_POINT('Ctrl Pts',(-37.7024851496972,-34.3703565790883,
271.112316176471));
#153227=CARTESIAN_POINT('Ctrl Pts',(-40.5392751458362,-30.6138395280662,
269.618198529412));
#153228=CARTESIAN_POINT('Ctrl Pts',(-43.3760651419751,-26.8573224770441,
268.124080882353));
#153229=CARTESIAN_POINT('Ctrl Pts',(-45.4742952008371,-22.6435084734481,
266.629963235294));
#153230=CARTESIAN_POINT('Ctrl Pts',(-47.5725252596992,-18.4296944698521,
265.135845588235));
#153231=CARTESIAN_POINT('Ctrl Pts',(-48.8607426731792,-13.9020798956618,
263.641727941176));
#153232=CARTESIAN_POINT('Ctrl Pts',(-50.1489600866593,-9.37446532147148,
262.147610294118));
#153233=CARTESIAN_POINT('Ctrl Pts',(-50.5832961557877,-4.68723266073574,
260.653492647059));
#153234=CARTESIAN_POINT('Ctrl Pts',(-51.0176322249162,-3.12392900021603E-15,
259.159375));
#153235=CARTESIAN_POINT('Ctrl Pts',(-50.5832961557877,4.68723266073573,
257.665257352941));
#153236=CARTESIAN_POINT('Ctrl Pts',(-50.1489600866593,9.37446532147149,
256.171139705882));
#153237=CARTESIAN_POINT('Ctrl Pts',(-48.8607426731792,13.9020798956618,
254.677022058823));
#153238=CARTESIAN_POINT('Ctrl Pts',(-47.5725252596992,18.4296944698521,
253.182904411765));
#153239=CARTESIAN_POINT('Ctrl Pts',(-45.4742952008371,22.6435084734481,
251.688786764706));
#153240=CARTESIAN_POINT('Ctrl Pts',(-43.3760651419751,26.8573224770442,
250.194669117647));
#153241=CARTESIAN_POINT('Ctrl Pts',(-40.5392751458362,30.6138395280662,
248.700551470588));
#153242=CARTESIAN_POINT('Ctrl Pts',(-37.7024851496972,34.3703565790883,
247.206433823529));
#153243=CARTESIAN_POINT('Ctrl Pts',(-34.2237386972451,37.5416529948095,
245.712316176471));
#153244=CARTESIAN_POINT('Ctrl Pts',(-30.744992244793,40.7129494105307,244.218198529412));
#153245=CARTESIAN_POINT('Ctrl Pts',(-26.7427538741697,43.1910304950644,
242.724080882353));
#153246=CARTESIAN_POINT('Ctrl Pts',(-22.7405155035463,45.6691115795981,
241.229963235294));
#153247=CARTESIAN_POINT('Ctrl Pts',(-18.3510766423074,47.3695892537413,
239.735845588235));
#153248=CARTESIAN_POINT('Ctrl Pts',(-13.9616377810684,49.0700669278844,
238.241727941177));
#153249=CARTESIAN_POINT('Ctrl Pts',(-9.33447550508177,49.9350334639422,
236.747610294118));
#153250=CARTESIAN_POINT('Ctrl Pts',(-4.7073132290951,50.8,235.253492647059));
#153251=CARTESIAN_POINT('Ctrl Pts',(-6.22120573966855E-15,50.8,233.759375));
#153252=CARTESIAN_POINT('Ctrl Pts',(4.70731322909511,50.8,232.265257352941));
#153253=CARTESIAN_POINT('Ctrl Pts',(9.33447550508176,49.9350334639422,230.771139705882));
#153254=CARTESIAN_POINT('Ctrl Pts',(13.9616377810684,49.0700669278844,229.277022058824));
#153255=CARTESIAN_POINT('Ctrl Pts',(18.3510766423074,47.3695892537413,227.782904411765));
#153256=CARTESIAN_POINT('Ctrl Pts',(22.7405155035463,45.6691115795981,226.288786764706));
#153257=CARTESIAN_POINT('Ctrl Pts',(26.7427538741697,43.1910304950644,224.794669117647));
#153258=CARTESIAN_POINT('Ctrl Pts',(30.744992244793,40.7129494105307,223.300551470588));
#153259=CARTESIAN_POINT('Ctrl Pts',(34.2237386972451,37.5416529948095,221.80643382353));
#153260=CARTESIAN_POINT('Ctrl Pts',(37.7024851496972,34.3703565790883,220.312316176471));
#153261=CARTESIAN_POINT('Ctrl Pts',(40.5392751458362,30.6138395280662,218.818198529412));
#153262=CARTESIAN_POINT('Ctrl Pts',(43.3760651419751,26.8573224770442,217.324080882353));
#153263=CARTESIAN_POINT('Ctrl Pts',(45.4742952008372,22.6435084734481,215.829963235294));
#153264=CARTESIAN_POINT('Ctrl Pts',(47.5725252596992,18.4296944698521,214.335845588235));
#153265=CARTESIAN_POINT('Ctrl Pts',(48.8607426731792,13.9020798956618,212.841727941177));
#153266=CARTESIAN_POINT('Ctrl Pts',(50.1489600866593,9.37446532147146,211.347610294118));
#153267=CARTESIAN_POINT('Ctrl Pts',(50.5832961557877,4.68723266073574,209.853492647059));
#153268=CARTESIAN_POINT('Ctrl Pts',(51.0176322249162,9.37178700064808E-15,
208.359375));
#153269=CARTESIAN_POINT('Ctrl Pts',(50.5832961557877,-4.68723266073572,
206.865257352941));
#153270=CARTESIAN_POINT('Ctrl Pts',(50.1489600866593,-9.37446532147149,
205.371139705882));
#153271=CARTESIAN_POINT('Ctrl Pts',(48.8607426731792,-13.9020798956618,
203.877022058824));
#153272=CARTESIAN_POINT('Ctrl Pts',(47.5725252596992,-18.4296944698521,
202.382904411765));
#153273=CARTESIAN_POINT('Ctrl Pts',(45.4742952008371,-22.6435084734482,
200.888786764706));
#153274=CARTESIAN_POINT('Ctrl Pts',(43.3760651419751,-26.8573224770441,
199.394669117647));
#153275=CARTESIAN_POINT('Ctrl Pts',(40.5392751458362,-30.6138395280662,
197.900551470588));
#153276=CARTESIAN_POINT('Ctrl Pts',(37.7024851496972,-34.3703565790883,
196.406433823529));
#153277=CARTESIAN_POINT('Ctrl Pts',(34.2237386972451,-37.5416529948095,
194.912316176471));
#153278=CARTESIAN_POINT('Ctrl Pts',(30.744992244793,-40.7129494105307,193.418198529412));
#153279=CARTESIAN_POINT('Ctrl Pts',(26.7427538741697,-43.1910304950644,
191.924080882353));
#153280=CARTESIAN_POINT('Ctrl Pts',(22.7405155035463,-45.6691115795981,
190.429963235294));
#153281=CARTESIAN_POINT('Ctrl Pts',(18.3510766423074,-47.3695892537413,
188.935845588235));
#153282=CARTESIAN_POINT('Ctrl Pts',(13.9616377810684,-49.0700669278844,
187.441727941176));
#153283=CARTESIAN_POINT('Ctrl Pts',(9.33447550508176,-49.9350334639422,
185.947610294118));
#153284=CARTESIAN_POINT('Ctrl Pts',(4.70731322909511,-50.8,184.453492647059));
#153285=CARTESIAN_POINT('Ctrl Pts',(0.,-50.8,182.959375));
#153286=CARTESIAN_POINT('Ctrl Pts',(-4.70731322909511,-50.8,181.465257352941));
#153287=CARTESIAN_POINT('Ctrl Pts',(-9.33447550508177,-49.9350334639422,
179.971139705882));
#153288=CARTESIAN_POINT('Ctrl Pts',(-13.9616377810684,-49.0700669278844,
178.477022058824));
#153289=CARTESIAN_POINT('Ctrl Pts',(-18.3510766423074,-47.3695892537413,
176.982904411765));
#153290=CARTESIAN_POINT('Ctrl Pts',(-22.7405155035463,-45.6691115795981,
175.488786764706));
#153291=CARTESIAN_POINT('Ctrl Pts',(-26.7427538741697,-43.1910304950644,
173.994669117647));
#153292=CARTESIAN_POINT('Ctrl Pts',(-30.744992244793,-40.7129494105307,
172.500551470588));
#153293=CARTESIAN_POINT('Ctrl Pts',(-34.2237386972451,-37.5416529948095,
171.00643382353));
#153294=CARTESIAN_POINT('Ctrl Pts',(-37.7024851496972,-34.3703565790883,
169.512316176471));
#153295=CARTESIAN_POINT('Ctrl Pts',(-40.5392751458362,-30.6138395280662,
168.018198529412));
#153296=CARTESIAN_POINT('Ctrl Pts',(-43.3760651419751,-26.8573224770441,
166.524080882353));
#153297=CARTESIAN_POINT('Ctrl Pts',(-45.4742952008371,-22.6435084734481,
165.029963235294));
#153298=CARTESIAN_POINT('Ctrl Pts',(-47.5725252596992,-18.4296944698521,
163.535845588235));
#153299=CARTESIAN_POINT('Ctrl Pts',(-48.8607426731792,-13.9020798956618,
162.041727941177));
#153300=CARTESIAN_POINT('Ctrl Pts',(-50.1489600866593,-9.37446532147148,
160.547610294118));
#153301=CARTESIAN_POINT('Ctrl Pts',(-50.5832961557877,-4.68723266073574,
159.053492647059));
#153302=CARTESIAN_POINT('Ctrl Pts',(-51.0176322249162,-3.12392900021603E-15,
157.559375));
#153303=CARTESIAN_POINT('Ctrl Pts',(-50.5832961557877,4.68723266073573,
156.065257352941));
#153304=CARTESIAN_POINT('Ctrl Pts',(-50.1489600866593,9.37446532147149,
154.571139705882));
#153305=CARTESIAN_POINT('Ctrl Pts',(-48.8607426731792,13.9020798956618,
153.077022058824));
#153306=CARTESIAN_POINT('Ctrl Pts',(-47.5725252596992,18.4296944698521,
151.582904411765));
#153307=CARTESIAN_POINT('Ctrl Pts',(-45.4742952008371,22.6435084734481,
150.088786764706));
#153308=CARTESIAN_POINT('Ctrl Pts',(-43.3760651419751,26.8573224770442,
148.594669117647));
#153309=CARTESIAN_POINT('Ctrl Pts',(-40.5392751458362,30.6138395280662,
147.100551470588));
#153310=CARTESIAN_POINT('Ctrl Pts',(-37.7024851496972,34.3703565790883,
145.606433823529));
#153311=CARTESIAN_POINT('Ctrl Pts',(-34.2237386972451,37.5416529948095,
144.112316176471));
#153312=CARTESIAN_POINT('Ctrl Pts',(-30.744992244793,40.7129494105307,142.618198529412));
#153313=CARTESIAN_POINT('Ctrl Pts',(-26.7427538741697,43.1910304950644,
141.124080882353));
#153314=CARTESIAN_POINT('Ctrl Pts',(-22.7405155035463,45.6691115795981,
139.629963235294));
#153315=CARTESIAN_POINT('Ctrl Pts',(-18.3510766423074,47.3695892537413,
138.135845588235));
#153316=CARTESIAN_POINT('Ctrl Pts',(-13.9616377810684,49.0700669278844,
136.641727941176));
#153317=CARTESIAN_POINT('Ctrl Pts',(-9.33447550508177,49.9350334639422,
135.147610294118));
#153318=CARTESIAN_POINT('Ctrl Pts',(-4.7073132290951,50.8,133.653492647059));
#153319=CARTESIAN_POINT('Ctrl Pts',(-6.22120573966855E-15,50.8,132.159375));
#153320=CARTESIAN_POINT('Ctrl Pts',(4.70731322909511,50.8,130.665257352941));
#153321=CARTESIAN_POINT('Ctrl Pts',(9.33447550508176,49.9350334639422,129.171139705882));
#153322=CARTESIAN_POINT('Ctrl Pts',(13.9616377810684,49.0700669278844,127.677022058823));
#153323=CARTESIAN_POINT('Ctrl Pts',(18.3510766423074,47.3695892537413,126.182904411765));
#153324=CARTESIAN_POINT('Ctrl Pts',(22.7405155035463,45.6691115795981,124.688786764706));
#153325=CARTESIAN_POINT('Ctrl Pts',(26.7427538741697,43.1910304950644,123.194669117647));
#153326=CARTESIAN_POINT('Ctrl Pts',(30.744992244793,40.7129494105307,121.700551470588));
#153327=CARTESIAN_POINT('Ctrl Pts',(34.2237386972451,37.5416529948095,120.206433823529));
#153328=CARTESIAN_POINT('Ctrl Pts',(37.7024851496972,34.3703565790883,118.712316176471));
#153329=CARTESIAN_POINT('Ctrl Pts',(40.5392751458362,30.6138395280662,117.218198529412));
#153330=CARTESIAN_POINT('Ctrl Pts',(43.3760651419751,26.8573224770442,115.724080882353));
#153331=CARTESIAN_POINT('Ctrl Pts',(45.4742952008372,22.6435084734481,114.229963235294));
#153332=CARTESIAN_POINT('Ctrl Pts',(47.5725252596992,18.4296944698521,112.735845588235));
#153333=CARTESIAN_POINT('Ctrl Pts',(48.8607426731792,13.9020798956618,111.241727941177));
#153334=CARTESIAN_POINT('Ctrl Pts',(50.1489600866593,9.37446532147146,109.747610294118));
#153335=CARTESIAN_POINT('Ctrl Pts',(50.5832961557877,4.68723266073574,108.253492647059));
#153336=CARTESIAN_POINT('Ctrl Pts',(51.0176322249162,9.37178700064808E-15,
106.759375));
#153337=CARTESIAN_POINT('Ctrl Pts',(50.5832961557877,-4.68723266073572,
105.265257352941));
#153338=CARTESIAN_POINT('Ctrl Pts',(50.1489600866593,-9.37446532147149,
103.771139705883));
#153339=CARTESIAN_POINT('Ctrl Pts',(48.8607426731792,-13.9020798956618,
102.277022058824));
#153340=CARTESIAN_POINT('Ctrl Pts',(47.5725252596992,-18.4296944698521,
100.782904411765));
#153341=CARTESIAN_POINT('Ctrl Pts',(45.4742952008371,-22.6435084734482,
99.2887867647059));
#153342=CARTESIAN_POINT('Ctrl Pts',(43.3760651419751,-26.8573224770441,
97.794669117647));
#153343=CARTESIAN_POINT('Ctrl Pts',(40.5392751458362,-30.6138395280662,
96.3005514705884));
#153344=CARTESIAN_POINT('Ctrl Pts',(37.7024851496972,-34.3703565790883,
94.8064338235295));
#153345=CARTESIAN_POINT('Ctrl Pts',(34.2237386972451,-37.5416529948095,
93.3123161764706));
#153346=CARTESIAN_POINT('Ctrl Pts',(30.744992244793,-40.7129494105307,91.8181985294118));
#153347=CARTESIAN_POINT('Ctrl Pts',(26.7427538741697,-43.1910304950644,
90.3240808823529));
#153348=CARTESIAN_POINT('Ctrl Pts',(22.7405155035463,-45.6691115795981,
88.8299632352943));
#153349=CARTESIAN_POINT('Ctrl Pts',(18.3510766423074,-47.3695892537413,
87.3358455882354));
#153350=CARTESIAN_POINT('Ctrl Pts',(13.9616377810684,-49.0700669278844,
85.8417279411765));
#153351=CARTESIAN_POINT('Ctrl Pts',(9.33447550508176,-49.9350334639422,
84.3476102941176));
#153352=CARTESIAN_POINT('Ctrl Pts',(4.70731322909511,-50.8,82.8534926470588));
#153353=CARTESIAN_POINT('Ctrl Pts',(0.,-50.8,81.3593750000001));
#153354=CARTESIAN_POINT('Ctrl Pts',(-4.70731322909511,-50.8,79.8652573529413));
#153355=CARTESIAN_POINT('Ctrl Pts',(-9.33447550508177,-49.9350334639422,
78.3711397058824));
#153356=CARTESIAN_POINT('Ctrl Pts',(-13.9616377810684,-49.0700669278844,
76.8770220588235));
#153357=CARTESIAN_POINT('Ctrl Pts',(-18.3510766423074,-47.3695892537413,
75.3829044117647));
#153358=CARTESIAN_POINT('Ctrl Pts',(-22.7405155035463,-45.6691115795981,
73.888786764706));
#153359=CARTESIAN_POINT('Ctrl Pts',(-26.7427538741697,-43.1910304950644,
72.3946691176471));
#153360=CARTESIAN_POINT('Ctrl Pts',(-30.744992244793,-40.7129494105307,
70.9005514705883));
#153361=CARTESIAN_POINT('Ctrl Pts',(-34.2237386972451,-37.5416529948095,
69.4064338235294));
#153362=CARTESIAN_POINT('Ctrl Pts',(-37.7024851496972,-34.3703565790883,
67.9123161764705));
#153363=CARTESIAN_POINT('Ctrl Pts',(-40.5392751458362,-30.6138395280662,
66.4181985294119));
#153364=CARTESIAN_POINT('Ctrl Pts',(-43.3760651419751,-26.8573224770441,
64.9240808823531));
#153365=CARTESIAN_POINT('Ctrl Pts',(-45.4742952008371,-22.6435084734481,
63.4299632352942));
#153366=CARTESIAN_POINT('Ctrl Pts',(-47.5725252596992,-18.4296944698521,
61.9358455882353));
#153367=CARTESIAN_POINT('Ctrl Pts',(-48.8607426731792,-13.9020798956618,
60.4417279411764));
#153368=CARTESIAN_POINT('Ctrl Pts',(-50.1489600866593,-9.37446532147148,
58.9476102941178));
#153369=CARTESIAN_POINT('Ctrl Pts',(-50.5832961557877,-4.68723266073574,
57.4534926470589));
#153370=CARTESIAN_POINT('Ctrl Pts',(-51.0176322249162,-3.12392900021603E-15,
55.9593750000001));
#153371=CARTESIAN_POINT('Ctrl Pts',(-50.5832961557877,4.68723266073573,
54.4652573529412));
#153372=CARTESIAN_POINT('Ctrl Pts',(-50.1489600866593,9.37446532147149,
52.9711397058823));
#153373=CARTESIAN_POINT('Ctrl Pts',(-48.8607426731792,13.9020798956618,
51.4770220588236));
#153374=CARTESIAN_POINT('Ctrl Pts',(-47.5725252596992,18.4296944698521,
49.9829044117648));
#153375=CARTESIAN_POINT('Ctrl Pts',(-45.4742952008371,22.6435084734481,
48.4887867647059));
#153376=CARTESIAN_POINT('Ctrl Pts',(-43.3760651419751,26.8573224770442,
46.994669117647));
#153377=CARTESIAN_POINT('Ctrl Pts',(-40.5392751458362,30.6138395280662,
45.5005514705882));
#153378=CARTESIAN_POINT('Ctrl Pts',(-37.7024851496972,34.3703565790883,
44.0064338235295));
#153379=CARTESIAN_POINT('Ctrl Pts',(-34.2237386972451,37.5416529948095,
42.5123161764707));
#153380=CARTESIAN_POINT('Ctrl Pts',(-30.744992244793,40.7129494105307,41.0181985294118));
#153381=CARTESIAN_POINT('Ctrl Pts',(-26.7427538741697,43.1910304950644,
39.5240808823529));
#153382=CARTESIAN_POINT('Ctrl Pts',(-22.7405155035463,45.6691115795981,
38.0299632352941));
#153383=CARTESIAN_POINT('Ctrl Pts',(-18.3510766423074,47.3695892537413,
36.5358455882354));
#153384=CARTESIAN_POINT('Ctrl Pts',(-13.9616377810684,49.0700669278844,
35.0417279411765));
#153385=CARTESIAN_POINT('Ctrl Pts',(-9.33447550508177,49.9350334639422,
33.5476102941177));
#153386=CARTESIAN_POINT('Ctrl Pts',(-4.7073132290951,50.8,32.0534926470588));
#153387=CARTESIAN_POINT('Ctrl Pts',(-6.22120573966855E-15,50.8,30.5593749999999));
#153388=CARTESIAN_POINT('Ctrl Pts',(4.70731322909511,50.8,29.0652573529413));
#153389=CARTESIAN_POINT('Ctrl Pts',(9.33447550508176,49.9350334639422,27.5711397058824));
#153390=CARTESIAN_POINT('Ctrl Pts',(13.9616377810684,49.0700669278844,26.0770220588236));
#153391=CARTESIAN_POINT('Ctrl Pts',(18.3510766423074,47.3695892537413,24.5829044117647));
#153392=CARTESIAN_POINT('Ctrl Pts',(22.7405155035463,45.6691115795981,23.0887867647058));
#153393=CARTESIAN_POINT('Ctrl Pts',(26.7427538741697,43.1910304950644,21.5946691176472));
#153394=CARTESIAN_POINT('Ctrl Pts',(30.744992244793,40.7129494105307,20.1005514705883));
#153395=CARTESIAN_POINT('Ctrl Pts',(34.2237386972451,37.5416529948095,18.6064338235294));
#153396=CARTESIAN_POINT('Ctrl Pts',(37.7024851496972,34.3703565790883,17.1123161764706));
#153397=CARTESIAN_POINT('Ctrl Pts',(40.5392751458362,30.6138395280662,15.6181985294117));
#153398=CARTESIAN_POINT('Ctrl Pts',(43.3760651419751,26.8573224770442,14.1240808823531));
#153399=CARTESIAN_POINT('Ctrl Pts',(45.4742952008372,22.6435084734481,12.6299632352942));
#153400=CARTESIAN_POINT('Ctrl Pts',(47.5725252596992,18.4296944698521,11.1358455882353));
#153401=CARTESIAN_POINT('Ctrl Pts',(48.8607426731792,13.9020798956618,9.64172794117646));
#153402=CARTESIAN_POINT('Ctrl Pts',(50.1489600866593,9.37446532147146,8.14761029411759));
#153403=CARTESIAN_POINT('Ctrl Pts',(50.5832961557877,4.68723266073574,6.65349264705895));
#153404=CARTESIAN_POINT('Ctrl Pts',(51.0176322249162,9.37178700064808E-15,
5.15937500000008));
#153405=CARTESIAN_POINT('Ctrl Pts',(50.5832961557877,-4.68723266073572,
3.66525735294121));
#153406=CARTESIAN_POINT('Ctrl Pts',(50.1489600866593,-9.37446532147149,
2.17113970588234));
#153407=CARTESIAN_POINT('Ctrl Pts',(48.8607426731792,-13.9020798956618,
0.677022058823473));
#153408=CARTESIAN_POINT('Ctrl Pts',(47.5725252596992,-18.4296944698521,
-0.817095588235173));
#153409=CARTESIAN_POINT('Ctrl Pts',(45.4742952008371,-22.6435084734482,
-2.31121323529404));
#153410=CARTESIAN_POINT('Ctrl Pts',(43.3760651419751,-26.8573224770441,
-3.80533088235291));
#153411=CARTESIAN_POINT('Ctrl Pts',(40.5392751458362,-30.6138395280662,
-5.29944852941178));
#153412=CARTESIAN_POINT('Ctrl Pts',(37.7024851496972,-34.3703565790883,
-6.79356617647064));
#153413=CARTESIAN_POINT('Ctrl Pts',(34.2237386972451,-37.5416529948095,
-8.28768382352929));
#153414=CARTESIAN_POINT('Ctrl Pts',(30.744992244793,-40.7129494105307,-9.78180147058816));
#153415=CARTESIAN_POINT('Ctrl Pts',(26.7427538741697,-43.1910304950644,
-11.275919117647));
#153416=CARTESIAN_POINT('Ctrl Pts',(22.7405155035463,-45.6691115795981,
-12.7700367647059));
#153417=CARTESIAN_POINT('Ctrl Pts',(18.3510766423074,-47.3695892537413,
-14.2641544117648));
#153418=CARTESIAN_POINT('Ctrl Pts',(13.9616377810684,-49.0700669278844,
-15.7582720588234));
#153419=CARTESIAN_POINT('Ctrl Pts',(9.33447550508176,-49.9350334639422,
-17.2523897058823));
#153420=CARTESIAN_POINT('Ctrl Pts',(4.70731322909511,-50.8,-18.7465073529412));
#153421=CARTESIAN_POINT('Ctrl Pts',(0.,-50.8,-20.240625));
#153422=CARTESIAN_POINT('Ctrl Pts',(-4.70731322909511,-50.8,-21.7347426470589));
#153423=CARTESIAN_POINT('Ctrl Pts',(-9.33447550508177,-49.9350334639422,
-23.2288602941175));
#153424=CARTESIAN_POINT('Ctrl Pts',(-13.9616377810684,-49.0700669278844,
-24.7229779411764));
#153425=CARTESIAN_POINT('Ctrl Pts',(-18.3510766423074,-47.3695892537413,
-26.2170955882353));
#153426=CARTESIAN_POINT('Ctrl Pts',(-22.7405155035463,-45.6691115795981,
-27.7112132352941));
#153427=CARTESIAN_POINT('Ctrl Pts',(-26.7427538741697,-43.1910304950644,
-29.205330882353));
#153428=CARTESIAN_POINT('Ctrl Pts',(-30.744992244793,-40.7129494105307,
-30.6994485294116));
#153429=CARTESIAN_POINT('Ctrl Pts',(-34.2237386972451,-37.5416529948095,
-32.1935661764705));
#153430=CARTESIAN_POINT('Ctrl Pts',(-37.7024851496972,-34.3703565790883,
-33.6876838235294));
#153431=CARTESIAN_POINT('Ctrl Pts',(-40.5392751458362,-30.6138395280662,
-35.1818014705882));
#153432=CARTESIAN_POINT('Ctrl Pts',(-43.3760651419751,-26.8573224770441,
-36.6759191176471));
#153433=CARTESIAN_POINT('Ctrl Pts',(-45.4742952008371,-22.6435084734481,
-38.1700367647058));
#153434=CARTESIAN_POINT('Ctrl Pts',(-47.5725252596992,-18.4296944698521,
-39.6641544117646));
#153435=CARTESIAN_POINT('Ctrl Pts',(-48.8607426731792,-13.9020798956618,
-41.1582720588235));
#153436=CARTESIAN_POINT('Ctrl Pts',(-50.1489600866593,-9.37446532147148,
-42.6523897058824));
#153437=CARTESIAN_POINT('Ctrl Pts',(-50.5832961557877,-4.68723266073574,
-44.1465073529412));
#153438=CARTESIAN_POINT('Ctrl Pts',(-51.0176322249162,-3.12392900021603E-15,
-45.6406249999999));
#153439=CARTESIAN_POINT('Ctrl Pts',(-50.5832961557877,4.68723266073573,
-47.1347426470587));
#153440=CARTESIAN_POINT('Ctrl Pts',(-50.1489600866593,9.37446532147149,
-48.6288602941176));
#153441=CARTESIAN_POINT('Ctrl Pts',(-48.8607426731792,13.9020798956618,
-50.1229779411765));
#153442=CARTESIAN_POINT('Ctrl Pts',(-47.5725252596992,18.4296944698521,
-51.6170955882354));
#153443=CARTESIAN_POINT('Ctrl Pts',(-45.4742952008371,22.6435084734481,
-53.111213235294));
#153444=CARTESIAN_POINT('Ctrl Pts',(-43.3760651419751,26.8573224770442,
-54.6053308823529));
#153445=CARTESIAN_POINT('Ctrl Pts',(-40.5392751458362,30.6138395280662,
-56.0994485294117));
#153446=CARTESIAN_POINT('Ctrl Pts',(-37.7024851496972,34.3703565790883,
-57.5935661764706));
#153447=CARTESIAN_POINT('Ctrl Pts',(-34.2237386972451,37.5416529948095,
-59.0876838235295));
#153448=CARTESIAN_POINT('Ctrl Pts',(-30.744992244793,40.7129494105307,-60.5818014705881));
#153449=CARTESIAN_POINT('Ctrl Pts',(-26.7427538741697,43.1910304950644,
-62.075919117647));
#153450=CARTESIAN_POINT('Ctrl Pts',(-22.7405155035463,45.6691115795981,
-63.5700367647058));
#153451=CARTESIAN_POINT('Ctrl Pts',(-18.3510766423074,47.3695892537413,
-65.0641544117647));
#153452=CARTESIAN_POINT('Ctrl Pts',(-13.9616377810684,49.0700669278844,
-66.5582720588236));
#153453=CARTESIAN_POINT('Ctrl Pts',(-9.33447550508177,49.9350334639422,
-68.0523897058822));
#153454=CARTESIAN_POINT('Ctrl Pts',(-4.7073132290951,50.8,-69.5465073529411));
#153455=CARTESIAN_POINT('Ctrl Pts',(-6.22120573966855E-15,50.8,-71.040625));
#153456=CARTESIAN_POINT('Ctrl Pts',(4.70731322909511,50.8,-72.5347426470588));
#153457=CARTESIAN_POINT('Ctrl Pts',(9.33447550508176,49.9350334639422,-74.0288602941177));
#153458=CARTESIAN_POINT('Ctrl Pts',(13.9616377810684,49.0700669278844,-75.5229779411764));
#153459=CARTESIAN_POINT('Ctrl Pts',(18.3510766423074,47.3695892537413,-77.0170955882352));
#153460=CARTESIAN_POINT('Ctrl Pts',(22.7405155035463,45.6691115795981,-78.5112132352941));
#153461=CARTESIAN_POINT('Ctrl Pts',(26.7427538741697,43.1910304950644,-80.005330882353));
#153462=CARTESIAN_POINT('Ctrl Pts',(30.744992244793,40.7129494105307,-81.4994485294118));
#153463=CARTESIAN_POINT('Ctrl Pts',(34.2237386972451,37.5416529948095,-82.9935661764705));
#153464=CARTESIAN_POINT('Ctrl Pts',(37.7024851496972,34.3703565790883,-84.4876838235294));
#153465=CARTESIAN_POINT('Ctrl Pts',(40.5392751458362,30.6138395280662,-85.9818014705882));
#153466=CARTESIAN_POINT('Ctrl Pts',(43.3760651419751,26.8573224770442,-87.4759191176471));
#153467=CARTESIAN_POINT('Ctrl Pts',(45.4742952008372,22.6435084734481,-88.970036764706));
#153468=CARTESIAN_POINT('Ctrl Pts',(47.5725252596992,18.4296944698521,-90.4641544117646));
#153469=CARTESIAN_POINT('Ctrl Pts',(48.8607426731792,13.9020798956618,-91.9582720588235));
#153470=CARTESIAN_POINT('Ctrl Pts',(50.1489600866593,9.37446532147146,-93.4523897058823));
#153471=CARTESIAN_POINT('Ctrl Pts',(50.5832961557877,4.68723266073574,-94.9465073529412));
#153472=CARTESIAN_POINT('Ctrl Pts',(51.0176322249162,9.37178700064808E-15,
-96.4406250000001));
#153473=CARTESIAN_POINT('Ctrl Pts',(50.5832961557877,-4.68723266073572,
-97.9347426470587));
#153474=CARTESIAN_POINT('Ctrl Pts',(50.1489600866593,-9.37446532147149,
-99.4288602941176));
#153475=CARTESIAN_POINT('Ctrl Pts',(48.8607426731792,-13.9020798956618,
-100.922977941176));
#153476=CARTESIAN_POINT('Ctrl Pts',(47.5725252596992,-18.4296944698521,
-102.417095588235));
#153477=CARTESIAN_POINT('Ctrl Pts',(45.4742952008371,-22.6435084734482,
-103.911213235294));
#153478=CARTESIAN_POINT('Ctrl Pts',(43.3760651419751,-26.8573224770441,
-105.405330882353));
#153479=CARTESIAN_POINT('Ctrl Pts',(40.5392751458362,-30.6138395280662,
-106.899448529412));
#153480=CARTESIAN_POINT('Ctrl Pts',(37.7024851496972,-34.3703565790883,
-108.393566176471));
#153481=CARTESIAN_POINT('Ctrl Pts',(34.2237386972451,-37.5416529948095,
-109.887683823529));
#153482=CARTESIAN_POINT('Ctrl Pts',(30.744992244793,-40.7129494105307,-111.381801470588));
#153483=CARTESIAN_POINT('Ctrl Pts',(26.7427538741697,-43.1910304950644,
-112.875919117647));
#153484=CARTESIAN_POINT('Ctrl Pts',(22.7405155035463,-45.6691115795981,
-114.370036764706));
#153485=CARTESIAN_POINT('Ctrl Pts',(18.3510766423074,-47.3695892537413,
-115.864154411765));
#153486=CARTESIAN_POINT('Ctrl Pts',(13.9616377810684,-49.0700669278844,
-117.358272058824));
#153487=CARTESIAN_POINT('Ctrl Pts',(9.33447550508176,-49.9350334639422,
-118.852389705882));
#153488=CARTESIAN_POINT('Ctrl Pts',(4.70731322909511,-50.8,-120.346507352941));
#153489=CARTESIAN_POINT('Ctrl Pts',(0.,-50.8,-121.840625));
#153490=CARTESIAN_POINT('Ctrl Pts',(-4.70731322909511,-50.8,-123.334742647059));
#153491=CARTESIAN_POINT('Ctrl Pts',(-9.33447550508177,-49.9350334639422,
-124.828860294118));
#153492=CARTESIAN_POINT('Ctrl Pts',(-13.9616377810684,-49.0700669278844,
-126.322977941177));
#153493=CARTESIAN_POINT('Ctrl Pts',(-18.3510766423074,-47.3695892537413,
-127.817095588235));
#153494=CARTESIAN_POINT('Ctrl Pts',(-22.7405155035463,-45.6691115795981,
-129.311213235294));
#153495=CARTESIAN_POINT('Ctrl Pts',(-26.7427538741697,-43.1910304950644,
-130.805330882353));
#153496=CARTESIAN_POINT('Ctrl Pts',(-30.744992244793,-40.7129494105307,
-132.299448529412));
#153497=CARTESIAN_POINT('Ctrl Pts',(-34.2237386972451,-37.5416529948095,
-133.793566176471));
#153498=CARTESIAN_POINT('Ctrl Pts',(-37.7024851496972,-34.3703565790883,
-135.287683823529));
#153499=CARTESIAN_POINT('Ctrl Pts',(-40.5392751458362,-30.6138395280662,
-136.781801470588));
#153500=CARTESIAN_POINT('Ctrl Pts',(-43.3760651419751,-26.8573224770441,
-138.275919117647));
#153501=CARTESIAN_POINT('Ctrl Pts',(-45.4742952008371,-22.6435084734481,
-139.770036764706));
#153502=CARTESIAN_POINT('Ctrl Pts',(-47.5725252596992,-18.4296944698521,
-141.264154411765));
#153503=CARTESIAN_POINT('Ctrl Pts',(-48.8607426731792,-13.9020798956618,
-142.758272058823));
#153504=CARTESIAN_POINT('Ctrl Pts',(-50.1489600866593,-9.37446532147148,
-144.252389705882));
#153505=CARTESIAN_POINT('Ctrl Pts',(-50.5832961557877,-4.68723266073574,
-145.746507352941));
#153506=CARTESIAN_POINT('Ctrl Pts',(-51.0176322249162,-3.12392900021603E-15,
-147.240625));
#153507=CARTESIAN_POINT('Ctrl Pts',(-50.5832961557877,4.68723266073573,
-148.734742647059));
#153508=CARTESIAN_POINT('Ctrl Pts',(-50.1489600866593,9.37446532147149,
-150.228860294118));
#153509=CARTESIAN_POINT('Ctrl Pts',(-48.8607426731792,13.9020798956618,
-151.722977941176));
#153510=CARTESIAN_POINT('Ctrl Pts',(-47.5725252596992,18.4296944698521,
-153.217095588235));
#153511=CARTESIAN_POINT('Ctrl Pts',(-45.4742952008371,22.6435084734481,
-154.711213235294));
#153512=CARTESIAN_POINT('Ctrl Pts',(-43.3760651419751,26.8573224770442,
-156.205330882353));
#153513=CARTESIAN_POINT('Ctrl Pts',(-40.5392751458362,30.6138395280662,
-157.699448529412));
#153514=CARTESIAN_POINT('Ctrl Pts',(-37.7024851496972,34.3703565790883,
-159.193566176471));
#153515=CARTESIAN_POINT('Ctrl Pts',(-34.2237386972451,37.5416529948095,
-160.687683823529));
#153516=CARTESIAN_POINT('Ctrl Pts',(-30.744992244793,40.7129494105307,-162.181801470588));
#153517=CARTESIAN_POINT('Ctrl Pts',(-26.7427538741697,43.1910304950644,
-163.675919117647));
#153518=CARTESIAN_POINT('Ctrl Pts',(-22.7405155035463,45.6691115795981,
-165.170036764706));
#153519=CARTESIAN_POINT('Ctrl Pts',(-18.3510766423074,47.3695892537413,
-166.664154411765));
#153520=CARTESIAN_POINT('Ctrl Pts',(-13.9616377810684,49.0700669278844,
-168.158272058824));
#153521=CARTESIAN_POINT('Ctrl Pts',(-9.33447550508177,49.9350334639422,
-169.652389705882));
#153522=CARTESIAN_POINT('Ctrl Pts',(-4.7073132290951,50.8,-171.146507352941));
#153523=CARTESIAN_POINT('Ctrl Pts',(-6.22120573966855E-15,50.8,-172.640625));
#153524=CARTESIAN_POINT('Ctrl Pts',(4.70731322909511,50.8,-174.134742647059));
#153525=CARTESIAN_POINT('Ctrl Pts',(9.33447550508176,49.9350334639422,-175.628860294118));
#153526=CARTESIAN_POINT('Ctrl Pts',(13.9616377810684,49.0700669278844,-177.122977941176));
#153527=CARTESIAN_POINT('Ctrl Pts',(18.3510766423074,47.3695892537413,-178.617095588235));
#153528=CARTESIAN_POINT('Ctrl Pts',(22.7405155035463,45.6691115795981,-180.111213235294));
#153529=CARTESIAN_POINT('Ctrl Pts',(26.7427538741697,43.1910304950644,-181.605330882353));
#153530=CARTESIAN_POINT('Ctrl Pts',(30.744992244793,40.7129494105307,-183.099448529412));
#153531=CARTESIAN_POINT('Ctrl Pts',(34.2237386972451,37.5416529948095,-184.593566176471));
#153532=CARTESIAN_POINT('Ctrl Pts',(37.7024851496972,34.3703565790883,-186.087683823529));
#153533=CARTESIAN_POINT('Ctrl Pts',(40.5392751458362,30.6138395280662,-187.581801470588));
#153534=CARTESIAN_POINT('Ctrl Pts',(43.3760651419751,26.8573224770442,-189.075919117647));
#153535=CARTESIAN_POINT('Ctrl Pts',(45.4742952008372,22.6435084734481,-190.570036764706));
#153536=CARTESIAN_POINT('Ctrl Pts',(47.5725252596992,18.4296944698521,-192.064154411765));
#153537=CARTESIAN_POINT('Ctrl Pts',(48.8607426731792,13.9020798956618,-193.558272058824));
#153538=CARTESIAN_POINT('Ctrl Pts',(50.1489600866593,9.37446532147146,-195.052389705882));
#153539=CARTESIAN_POINT('Ctrl Pts',(50.5832961557877,4.68723266073574,-196.546507352941));
#153540=CARTESIAN_POINT('Ctrl Pts',(51.0176322249162,9.37178700064808E-15,
-198.040625));
#153541=CARTESIAN_POINT('Ctrl Pts',(50.5832961557877,-4.68723266073572,
-199.534742647059));
#153542=CARTESIAN_POINT('Ctrl Pts',(50.1489600866593,-9.37446532147149,
-201.028860294118));
#153543=CARTESIAN_POINT('Ctrl Pts',(48.8607426731792,-13.9020798956618,
-202.522977941176));
#153544=CARTESIAN_POINT('Ctrl Pts',(47.5725252596992,-18.4296944698521,
-204.017095588235));
#153545=CARTESIAN_POINT('Ctrl Pts',(45.4742952008371,-22.6435084734482,
-205.511213235294));
#153546=CARTESIAN_POINT('Ctrl Pts',(43.3760651419751,-26.8573224770441,
-207.005330882353));
#153547=CARTESIAN_POINT('Ctrl Pts',(40.5392751458362,-30.6138395280662,
-208.499448529412));
#153548=CARTESIAN_POINT('Ctrl Pts',(37.7024851496972,-34.3703565790883,
-209.99356617647));
#153549=CARTESIAN_POINT('Ctrl Pts',(34.2237386972451,-37.5416529948095,
-211.487683823529));
#153550=CARTESIAN_POINT('Ctrl Pts',(30.744992244793,-40.7129494105307,-212.981801470588));
#153551=CARTESIAN_POINT('Ctrl Pts',(26.7427538741697,-43.1910304950644,
-214.475919117647));
#153552=CARTESIAN_POINT('Ctrl Pts',(22.7405155035463,-45.6691115795981,
-215.970036764706));
#153553=CARTESIAN_POINT('Ctrl Pts',(18.3510766423074,-47.3695892537413,
-217.464154411765));
#153554=CARTESIAN_POINT('Ctrl Pts',(13.9616377810684,-49.0700669278844,
-218.958272058824));
#153555=CARTESIAN_POINT('Ctrl Pts',(9.33447550508176,-49.9350334639422,
-220.452389705882));
#153556=CARTESIAN_POINT('Ctrl Pts',(4.70731322909511,-50.8,-221.946507352941));
#153557=CARTESIAN_POINT('Ctrl Pts',(0.,-50.8,-223.440625));
#153558=CARTESIAN_POINT('Ctrl Pts',(-4.70731322909511,-50.8,-224.934742647059));
#153559=CARTESIAN_POINT('Ctrl Pts',(-9.33447550508177,-49.9350334639422,
-226.428860294118));
#153560=CARTESIAN_POINT('Ctrl Pts',(-13.9616377810684,-49.0700669278844,
-227.922977941176));
#153561=CARTESIAN_POINT('Ctrl Pts',(-18.3510766423074,-47.3695892537413,
-229.417095588235));
#153562=CARTESIAN_POINT('Ctrl Pts',(-22.7405155035463,-45.6691115795981,
-230.911213235294));
#153563=CARTESIAN_POINT('Ctrl Pts',(-26.7427538741697,-43.1910304950644,
-232.405330882353));
#153564=CARTESIAN_POINT('Ctrl Pts',(-30.744992244793,-40.7129494105307,
-233.899448529412));
#153565=CARTESIAN_POINT('Ctrl Pts',(-34.2237386972451,-37.5416529948095,
-235.393566176471));
#153566=CARTESIAN_POINT('Ctrl Pts',(-37.7024851496972,-34.3703565790883,
-236.887683823529));
#153567=CARTESIAN_POINT('Ctrl Pts',(-40.5392751458362,-30.6138395280662,
-238.381801470588));
#153568=CARTESIAN_POINT('Ctrl Pts',(-43.3760651419751,-26.8573224770441,
-239.875919117647));
#153569=CARTESIAN_POINT('Ctrl Pts',(-45.4742952008371,-22.6435084734481,
-241.370036764706));
#153570=CARTESIAN_POINT('Ctrl Pts',(-47.5725252596992,-18.4296944698521,
-242.864154411765));
#153571=CARTESIAN_POINT('Ctrl Pts',(-48.8607426731792,-13.9020798956618,
-244.358272058824));
#153572=CARTESIAN_POINT('Ctrl Pts',(-50.1489600866593,-9.37446532147148,
-245.852389705882));
#153573=CARTESIAN_POINT('Ctrl Pts',(-50.5832961557877,-4.68723266073574,
-247.346507352941));
#153574=CARTESIAN_POINT('Ctrl Pts',(-51.0176322249162,-3.12392900021603E-15,
-248.840625));
#153575=CARTESIAN_POINT('Ctrl Pts',(-50.5832961557877,4.68723266073573,
-250.334742647059));
#153576=CARTESIAN_POINT('Ctrl Pts',(-50.1489600866593,9.37446532147149,
-251.828860294118));
#153577=CARTESIAN_POINT('Ctrl Pts',(-48.8607426731792,13.9020798956618,
-253.322977941177));
#153578=CARTESIAN_POINT('Ctrl Pts',(-47.5725252596992,18.4296944698521,
-254.817095588235));
#153579=CARTESIAN_POINT('Ctrl Pts',(-45.4742952008371,22.6435084734481,
-256.311213235294));
#153580=CARTESIAN_POINT('Ctrl Pts',(-43.3760651419751,26.8573224770442,
-257.805330882353));
#153581=CARTESIAN_POINT('Ctrl Pts',(-40.5392751458362,30.6138395280662,
-259.299448529412));
#153582=CARTESIAN_POINT('Ctrl Pts',(-37.7024851496972,34.3703565790883,
-260.793566176471));
#153583=CARTESIAN_POINT('Ctrl Pts',(-34.2237386972451,37.5416529948095,
-262.287683823529));
#153584=CARTESIAN_POINT('Ctrl Pts',(-30.744992244793,40.7129494105307,-263.781801470588));
#153585=CARTESIAN_POINT('Ctrl Pts',(-26.7427538741697,43.1910304950644,
-265.275919117647));
#153586=CARTESIAN_POINT('Ctrl Pts',(-22.7405155035463,45.6691115795981,
-266.770036764706));
#153587=CARTESIAN_POINT('Ctrl Pts',(-18.3510766423074,47.3695892537413,
-268.264154411765));
#153588=CARTESIAN_POINT('Ctrl Pts',(-13.9616377810684,49.0700669278844,
-269.758272058823));
#153589=CARTESIAN_POINT('Ctrl Pts',(-9.33447550508177,49.9350334639422,
-271.252389705882));
#153590=CARTESIAN_POINT('Ctrl Pts',(-4.7073132290951,50.8,-272.746507352941));
#153591=CARTESIAN_POINT('Ctrl Pts',(-6.22120573966855E-15,50.8,-274.240625));
#153592=CARTESIAN_POINT('Ctrl Pts',(4.70731322909511,50.8,-275.734742647059));
#153593=CARTESIAN_POINT('Ctrl Pts',(9.33447550508176,49.9350334639422,-277.228860294118));
#153594=CARTESIAN_POINT('Ctrl Pts',(13.9616377810684,49.0700669278844,-278.722977941176));
#153595=CARTESIAN_POINT('Ctrl Pts',(18.3510766423074,47.3695892537413,-280.217095588235));
#153596=CARTESIAN_POINT('Ctrl Pts',(22.7405155035463,45.6691115795981,-281.711213235294));
#153597=CARTESIAN_POINT('Ctrl Pts',(26.7427538741697,43.1910304950644,-283.205330882353));
#153598=CARTESIAN_POINT('Ctrl Pts',(30.744992244793,40.7129494105307,-284.699448529412));
#153599=CARTESIAN_POINT('Ctrl Pts',(34.2237386972451,37.5416529948095,-286.193566176471));
#153600=CARTESIAN_POINT('Ctrl Pts',(37.7024851496972,34.3703565790883,-287.687683823529));
#153601=CARTESIAN_POINT('Ctrl Pts',(40.5392751458362,30.6138395280662,-289.181801470588));
#153602=CARTESIAN_POINT('Ctrl Pts',(43.3760651419751,26.8573224770442,-290.675919117647));
#153603=CARTESIAN_POINT('Ctrl Pts',(45.4742952008372,22.6435084734481,-292.170036764706));
#153604=CARTESIAN_POINT('Ctrl Pts',(47.5725252596992,18.4296944698521,-293.664154411765));
#153605=CARTESIAN_POINT('Ctrl Pts',(48.8607426731792,13.9020798956618,-295.158272058824));
#153606=CARTESIAN_POINT('Ctrl Pts',(50.1489600866593,9.37446532147146,-296.652389705882));
#153607=CARTESIAN_POINT('Ctrl Pts',(50.5832961557877,4.68723266073574,-298.146507352941));
#153608=CARTESIAN_POINT('Ctrl Pts',(51.0176322249162,9.37178700064808E-15,
-299.640625));
#153609=CARTESIAN_POINT('Ctrl Pts',(50.5832961557877,-4.68723266073572,
-301.134742647059));
#153610=CARTESIAN_POINT('Ctrl Pts',(50.1489600866593,-9.37446532147149,
-302.628860294118));
#153611=CARTESIAN_POINT('Ctrl Pts',(48.8607426731792,-13.9020798956618,
-304.122977941176));
#153612=CARTESIAN_POINT('Ctrl Pts',(47.5725252596992,-18.4296944698521,
-305.617095588235));
#153613=CARTESIAN_POINT('Ctrl Pts',(45.4742952008371,-22.6435084734482,
-307.111213235294));
#153614=CARTESIAN_POINT('Ctrl Pts',(43.3760651419751,-26.8573224770441,
-308.605330882353));
#153615=CARTESIAN_POINT('Ctrl Pts',(40.5392751458362,-30.6138395280662,
-310.099448529412));
#153616=CARTESIAN_POINT('Ctrl Pts',(37.7024851496972,-34.3703565790883,
-311.593566176471));
#153617=CARTESIAN_POINT('Ctrl Pts',(34.2237386972451,-37.5416529948095,
-313.087683823529));
#153618=CARTESIAN_POINT('Ctrl Pts',(30.744992244793,-40.7129494105307,-314.581801470588));
#153619=CARTESIAN_POINT('Ctrl Pts',(26.7427538741697,-43.1910304950644,
-316.075919117647));
#153620=CARTESIAN_POINT('Ctrl Pts',(22.7405155035463,-45.6691115795981,
-317.570036764706));
#153621=CARTESIAN_POINT('Ctrl Pts',(18.3510766423074,-47.3695892537413,
-319.064154411765));
#153622=CARTESIAN_POINT('Ctrl Pts',(13.9616377810684,-49.0700669278844,
-320.558272058824));
#153623=CARTESIAN_POINT('Ctrl Pts',(9.33447550508176,-49.9350334639422,
-322.052389705882));
#153624=CARTESIAN_POINT('Ctrl Pts',(4.70731322909511,-50.8,-323.546507352941));
#153625=CARTESIAN_POINT('Ctrl Pts',(0.,-50.8,-325.040625));
#153626=CARTESIAN_POINT('Ctrl Pts',(-4.70731322909511,-50.8,-326.534742647059));
#153627=CARTESIAN_POINT('Ctrl Pts',(-9.33447550508177,-49.9350334639422,
-328.028860294118));
#153628=CARTESIAN_POINT('Ctrl Pts',(-13.9616377810684,-49.0700669278844,
-329.522977941176));
#153629=CARTESIAN_POINT('Ctrl Pts',(-18.3510766423074,-47.3695892537413,
-331.017095588235));
#153630=CARTESIAN_POINT('Ctrl Pts',(-22.7405155035463,-45.6691115795981,
-332.511213235294));
#153631=CARTESIAN_POINT('Ctrl Pts',(-26.7427538741697,-43.1910304950644,
-334.005330882353));
#153632=CARTESIAN_POINT('Ctrl Pts',(-30.744992244793,-40.7129494105307,
-335.499448529412));
#153633=CARTESIAN_POINT('Ctrl Pts',(-34.2237386972451,-37.5416529948095,
-336.99356617647));
#153634=CARTESIAN_POINT('Ctrl Pts',(-37.7024851496972,-34.3703565790883,
-338.487683823529));
#153635=CARTESIAN_POINT('Ctrl Pts',(-40.5392751458362,-30.6138395280662,
-339.981801470588));
#153636=CARTESIAN_POINT('Ctrl Pts',(-43.3760651419751,-26.8573224770441,
-341.475919117647));
#153637=CARTESIAN_POINT('Ctrl Pts',(-45.4742952008371,-22.6435084734481,
-342.970036764706));
#153638=CARTESIAN_POINT('Ctrl Pts',(-47.5725252596992,-18.4296944698521,
-344.464154411765));
#153639=CARTESIAN_POINT('Ctrl Pts',(-48.8607426731792,-13.9020798956618,
-345.958272058824));
#153640=CARTESIAN_POINT('Ctrl Pts',(-50.1489600866593,-9.37446532147148,
-347.452389705882));
#153641=CARTESIAN_POINT('Ctrl Pts',(-50.5832961557877,-4.68723266073574,
-348.946507352941));
#153642=CARTESIAN_POINT('Ctrl Pts',(-51.0176322249162,-3.12392900021603E-15,
-350.440625));
#153643=CARTESIAN_POINT('Ctrl Pts',(-50.5832961557877,4.68723266073573,
-351.934742647059));
#153644=CARTESIAN_POINT('Ctrl Pts',(-50.1489600866593,9.37446532147149,
-353.428860294118));
#153645=CARTESIAN_POINT('Ctrl Pts',(-48.8607426731792,13.9020798956618,
-354.922977941176));
#153646=CARTESIAN_POINT('Ctrl Pts',(-47.5725252596992,18.4296944698521,
-356.417095588235));
#153647=CARTESIAN_POINT('Ctrl Pts',(-45.4742952008371,22.6435084734481,
-357.911213235294));
#153648=CARTESIAN_POINT('Ctrl Pts',(-43.3760651419751,26.8573224770442,
-359.405330882353));
#153649=CARTESIAN_POINT('Ctrl Pts',(-40.5392751458362,30.6138395280662,
-360.899448529412));
#153650=CARTESIAN_POINT('Ctrl Pts',(-37.7024851496972,34.3703565790883,
-362.393566176471));
#153651=CARTESIAN_POINT('Ctrl Pts',(-34.2237386972451,37.5416529948095,
-363.887683823529));
#153652=CARTESIAN_POINT('Ctrl Pts',(-30.744992244793,40.7129494105307,-365.381801470588));
#153653=CARTESIAN_POINT('Ctrl Pts',(-26.7427538741697,43.1910304950644,
-366.875919117647));
#153654=CARTESIAN_POINT('Ctrl Pts',(-22.7405155035463,45.6691115795981,
-368.370036764706));
#153655=CARTESIAN_POINT('Ctrl Pts',(-18.3510766423074,47.3695892537413,
-369.864154411765));
#153656=CARTESIAN_POINT('Ctrl Pts',(-13.9616377810684,49.0700669278844,
-371.358272058824));
#153657=CARTESIAN_POINT('Ctrl Pts',(-9.33447550508177,49.9350334639422,
-372.852389705882));
#153658=CARTESIAN_POINT('Ctrl Pts',(-4.7073132290951,50.8,-374.346507352941));
#153659=CARTESIAN_POINT('Ctrl Pts',(-6.22120573966855E-15,50.8,-375.840625));
#153660=CARTESIAN_POINT('Ctrl Pts',(4.70731322909511,50.8,-377.334742647059));
#153661=CARTESIAN_POINT('Ctrl Pts',(9.33447550508176,49.9350334639422,-378.828860294118));
#153662=CARTESIAN_POINT('Ctrl Pts',(13.9616377810684,49.0700669278844,-380.322977941177));
#153663=CARTESIAN_POINT('Ctrl Pts',(18.3510766423074,47.3695892537413,-381.817095588235));
#153664=CARTESIAN_POINT('Ctrl Pts',(22.7405155035463,45.6691115795981,-383.311213235294));
#153665=CARTESIAN_POINT('Ctrl Pts',(26.7427538741697,43.1910304950644,-384.805330882353));
#153666=CARTESIAN_POINT('Ctrl Pts',(30.744992244793,40.7129494105307,-386.299448529412));
#153667=CARTESIAN_POINT('Ctrl Pts',(34.2237386972451,37.5416529948095,-387.793566176471));
#153668=CARTESIAN_POINT('Ctrl Pts',(37.7024851496972,34.3703565790883,-389.287683823529));
#153669=CARTESIAN_POINT('Ctrl Pts',(40.5392751458362,30.6138395280662,-390.781801470588));
#153670=CARTESIAN_POINT('Ctrl Pts',(43.3760651419751,26.8573224770442,-392.275919117647));
#153671=CARTESIAN_POINT('Ctrl Pts',(45.4742952008372,22.6435084734481,-393.770036764706));
#153672=CARTESIAN_POINT('Ctrl Pts',(47.5725252596992,18.4296944698521,-395.264154411765));
#153673=CARTESIAN_POINT('Ctrl Pts',(48.8607426731792,13.9020798956618,-396.758272058823));
#153674=CARTESIAN_POINT('Ctrl Pts',(50.1489600866593,9.37446532147146,-398.252389705882));
#153675=CARTESIAN_POINT('Ctrl Pts',(50.5832961557877,4.68723266073574,-399.746507352941));
#153676=CARTESIAN_POINT('Ctrl Pts',(51.0176322249162,9.37178700064808E-15,
-401.240625));
#153677=CARTESIAN_POINT('Ctrl Pts',(50.5832961557877,-4.68723266073572,
-402.734742647059));
#153678=CARTESIAN_POINT('Ctrl Pts',(50.1489600866593,-9.37446532147149,
-404.228860294118));
#153679=CARTESIAN_POINT('Ctrl Pts',(48.8607426731792,-13.9020798956618,
-405.722977941176));
#153680=CARTESIAN_POINT('Ctrl Pts',(47.5725252596992,-18.4296944698521,
-407.217095588235));
#153681=CARTESIAN_POINT('Ctrl Pts',(45.4742952008371,-22.6435084734482,
-408.711213235294));
#153682=CARTESIAN_POINT('Ctrl Pts',(43.3760651419751,-26.8573224770441,
-410.205330882353));
#153683=CARTESIAN_POINT('Ctrl Pts',(40.5392751458362,-30.6138395280662,
-411.699448529412));
#153684=CARTESIAN_POINT('Ctrl Pts',(37.7024851496972,-34.3703565790883,
-413.193566176471));
#153685=CARTESIAN_POINT('Ctrl Pts',(34.2237386972451,-37.5416529948095,
-414.687683823529));
#153686=CARTESIAN_POINT('Ctrl Pts',(30.744992244793,-40.7129494105307,-416.181801470588));
#153687=CARTESIAN_POINT('Ctrl Pts',(26.7427538741697,-43.1910304950644,
-417.675919117647));
#153688=CARTESIAN_POINT('Ctrl Pts',(22.7405155035463,-45.6691115795981,
-419.170036764706));
#153689=CARTESIAN_POINT('Ctrl Pts',(18.3510766423074,-47.3695892537413,
-420.664154411765));
#153690=CARTESIAN_POINT('Ctrl Pts',(13.9616377810684,-49.0700669278844,
-422.158272058824));
#153691=CARTESIAN_POINT('Ctrl Pts',(9.33447550508176,-49.9350334639422,
-423.652389705882));
#153692=CARTESIAN_POINT('Ctrl Pts',(4.70731322909511,-50.8,-425.146507352941));
#153693=CARTESIAN_POINT('Ctrl Pts',(0.,-50.8,-426.640625));
#153694=CARTESIAN_POINT('Ctrl Pts',(-4.70731322909511,-50.8,-428.134742647059));
#153695=CARTESIAN_POINT('Ctrl Pts',(-9.33447550508177,-49.9350334639422,
-429.628860294118));
#153696=CARTESIAN_POINT('Ctrl Pts',(-13.9616377810684,-49.0700669278844,
-431.122977941177));
#153697=CARTESIAN_POINT('Ctrl Pts',(-18.3510766423074,-47.3695892537413,
-432.617095588235));
#153698=CARTESIAN_POINT('Ctrl Pts',(-22.7405155035463,-45.6691115795981,
-434.111213235294));
#153699=CARTESIAN_POINT('Ctrl Pts',(-26.7427538741697,-43.1910304950644,
-435.605330882353));
#153700=CARTESIAN_POINT('Ctrl Pts',(-30.744992244793,-40.7129494105307,
-437.099448529412));
#153701=CARTESIAN_POINT('Ctrl Pts',(-34.2237386972451,-37.5416529948095,
-438.593566176471));
#153702=CARTESIAN_POINT('Ctrl Pts',(-37.7024851496972,-34.3703565790883,
-440.087683823529));
#153703=CARTESIAN_POINT('Ctrl Pts',(-40.5392751458362,-30.6138395280662,
-441.581801470588));
#153704=CARTESIAN_POINT('Ctrl Pts',(-43.3760651419751,-26.8573224770441,
-443.075919117647));
#153705=CARTESIAN_POINT('Ctrl Pts',(-45.4742952008371,-22.6435084734481,
-444.570036764706));
#153706=CARTESIAN_POINT('Ctrl Pts',(-47.5725252596992,-18.4296944698521,
-446.064154411765));
#153707=CARTESIAN_POINT('Ctrl Pts',(-48.8607426731792,-13.9020798956618,
-447.558272058824));
#153708=CARTESIAN_POINT('Ctrl Pts',(-50.1489600866593,-9.37446532147148,
-449.052389705882));
#153709=CARTESIAN_POINT('Ctrl Pts',(-50.5832961557877,-4.68723266073574,
-450.546507352941));
#153710=CARTESIAN_POINT('Ctrl Pts',(-51.0176322249162,-3.12392900021603E-15,
-452.040625));
#153711=CARTESIAN_POINT('Ctrl Pts',(-50.5832961557877,4.68723266073573,
-453.534742647059));
#153712=CARTESIAN_POINT('Ctrl Pts',(-50.1489600866593,9.37446532147149,
-455.028860294118));
#153713=CARTESIAN_POINT('Ctrl Pts',(-48.8607426731792,13.9020798956618,
-456.522977941176));
#153714=CARTESIAN_POINT('Ctrl Pts',(-47.5725252596992,18.4296944698521,
-458.017095588235));
#153715=CARTESIAN_POINT('Ctrl Pts',(-45.4742952008371,22.6435084734481,
-459.511213235294));
#153716=CARTESIAN_POINT('Ctrl Pts',(-43.3760651419751,26.8573224770442,
-461.005330882353));
#153717=CARTESIAN_POINT('Ctrl Pts',(-40.5392751458362,30.6138395280662,
-462.499448529412));
#153718=CARTESIAN_POINT('Ctrl Pts',(-37.7024851496972,34.3703565790883,
-463.993566176471));
#153719=CARTESIAN_POINT('Ctrl Pts',(-34.2237386972451,37.5416529948095,
-465.487683823529));
#153720=CARTESIAN_POINT('Ctrl Pts',(-30.744992244793,40.7129494105307,-466.981801470588));
#153721=CARTESIAN_POINT('Ctrl Pts',(-26.7427538741697,43.1910304950644,
-468.475919117647));
#153722=CARTESIAN_POINT('Ctrl Pts',(-22.7405155035463,45.6691115795981,
-469.970036764706));
#153723=CARTESIAN_POINT('Ctrl Pts',(-18.3510766423074,47.3695892537413,
-471.464154411765));
#153724=CARTESIAN_POINT('Ctrl Pts',(-13.9616377810684,49.0700669278844,
-472.958272058823));
#153725=CARTESIAN_POINT('Ctrl Pts',(-9.33447550508177,49.9350334639422,
-474.452389705882));
#153726=CARTESIAN_POINT('Ctrl Pts',(-4.7073132290951,50.8,-475.946507352941));
#153727=CARTESIAN_POINT('Ctrl Pts',(-6.22120573966855E-15,50.8,-477.440625));
#153728=CARTESIAN_POINT('Ctrl Pts',(4.70731322909511,50.8,-478.934742647059));
#153729=CARTESIAN_POINT('Ctrl Pts',(9.33447550508176,49.9350334639422,-480.428860294118));
#153730=CARTESIAN_POINT('Ctrl Pts',(13.9616377810684,49.0700669278844,-481.922977941177));
#153731=CARTESIAN_POINT('Ctrl Pts',(18.3510766423074,47.3695892537413,-483.417095588235));
#153732=CARTESIAN_POINT('Ctrl Pts',(22.7405155035463,45.6691115795981,-484.911213235294));
#153733=CARTESIAN_POINT('Ctrl Pts',(26.7427538741697,43.1910304950644,-486.405330882353));
#153734=CARTESIAN_POINT('Ctrl Pts',(30.744992244793,40.7129494105307,-487.899448529412));
#153735=CARTESIAN_POINT('Ctrl Pts',(34.2237386972451,37.5416529948095,-489.393566176471));
#153736=CARTESIAN_POINT('Ctrl Pts',(37.7024851496972,34.3703565790883,-490.88768382353));
#153737=CARTESIAN_POINT('Ctrl Pts',(40.5392751458362,30.6138395280662,-492.381801470588));
#153738=CARTESIAN_POINT('Ctrl Pts',(43.3760651419751,26.8573224770442,-493.875919117647));
#153739=CARTESIAN_POINT('Ctrl Pts',(45.4742952008372,22.6435084734481,-495.370036764706));
#153740=CARTESIAN_POINT('Ctrl Pts',(47.5725252596992,18.4296944698521,-496.864154411765));
#153741=CARTESIAN_POINT('Ctrl Pts',(48.8607426731792,13.9020798956618,-498.358272058824));
#153742=CARTESIAN_POINT('Ctrl Pts',(50.1489600866593,9.37446532147146,-499.852389705883));
#153743=CARTESIAN_POINT('Ctrl Pts',(50.5832961557877,4.68723266073574,-501.346507352941));
#153744=CARTESIAN_POINT('Ctrl Pts',(51.0176322249162,9.37178700064808E-15,
-502.840625));
#153745=CARTESIAN_POINT('Ctrl Pts',(50.5832961557877,-4.68723266073572,
-504.334742647059));
#153746=CARTESIAN_POINT('Ctrl Pts',(50.1489600866593,-9.37446532147149,
-505.828860294118));
#153747=CARTESIAN_POINT('Ctrl Pts',(48.8607426731792,-13.9020798956618,
-507.322977941176));
#153748=CARTESIAN_POINT('Ctrl Pts',(47.5725252596992,-18.4296944698521,
-508.817095588235));
#153749=CARTESIAN_POINT('Ctrl Pts',(45.4742952008371,-22.6435084734482,
-510.311213235294));
#153750=CARTESIAN_POINT('Ctrl Pts',(43.3760651419751,-26.8573224770441,
-511.805330882353));
#153751=CARTESIAN_POINT('Ctrl Pts',(40.5392751458362,-30.6138395280662,
-513.299448529412));
#153752=CARTESIAN_POINT('Ctrl Pts',(37.7024851496972,-34.3703565790883,
-514.793566176471));
#153753=CARTESIAN_POINT('Ctrl Pts',(34.2237386972451,-37.5416529948095,
-516.28768382353));
#153754=CARTESIAN_POINT('Ctrl Pts',(30.744992244793,-40.7129494105307,-517.781801470588));
#153755=CARTESIAN_POINT('Ctrl Pts',(26.7427538741697,-43.1910304950644,
-519.275919117647));
#153756=CARTESIAN_POINT('Ctrl Pts',(22.7405155035463,-45.6691115795981,
-520.770036764706));
#153757=CARTESIAN_POINT('Ctrl Pts',(18.3510766423074,-47.3695892537413,
-522.264154411765));
#153758=CARTESIAN_POINT('Ctrl Pts',(13.9616377810684,-49.0700669278844,
-523.758272058823));
#153759=CARTESIAN_POINT('Ctrl Pts',(9.33447550508176,-49.9350334639422,
-525.252389705882));
#153760=CARTESIAN_POINT('Ctrl Pts',(4.70731322909511,-50.8,-526.746507352941));
#153761=CARTESIAN_POINT('Ctrl Pts',(0.,-50.8,-528.240625));
#153762=CARTESIAN_POINT('Ctrl Pts',(-4.70731322909511,-50.8,-529.734742647059));
#153763=CARTESIAN_POINT('Ctrl Pts',(-9.33447550508177,-49.9350334639422,
-531.228860294118));
#153764=CARTESIAN_POINT('Ctrl Pts',(-13.9616377810684,-49.0700669278844,
-532.722977941177));
#153765=CARTESIAN_POINT('Ctrl Pts',(-18.3510766423074,-47.3695892537413,
-534.217095588235));
#153766=CARTESIAN_POINT('Ctrl Pts',(-22.7405155035463,-45.6691115795981,
-535.711213235294));
#153767=CARTESIAN_POINT('Ctrl Pts',(-26.7427538741697,-43.1910304950644,
-537.205330882353));
#153768=CARTESIAN_POINT('Ctrl Pts',(-30.744992244793,-40.7129494105307,
-538.699448529412));
#153769=CARTESIAN_POINT('Ctrl Pts',(-34.2237386972451,-37.5416529948095,
-540.193566176471));
#153770=CARTESIAN_POINT('Ctrl Pts',(-37.7024851496972,-34.3703565790883,
-541.687683823529));
#153771=CARTESIAN_POINT('Ctrl Pts',(-40.5392751458362,-30.6138395280662,
-543.181801470588));
#153772=CARTESIAN_POINT('Ctrl Pts',(-43.3760651419751,-26.8573224770441,
-544.675919117647));
#153773=CARTESIAN_POINT('Ctrl Pts',(-45.4742952008371,-22.6435084734481,
-546.170036764706));
#153774=CARTESIAN_POINT('Ctrl Pts',(-47.5725252596992,-18.4296944698521,
-547.664154411765));
#153775=CARTESIAN_POINT('Ctrl Pts',(-48.8607426731792,-13.9020798956618,
-549.158272058823));
#153776=CARTESIAN_POINT('Ctrl Pts',(-50.1489600866593,-9.37446532147148,
-550.652389705882));
#153777=CARTESIAN_POINT('Ctrl Pts',(-50.5832961557877,-4.68723266073574,
-552.146507352941));
#153778=CARTESIAN_POINT('Ctrl Pts',(-51.0176322249162,-3.12392900021603E-15,
-553.640625));
#153779=CARTESIAN_POINT('Ctrl Pts',(-50.5832961557877,4.68723266073573,
-555.134742647059));
#153780=CARTESIAN_POINT('Ctrl Pts',(-50.1489600866593,9.37446532147149,
-556.628860294118));
#153781=CARTESIAN_POINT('Ctrl Pts',(-48.8607426731792,13.9020798956618,
-558.122977941176));
#153782=CARTESIAN_POINT('Ctrl Pts',(-47.5725252596992,18.4296944698521,
-559.617095588235));
#153783=CARTESIAN_POINT('Ctrl Pts',(-45.4742952008371,22.6435084734481,
-561.111213235294));
#153784=CARTESIAN_POINT('Ctrl Pts',(-43.3760651419751,26.8573224770442,
-562.605330882353));
#153785=CARTESIAN_POINT('Ctrl Pts',(-40.5392751458362,30.6138395280662,
-564.099448529412));
#153786=CARTESIAN_POINT('Ctrl Pts',(-37.7024851496972,34.3703565790883,
-565.593566176471));
#153787=CARTESIAN_POINT('Ctrl Pts',(-34.2237386972451,37.5416529948095,
-567.087683823529));
#153788=CARTESIAN_POINT('Ctrl Pts',(-30.744992244793,40.7129494105307,-568.581801470588));
#153789=CARTESIAN_POINT('Ctrl Pts',(-26.7427538741697,43.1910304950644,
-570.075919117647));
#153790=CARTESIAN_POINT('Ctrl Pts',(-22.7405155035463,45.6691115795981,
-571.570036764706));
#153791=CARTESIAN_POINT('Ctrl Pts',(-18.3510766423074,47.3695892537413,
-573.064154411765));
#153792=CARTESIAN_POINT('Ctrl Pts',(-13.9616377810684,49.0700669278844,
-574.558272058824));
#153793=CARTESIAN_POINT('Ctrl Pts',(-9.33447550508177,49.9350334639422,
-576.052389705882));
#153794=CARTESIAN_POINT('Ctrl Pts',(-4.7073132290951,50.8,-577.546507352941));
#153795=CARTESIAN_POINT('Ctrl Pts',(-6.22120573966855E-15,50.8,-579.040625));
#153796=CARTESIAN_POINT('Ctrl Pts',(4.70731322909511,50.8,-580.534742647059));
#153797=CARTESIAN_POINT('Ctrl Pts',(9.33447550508176,49.9350334639422,-582.028860294118));
#153798=CARTESIAN_POINT('Ctrl Pts',(13.9616377810684,49.0700669278844,-583.522977941176));
#153799=CARTESIAN_POINT('Ctrl Pts',(18.3510766423074,47.3695892537413,-585.017095588235));
#153800=CARTESIAN_POINT('Ctrl Pts',(22.7405155035463,45.6691115795981,-586.511213235294));
#153801=CARTESIAN_POINT('Ctrl Pts',(26.7427538741697,43.1910304950644,-588.005330882353));
#153802=CARTESIAN_POINT('Ctrl Pts',(30.744992244793,40.7129494105307,-589.499448529412));
#153803=CARTESIAN_POINT('Ctrl Pts',(34.2237386972451,37.5416529948095,-590.993566176471));
#153804=CARTESIAN_POINT('Ctrl Pts',(37.7024851496972,34.3703565790883,-592.48768382353));
#153805=CARTESIAN_POINT('Ctrl Pts',(40.5392751458362,30.6138395280662,-593.981801470588));
#153806=CARTESIAN_POINT('Ctrl Pts',(43.3760651419751,26.8573224770442,-595.475919117647));
#153807=CARTESIAN_POINT('Ctrl Pts',(45.4742952008372,22.6435084734481,-596.970036764706));
#153808=CARTESIAN_POINT('Ctrl Pts',(47.5725252596992,18.4296944698521,-598.464154411765));
#153809=CARTESIAN_POINT('Ctrl Pts',(48.8607426731792,13.9020798956618,-599.958272058823));
#153810=CARTESIAN_POINT('Ctrl Pts',(50.1489600866593,9.37446532147146,-601.452389705883));
#153811=CARTESIAN_POINT('Ctrl Pts',(50.5832961557877,4.68723266073574,-602.946507352941));
#153812=CARTESIAN_POINT('Ctrl Pts',(51.0176322249162,9.37178700064808E-15,
-604.440625));
#153813=CARTESIAN_POINT('Ctrl Pts',(50.5832961557877,-4.68723266073572,
-605.934742647059));
#153814=CARTESIAN_POINT('Ctrl Pts',(50.1489600866593,-9.37446532147149,
-607.428860294118));
#153815=CARTESIAN_POINT('Ctrl Pts',(48.8607426731792,-13.9020798956618,
-608.922977941176));
#153816=CARTESIAN_POINT('Ctrl Pts',(47.5725252596992,-18.4296944698521,
-610.417095588235));
#153817=CARTESIAN_POINT('Ctrl Pts',(45.4742952008371,-22.6435084734482,
-611.911213235294));
#153818=CARTESIAN_POINT('Ctrl Pts',(43.3760651419751,-26.8573224770441,
-613.405330882353));
#153819=CARTESIAN_POINT('Ctrl Pts',(40.5392751458362,-30.6138395280662,
-614.899448529412));
#153820=CARTESIAN_POINT('Ctrl Pts',(37.7024851496972,-34.3703565790883,
-616.393566176471));
#153821=CARTESIAN_POINT('Ctrl Pts',(34.2237386972451,-37.5416529948095,
-617.887683823529));
#153822=CARTESIAN_POINT('Ctrl Pts',(30.744992244793,-40.7129494105307,-619.381801470588));
#153823=CARTESIAN_POINT('Ctrl Pts',(26.7427538741697,-43.1910304950644,
-620.875919117647));
#153824=CARTESIAN_POINT('Ctrl Pts',(22.7405155035463,-45.6691115795981,
-622.370036764706));
#153825=CARTESIAN_POINT('Ctrl Pts',(18.3510766423074,-47.3695892537413,
-623.864154411765));
#153826=CARTESIAN_POINT('Ctrl Pts',(13.9616377810684,-49.0700669278844,
-625.358272058823));
#153827=CARTESIAN_POINT('Ctrl Pts',(9.33447550508176,-49.9350334639422,
-626.852389705882));
#153828=CARTESIAN_POINT('Ctrl Pts',(4.70731322909511,-50.8,-628.346507352941));
#153829=CARTESIAN_POINT('Ctrl Pts',(0.,-50.8,-629.840625));
#153830=CARTESIAN_POINT('Ctrl Pts',(-4.70731322909511,-50.8,-631.334742647059));
#153831=CARTESIAN_POINT('Ctrl Pts',(-9.33447550508177,-49.9350334639422,
-632.828860294118));
#153832=CARTESIAN_POINT('Ctrl Pts',(-13.9616377810684,-49.0700669278844,
-634.322977941177));
#153833=CARTESIAN_POINT('Ctrl Pts',(-18.3510766423074,-47.3695892537413,
-635.817095588235));
#153834=CARTESIAN_POINT('Ctrl Pts',(-22.7405155035463,-45.6691115795981,
-637.311213235294));
#153835=CARTESIAN_POINT('Ctrl Pts',(-26.7427538741697,-43.1910304950644,
-638.805330882353));
#153836=CARTESIAN_POINT('Ctrl Pts',(-30.744992244793,-40.7129494105307,
-640.299448529412));
#153837=CARTESIAN_POINT('Ctrl Pts',(-34.2237386972451,-37.5416529948095,
-641.79356617647));
#153838=CARTESIAN_POINT('Ctrl Pts',(-37.7024851496972,-34.3703565790883,
-643.287683823529));
#153839=CARTESIAN_POINT('Ctrl Pts',(-40.5392751458362,-30.6138395280662,
-644.781801470588));
#153840=CARTESIAN_POINT('Ctrl Pts',(-43.3760651419751,-26.8573224770441,
-646.275919117647));
#153841=CARTESIAN_POINT('Ctrl Pts',(-45.4742952008371,-22.6435084734481,
-647.770036764706));
#153842=CARTESIAN_POINT('Ctrl Pts',(-47.5725252596992,-18.4296944698521,
-649.264154411765));
#153843=CARTESIAN_POINT('Ctrl Pts',(-48.8607426731792,-13.9020798956618,
-650.758272058824));
#153844=CARTESIAN_POINT('Ctrl Pts',(-50.1489600866593,-9.37446532147148,
-652.252389705883));
#153845=CARTESIAN_POINT('Ctrl Pts',(-50.5832961557877,-4.68723266073574,
-653.746507352941));
#153846=CARTESIAN_POINT('Ctrl Pts',(-51.0176322249162,-3.12392900021603E-15,
-655.240625));
#153847=CARTESIAN_POINT('Ctrl Pts',(-50.5832961557877,4.68723266073573,
-656.734742647059));
#153848=CARTESIAN_POINT('Ctrl Pts',(-50.1489600866593,9.37446532147149,
-658.228860294118));
#153849=CARTESIAN_POINT('Ctrl Pts',(-48.8607426731792,13.9020798956618,
-659.722977941176));
#153850=CARTESIAN_POINT('Ctrl Pts',(-47.5725252596992,18.4296944698521,
-661.217095588236));
#153851=CARTESIAN_POINT('Ctrl Pts',(-45.4742952008371,22.6435084734481,
-662.711213235294));
#153852=CARTESIAN_POINT('Ctrl Pts',(-43.3760651419751,26.8573224770442,
-664.205330882353));
#153853=CARTESIAN_POINT('Ctrl Pts',(-40.5392751458362,30.6138395280662,
-665.699448529412));
#153854=CARTESIAN_POINT('Ctrl Pts',(-37.7024851496972,34.3703565790883,
-667.193566176471));
#153855=CARTESIAN_POINT('Ctrl Pts',(-34.2237386972451,37.5416529948095,
-668.687683823529));
#153856=CARTESIAN_POINT('Ctrl Pts',(-30.744992244793,40.7129494105307,-670.181801470588));
#153857=CARTESIAN_POINT('Ctrl Pts',(-26.7427538741697,43.1910304950644,
-671.675919117647));
#153858=CARTESIAN_POINT('Ctrl Pts',(-22.7405155035463,45.6691115795981,
-673.170036764706));
#153859=CARTESIAN_POINT('Ctrl Pts',(-18.3510766423074,47.3695892537413,
-674.664154411765));
#153860=CARTESIAN_POINT('Ctrl Pts',(-13.9616377810684,49.0700669278844,
-676.158272058824));
#153861=CARTESIAN_POINT('Ctrl Pts',(-9.33447550508177,49.9350334639422,
-677.652389705882));
#153862=CARTESIAN_POINT('Ctrl Pts',(-4.7073132290951,50.8,-679.146507352941));
#153863=CARTESIAN_POINT('Ctrl Pts',(-6.22120573966855E-15,50.8,-680.640625));
#153864=CARTESIAN_POINT('Ctrl Pts',(4.70731322909511,50.8,-682.134742647059));
#153865=CARTESIAN_POINT('Ctrl Pts',(9.33447550508176,49.9350334639422,-683.628860294117));
#153866=CARTESIAN_POINT('Ctrl Pts',(13.9616377810684,49.0700669278844,-685.122977941176));
#153867=CARTESIAN_POINT('Ctrl Pts',(18.3510766423074,47.3695892537413,-686.617095588235));
#153868=CARTESIAN_POINT('Ctrl Pts',(22.7405155035463,45.6691115795981,-688.111213235294));
#153869=CARTESIAN_POINT('Ctrl Pts',(26.7427538741697,43.1910304950644,-689.605330882353));
#153870=CARTESIAN_POINT('Ctrl Pts',(30.744992244793,40.7129494105307,-691.099448529412));
#153871=CARTESIAN_POINT('Ctrl Pts',(34.2237386972451,37.5416529948095,-692.593566176471));
#153872=CARTESIAN_POINT('Ctrl Pts',(37.7024851496972,34.3703565790883,-694.087683823529));
#153873=CARTESIAN_POINT('Ctrl Pts',(40.5392751458362,30.6138395280662,-695.581801470588));
#153874=CARTESIAN_POINT('Ctrl Pts',(43.3760651419751,26.8573224770442,-697.075919117647));
#153875=CARTESIAN_POINT('Ctrl Pts',(45.4742952008372,22.6435084734481,-698.570036764706));
#153876=CARTESIAN_POINT('Ctrl Pts',(47.5725252596992,18.4296944698521,-700.064154411765));
#153877=CARTESIAN_POINT('Ctrl Pts',(48.8607426731792,13.9020798956618,-701.558272058823));
#153878=CARTESIAN_POINT('Ctrl Pts',(50.1489600866593,9.37446532147146,-703.052389705882));
#153879=CARTESIAN_POINT('Ctrl Pts',(50.5832961557877,4.68723266073574,-704.546507352941));
#153880=CARTESIAN_POINT('Ctrl Pts',(51.0176322249162,9.37178700064808E-15,
-706.040625));
#153881=CARTESIAN_POINT('Ctrl Pts',(50.5832961557877,-4.68723266073572,
-707.534742647059));
#153882=CARTESIAN_POINT('Ctrl Pts',(50.1489600866593,-9.37446532147149,
-709.028860294118));
#153883=CARTESIAN_POINT('Ctrl Pts',(48.8607426731792,-13.9020798956618,
-710.522977941177));
#153884=CARTESIAN_POINT('Ctrl Pts',(47.5725252596992,-18.4296944698521,
-712.017095588236));
#153885=CARTESIAN_POINT('Ctrl Pts',(45.4742952008371,-22.6435084734482,
-713.511213235294));
#153886=CARTESIAN_POINT('Ctrl Pts',(43.3760651419751,-26.8573224770441,
-715.005330882353));
#153887=CARTESIAN_POINT('Ctrl Pts',(40.5392751458362,-30.6138395280662,
-716.499448529412));
#153888=CARTESIAN_POINT('Ctrl Pts',(37.7024851496972,-34.3703565790883,
-717.99356617647));
#153889=CARTESIAN_POINT('Ctrl Pts',(34.2237386972451,-37.5416529948095,
-719.487683823529));
#153890=CARTESIAN_POINT('Ctrl Pts',(30.744992244793,-40.7129494105307,-720.981801470588));
#153891=CARTESIAN_POINT('Ctrl Pts',(26.7427538741697,-43.1910304950644,
-722.475919117647));
#153892=CARTESIAN_POINT('Ctrl Pts',(22.7405155035463,-45.6691115795981,
-723.970036764706));
#153893=CARTESIAN_POINT('Ctrl Pts',(18.3510766423074,-47.3695892537413,
-725.464154411765));
#153894=CARTESIAN_POINT('Ctrl Pts',(13.9616377810684,-49.0700669278844,
-726.958272058824));
#153895=CARTESIAN_POINT('Ctrl Pts',(9.33447550508176,-49.9350334639422,
-728.452389705882));
#153896=CARTESIAN_POINT('Ctrl Pts',(4.70731322909511,-50.8,-729.946507352941));
#153897=CARTESIAN_POINT('Ctrl Pts',(0.,-50.8,-731.440625));
#153898=CARTESIAN_POINT('Ctrl Pts',(-4.70731322909511,-50.8,-732.934742647059));
#153899=CARTESIAN_POINT('Ctrl Pts',(-9.33447550508177,-49.9350334639422,
-734.428860294118));
#153900=CARTESIAN_POINT('Ctrl Pts',(-13.9616377810684,-49.0700669278844,
-735.922977941176));
#153901=CARTESIAN_POINT('Ctrl Pts',(-18.3510766423074,-47.3695892537413,
-737.417095588235));
#153902=CARTESIAN_POINT('Ctrl Pts',(-22.7405155035463,-45.6691115795981,
-738.911213235294));
#153903=CARTESIAN_POINT('Ctrl Pts',(-26.7427538741697,-43.1910304950644,
-740.405330882353));
#153904=CARTESIAN_POINT('Ctrl Pts',(-30.744992244793,-40.7129494105307,
-741.899448529412));
#153905=CARTESIAN_POINT('Ctrl Pts',(-34.2237386972451,-37.5416529948095,
-743.39356617647));
#153906=CARTESIAN_POINT('Ctrl Pts',(-37.7024851496972,-34.3703565790883,
-744.887683823529));
#153907=CARTESIAN_POINT('Ctrl Pts',(-40.5392751458362,-30.6138395280662,
-746.381801470588));
#153908=CARTESIAN_POINT('Ctrl Pts',(-43.3760651419751,-26.8573224770441,
-747.875919117647));
#153909=CARTESIAN_POINT('Ctrl Pts',(-45.4742952008371,-22.6435084734481,
-749.370036764706));
#153910=CARTESIAN_POINT('Ctrl Pts',(-47.5725252596992,-18.4296944698521,
-750.864154411765));
#153911=CARTESIAN_POINT('Ctrl Pts',(-48.8607426731792,-13.9020798956618,
-752.358272058824));
#153912=CARTESIAN_POINT('Ctrl Pts',(-50.1489600866593,-9.37446532147148,
-753.852389705883));
#153913=CARTESIAN_POINT('Ctrl Pts',(-50.5832961557877,-4.68723266073574,
-755.346507352941));
#153914=CARTESIAN_POINT('Ctrl Pts',(-51.0176322249162,-3.12392900021603E-15,
-756.840625));
#153915=CARTESIAN_POINT('Ctrl Pts',(-50.5832961557877,4.68723266073573,
-758.334742647059));
#153916=CARTESIAN_POINT('Ctrl Pts',(-50.1489600866593,9.37446532147149,
-759.828860294117));
#153917=CARTESIAN_POINT('Ctrl Pts',(-48.8607426731792,13.9020798956618,
-761.322977941176));
#153918=CARTESIAN_POINT('Ctrl Pts',(-47.5725252596992,18.4296944698521,
-762.817095588235));
#153919=CARTESIAN_POINT('Ctrl Pts',(-45.4742952008371,22.6435084734481,
-764.311213235294));
#153920=CARTESIAN_POINT('Ctrl Pts',(-43.3760651419751,26.8573224770442,
-765.805330882353));
#153921=CARTESIAN_POINT('Ctrl Pts',(-40.5392751458362,30.6138395280662,
-767.299448529412));
#153922=CARTESIAN_POINT('Ctrl Pts',(-37.7024851496972,34.3703565790883,
-768.793566176471));
#153923=CARTESIAN_POINT('Ctrl Pts',(-34.2237386972451,37.5416529948095,
-770.28768382353));
#153924=CARTESIAN_POINT('Ctrl Pts',(-30.744992244793,40.7129494105307,-771.781801470589));
#153925=CARTESIAN_POINT('Ctrl Pts',(-26.7427538741697,43.1910304950644,
-773.275919117647));
#153926=CARTESIAN_POINT('Ctrl Pts',(-22.7405155035463,45.6691115795981,
-774.770036764706));
#153927=CARTESIAN_POINT('Ctrl Pts',(-18.3510766423074,47.3695892537413,
-776.264154411765));
#153928=CARTESIAN_POINT('Ctrl Pts',(-13.9616377810684,49.0700669278844,
-777.758272058824));
#153929=CARTESIAN_POINT('Ctrl Pts',(-9.33447550508177,49.9350334639422,
-779.252389705882));
#153930=CARTESIAN_POINT('Ctrl Pts',(-4.7073132290951,50.8,-780.746507352941));
#153931=CARTESIAN_POINT('Ctrl Pts',(-6.22120573966855E-15,50.8,-782.240625));
#153932=CARTESIAN_POINT('Ctrl Pts',(4.70731322909511,50.8,-783.734742647059));
#153933=CARTESIAN_POINT('Ctrl Pts',(9.33447550508176,49.9350334639422,-785.228860294118));
#153934=CARTESIAN_POINT('Ctrl Pts',(13.9616377810684,49.0700669278844,-786.722977941177));
#153935=CARTESIAN_POINT('Ctrl Pts',(18.3510766423074,47.3695892537413,-788.217095588235));
#153936=CARTESIAN_POINT('Ctrl Pts',(22.7405155035463,45.6691115795981,-789.711213235294));
#153937=CARTESIAN_POINT('Ctrl Pts',(26.7427538741697,43.1910304950644,-791.205330882353));
#153938=CARTESIAN_POINT('Ctrl Pts',(30.744992244793,40.7129494105307,-792.699448529412));
#153939=CARTESIAN_POINT('Ctrl Pts',(34.2237386972451,37.5416529948095,-794.193566176471));
#153940=CARTESIAN_POINT('Ctrl Pts',(37.7024851496972,34.3703565790883,-795.687683823529));
#153941=CARTESIAN_POINT('Ctrl Pts',(40.5392751458362,30.6138395280662,-797.181801470588));
#153942=CARTESIAN_POINT('Ctrl Pts',(43.3760651419751,26.8573224770442,-798.675919117647));
#153943=CARTESIAN_POINT('Ctrl Pts',(45.4742952008372,22.6435084734481,-800.170036764706));
#153944=CARTESIAN_POINT('Ctrl Pts',(47.5725252596992,18.4296944698521,-801.664154411765));
#153945=CARTESIAN_POINT('Ctrl Pts',(48.8607426731792,13.9020798956618,-803.158272058823));
#153946=CARTESIAN_POINT('Ctrl Pts',(50.1489600866593,9.37446532147146,-804.652389705882));
#153947=CARTESIAN_POINT('Ctrl Pts',(50.5832961557877,4.68723266073574,-806.146507352941));
#153948=CARTESIAN_POINT('Ctrl Pts',(51.0176322249162,9.37178700064808E-15,
-807.640625));
#153949=CARTESIAN_POINT('Ctrl Pts',(50.5832961557877,-4.68723266073572,
-809.134742647059));
#153950=CARTESIAN_POINT('Ctrl Pts',(50.1489600866593,-9.37446532147149,
-810.628860294118));
#153951=CARTESIAN_POINT('Ctrl Pts',(48.8607426731792,-13.9020798956618,
-812.122977941177));
#153952=CARTESIAN_POINT('Ctrl Pts',(47.5725252596992,-18.4296944698521,
-813.617095588236));
#153953=CARTESIAN_POINT('Ctrl Pts',(45.4742952008371,-22.6435084734482,
-815.111213235294));
#153954=CARTESIAN_POINT('Ctrl Pts',(43.3760651419751,-26.8573224770441,
-816.605330882353));
#153955=CARTESIAN_POINT('Ctrl Pts',(40.5392751458362,-30.6138395280662,
-818.099448529412));
#153956=CARTESIAN_POINT('Ctrl Pts',(37.7024851496972,-34.3703565790883,
-819.59356617647));
#153957=CARTESIAN_POINT('Ctrl Pts',(34.2237386972451,-37.5416529948095,
-821.087683823529));
#153958=CARTESIAN_POINT('Ctrl Pts',(30.744992244793,-40.7129494105307,-822.581801470588));
#153959=CARTESIAN_POINT('Ctrl Pts',(26.7427538741697,-43.1910304950644,
-824.075919117647));
#153960=CARTESIAN_POINT('Ctrl Pts',(22.7405155035463,-45.6691115795981,
-825.570036764706));
#153961=CARTESIAN_POINT('Ctrl Pts',(18.3510766423074,-47.3695892537413,
-827.064154411765));
#153962=CARTESIAN_POINT('Ctrl Pts',(13.9616377810684,-49.0700669278844,
-828.558272058824));
#153963=CARTESIAN_POINT('Ctrl Pts',(9.33447550508176,-49.9350334639422,
-830.052389705883));
#153964=CARTESIAN_POINT('Ctrl Pts',(4.70731322909511,-50.8,-831.546507352941));
#153965=CARTESIAN_POINT('Ctrl Pts',(0.,-50.8,-833.040625));
#153966=CARTESIAN_POINT('Ctrl Pts',(-4.70731322909511,-50.8,-834.534742647059));
#153967=CARTESIAN_POINT('Ctrl Pts',(-9.33447550508177,-49.9350334639422,
-836.028860294118));
#153968=CARTESIAN_POINT('Ctrl Pts',(-13.9616377810684,-49.0700669278844,
-837.522977941177));
#153969=CARTESIAN_POINT('Ctrl Pts',(-18.3510766423074,-47.3695892537413,
-839.017095588235));
#153970=CARTESIAN_POINT('Ctrl Pts',(-22.7405155035463,-45.6691115795981,
-840.511213235294));
#153971=CARTESIAN_POINT('Ctrl Pts',(-26.7427538741697,-43.1910304950644,
-842.005330882353));
#153972=CARTESIAN_POINT('Ctrl Pts',(-30.744992244793,-40.7129494105307,
-843.499448529412));
#153973=CARTESIAN_POINT('Ctrl Pts',(-34.2237386972451,-37.5416529948095,
-844.993566176471));
#153974=CARTESIAN_POINT('Ctrl Pts',(-37.7024851496972,-34.3703565790883,
-846.48768382353));
#153975=CARTESIAN_POINT('Ctrl Pts',(-40.5392751458362,-30.6138395280662,
-847.981801470588));
#153976=CARTESIAN_POINT('Ctrl Pts',(-43.3760651419751,-26.8573224770441,
-849.475919117647));
#153977=CARTESIAN_POINT('Ctrl Pts',(-45.4742952008371,-22.6435084734481,
-850.970036764706));
#153978=CARTESIAN_POINT('Ctrl Pts',(-47.5725252596992,-18.4296944698521,
-852.464154411765));
#153979=CARTESIAN_POINT('Ctrl Pts',(-48.8607426731792,-13.9020798956618,
-853.958272058824));
#153980=CARTESIAN_POINT('Ctrl Pts',(-50.1489600866593,-9.37446532147148,
-855.452389705882));
#153981=CARTESIAN_POINT('Ctrl Pts',(-50.5832961557877,-4.68723266073574,
-856.946507352941));
#153982=CARTESIAN_POINT('Ctrl Pts',(-51.0176322249162,-3.12392900021603E-15,
-858.440625));
#153983=CARTESIAN_POINT('Ctrl Pts',(-50.5832961557877,4.68723266073573,
-859.934742647059));
#153984=CARTESIAN_POINT('Ctrl Pts',(-50.1489600866593,9.37446532147149,
-861.428860294118));
#153985=CARTESIAN_POINT('Ctrl Pts',(-48.8607426731792,13.9020798956618,
-862.922977941176));
#153986=CARTESIAN_POINT('Ctrl Pts',(-47.5725252596992,18.4296944698521,
-864.417095588235));
#153987=CARTESIAN_POINT('Ctrl Pts',(-45.4742952008371,22.6435084734481,
-865.911213235294));
#153988=CARTESIAN_POINT('Ctrl Pts',(-43.3760651419751,26.8573224770442,
-867.405330882353));
#153989=CARTESIAN_POINT('Ctrl Pts',(-40.5392751458362,30.6138395280662,
-868.899448529412));
#153990=CARTESIAN_POINT('Ctrl Pts',(-37.7024851496972,34.3703565790883,
-870.393566176471));
#153991=CARTESIAN_POINT('Ctrl Pts',(-34.2237386972451,37.5416529948095,
-871.887683823529));
#153992=CARTESIAN_POINT('Ctrl Pts',(-30.744992244793,40.7129494105307,-873.381801470588));
#153993=CARTESIAN_POINT('Ctrl Pts',(-26.7427538741697,43.1910304950644,
-874.875919117647));
#153994=CARTESIAN_POINT('Ctrl Pts',(-22.7405155035463,45.6691115795981,
-876.370036764706));
#153995=CARTESIAN_POINT('Ctrl Pts',(-18.3510766423074,47.3695892537413,
-877.864154411765));
#153996=CARTESIAN_POINT('Ctrl Pts',(-13.9616377810684,49.0700669278844,
-879.358272058823));
#153997=CARTESIAN_POINT('Ctrl Pts',(-9.33447550508177,49.9350334639422,
-880.852389705882));
#153998=CARTESIAN_POINT('Ctrl Pts',(-4.7073132290951,50.8,-882.346507352941));
#153999=CARTESIAN_POINT('Ctrl Pts',(-6.22120573966855E-15,50.8,-883.840625));
#154000=CARTESIAN_POINT('Ctrl Pts',(4.70731322909511,50.8,-885.334742647059));
#154001=CARTESIAN_POINT('Ctrl Pts',(9.33447550508176,49.9350334639422,-886.828860294118));
#154002=CARTESIAN_POINT('Ctrl Pts',(13.9616377810684,49.0700669278844,-888.322977941177));
#154003=CARTESIAN_POINT('Ctrl Pts',(18.3510766423074,47.3695892537413,-889.817095588235));
#154004=CARTESIAN_POINT('Ctrl Pts',(22.7405155035463,45.6691115795981,-891.311213235294));
#154005=CARTESIAN_POINT('Ctrl Pts',(26.7427538741697,43.1910304950644,-892.805330882353));
#154006=CARTESIAN_POINT('Ctrl Pts',(30.744992244793,40.7129494105307,-894.299448529412));
#154007=CARTESIAN_POINT('Ctrl Pts',(34.2237386972451,37.5416529948095,-895.79356617647));
#154008=CARTESIAN_POINT('Ctrl Pts',(37.7024851496972,34.3703565790883,-897.287683823529));
#154009=CARTESIAN_POINT('Ctrl Pts',(40.5392751458362,30.6138395280662,-898.781801470588));
#154010=CARTESIAN_POINT('Ctrl Pts',(43.3760651419751,26.8573224770442,-900.275919117647));
#154011=CARTESIAN_POINT('Ctrl Pts',(45.4742952008372,22.6435084734481,-901.770036764706));
#154012=CARTESIAN_POINT('Ctrl Pts',(47.5725252596992,18.4296944698521,-903.264154411765));
#154013=CARTESIAN_POINT('Ctrl Pts',(48.8607426731792,13.9020798956618,-904.758272058824));
#154014=CARTESIAN_POINT('Ctrl Pts',(50.1489600866593,9.37446532147146,-906.252389705883));
#154015=CARTESIAN_POINT('Ctrl Pts',(50.5832961557877,4.68723266073574,-907.746507352941));
#154016=CARTESIAN_POINT('Ctrl Pts',(51.0176322249162,9.37178700064808E-15,
-909.240625));
#154017=CARTESIAN_POINT('Ctrl Pts',(50.5832961557877,-4.68723266073572,
-910.734742647059));
#154018=CARTESIAN_POINT('Ctrl Pts',(50.1489600866593,-9.37446532147149,
-912.228860294118));
#154019=CARTESIAN_POINT('Ctrl Pts',(48.8607426731792,-13.9020798956618,
-913.722977941176));
#154020=CARTESIAN_POINT('Ctrl Pts',(47.5725252596992,-18.4296944698521,
-915.217095588235));
#154021=CARTESIAN_POINT('Ctrl Pts',(45.4742952008371,-22.6435084734482,
-916.711213235294));
#154022=CARTESIAN_POINT('Ctrl Pts',(43.3760651419751,-26.8573224770441,
-918.205330882353));
#154023=CARTESIAN_POINT('Ctrl Pts',(40.5392751458362,-30.6138395280662,
-919.699448529412));
#154024=CARTESIAN_POINT('Ctrl Pts',(37.7024851496972,-34.3703565790883,
-921.193566176471));
#154025=CARTESIAN_POINT('Ctrl Pts',(34.2237386972451,-37.5416529948095,
-922.687683823529));
#154026=CARTESIAN_POINT('Ctrl Pts',(30.744992244793,-40.7129494105307,-924.181801470588));
#154027=CARTESIAN_POINT('Ctrl Pts',(26.7427538741697,-43.1910304950644,
-925.675919117647));
#154028=CARTESIAN_POINT('Ctrl Pts',(22.7405155035463,-45.6691115795981,
-927.170036764706));
#154029=CARTESIAN_POINT('Ctrl Pts',(18.3510766423074,-47.3695892537413,
-928.664154411765));
#154030=CARTESIAN_POINT('Ctrl Pts',(13.9616377810684,-49.0700669278844,
-930.158272058824));
#154031=CARTESIAN_POINT('Ctrl Pts',(9.33447550508176,-49.9350334639422,
-931.652389705882));
#154032=CARTESIAN_POINT('Ctrl Pts',(4.70731322909511,-50.8,-933.146507352942));
#154033=CARTESIAN_POINT('Ctrl Pts',(0.,-50.8,-934.640625));
#154034=CARTESIAN_POINT('Ctrl Pts',(-4.70731322909511,-50.8,-936.134742647059));
#154035=CARTESIAN_POINT('Ctrl Pts',(-9.33447550508177,-49.9350334639422,
-937.628860294117));
#154036=CARTESIAN_POINT('Ctrl Pts',(-13.9616377810684,-49.0700669278844,
-939.122977941176));
#154037=CARTESIAN_POINT('Ctrl Pts',(-18.3510766423074,-47.3695892537413,
-940.617095588235));
#154038=CARTESIAN_POINT('Ctrl Pts',(-22.7405155035463,-45.6691115795981,
-942.111213235294));
#154039=CARTESIAN_POINT('Ctrl Pts',(-26.7427538741697,-43.1910304950644,
-943.605330882353));
#154040=CARTESIAN_POINT('Ctrl Pts',(-30.744992244793,-40.7129494105307,
-945.099448529412));
#154041=CARTESIAN_POINT('Ctrl Pts',(-34.2237386972451,-37.5416529948095,
-946.593566176471));
#154042=CARTESIAN_POINT('Ctrl Pts',(-37.7024851496972,-34.3703565790883,
-948.08768382353));
#154043=CARTESIAN_POINT('Ctrl Pts',(-40.5392751458362,-30.6138395280662,
-949.581801470588));
#154044=CARTESIAN_POINT('Ctrl Pts',(-43.3760651419751,-26.8573224770441,
-951.075919117647));
#154045=CARTESIAN_POINT('Ctrl Pts',(-45.4742952008371,-22.6435084734481,
-952.570036764706));
#154046=CARTESIAN_POINT('Ctrl Pts',(-47.5725252596992,-18.4296944698521,
-954.064154411765));
#154047=CARTESIAN_POINT('Ctrl Pts',(-48.8607426731792,-13.9020798956618,
-955.558272058823));
#154048=CARTESIAN_POINT('Ctrl Pts',(-50.1489600866593,-9.37446532147148,
-957.052389705882));
#154049=CARTESIAN_POINT('Ctrl Pts',(-50.5832961557877,-4.68723266073574,
-958.546507352941));
#154050=CARTESIAN_POINT('Ctrl Pts',(-51.0176322249162,-3.12392900021603E-15,
-960.040625));
#154051=CARTESIAN_POINT('Ctrl Pts',(-50.5832961557877,4.68723266073573,
-961.534742647059));
#154052=CARTESIAN_POINT('Ctrl Pts',(-50.1489600866593,9.37446532147149,
-963.028860294118));
#154053=CARTESIAN_POINT('Ctrl Pts',(-48.8607426731792,13.9020798956618,
-964.522977941177));
#154054=CARTESIAN_POINT('Ctrl Pts',(-47.5725252596992,18.4296944698521,
-966.017095588235));
#154055=CARTESIAN_POINT('Ctrl Pts',(-45.4742952008371,22.6435084734481,
-967.511213235294));
#154056=CARTESIAN_POINT('Ctrl Pts',(-43.3760651419751,26.8573224770442,
-969.005330882353));
#154057=CARTESIAN_POINT('Ctrl Pts',(-40.5392751458362,30.6138395280662,
-970.499448529412));
#154058=CARTESIAN_POINT('Ctrl Pts',(-37.7024851496972,34.3703565790883,
-971.99356617647));
#154059=CARTESIAN_POINT('Ctrl Pts',(-34.2237386972451,37.5416529948095,
-973.487683823529));
#154060=CARTESIAN_POINT('Ctrl Pts',(-30.744992244793,40.7129494105307,-974.981801470588));
#154061=CARTESIAN_POINT('Ctrl Pts',(-26.7427538741697,43.1910304950644,
-976.475919117647));
#154062=CARTESIAN_POINT('Ctrl Pts',(-22.7405155035463,45.6691115795981,
-977.970036764706));
#154063=CARTESIAN_POINT('Ctrl Pts',(-18.3510766423074,47.3695892537413,
-979.464154411765));
#154064=CARTESIAN_POINT('Ctrl Pts',(-13.9616377810684,49.0700669278844,
-980.958272058824));
#154065=CARTESIAN_POINT('Ctrl Pts',(-9.33447550508177,49.9350334639422,
-982.452389705882));
#154066=CARTESIAN_POINT('Ctrl Pts',(-4.7073132290951,50.8,-983.946507352941));
#154067=CARTESIAN_POINT('Ctrl Pts',(-6.22120573966855E-15,50.8,-985.440625));
#154068=CARTESIAN_POINT('Ctrl Pts',(4.70731322909511,50.8,-986.934742647059));
#154069=CARTESIAN_POINT('Ctrl Pts',(9.33447550508176,49.9350334639422,-988.428860294118));
#154070=CARTESIAN_POINT('Ctrl Pts',(13.9616377810684,49.0700669278844,-989.922977941177));
#154071=CARTESIAN_POINT('Ctrl Pts',(18.3510766423074,47.3695892537413,-991.417095588235));
#154072=CARTESIAN_POINT('Ctrl Pts',(22.7405155035463,45.6691115795981,-992.911213235294));
#154073=CARTESIAN_POINT('Ctrl Pts',(26.7427538741697,43.1910304950644,-994.405330882353));
#154074=CARTESIAN_POINT('Ctrl Pts',(30.744992244793,40.7129494105307,-995.899448529412));
#154075=CARTESIAN_POINT('Ctrl Pts',(34.2237386972451,37.5416529948095,-997.39356617647));
#154076=CARTESIAN_POINT('Ctrl Pts',(37.7024851496972,34.3703565790883,-998.887683823529));
#154077=CARTESIAN_POINT('Ctrl Pts',(40.5392751458362,30.6138395280662,-1000.38180147059));
#154078=CARTESIAN_POINT('Ctrl Pts',(43.3760651419751,26.8573224770442,-1001.87591911765));
#154079=CARTESIAN_POINT('Ctrl Pts',(45.4742952008372,22.6435084734481,-1003.37003676471));
#154080=CARTESIAN_POINT('Ctrl Pts',(47.5725252596992,18.4296944698521,-1004.86415441176));
#154081=CARTESIAN_POINT('Ctrl Pts',(48.8607426731792,13.9020798956618,-1006.35827205882));
#154082=CARTESIAN_POINT('Ctrl Pts',(50.1489600866593,9.37446532147146,-1007.85238970588));
#154083=CARTESIAN_POINT('Ctrl Pts',(50.5832961557877,4.68723266073574,-1009.34650735294));
#154084=CARTESIAN_POINT('Ctrl Pts',(51.0176322249162,9.37178700064808E-15,
-1010.840625));
#154085=CARTESIAN_POINT('Ctrl Pts',(50.5832961557877,-4.68723266073572,
-1012.33474264706));
#154086=CARTESIAN_POINT('Ctrl Pts',(50.1489600866593,-9.37446532147149,
-1013.82886029412));
#154087=CARTESIAN_POINT('Ctrl Pts',(48.8607426731792,-13.9020798956618,
-1015.32297794118));
#154088=CARTESIAN_POINT('Ctrl Pts',(47.5725252596992,-18.4296944698521,
-1016.81709558824));
#154089=CARTESIAN_POINT('Ctrl Pts',(45.4742952008371,-22.6435084734482,
-1018.31121323529));
#154090=CARTESIAN_POINT('Ctrl Pts',(43.3760651419751,-26.8573224770441,
-1019.80533088235));
#154091=CARTESIAN_POINT('Ctrl Pts',(40.5392751458362,-30.6138395280662,
-1021.29944852941));
#154092=CARTESIAN_POINT('Ctrl Pts',(37.7024851496972,-34.3703565790883,
-1022.79356617647));
#154093=CARTESIAN_POINT('Ctrl Pts',(34.2237386972451,-37.5416529948095,
-1024.28768382353));
#154094=CARTESIAN_POINT('Ctrl Pts',(30.744992244793,-40.7129494105307,-1025.78180147059));
#154095=CARTESIAN_POINT('Ctrl Pts',(26.7427538741697,-43.1910304950644,
-1027.27591911765));
#154096=CARTESIAN_POINT('Ctrl Pts',(22.7405155035463,-45.6691115795981,
-1028.77003676471));
#154097=CARTESIAN_POINT('Ctrl Pts',(18.3510766423074,-47.3695892537413,
-1030.26415441176));
#154098=CARTESIAN_POINT('Ctrl Pts',(13.9616377810684,-49.0700669278844,
-1031.75827205882));
#154099=CARTESIAN_POINT('Ctrl Pts',(9.33447550508176,-49.9350334639422,
-1033.25238970588));
#154100=CARTESIAN_POINT('Ctrl Pts',(4.70731322909511,-50.8,-1034.74650735294));
#154101=CARTESIAN_POINT('Ctrl Pts',(0.,-50.8,-1036.240625));
#154102=CARTESIAN_POINT('Ctrl Pts',(-4.70731322909511,-50.8,-1037.73474264706));
#154103=CARTESIAN_POINT('Ctrl Pts',(-9.33447550508177,-49.9350334639422,
-1039.22886029412));
#154104=CARTESIAN_POINT('Ctrl Pts',(-13.9616377810684,-49.0700669278844,
-1040.72297794118));
#154105=CARTESIAN_POINT('Ctrl Pts',(-18.3510766423074,-47.3695892537413,
-1042.21709558823));
#154106=CARTESIAN_POINT('Ctrl Pts',(-22.7405155035463,-45.6691115795981,
-1043.71121323529));
#154107=CARTESIAN_POINT('Ctrl Pts',(-26.7427538741697,-43.1910304950644,
-1045.20533088235));
#154108=CARTESIAN_POINT('Ctrl Pts',(-30.744992244793,-40.7129494105307,
-1046.69944852941));
#154109=CARTESIAN_POINT('Ctrl Pts',(-34.2237386972451,-37.5416529948095,
-1048.19356617647));
#154110=CARTESIAN_POINT('Ctrl Pts',(-37.7024851496972,-34.3703565790883,
-1049.68768382353));
#154111=CARTESIAN_POINT('Ctrl Pts',(-40.5392751458362,-30.6138395280662,
-1051.18180147059));
#154112=CARTESIAN_POINT('Ctrl Pts',(-43.3760651419751,-26.8573224770441,
-1052.67591911765));
#154113=CARTESIAN_POINT('Ctrl Pts',(-45.4742952008371,-22.6435084734481,
-1054.17003676471));
#154114=CARTESIAN_POINT('Ctrl Pts',(-47.5725252596992,-18.4296944698521,
-1055.66415441177));
#154115=CARTESIAN_POINT('Ctrl Pts',(-48.8607426731792,-13.9020798956618,
-1057.15827205882));
#154116=CARTESIAN_POINT('Ctrl Pts',(-50.1489600866593,-9.37446532147148,
-1058.65238970588));
#154117=CARTESIAN_POINT('Ctrl Pts',(-50.5832961557877,-4.68723266073574,
-1060.14650735294));
#154118=CARTESIAN_POINT('Ctrl Pts',(-51.0176322249162,-3.12392900021603E-15,
-1061.640625));
#154119=CARTESIAN_POINT('Ctrl Pts',(-50.5832961557877,4.68723266073573,
-1063.13474264706));
#154120=CARTESIAN_POINT('Ctrl Pts',(-50.1489600866593,9.37446532147149,
-1064.62886029412));
#154121=CARTESIAN_POINT('Ctrl Pts',(-48.8607426731792,13.9020798956618,
-1066.12297794118));
#154122=CARTESIAN_POINT('Ctrl Pts',(-47.5725252596992,18.4296944698521,
-1067.61709558824));
#154123=CARTESIAN_POINT('Ctrl Pts',(-45.4742952008371,22.6435084734481,
-1069.11121323529));
#154124=CARTESIAN_POINT('Ctrl Pts',(-43.3760651419751,26.8573224770442,
-1070.60533088235));
#154125=CARTESIAN_POINT('Ctrl Pts',(-40.5392751458362,30.6138395280662,
-1072.09944852941));
#154126=CARTESIAN_POINT('Ctrl Pts',(-37.7024851496972,34.3703565790883,
-1073.59356617647));
#154127=CARTESIAN_POINT('Ctrl Pts',(-34.2237386972451,37.5416529948095,
-1075.08768382353));
#154128=CARTESIAN_POINT('Ctrl Pts',(-30.744992244793,40.7129494105307,-1076.58180147059));
#154129=CARTESIAN_POINT('Ctrl Pts',(-26.7427538741697,43.1910304950644,
-1078.07591911765));
#154130=CARTESIAN_POINT('Ctrl Pts',(-22.7405155035463,45.6691115795981,
-1079.57003676471));
#154131=CARTESIAN_POINT('Ctrl Pts',(-18.3510766423074,47.3695892537413,
-1081.06415441176));
#154132=CARTESIAN_POINT('Ctrl Pts',(-13.9616377810684,49.0700669278844,
-1082.55827205882));
#154133=CARTESIAN_POINT('Ctrl Pts',(-9.33447550508177,49.9350334639422,
-1084.05238970588));
#154134=CARTESIAN_POINT('Ctrl Pts',(-4.7073132290951,50.8,-1085.54650735294));
#154135=CARTESIAN_POINT('Ctrl Pts',(-6.22120573966855E-15,50.8,-1087.040625));
#154136=CARTESIAN_POINT('Ctrl Pts',(4.70731322909511,50.8,-1088.53474264706));
#154137=CARTESIAN_POINT('Ctrl Pts',(9.33447550508176,49.9350334639422,-1090.02886029412));
#154138=CARTESIAN_POINT('Ctrl Pts',(13.9616377810684,49.0700669278844,-1091.52297794118));
#154139=CARTESIAN_POINT('Ctrl Pts',(18.3510766423074,47.3695892537413,-1093.01709558824));
#154140=CARTESIAN_POINT('Ctrl Pts',(22.7405155035463,45.6691115795981,-1094.51121323529));
#154141=CARTESIAN_POINT('Ctrl Pts',(26.7427538741697,43.1910304950644,-1096.00533088235));
#154142=CARTESIAN_POINT('Ctrl Pts',(30.744992244793,40.7129494105307,-1097.49944852941));
#154143=CARTESIAN_POINT('Ctrl Pts',(34.2237386972451,37.5416529948095,-1098.99356617647));
#154144=CARTESIAN_POINT('Ctrl Pts',(37.7024851496972,34.3703565790883,-1100.48768382353));
#154145=CARTESIAN_POINT('Ctrl Pts',(40.5392751458362,30.6138395280662,-1101.98180147059));
#154146=CARTESIAN_POINT('Ctrl Pts',(43.3760651419751,26.8573224770442,-1103.47591911765));
#154147=CARTESIAN_POINT('Ctrl Pts',(45.4742952008372,22.6435084734481,-1104.97003676471));
#154148=CARTESIAN_POINT('Ctrl Pts',(47.5725252596992,18.4296944698521,-1106.46415441176));
#154149=CARTESIAN_POINT('Ctrl Pts',(48.8607426731792,13.9020798956618,-1107.95827205882));
#154150=CARTESIAN_POINT('Ctrl Pts',(50.1489600866593,9.37446532147146,-1109.45238970588));
#154151=CARTESIAN_POINT('Ctrl Pts',(50.5832961557877,4.68723266073574,-1110.94650735294));
#154152=CARTESIAN_POINT('Ctrl Pts',(51.0176322249162,9.37178700064808E-15,
-1112.440625));
#154153=CARTESIAN_POINT('Ctrl Pts',(50.5832961557877,-4.68723266073572,
-1113.93474264706));
#154154=CARTESIAN_POINT('Ctrl Pts',(50.1489600866593,-9.37446532147149,
-1115.42886029412));
#154155=CARTESIAN_POINT('Ctrl Pts',(48.8607426731792,-13.9020798956618,
-1116.92297794118));
#154156=CARTESIAN_POINT('Ctrl Pts',(47.5725252596992,-18.4296944698521,
-1118.41709558824));
#154157=CARTESIAN_POINT('Ctrl Pts',(45.4742952008371,-22.6435084734482,
-1119.91121323529));
#154158=CARTESIAN_POINT('Ctrl Pts',(43.3760651419751,-26.8573224770441,
-1121.40533088235));
#154159=CARTESIAN_POINT('Ctrl Pts',(40.5392751458362,-30.6138395280662,
-1122.89944852941));
#154160=CARTESIAN_POINT('Ctrl Pts',(37.7024851496972,-34.3703565790883,
-1124.39356617647));
#154161=CARTESIAN_POINT('Ctrl Pts',(34.2237386972451,-37.5416529948095,
-1125.88768382353));
#154162=CARTESIAN_POINT('Ctrl Pts',(30.744992244793,-40.7129494105307,-1127.38180147059));
#154163=CARTESIAN_POINT('Ctrl Pts',(26.7427538741697,-43.1910304950644,
-1128.87591911765));
#154164=CARTESIAN_POINT('Ctrl Pts',(22.7405155035463,-45.6691115795981,
-1130.37003676471));
#154165=CARTESIAN_POINT('Ctrl Pts',(18.3510766423074,-47.3695892537413,
-1131.86415441176));
#154166=CARTESIAN_POINT('Ctrl Pts',(13.9616377810684,-49.0700669278844,
-1133.35827205882));
#154167=CARTESIAN_POINT('Ctrl Pts',(9.33447550508176,-49.9350334639422,
-1134.85238970588));
#154168=CARTESIAN_POINT('Ctrl Pts',(4.70731322909511,-50.8,-1136.34650735294));
#154169=CARTESIAN_POINT('Ctrl Pts',(0.,-50.8,-1137.840625));
#154170=CARTESIAN_POINT('Ctrl Pts',(-4.70731322909511,-50.8,-1139.33474264706));
#154171=CARTESIAN_POINT('Ctrl Pts',(-9.33447550508177,-49.9350334639422,
-1140.82886029412));
#154172=CARTESIAN_POINT('Ctrl Pts',(-13.9616377810684,-49.0700669278844,
-1142.32297794118));
#154173=CARTESIAN_POINT('Ctrl Pts',(-18.3510766423074,-47.3695892537413,
-1143.81709558824));
#154174=CARTESIAN_POINT('Ctrl Pts',(-22.7405155035463,-45.6691115795981,
-1145.31121323529));
#154175=CARTESIAN_POINT('Ctrl Pts',(-26.7427538741697,-43.1910304950644,
-1146.80533088235));
#154176=CARTESIAN_POINT('Ctrl Pts',(-30.744992244793,-40.7129494105307,
-1148.29944852941));
#154177=CARTESIAN_POINT('Ctrl Pts',(-34.2237386972451,-37.5416529948095,
-1149.79356617647));
#154178=CARTESIAN_POINT('Ctrl Pts',(-37.7024851496972,-34.3703565790883,
-1151.28768382353));
#154179=CARTESIAN_POINT('Ctrl Pts',(-40.5392751458362,-30.6138395280662,
-1152.78180147059));
#154180=CARTESIAN_POINT('Ctrl Pts',(-43.3760651419751,-26.8573224770441,
-1154.27591911765));
#154181=CARTESIAN_POINT('Ctrl Pts',(-45.4742952008371,-22.6435084734481,
-1155.77003676471));
#154182=CARTESIAN_POINT('Ctrl Pts',(-47.5725252596992,-18.4296944698521,
-1157.26415441177));
#154183=CARTESIAN_POINT('Ctrl Pts',(-48.8607426731792,-13.9020798956618,
-1158.75827205882));
#154184=CARTESIAN_POINT('Ctrl Pts',(-50.1489600866593,-9.37446532147148,
-1160.25238970588));
#154185=CARTESIAN_POINT('Ctrl Pts',(-50.5832961557877,-4.68723266073574,
-1161.74650735294));
#154186=CARTESIAN_POINT('Ctrl Pts',(-51.0176322249162,-3.12392900021603E-15,
-1163.240625));
#154187=CARTESIAN_POINT('Ctrl Pts',(-50.5832961557877,4.68723266073573,
-1164.73474264706));
#154188=CARTESIAN_POINT('Ctrl Pts',(-50.1489600866593,9.37446532147149,
-1166.22886029412));
#154189=CARTESIAN_POINT('Ctrl Pts',(-48.8607426731792,13.9020798956618,
-1167.72297794118));
#154190=CARTESIAN_POINT('Ctrl Pts',(-47.5725252596992,18.4296944698521,
-1169.21709558824));
#154191=CARTESIAN_POINT('Ctrl Pts',(-45.4742952008371,22.6435084734481,
-1170.71121323529));
#154192=CARTESIAN_POINT('Ctrl Pts',(-43.3760651419751,26.8573224770442,
-1172.20533088235));
#154193=CARTESIAN_POINT('Ctrl Pts',(-40.5392751458362,30.6138395280662,
-1173.69944852941));
#154194=CARTESIAN_POINT('Ctrl Pts',(-37.7024851496972,34.3703565790883,
-1175.19356617647));
#154195=CARTESIAN_POINT('Ctrl Pts',(-34.2237386972451,37.5416529948095,
-1176.68768382353));
#154196=CARTESIAN_POINT('Ctrl Pts',(-30.744992244793,40.7129494105307,-1178.18180147059));
#154197=CARTESIAN_POINT('Ctrl Pts',(-26.7427538741697,43.1910304950644,
-1179.67591911765));
#154198=CARTESIAN_POINT('Ctrl Pts',(-22.7405155035463,45.6691115795981,
-1181.17003676471));
#154199=CARTESIAN_POINT('Ctrl Pts',(-18.3510766423074,47.3695892537413,
-1182.66415441176));
#154200=CARTESIAN_POINT('Ctrl Pts',(-13.9616377810684,49.0700669278844,
-1184.15827205882));
#154201=CARTESIAN_POINT('Ctrl Pts',(-9.33447550508177,49.9350334639422,
-1185.65238970588));
#154202=CARTESIAN_POINT('Ctrl Pts',(-4.7073132290951,50.8,-1187.14650735294));
#154203=CARTESIAN_POINT('Ctrl Pts',(-6.22120573966855E-15,50.8,-1188.640625));
#154204=CARTESIAN_POINT('Ctrl Pts',(4.70731322909511,50.8,-1190.13474264706));
#154205=CARTESIAN_POINT('Ctrl Pts',(9.33447550508176,49.9350334639422,-1191.62886029412));
#154206=CARTESIAN_POINT('Ctrl Pts',(13.9616377810684,49.0700669278844,-1193.12297794118));
#154207=CARTESIAN_POINT('Ctrl Pts',(18.3510766423074,47.3695892537413,-1194.61709558824));
#154208=CARTESIAN_POINT('Ctrl Pts',(22.7405155035463,45.6691115795981,-1196.11121323529));
#154209=CARTESIAN_POINT('Ctrl Pts',(26.7427538741697,43.1910304950644,-1197.60533088235));
#154210=CARTESIAN_POINT('Ctrl Pts',(30.744992244793,40.7129494105307,-1199.09944852941));
#154211=CARTESIAN_POINT('Ctrl Pts',(34.2237386972451,37.5416529948095,-1200.59356617647));
#154212=CARTESIAN_POINT('Ctrl Pts',(37.7024851496972,34.3703565790883,-1202.08768382353));
#154213=CARTESIAN_POINT('Ctrl Pts',(40.5392751458362,30.6138395280662,-1203.58180147059));
#154214=CARTESIAN_POINT('Ctrl Pts',(43.3760651419751,26.8573224770442,-1205.07591911765));
#154215=CARTESIAN_POINT('Ctrl Pts',(45.4742952008372,22.6435084734481,-1206.57003676471));
#154216=CARTESIAN_POINT('Ctrl Pts',(47.5725252596992,18.4296944698521,-1208.06415441176));
#154217=CARTESIAN_POINT('Ctrl Pts',(48.8607426731792,13.9020798956618,-1209.55827205882));
#154218=CARTESIAN_POINT('Ctrl Pts',(50.1489600866593,9.37446532147146,-1211.05238970588));
#154219=CARTESIAN_POINT('Ctrl Pts',(50.5832961557877,4.68723266073574,-1212.54650735294));
#154220=CARTESIAN_POINT('Ctrl Pts',(51.0176322249162,9.37178700064808E-15,
-1214.040625));
#154221=CARTESIAN_POINT('Ctrl Pts',(50.5832961557877,-4.68723266073572,
-1215.53474264706));
#154222=CARTESIAN_POINT('Ctrl Pts',(50.1489600866593,-9.37446532147149,
-1217.02886029412));
#154223=CARTESIAN_POINT('Ctrl Pts',(48.8607426731792,-13.9020798956618,
-1218.52297794118));
#154224=CARTESIAN_POINT('Ctrl Pts',(47.5725252596992,-18.4296944698521,
-1220.01709558824));
#154225=CARTESIAN_POINT('Ctrl Pts',(45.4742952008371,-22.6435084734482,
-1221.51121323529));
#154226=CARTESIAN_POINT('Ctrl Pts',(43.3760651419751,-26.8573224770441,
-1223.00533088235));
#154227=CARTESIAN_POINT('Ctrl Pts',(40.5392751458362,-30.6138395280662,
-1224.49944852941));
#154228=CARTESIAN_POINT('Ctrl Pts',(37.7024851496972,-34.3703565790883,
-1225.99356617647));
#154229=CARTESIAN_POINT('Ctrl Pts',(34.2237386972451,-37.5416529948095,
-1227.48768382353));
#154230=CARTESIAN_POINT('Ctrl Pts',(30.744992244793,-40.7129494105307,-1228.98180147059));
#154231=CARTESIAN_POINT('Ctrl Pts',(26.7427538741697,-43.1910304950644,
-1230.47591911765));
#154232=CARTESIAN_POINT('Ctrl Pts',(22.7405155035463,-45.6691115795981,
-1231.97003676471));
#154233=CARTESIAN_POINT('Ctrl Pts',(18.3510766423074,-47.3695892537413,
-1233.46415441176));
#154234=CARTESIAN_POINT('Ctrl Pts',(13.9616377810684,-49.0700669278844,
-1234.95827205882));
#154235=CARTESIAN_POINT('Ctrl Pts',(9.33447550508176,-49.9350334639422,
-1236.45238970588));
#154236=CARTESIAN_POINT('Ctrl Pts',(4.70731322909511,-50.8,-1237.94650735294));
#154237=CARTESIAN_POINT('Ctrl Pts',(0.,-50.8,-1239.440625));
#154238=CARTESIAN_POINT('Ctrl Pts',(-4.70731322909511,-50.8,-1240.93474264706));
#154239=CARTESIAN_POINT('Ctrl Pts',(-9.33447550508177,-49.9350334639422,
-1242.42886029412));
#154240=CARTESIAN_POINT('Ctrl Pts',(-13.9616377810684,-49.0700669278844,
-1243.92297794118));
#154241=CARTESIAN_POINT('Ctrl Pts',(-18.3510766423074,-47.3695892537413,
-1245.41709558824));
#154242=CARTESIAN_POINT('Ctrl Pts',(-22.7405155035463,-45.6691115795981,
-1246.91121323529));
#154243=CARTESIAN_POINT('Ctrl Pts',(-26.7427538741697,-43.1910304950644,
-1248.40533088235));
#154244=CARTESIAN_POINT('Ctrl Pts',(-30.744992244793,-40.7129494105307,
-1249.89944852941));
#154245=CARTESIAN_POINT('Ctrl Pts',(-34.2237386972451,-37.5416529948095,
-1251.39356617647));
#154246=CARTESIAN_POINT('Ctrl Pts',(-37.7024851496972,-34.3703565790883,
-1252.88768382353));
#154247=CARTESIAN_POINT('Ctrl Pts',(-40.5392751458362,-30.6138395280662,
-1254.38180147059));
#154248=CARTESIAN_POINT('Ctrl Pts',(-43.3760651419751,-26.8573224770441,
-1255.87591911765));
#154249=CARTESIAN_POINT('Ctrl Pts',(-45.4742952008371,-22.6435084734481,
-1257.37003676471));
#154250=CARTESIAN_POINT('Ctrl Pts',(-47.5725252596992,-18.4296944698521,
-1258.86415441177));
#154251=CARTESIAN_POINT('Ctrl Pts',(-48.8607426731792,-13.9020798956618,
-1260.35827205882));
#154252=CARTESIAN_POINT('Ctrl Pts',(-50.1489600866593,-9.37446532147148,
-1261.85238970588));
#154253=CARTESIAN_POINT('Ctrl Pts',(-50.5832961557877,-4.68723266073574,
-1263.34650735294));
#154254=CARTESIAN_POINT('Ctrl Pts',(-51.0176322249162,-3.12392900021603E-15,
-1264.840625));
#154255=CARTESIAN_POINT('Ctrl Pts',(-50.5832961557877,4.68723266073573,
-1266.33474264706));
#154256=CARTESIAN_POINT('Ctrl Pts',(-50.1489600866593,9.37446532147149,
-1267.82886029412));
#154257=CARTESIAN_POINT('Ctrl Pts',(-48.8607426731792,13.9020798956618,
-1269.32297794118));
#154258=CARTESIAN_POINT('Ctrl Pts',(-47.5725252596992,18.4296944698521,
-1270.81709558824));
#154259=CARTESIAN_POINT('Ctrl Pts',(-45.4742952008371,22.6435084734481,
-1272.31121323529));
#154260=CARTESIAN_POINT('Ctrl Pts',(-43.3760651419751,26.8573224770442,
-1273.80533088235));
#154261=CARTESIAN_POINT('Ctrl Pts',(-40.5392751458362,30.6138395280662,
-1275.29944852941));
#154262=CARTESIAN_POINT('Ctrl Pts',(-37.7024851496972,34.3703565790883,
-1276.79356617647));
#154263=CARTESIAN_POINT('Ctrl Pts',(-34.2237386972451,37.5416529948095,
-1278.28768382353));
#154264=CARTESIAN_POINT('Ctrl Pts',(-30.744992244793,40.7129494105307,-1279.78180147059));
#154265=CARTESIAN_POINT('Ctrl Pts',(-26.7427538741697,43.1910304950644,
-1281.27591911765));
#154266=CARTESIAN_POINT('Ctrl Pts',(-22.7405155035463,45.6691115795981,
-1282.77003676471));
#154267=CARTESIAN_POINT('Ctrl Pts',(-18.3510766423074,47.3695892537413,
-1284.26415441176));
#154268=CARTESIAN_POINT('Ctrl Pts',(-13.9616377810684,49.0700669278844,
-1285.75827205882));
#154269=CARTESIAN_POINT('Ctrl Pts',(-9.33447550508177,49.9350334639422,
-1287.25238970588));
#154270=CARTESIAN_POINT('Ctrl Pts',(-4.7073132290951,50.8,-1288.74650735294));
#154271=CARTESIAN_POINT('Ctrl Pts',(-6.22120573966855E-15,50.8,-1290.240625));
#154272=CARTESIAN_POINT('Ctrl Pts',(4.70731322909511,50.8,-1291.73474264706));
#154273=CARTESIAN_POINT('Ctrl Pts',(9.33447550508176,49.9350334639422,-1293.22886029412));
#154274=CARTESIAN_POINT('Ctrl Pts',(13.9616377810684,49.0700669278844,-1294.72297794118));
#154275=CARTESIAN_POINT('Ctrl Pts',(18.3510766423074,47.3695892537413,-1296.21709558824));
#154276=CARTESIAN_POINT('Ctrl Pts',(22.7405155035463,45.6691115795981,-1297.71121323529));
#154277=CARTESIAN_POINT('Ctrl Pts',(26.7427538741697,43.1910304950644,-1299.20533088235));
#154278=CARTESIAN_POINT('Ctrl Pts',(30.744992244793,40.7129494105307,-1300.69944852941));
#154279=CARTESIAN_POINT('Ctrl Pts',(34.2237386972451,37.5416529948095,-1302.19356617647));
#154280=CARTESIAN_POINT('Ctrl Pts',(37.7024851496972,34.3703565790883,-1303.68768382353));
#154281=CARTESIAN_POINT('Ctrl Pts',(40.5392751458362,30.6138395280662,-1305.18180147059));
#154282=CARTESIAN_POINT('Ctrl Pts',(43.3760651419751,26.8573224770442,-1306.67591911765));
#154283=CARTESIAN_POINT('Ctrl Pts',(45.4742952008372,22.6435084734481,-1308.17003676471));
#154284=CARTESIAN_POINT('Ctrl Pts',(47.5725252596992,18.4296944698521,-1309.66415441177));
#154285=CARTESIAN_POINT('Ctrl Pts',(48.8607426731792,13.9020798956618,-1311.15827205882));
#154286=CARTESIAN_POINT('Ctrl Pts',(50.1489600866593,9.37446532147146,-1312.65238970588));
#154287=CARTESIAN_POINT('Ctrl Pts',(50.5832961557877,4.68723266073574,-1314.14650735294));
#154288=CARTESIAN_POINT('Ctrl Pts',(51.0176322249162,9.37178700064808E-15,
-1315.640625));
#154289=CARTESIAN_POINT('Ctrl Pts',(50.5832961557877,-4.68723266073572,
-1317.13474264706));
#154290=CARTESIAN_POINT('Ctrl Pts',(50.1489600866593,-9.37446532147149,
-1318.62886029412));
#154291=CARTESIAN_POINT('Ctrl Pts',(48.8607426731792,-13.9020798956618,
-1320.12297794118));
#154292=CARTESIAN_POINT('Ctrl Pts',(47.5725252596992,-18.4296944698521,
-1321.61709558824));
#154293=CARTESIAN_POINT('Ctrl Pts',(45.4742952008371,-22.6435084734482,
-1323.11121323529));
#154294=CARTESIAN_POINT('Ctrl Pts',(43.3760651419751,-26.8573224770441,
-1324.60533088235));
#154295=CARTESIAN_POINT('Ctrl Pts',(40.5392751458362,-30.6138395280662,
-1326.09944852941));
#154296=CARTESIAN_POINT('Ctrl Pts',(37.7024851496972,-34.3703565790883,
-1327.59356617647));
#154297=CARTESIAN_POINT('Ctrl Pts',(34.2237386972451,-37.5416529948095,
-1329.08768382353));
#154298=CARTESIAN_POINT('Ctrl Pts',(30.744992244793,-40.7129494105307,-1330.58180147059));
#154299=CARTESIAN_POINT('Ctrl Pts',(26.7427538741697,-43.1910304950644,
-1332.07591911765));
#154300=CARTESIAN_POINT('Ctrl Pts',(22.7405155035463,-45.6691115795981,
-1333.57003676471));
#154301=CARTESIAN_POINT('Ctrl Pts',(18.3510766423074,-47.3695892537413,
-1335.06415441176));
#154302=CARTESIAN_POINT('Ctrl Pts',(13.9616377810684,-49.0700669278844,
-1336.55827205882));
#154303=CARTESIAN_POINT('Ctrl Pts',(9.33447550508176,-49.9350334639422,
-1338.05238970588));
#154304=CARTESIAN_POINT('Ctrl Pts',(4.70731322909511,-50.8,-1339.54650735294));
#154305=CARTESIAN_POINT('Ctrl Pts',(0.,-50.8,-1341.040625));
#154306=CARTESIAN_POINT('Ctrl Pts',(-4.70731322909511,-50.8,-1342.53474264706));
#154307=CARTESIAN_POINT('Ctrl Pts',(-9.33447550508177,-49.9350334639422,
-1344.02886029412));
#154308=CARTESIAN_POINT('Ctrl Pts',(-13.9616377810684,-49.0700669278844,
-1345.52297794118));
#154309=CARTESIAN_POINT('Ctrl Pts',(-18.3510766423074,-47.3695892537413,
-1347.01709558824));
#154310=CARTESIAN_POINT('Ctrl Pts',(-22.7405155035463,-45.6691115795981,
-1348.51121323529));
#154311=CARTESIAN_POINT('Ctrl Pts',(-26.7427538741697,-43.1910304950644,
-1350.00533088235));
#154312=CARTESIAN_POINT('Ctrl Pts',(-30.744992244793,-40.7129494105307,
-1351.49944852941));
#154313=CARTESIAN_POINT('Ctrl Pts',(-34.2237386972451,-37.5416529948095,
-1352.99356617647));
#154314=CARTESIAN_POINT('Ctrl Pts',(-37.7024851496972,-34.3703565790883,
-1354.48768382353));
#154315=CARTESIAN_POINT('Ctrl Pts',(-40.5392751458362,-30.6138395280662,
-1355.98180147059));
#154316=CARTESIAN_POINT('Ctrl Pts',(-43.3760651419751,-26.8573224770441,
-1357.47591911765));
#154317=CARTESIAN_POINT('Ctrl Pts',(-45.4742952008371,-22.6435084734481,
-1358.97003676471));
#154318=CARTESIAN_POINT('Ctrl Pts',(-47.5725252596992,-18.4296944698521,
-1360.46415441177));
#154319=CARTESIAN_POINT('Ctrl Pts',(-48.8607426731792,-13.9020798956618,
-1361.95827205882));
#154320=CARTESIAN_POINT('Ctrl Pts',(-50.1489600866593,-9.37446532147148,
-1363.45238970588));
#154321=CARTESIAN_POINT('Ctrl Pts',(-50.5832961557877,-4.68723266073574,
-1364.94650735294));
#154322=CARTESIAN_POINT('Ctrl Pts',(-51.0176322249162,-3.12392900021603E-15,
-1366.440625));
#154323=CARTESIAN_POINT('Ctrl Pts',(-50.5832961557877,4.68723266073573,
-1367.93474264706));
#154324=CARTESIAN_POINT('Ctrl Pts',(-50.1489600866593,9.37446532147149,
-1369.42886029412));
#154325=CARTESIAN_POINT('Ctrl Pts',(-48.8607426731792,13.9020798956618,
-1370.92297794118));
#154326=CARTESIAN_POINT('Ctrl Pts',(-47.5725252596992,18.4296944698521,
-1372.41709558824));
#154327=CARTESIAN_POINT('Ctrl Pts',(-45.4742952008371,22.6435084734481,
-1373.91121323529));
#154328=CARTESIAN_POINT('Ctrl Pts',(-43.3760651419751,26.8573224770442,
-1375.40533088235));
#154329=CARTESIAN_POINT('Ctrl Pts',(-40.5392751458362,30.6138395280662,
-1376.89944852941));
#154330=CARTESIAN_POINT('Ctrl Pts',(-37.7024851496972,34.3703565790883,
-1378.39356617647));
#154331=CARTESIAN_POINT('Ctrl Pts',(-34.2237386972451,37.5416529948095,
-1379.88768382353));
#154332=CARTESIAN_POINT('Ctrl Pts',(-30.744992244793,40.7129494105307,-1381.38180147059));
#154333=CARTESIAN_POINT('Ctrl Pts',(-26.7427538741697,43.1910304950644,
-1382.87591911765));
#154334=CARTESIAN_POINT('Ctrl Pts',(-22.7405155035463,45.6691115795981,
-1384.37003676471));
#154335=CARTESIAN_POINT('Ctrl Pts',(-18.3510766423074,47.3695892537413,
-1385.86415441176));
#154336=CARTESIAN_POINT('Ctrl Pts',(-13.9616377810684,49.0700669278844,
-1387.35827205882));
#154337=CARTESIAN_POINT('Ctrl Pts',(-9.33447550508177,49.9350334639422,
-1388.85238970588));
#154338=CARTESIAN_POINT('Ctrl Pts',(-4.7073132290951,50.8,-1390.34650735294));
#154339=CARTESIAN_POINT('Ctrl Pts',(-6.22120573966855E-15,50.8,-1391.840625));
#154340=CARTESIAN_POINT('Ctrl Pts',(4.70731322909511,50.8,-1393.33474264706));
#154341=CARTESIAN_POINT('Ctrl Pts',(9.33447550508176,49.9350334639422,-1394.82886029412));
#154342=CARTESIAN_POINT('Ctrl Pts',(13.9616377810684,49.0700669278844,-1396.32297794118));
#154343=CARTESIAN_POINT('Ctrl Pts',(18.3510766423074,47.3695892537413,-1397.81709558824));
#154344=CARTESIAN_POINT('Ctrl Pts',(22.7405155035463,45.6691115795981,-1399.31121323529));
#154345=CARTESIAN_POINT('Ctrl Pts',(26.7427538741697,43.1910304950644,-1400.80533088235));
#154346=CARTESIAN_POINT('Ctrl Pts',(30.744992244793,40.7129494105307,-1402.29944852941));
#154347=CARTESIAN_POINT('Ctrl Pts',(34.2237386972451,37.5416529948095,-1403.79356617647));
#154348=CARTESIAN_POINT('Ctrl Pts',(37.7024851496972,34.3703565790883,-1405.28768382353));
#154349=CARTESIAN_POINT('Ctrl Pts',(40.5392751458362,30.6138395280662,-1406.78180147059));
#154350=CARTESIAN_POINT('Ctrl Pts',(43.3760651419751,26.8573224770442,-1408.27591911765));
#154351=CARTESIAN_POINT('Ctrl Pts',(45.4742952008372,22.6435084734481,-1409.77003676471));
#154352=CARTESIAN_POINT('Ctrl Pts',(47.5725252596992,18.4296944698521,-1411.26415441176));
#154353=CARTESIAN_POINT('Ctrl Pts',(48.8607426731792,13.9020798956618,-1412.75827205882));
#154354=CARTESIAN_POINT('Ctrl Pts',(50.1489600866593,9.37446532147146,-1414.25238970588));
#154355=CARTESIAN_POINT('Ctrl Pts',(50.5832961557877,4.68723266073574,-1415.74650735294));
#154356=CARTESIAN_POINT('Ctrl Pts',(51.0176322249162,9.37178700064808E-15,
-1417.240625));
#154357=CARTESIAN_POINT('Ctrl Pts',(50.5832961557877,-4.68723266073572,
-1418.73474264706));
#154358=CARTESIAN_POINT('Ctrl Pts',(50.1489600866593,-9.37446532147149,
-1420.22886029412));
#154359=CARTESIAN_POINT('Ctrl Pts',(48.8607426731792,-13.9020798956618,
-1421.72297794118));
#154360=CARTESIAN_POINT('Ctrl Pts',(47.5725252596992,-18.4296944698521,
-1423.21709558824));
#154361=CARTESIAN_POINT('Ctrl Pts',(45.4742952008371,-22.6435084734482,
-1424.71121323529));
#154362=CARTESIAN_POINT('Ctrl Pts',(43.3760651419751,-26.8573224770441,
-1426.20533088235));
#154363=CARTESIAN_POINT('Ctrl Pts',(40.5392751458362,-30.6138395280662,
-1427.69944852941));
#154364=CARTESIAN_POINT('Ctrl Pts',(37.7024851496972,-34.3703565790883,
-1429.19356617647));
#154365=CARTESIAN_POINT('Ctrl Pts',(34.2237386972451,-37.5416529948095,
-1430.68768382353));
#154366=CARTESIAN_POINT('Ctrl Pts',(30.744992244793,-40.7129494105307,-1432.18180147059));
#154367=CARTESIAN_POINT('Ctrl Pts',(26.7427538741697,-43.1910304950644,
-1433.67591911765));
#154368=CARTESIAN_POINT('Ctrl Pts',(22.7405155035463,-45.6691115795981,
-1435.17003676471));
#154369=CARTESIAN_POINT('Ctrl Pts',(18.3510766423074,-47.3695892537413,
-1436.66415441176));
#154370=CARTESIAN_POINT('Ctrl Pts',(13.9616377810684,-49.0700669278844,
-1438.15827205882));
#154371=CARTESIAN_POINT('Ctrl Pts',(9.33447550508176,-49.9350334639422,
-1439.65238970588));
#154372=CARTESIAN_POINT('Ctrl Pts',(4.70731322909511,-50.8,-1441.14650735294));
#154373=CARTESIAN_POINT('Ctrl Pts',(0.,-50.8,-1442.640625));
#154374=CARTESIAN_POINT('Ctrl Pts',(-4.70731322909511,-50.8,-1444.13474264706));
#154375=CARTESIAN_POINT('Ctrl Pts',(-9.33447550508177,-49.9350334639422,
-1445.62886029412));
#154376=CARTESIAN_POINT('Ctrl Pts',(-13.9616377810684,-49.0700669278844,
-1447.12297794118));
#154377=CARTESIAN_POINT('Ctrl Pts',(-18.3510766423074,-47.3695892537413,
-1448.61709558824));
#154378=CARTESIAN_POINT('Ctrl Pts',(-22.7405155035463,-45.6691115795981,
-1450.11121323529));
#154379=CARTESIAN_POINT('Ctrl Pts',(-26.7427538741697,-43.1910304950644,
-1451.60533088235));
#154380=CARTESIAN_POINT('Ctrl Pts',(-30.744992244793,-40.7129494105307,
-1453.09944852941));
#154381=CARTESIAN_POINT('Ctrl Pts',(-34.2237386972451,-37.5416529948095,
-1454.59356617647));
#154382=CARTESIAN_POINT('Ctrl Pts',(-37.7024851496972,-34.3703565790883,
-1456.08768382353));
#154383=CARTESIAN_POINT('Ctrl Pts',(-40.5392751458362,-30.6138395280662,
-1457.58180147059));
#154384=CARTESIAN_POINT('Ctrl Pts',(-43.3760651419751,-26.8573224770441,
-1459.07591911765));
#154385=CARTESIAN_POINT('Ctrl Pts',(-45.4742952008371,-22.6435084734481,
-1460.57003676471));
#154386=CARTESIAN_POINT('Ctrl Pts',(-47.5725252596992,-18.4296944698521,
-1462.06415441176));
#154387=CARTESIAN_POINT('Ctrl Pts',(-48.8607426731792,-13.9020798956618,
-1463.55827205882));
#154388=CARTESIAN_POINT('Ctrl Pts',(-50.1489600866593,-9.37446532147148,
-1465.05238970588));
#154389=CARTESIAN_POINT('Ctrl Pts',(-50.5832961557877,-4.68723266073574,
-1466.54650735294));
#154390=CARTESIAN_POINT('Ctrl Pts',(-51.0176322249162,-3.12392900021603E-15,
-1468.040625));
#154391=CARTESIAN_POINT('Ctrl Pts',(-50.5832961557877,4.68723266073573,
-1469.53474264706));
#154392=CARTESIAN_POINT('Ctrl Pts',(-50.1489600866593,9.37446532147149,
-1471.02886029412));
#154393=CARTESIAN_POINT('Ctrl Pts',(-48.8607426731792,13.9020798956618,
-1472.52297794118));
#154394=CARTESIAN_POINT('Ctrl Pts',(-47.5725252596992,18.4296944698521,
-1474.01709558824));
#154395=CARTESIAN_POINT('Ctrl Pts',(-45.4742952008371,22.6435084734481,
-1475.51121323529));
#154396=CARTESIAN_POINT('Ctrl Pts',(-43.3760651419751,26.8573224770442,
-1477.00533088235));
#154397=CARTESIAN_POINT('Ctrl Pts',(-40.5392751458362,30.6138395280662,
-1478.49944852941));
#154398=CARTESIAN_POINT('Ctrl Pts',(-37.7024851496972,34.3703565790883,
-1479.99356617647));
#154399=CARTESIAN_POINT('Ctrl Pts',(-34.2237386972451,37.5416529948095,
-1481.48768382353));
#154400=CARTESIAN_POINT('Ctrl Pts',(-30.744992244793,40.7129494105307,-1482.98180147059));
#154401=CARTESIAN_POINT('Ctrl Pts',(-26.7427538741697,43.1910304950644,
-1484.47591911765));
#154402=CARTESIAN_POINT('Ctrl Pts',(-22.7405155035463,45.6691115795981,
-1485.97003676471));
#154403=CARTESIAN_POINT('Ctrl Pts',(-18.3510766423074,47.3695892537413,
-1487.46415441176));
#154404=CARTESIAN_POINT('Ctrl Pts',(-13.9616377810684,49.0700669278844,
-1488.95827205882));
#154405=CARTESIAN_POINT('Ctrl Pts',(-9.33447550508177,49.9350334639422,
-1490.45238970588));
#154406=CARTESIAN_POINT('Ctrl Pts',(-4.7073132290951,50.8,-1491.94650735294));
#154407=CARTESIAN_POINT('Ctrl Pts',(-6.22120573966855E-15,50.8,-1493.440625));
#154408=CARTESIAN_POINT('Ctrl Pts',(4.70731322909511,50.8,-1494.93474264706));
#154409=CARTESIAN_POINT('Ctrl Pts',(9.33447550508176,49.9350334639422,-1496.42886029412));
#154410=CARTESIAN_POINT('Ctrl Pts',(13.9616377810684,49.0700669278844,-1497.92297794118));
#154411=CARTESIAN_POINT('Ctrl Pts',(18.3510766423074,47.3695892537413,-1499.41709558824));
#154412=CARTESIAN_POINT('Ctrl Pts',(21.2265761645012,46.2556148041416,-1500.39588461254));
#154413=CARTESIAN_POINT('Ctrl Pts',(23.9462138071277,44.8019959857072,-1501.3784575767));
#154414=CARTESIAN_POINT('',(-0.0544255098126717,-18.0479179370885,692.));
#154415=CARTESIAN_POINT('Ctrl Pts',(1.56487907968285,-38.9685918845674,
692.));
#154416=CARTESIAN_POINT('Ctrl Pts',(1.14513258304983,-35.4925583907916,
692.));
#154417=CARTESIAN_POINT('Ctrl Pts',(0.79988902048975,-32.0079330910613,
692.000000000004));
#154418=CARTESIAN_POINT('Ctrl Pts',(0.259957461376307,-25.0319090278082,
692.000000000004));
#154419=CARTESIAN_POINT('Ctrl Pts',(0.0649945143077899,-21.5401136171893,
692.));
#154420=CARTESIAN_POINT('Ctrl Pts',(-0.0544255098127947,-18.0479179370885,
692.));
#154421=CARTESIAN_POINT('',(0.,-18.048,1504.84863058659));
#154422=CARTESIAN_POINT('Ctrl Pts',(-2.21024254310115E-15,18.048,742.848630586592));
#154423=CARTESIAN_POINT('Ctrl Pts',(1.67239348737616,18.048,741.354512939533));
#154424=CARTESIAN_POINT('Ctrl Pts',(3.31631129755346,17.7406985030951,739.860395292475));
#154425=CARTESIAN_POINT('Ctrl Pts',(4.96022910773077,17.4333970061901,738.366277645416));
#154426=CARTESIAN_POINT('Ctrl Pts',(6.51968959134575,16.8292587962898,736.872159998357));
#154427=CARTESIAN_POINT('Ctrl Pts',(8.07915007496071,16.2251205863895,735.378042351298));
#154428=CARTESIAN_POINT('Ctrl Pts',(9.50104767561053,15.3447188656481,733.883924704239));
#154429=CARTESIAN_POINT('Ctrl Pts',(10.9229452762603,14.4643171449067,732.389807057181));
#154430=CARTESIAN_POINT('Ctrl Pts',(12.1588589765331,13.3376329379985,730.895689410122));
#154431=CARTESIAN_POINT('Ctrl Pts',(13.3947726768058,12.2109487310903,729.401571763063));
#154432=CARTESIAN_POINT('Ctrl Pts',(14.4026149179538,10.8763499173728,727.907454116004));
#154433=CARTESIAN_POINT('Ctrl Pts',(15.4104571591017,9.54175110365539,726.413336468945));
#154434=CARTESIAN_POINT('Ctrl Pts',(16.1559070823762,8.04468584505496,724.919218821886));
#154435=CARTESIAN_POINT('Ctrl Pts',(16.9013570056506,6.54762058645456,723.425101174828));
#154436=CARTESIAN_POINT('Ctrl Pts',(17.3590292079831,4.93906964482096,721.930983527769));
#154437=CARTESIAN_POINT('Ctrl Pts',(17.8167014103155,3.33051870318735,720.43686588071));
#154438=CARTESIAN_POINT('Ctrl Pts',(17.9710104137728,1.66525935159367,718.942748233651));
#154439=CARTESIAN_POINT('Ctrl Pts',(18.1253194172301,3.32956716117513E-15,
717.448630586592));
#154440=CARTESIAN_POINT('Ctrl Pts',(17.9710104137728,-1.66525935159367,
715.954512939534));
#154441=CARTESIAN_POINT('Ctrl Pts',(17.8167014103155,-3.33051870318736,
714.460395292475));
#154442=CARTESIAN_POINT('Ctrl Pts',(17.3590292079831,-4.93906964482095,
712.966277645416));
#154443=CARTESIAN_POINT('Ctrl Pts',(16.9013570056506,-6.54762058645456,
711.472159998357));
#154444=CARTESIAN_POINT('Ctrl Pts',(16.1559070823762,-8.04468584505497,
709.978042351298));
#154445=CARTESIAN_POINT('Ctrl Pts',(15.4104571591017,-9.54175110365538,
708.483924704239));
#154446=CARTESIAN_POINT('Ctrl Pts',(14.4026149179538,-10.8763499173728,
706.989807057181));
#154447=CARTESIAN_POINT('Ctrl Pts',(13.3947726768058,-12.2109487310903,
705.495689410122));
#154448=CARTESIAN_POINT('Ctrl Pts',(12.1588589765331,-13.3376329379985,
704.001571763063));
#154449=CARTESIAN_POINT('Ctrl Pts',(10.9229452762603,-14.4643171449067,
702.507454116004));
#154450=CARTESIAN_POINT('Ctrl Pts',(9.50104767561053,-15.3447188656481,
701.013336468945));
#154451=CARTESIAN_POINT('Ctrl Pts',(8.07915007496071,-16.2251205863895,
699.519218821886));
#154452=CARTESIAN_POINT('Ctrl Pts',(6.51968959134574,-16.8292587962898,
698.025101174828));
#154453=CARTESIAN_POINT('Ctrl Pts',(4.96022910773078,-17.4333970061901,
696.530983527769));
#154454=CARTESIAN_POINT('Ctrl Pts',(3.31631129755346,-17.7406985030951,
695.03686588071));
#154455=CARTESIAN_POINT('Ctrl Pts',(1.67239348737615,-18.048,693.542748233651));
#154456=CARTESIAN_POINT('Ctrl Pts',(0.,-18.048,692.048630586592));
#154457=CARTESIAN_POINT('Ctrl Pts',(-0.0272128167736711,-18.048,692.024318634845));
#154458=CARTESIAN_POINT('Ctrl Pts',(-0.0544255098126717,-18.0479179370885,
692.000000000001));
#154459=CARTESIAN_POINT('Ctrl Pts',(0.,-15.,1504.95));
#154460=CARTESIAN_POINT('Ctrl Pts',(-1.38995469363045,-15.,1503.45588235294));
#154461=CARTESIAN_POINT('Ctrl Pts',(-2.75624276724856,-14.7445964952585,
1501.96176470588));
#154462=CARTESIAN_POINT('Ctrl Pts',(-4.12253084086666,-14.4891929905171,
1500.46764705882));
#154463=CARTESIAN_POINT('Ctrl Pts',(-5.41862499280729,-13.9870834410653,
1498.97352941176));
#154464=CARTESIAN_POINT('Ctrl Pts',(-6.71471914474793,-13.4849738916136,
1497.47941176471));
#154465=CARTESIAN_POINT('Ctrl Pts',(-7.89648244316034,-12.7532570359442,
1495.98529411765));
#154466=CARTESIAN_POINT('Ctrl Pts',(-9.07824574157275,-12.0215401802748,
1494.49117647059));
#154467=CARTESIAN_POINT('Ctrl Pts',(-10.1054346546984,-11.0851337583099,
1492.99705882353));
#154468=CARTESIAN_POINT('Ctrl Pts',(-11.132623567824,-10.148727336345,1491.50294117647));
#154469=CARTESIAN_POINT('Ctrl Pts',(-11.9702584092036,-9.03951954568885,
1490.00882352941));
#154470=CARTESIAN_POINT('Ctrl Pts',(-12.8078932505832,-7.93031175503273,
1488.51470588235));
#154471=CARTESIAN_POINT('Ctrl Pts',(-13.4274493703259,-6.68607533664808,
1487.02058823529));
#154472=CARTESIAN_POINT('Ctrl Pts',(-14.0470054900687,-5.44183891826343,
1485.52647058824));
#154473=CARTESIAN_POINT('Ctrl Pts',(-14.4273846475923,-4.10494485108124,
1484.03235294118));
#154474=CARTESIAN_POINT('Ctrl Pts',(-14.8077638051159,-2.76805078389906,
1482.53823529412));
#154475=CARTESIAN_POINT('Ctrl Pts',(-14.9360126444255,-1.38402539194953,
1481.04411764706));
#154476=CARTESIAN_POINT('Ctrl Pts',(-15.0642614837351,-9.22419980378748E-16,
1479.55));
#154477=CARTESIAN_POINT('Ctrl Pts',(-14.9360126444255,1.38402539194953,
1478.05588235294));
#154478=CARTESIAN_POINT('Ctrl Pts',(-14.8077638051159,2.76805078389906,
1476.56176470588));
#154479=CARTESIAN_POINT('Ctrl Pts',(-14.4273846475923,4.10494485108124,
1475.06764705882));
#154480=CARTESIAN_POINT('Ctrl Pts',(-14.0470054900687,5.44183891826343,
1473.57352941176));
#154481=CARTESIAN_POINT('Ctrl Pts',(-13.4274493703259,6.68607533664807,
1472.07941176471));
#154482=CARTESIAN_POINT('Ctrl Pts',(-12.8078932505832,7.93031175503273,
1470.58529411765));
#154483=CARTESIAN_POINT('Ctrl Pts',(-11.9702584092036,9.03951954568884,
1469.09117647059));
#154484=CARTESIAN_POINT('Ctrl Pts',(-11.132623567824,10.148727336345,1467.59705882353));
#154485=CARTESIAN_POINT('Ctrl Pts',(-10.1054346546984,11.0851337583099,
1466.10294117647));
#154486=CARTESIAN_POINT('Ctrl Pts',(-9.07824574157275,12.0215401802748,
1464.60882352941));
#154487=CARTESIAN_POINT('Ctrl Pts',(-7.89648244316034,12.7532570359442,
1463.11470588235));
#154488=CARTESIAN_POINT('Ctrl Pts',(-6.71471914474793,13.4849738916136,
1461.62058823529));
#154489=CARTESIAN_POINT('Ctrl Pts',(-5.41862499280729,13.9870834410653,
1460.12647058824));
#154490=CARTESIAN_POINT('Ctrl Pts',(-4.12253084086667,14.4891929905171,
1458.63235294118));
#154491=CARTESIAN_POINT('Ctrl Pts',(-2.75624276724856,14.7445964952585,
1457.13823529412));
#154492=CARTESIAN_POINT('Ctrl Pts',(-1.38995469363044,15.,1455.64411764706));
#154493=CARTESIAN_POINT('Ctrl Pts',(-1.83697019872103E-15,15.,1454.15));
#154494=CARTESIAN_POINT('Ctrl Pts',(1.38995469363045,15.,1452.65588235294));
#154495=CARTESIAN_POINT('Ctrl Pts',(2.75624276724855,14.7445964952585,1451.16176470588));
#154496=CARTESIAN_POINT('Ctrl Pts',(4.12253084086666,14.4891929905171,1449.66764705882));
#154497=CARTESIAN_POINT('Ctrl Pts',(5.4186249928073,13.9870834410653,1448.17352941177));
#154498=CARTESIAN_POINT('Ctrl Pts',(6.71471914474792,13.4849738916136,1446.67941176471));
#154499=CARTESIAN_POINT('Ctrl Pts',(7.89648244316034,12.7532570359442,1445.18529411765));
#154500=CARTESIAN_POINT('Ctrl Pts',(9.07824574157275,12.0215401802748,1443.69117647059));
#154501=CARTESIAN_POINT('Ctrl Pts',(10.1054346546984,11.0851337583099,1442.19705882353));
#154502=CARTESIAN_POINT('Ctrl Pts',(11.132623567824,10.148727336345,1440.70294117647));
#154503=CARTESIAN_POINT('Ctrl Pts',(11.9702584092036,9.03951954568885,1439.20882352941));
#154504=CARTESIAN_POINT('Ctrl Pts',(12.8078932505832,7.93031175503273,1437.71470588235));
#154505=CARTESIAN_POINT('Ctrl Pts',(13.4274493703259,6.68607533664807,1436.22058823529));
#154506=CARTESIAN_POINT('Ctrl Pts',(14.0470054900687,5.44183891826343,1434.72647058824));
#154507=CARTESIAN_POINT('Ctrl Pts',(14.4273846475923,4.10494485108125,1433.23235294118));
#154508=CARTESIAN_POINT('Ctrl Pts',(14.8077638051159,2.76805078389905,1431.73823529412));
#154509=CARTESIAN_POINT('Ctrl Pts',(14.9360126444255,1.38402539194953,1430.24411764706));
#154510=CARTESIAN_POINT('Ctrl Pts',(15.0642614837351,2.76725994113625E-15,
1428.75));
#154511=CARTESIAN_POINT('Ctrl Pts',(14.9360126444255,-1.38402539194952,
1427.25588235294));
#154512=CARTESIAN_POINT('Ctrl Pts',(14.8077638051159,-2.76805078389906,
1425.76176470588));
#154513=CARTESIAN_POINT('Ctrl Pts',(14.4273846475923,-4.10494485108124,
1424.26764705882));
#154514=CARTESIAN_POINT('Ctrl Pts',(14.0470054900687,-5.44183891826342,
1422.77352941176));
#154515=CARTESIAN_POINT('Ctrl Pts',(13.4274493703259,-6.68607533664808,
1421.27941176471));
#154516=CARTESIAN_POINT('Ctrl Pts',(12.8078932505832,-7.93031175503273,
1419.78529411765));
#154517=CARTESIAN_POINT('Ctrl Pts',(11.9702584092036,-9.03951954568884,
1418.29117647059));
#154518=CARTESIAN_POINT('Ctrl Pts',(11.132623567824,-10.148727336345,1416.79705882353));
#154519=CARTESIAN_POINT('Ctrl Pts',(10.1054346546984,-11.0851337583099,
1415.30294117647));
#154520=CARTESIAN_POINT('Ctrl Pts',(9.07824574157275,-12.0215401802748,
1413.80882352941));
#154521=CARTESIAN_POINT('Ctrl Pts',(7.89648244316034,-12.7532570359442,
1412.31470588235));
#154522=CARTESIAN_POINT('Ctrl Pts',(6.71471914474792,-13.4849738916136,
1410.82058823529));
#154523=CARTESIAN_POINT('Ctrl Pts',(5.4186249928073,-13.9870834410653,1409.32647058824));
#154524=CARTESIAN_POINT('Ctrl Pts',(4.12253084086667,-14.4891929905171,
1407.83235294118));
#154525=CARTESIAN_POINT('Ctrl Pts',(2.75624276724855,-14.7445964952585,
1406.33823529412));
#154526=CARTESIAN_POINT('Ctrl Pts',(1.38995469363045,-15.,1404.84411764706));
#154527=CARTESIAN_POINT('Ctrl Pts',(0.,-15.,1403.35));
#154528=CARTESIAN_POINT('Ctrl Pts',(-1.38995469363045,-15.,1401.85588235294));
#154529=CARTESIAN_POINT('Ctrl Pts',(-2.75624276724856,-14.7445964952585,
1400.36176470588));
#154530=CARTESIAN_POINT('Ctrl Pts',(-4.12253084086666,-14.4891929905171,
1398.86764705882));
#154531=CARTESIAN_POINT('Ctrl Pts',(-5.41862499280729,-13.9870834410653,
1397.37352941176));
#154532=CARTESIAN_POINT('Ctrl Pts',(-6.71471914474793,-13.4849738916136,
1395.87941176471));
#154533=CARTESIAN_POINT('Ctrl Pts',(-7.89648244316034,-12.7532570359442,
1394.38529411765));
#154534=CARTESIAN_POINT('Ctrl Pts',(-9.07824574157275,-12.0215401802748,
1392.89117647059));
#154535=CARTESIAN_POINT('Ctrl Pts',(-10.1054346546984,-11.0851337583099,
1391.39705882353));
#154536=CARTESIAN_POINT('Ctrl Pts',(-11.132623567824,-10.148727336345,1389.90294117647));
#154537=CARTESIAN_POINT('Ctrl Pts',(-11.9702584092036,-9.03951954568885,
1388.40882352941));
#154538=CARTESIAN_POINT('Ctrl Pts',(-12.8078932505832,-7.93031175503273,
1386.91470588235));
#154539=CARTESIAN_POINT('Ctrl Pts',(-13.4274493703259,-6.68607533664808,
1385.42058823529));
#154540=CARTESIAN_POINT('Ctrl Pts',(-14.0470054900687,-5.44183891826343,
1383.92647058824));
#154541=CARTESIAN_POINT('Ctrl Pts',(-14.4273846475923,-4.10494485108124,
1382.43235294118));
#154542=CARTESIAN_POINT('Ctrl Pts',(-14.8077638051159,-2.76805078389906,
1380.93823529412));
#154543=CARTESIAN_POINT('Ctrl Pts',(-14.9360126444255,-1.38402539194953,
1379.44411764706));
#154544=CARTESIAN_POINT('Ctrl Pts',(-15.0642614837351,-9.22419980378748E-16,
1377.95));
#154545=CARTESIAN_POINT('Ctrl Pts',(-14.9360126444255,1.38402539194953,
1376.45588235294));
#154546=CARTESIAN_POINT('Ctrl Pts',(-14.8077638051159,2.76805078389906,
1374.96176470588));
#154547=CARTESIAN_POINT('Ctrl Pts',(-14.4273846475923,4.10494485108124,
1373.46764705882));
#154548=CARTESIAN_POINT('Ctrl Pts',(-14.0470054900687,5.44183891826343,
1371.97352941176));
#154549=CARTESIAN_POINT('Ctrl Pts',(-13.4274493703259,6.68607533664807,
1370.47941176471));
#154550=CARTESIAN_POINT('Ctrl Pts',(-12.8078932505832,7.93031175503273,
1368.98529411765));
#154551=CARTESIAN_POINT('Ctrl Pts',(-11.9702584092036,9.03951954568884,
1367.49117647059));
#154552=CARTESIAN_POINT('Ctrl Pts',(-11.132623567824,10.148727336345,1365.99705882353));
#154553=CARTESIAN_POINT('Ctrl Pts',(-10.1054346546984,11.0851337583099,
1364.50294117647));
#154554=CARTESIAN_POINT('Ctrl Pts',(-9.07824574157275,12.0215401802748,
1363.00882352941));
#154555=CARTESIAN_POINT('Ctrl Pts',(-7.89648244316034,12.7532570359442,
1361.51470588235));
#154556=CARTESIAN_POINT('Ctrl Pts',(-6.71471914474793,13.4849738916136,
1360.02058823529));
#154557=CARTESIAN_POINT('Ctrl Pts',(-5.41862499280729,13.9870834410653,
1358.52647058824));
#154558=CARTESIAN_POINT('Ctrl Pts',(-4.12253084086667,14.4891929905171,
1357.03235294118));
#154559=CARTESIAN_POINT('Ctrl Pts',(-2.75624276724856,14.7445964952585,
1355.53823529412));
#154560=CARTESIAN_POINT('Ctrl Pts',(-1.38995469363044,15.,1354.04411764706));
#154561=CARTESIAN_POINT('Ctrl Pts',(-1.83697019872103E-15,15.,1352.55));
#154562=CARTESIAN_POINT('Ctrl Pts',(1.38995469363045,15.,1351.05588235294));
#154563=CARTESIAN_POINT('Ctrl Pts',(2.75624276724855,14.7445964952585,1349.56176470588));
#154564=CARTESIAN_POINT('Ctrl Pts',(4.12253084086666,14.4891929905171,1348.06764705882));
#154565=CARTESIAN_POINT('Ctrl Pts',(5.4186249928073,13.9870834410653,1346.57352941176));
#154566=CARTESIAN_POINT('Ctrl Pts',(6.71471914474792,13.4849738916136,1345.07941176471));
#154567=CARTESIAN_POINT('Ctrl Pts',(7.89648244316034,12.7532570359442,1343.58529411765));
#154568=CARTESIAN_POINT('Ctrl Pts',(9.07824574157275,12.0215401802748,1342.09117647059));
#154569=CARTESIAN_POINT('Ctrl Pts',(10.1054346546984,11.0851337583099,1340.59705882353));
#154570=CARTESIAN_POINT('Ctrl Pts',(11.132623567824,10.148727336345,1339.10294117647));
#154571=CARTESIAN_POINT('Ctrl Pts',(11.9702584092036,9.03951954568885,1337.60882352941));
#154572=CARTESIAN_POINT('Ctrl Pts',(12.8078932505832,7.93031175503273,1336.11470588235));
#154573=CARTESIAN_POINT('Ctrl Pts',(13.4274493703259,6.68607533664807,1334.62058823529));
#154574=CARTESIAN_POINT('Ctrl Pts',(14.0470054900687,5.44183891826343,1333.12647058824));
#154575=CARTESIAN_POINT('Ctrl Pts',(14.4273846475923,4.10494485108125,1331.63235294118));
#154576=CARTESIAN_POINT('Ctrl Pts',(14.8077638051159,2.76805078389905,1330.13823529412));
#154577=CARTESIAN_POINT('Ctrl Pts',(14.9360126444255,1.38402539194953,1328.64411764706));
#154578=CARTESIAN_POINT('Ctrl Pts',(15.0642614837351,2.76725994113625E-15,
1327.15));
#154579=CARTESIAN_POINT('Ctrl Pts',(14.9360126444255,-1.38402539194952,
1325.65588235294));
#154580=CARTESIAN_POINT('Ctrl Pts',(14.8077638051159,-2.76805078389906,
1324.16176470588));
#154581=CARTESIAN_POINT('Ctrl Pts',(14.4273846475923,-4.10494485108124,
1322.66764705882));
#154582=CARTESIAN_POINT('Ctrl Pts',(14.0470054900687,-5.44183891826342,
1321.17352941176));
#154583=CARTESIAN_POINT('Ctrl Pts',(13.4274493703259,-6.68607533664808,
1319.67941176471));
#154584=CARTESIAN_POINT('Ctrl Pts',(12.8078932505832,-7.93031175503273,
1318.18529411765));
#154585=CARTESIAN_POINT('Ctrl Pts',(11.9702584092036,-9.03951954568884,
1316.69117647059));
#154586=CARTESIAN_POINT('Ctrl Pts',(11.132623567824,-10.148727336345,1315.19705882353));
#154587=CARTESIAN_POINT('Ctrl Pts',(10.1054346546984,-11.0851337583099,
1313.70294117647));
#154588=CARTESIAN_POINT('Ctrl Pts',(9.07824574157275,-12.0215401802748,
1312.20882352941));
#154589=CARTESIAN_POINT('Ctrl Pts',(7.89648244316034,-12.7532570359442,
1310.71470588235));
#154590=CARTESIAN_POINT('Ctrl Pts',(6.71471914474792,-13.4849738916136,
1309.22058823529));
#154591=CARTESIAN_POINT('Ctrl Pts',(5.4186249928073,-13.9870834410653,1307.72647058824));
#154592=CARTESIAN_POINT('Ctrl Pts',(4.12253084086667,-14.4891929905171,
1306.23235294118));
#154593=CARTESIAN_POINT('Ctrl Pts',(2.75624276724855,-14.7445964952585,
1304.73823529412));
#154594=CARTESIAN_POINT('Ctrl Pts',(1.38995469363045,-15.,1303.24411764706));
#154595=CARTESIAN_POINT('Ctrl Pts',(0.,-15.,1301.75));
#154596=CARTESIAN_POINT('Ctrl Pts',(-1.38995469363045,-15.,1300.25588235294));
#154597=CARTESIAN_POINT('Ctrl Pts',(-2.75624276724856,-14.7445964952585,
1298.76176470588));
#154598=CARTESIAN_POINT('Ctrl Pts',(-4.12253084086666,-14.4891929905171,
1297.26764705882));
#154599=CARTESIAN_POINT('Ctrl Pts',(-5.41862499280729,-13.9870834410653,
1295.77352941176));
#154600=CARTESIAN_POINT('Ctrl Pts',(-6.71471914474793,-13.4849738916136,
1294.27941176471));
#154601=CARTESIAN_POINT('Ctrl Pts',(-7.89648244316034,-12.7532570359442,
1292.78529411765));
#154602=CARTESIAN_POINT('Ctrl Pts',(-9.07824574157275,-12.0215401802748,
1291.29117647059));
#154603=CARTESIAN_POINT('Ctrl Pts',(-10.1054346546984,-11.0851337583099,
1289.79705882353));
#154604=CARTESIAN_POINT('Ctrl Pts',(-11.132623567824,-10.148727336345,1288.30294117647));
#154605=CARTESIAN_POINT('Ctrl Pts',(-11.9702584092036,-9.03951954568885,
1286.80882352941));
#154606=CARTESIAN_POINT('Ctrl Pts',(-12.8078932505832,-7.93031175503273,
1285.31470588235));
#154607=CARTESIAN_POINT('Ctrl Pts',(-13.4274493703259,-6.68607533664808,
1283.82058823529));
#154608=CARTESIAN_POINT('Ctrl Pts',(-14.0470054900687,-5.44183891826343,
1282.32647058824));
#154609=CARTESIAN_POINT('Ctrl Pts',(-14.4273846475923,-4.10494485108124,
1280.83235294118));
#154610=CARTESIAN_POINT('Ctrl Pts',(-14.8077638051159,-2.76805078389906,
1279.33823529412));
#154611=CARTESIAN_POINT('Ctrl Pts',(-14.9360126444255,-1.38402539194953,
1277.84411764706));
#154612=CARTESIAN_POINT('Ctrl Pts',(-15.0642614837351,-9.22419980378748E-16,
1276.35));
#154613=CARTESIAN_POINT('Ctrl Pts',(-14.9360126444255,1.38402539194953,
1274.85588235294));
#154614=CARTESIAN_POINT('Ctrl Pts',(-14.8077638051159,2.76805078389906,
1273.36176470588));
#154615=CARTESIAN_POINT('Ctrl Pts',(-14.4273846475923,4.10494485108124,
1271.86764705882));
#154616=CARTESIAN_POINT('Ctrl Pts',(-14.0470054900687,5.44183891826343,
1270.37352941176));
#154617=CARTESIAN_POINT('Ctrl Pts',(-13.4274493703259,6.68607533664807,
1268.87941176471));
#154618=CARTESIAN_POINT('Ctrl Pts',(-12.8078932505832,7.93031175503273,
1267.38529411765));
#154619=CARTESIAN_POINT('Ctrl Pts',(-11.9702584092036,9.03951954568884,
1265.89117647059));
#154620=CARTESIAN_POINT('Ctrl Pts',(-11.132623567824,10.148727336345,1264.39705882353));
#154621=CARTESIAN_POINT('Ctrl Pts',(-10.1054346546984,11.0851337583099,
1262.90294117647));
#154622=CARTESIAN_POINT('Ctrl Pts',(-9.07824574157275,12.0215401802748,
1261.40882352941));
#154623=CARTESIAN_POINT('Ctrl Pts',(-7.89648244316034,12.7532570359442,
1259.91470588235));
#154624=CARTESIAN_POINT('Ctrl Pts',(-6.71471914474793,13.4849738916136,
1258.42058823529));
#154625=CARTESIAN_POINT('Ctrl Pts',(-5.41862499280729,13.9870834410653,
1256.92647058824));
#154626=CARTESIAN_POINT('Ctrl Pts',(-4.12253084086667,14.4891929905171,
1255.43235294118));
#154627=CARTESIAN_POINT('Ctrl Pts',(-2.75624276724856,14.7445964952585,
1253.93823529412));
#154628=CARTESIAN_POINT('Ctrl Pts',(-1.38995469363044,15.,1252.44411764706));
#154629=CARTESIAN_POINT('Ctrl Pts',(-1.83697019872103E-15,15.,1250.95));
#154630=CARTESIAN_POINT('Ctrl Pts',(1.38995469363045,15.,1249.45588235294));
#154631=CARTESIAN_POINT('Ctrl Pts',(2.75624276724855,14.7445964952585,1247.96176470588));
#154632=CARTESIAN_POINT('Ctrl Pts',(4.12253084086666,14.4891929905171,1246.46764705882));
#154633=CARTESIAN_POINT('Ctrl Pts',(5.4186249928073,13.9870834410653,1244.97352941176));
#154634=CARTESIAN_POINT('Ctrl Pts',(6.71471914474792,13.4849738916136,1243.47941176471));
#154635=CARTESIAN_POINT('Ctrl Pts',(7.89648244316034,12.7532570359442,1241.98529411765));
#154636=CARTESIAN_POINT('Ctrl Pts',(9.07824574157275,12.0215401802748,1240.49117647059));
#154637=CARTESIAN_POINT('Ctrl Pts',(10.1054346546984,11.0851337583099,1238.99705882353));
#154638=CARTESIAN_POINT('Ctrl Pts',(11.132623567824,10.148727336345,1237.50294117647));
#154639=CARTESIAN_POINT('Ctrl Pts',(11.9702584092036,9.03951954568885,1236.00882352941));
#154640=CARTESIAN_POINT('Ctrl Pts',(12.8078932505832,7.93031175503273,1234.51470588235));
#154641=CARTESIAN_POINT('Ctrl Pts',(13.4274493703259,6.68607533664807,1233.02058823529));
#154642=CARTESIAN_POINT('Ctrl Pts',(14.0470054900687,5.44183891826343,1231.52647058824));
#154643=CARTESIAN_POINT('Ctrl Pts',(14.4273846475923,4.10494485108125,1230.03235294118));
#154644=CARTESIAN_POINT('Ctrl Pts',(14.8077638051159,2.76805078389905,1228.53823529412));
#154645=CARTESIAN_POINT('Ctrl Pts',(14.9360126444255,1.38402539194953,1227.04411764706));
#154646=CARTESIAN_POINT('Ctrl Pts',(15.0642614837351,2.76725994113625E-15,
1225.55));
#154647=CARTESIAN_POINT('Ctrl Pts',(14.9360126444255,-1.38402539194952,
1224.05588235294));
#154648=CARTESIAN_POINT('Ctrl Pts',(14.8077638051159,-2.76805078389906,
1222.56176470588));
#154649=CARTESIAN_POINT('Ctrl Pts',(14.4273846475923,-4.10494485108124,
1221.06764705882));
#154650=CARTESIAN_POINT('Ctrl Pts',(14.0470054900687,-5.44183891826342,
1219.57352941176));
#154651=CARTESIAN_POINT('Ctrl Pts',(13.4274493703259,-6.68607533664808,
1218.07941176471));
#154652=CARTESIAN_POINT('Ctrl Pts',(12.8078932505832,-7.93031175503273,
1216.58529411765));
#154653=CARTESIAN_POINT('Ctrl Pts',(11.9702584092036,-9.03951954568884,
1215.09117647059));
#154654=CARTESIAN_POINT('Ctrl Pts',(11.132623567824,-10.148727336345,1213.59705882353));
#154655=CARTESIAN_POINT('Ctrl Pts',(10.1054346546984,-11.0851337583099,
1212.10294117647));
#154656=CARTESIAN_POINT('Ctrl Pts',(9.07824574157275,-12.0215401802748,
1210.60882352941));
#154657=CARTESIAN_POINT('Ctrl Pts',(7.89648244316034,-12.7532570359442,
1209.11470588235));
#154658=CARTESIAN_POINT('Ctrl Pts',(6.71471914474792,-13.4849738916136,
1207.62058823529));
#154659=CARTESIAN_POINT('Ctrl Pts',(5.4186249928073,-13.9870834410653,1206.12647058824));
#154660=CARTESIAN_POINT('Ctrl Pts',(4.12253084086667,-14.4891929905171,
1204.63235294118));
#154661=CARTESIAN_POINT('Ctrl Pts',(2.75624276724855,-14.7445964952585,
1203.13823529412));
#154662=CARTESIAN_POINT('Ctrl Pts',(1.38995469363045,-15.,1201.64411764706));
#154663=CARTESIAN_POINT('Ctrl Pts',(0.,-15.,1200.15));
#154664=CARTESIAN_POINT('Ctrl Pts',(-1.38995469363045,-15.,1198.65588235294));
#154665=CARTESIAN_POINT('Ctrl Pts',(-2.75624276724856,-14.7445964952585,
1197.16176470588));
#154666=CARTESIAN_POINT('Ctrl Pts',(-4.12253084086666,-14.4891929905171,
1195.66764705882));
#154667=CARTESIAN_POINT('Ctrl Pts',(-5.41862499280729,-13.9870834410653,
1194.17352941176));
#154668=CARTESIAN_POINT('Ctrl Pts',(-6.71471914474793,-13.4849738916136,
1192.67941176471));
#154669=CARTESIAN_POINT('Ctrl Pts',(-7.89648244316034,-12.7532570359442,
1191.18529411765));
#154670=CARTESIAN_POINT('Ctrl Pts',(-9.07824574157275,-12.0215401802748,
1189.69117647059));
#154671=CARTESIAN_POINT('Ctrl Pts',(-10.1054346546984,-11.0851337583099,
1188.19705882353));
#154672=CARTESIAN_POINT('Ctrl Pts',(-11.132623567824,-10.148727336345,1186.70294117647));
#154673=CARTESIAN_POINT('Ctrl Pts',(-11.9702584092036,-9.03951954568885,
1185.20882352941));
#154674=CARTESIAN_POINT('Ctrl Pts',(-12.8078932505832,-7.93031175503273,
1183.71470588235));
#154675=CARTESIAN_POINT('Ctrl Pts',(-13.4274493703259,-6.68607533664808,
1182.22058823529));
#154676=CARTESIAN_POINT('Ctrl Pts',(-14.0470054900687,-5.44183891826343,
1180.72647058824));
#154677=CARTESIAN_POINT('Ctrl Pts',(-14.4273846475923,-4.10494485108124,
1179.23235294118));
#154678=CARTESIAN_POINT('Ctrl Pts',(-14.8077638051159,-2.76805078389906,
1177.73823529412));
#154679=CARTESIAN_POINT('Ctrl Pts',(-14.9360126444255,-1.38402539194953,
1176.24411764706));
#154680=CARTESIAN_POINT('Ctrl Pts',(-15.0642614837351,-9.22419980378748E-16,
1174.75));
#154681=CARTESIAN_POINT('Ctrl Pts',(-14.9360126444255,1.38402539194953,
1173.25588235294));
#154682=CARTESIAN_POINT('Ctrl Pts',(-14.8077638051159,2.76805078389906,
1171.76176470588));
#154683=CARTESIAN_POINT('Ctrl Pts',(-14.4273846475923,4.10494485108124,
1170.26764705882));
#154684=CARTESIAN_POINT('Ctrl Pts',(-14.0470054900687,5.44183891826343,
1168.77352941176));
#154685=CARTESIAN_POINT('Ctrl Pts',(-13.4274493703259,6.68607533664807,
1167.27941176471));
#154686=CARTESIAN_POINT('Ctrl Pts',(-12.8078932505832,7.93031175503273,
1165.78529411765));
#154687=CARTESIAN_POINT('Ctrl Pts',(-11.9702584092036,9.03951954568884,
1164.29117647059));
#154688=CARTESIAN_POINT('Ctrl Pts',(-11.132623567824,10.148727336345,1162.79705882353));
#154689=CARTESIAN_POINT('Ctrl Pts',(-10.1054346546984,11.0851337583099,
1161.30294117647));
#154690=CARTESIAN_POINT('Ctrl Pts',(-9.07824574157275,12.0215401802748,
1159.80882352941));
#154691=CARTESIAN_POINT('Ctrl Pts',(-7.89648244316034,12.7532570359442,
1158.31470588235));
#154692=CARTESIAN_POINT('Ctrl Pts',(-6.71471914474793,13.4849738916136,
1156.82058823529));
#154693=CARTESIAN_POINT('Ctrl Pts',(-5.41862499280729,13.9870834410653,
1155.32647058824));
#154694=CARTESIAN_POINT('Ctrl Pts',(-4.12253084086667,14.4891929905171,
1153.83235294118));
#154695=CARTESIAN_POINT('Ctrl Pts',(-2.75624276724856,14.7445964952585,
1152.33823529412));
#154696=CARTESIAN_POINT('Ctrl Pts',(-1.38995469363044,15.,1150.84411764706));
#154697=CARTESIAN_POINT('Ctrl Pts',(-1.83697019872103E-15,15.,1149.35));
#154698=CARTESIAN_POINT('Ctrl Pts',(1.38995469363045,15.,1147.85588235294));
#154699=CARTESIAN_POINT('Ctrl Pts',(2.75624276724855,14.7445964952585,1146.36176470588));
#154700=CARTESIAN_POINT('Ctrl Pts',(4.12253084086666,14.4891929905171,1144.86764705882));
#154701=CARTESIAN_POINT('Ctrl Pts',(5.4186249928073,13.9870834410653,1143.37352941176));
#154702=CARTESIAN_POINT('Ctrl Pts',(6.71471914474792,13.4849738916136,1141.87941176471));
#154703=CARTESIAN_POINT('Ctrl Pts',(7.89648244316034,12.7532570359442,1140.38529411765));
#154704=CARTESIAN_POINT('Ctrl Pts',(9.07824574157275,12.0215401802748,1138.89117647059));
#154705=CARTESIAN_POINT('Ctrl Pts',(10.1054346546984,11.0851337583099,1137.39705882353));
#154706=CARTESIAN_POINT('Ctrl Pts',(11.132623567824,10.148727336345,1135.90294117647));
#154707=CARTESIAN_POINT('Ctrl Pts',(11.9702584092036,9.03951954568885,1134.40882352941));
#154708=CARTESIAN_POINT('Ctrl Pts',(12.8078932505832,7.93031175503273,1132.91470588235));
#154709=CARTESIAN_POINT('Ctrl Pts',(13.4274493703259,6.68607533664807,1131.42058823529));
#154710=CARTESIAN_POINT('Ctrl Pts',(14.0470054900687,5.44183891826343,1129.92647058824));
#154711=CARTESIAN_POINT('Ctrl Pts',(14.4273846475923,4.10494485108125,1128.43235294118));
#154712=CARTESIAN_POINT('Ctrl Pts',(14.8077638051159,2.76805078389905,1126.93823529412));
#154713=CARTESIAN_POINT('Ctrl Pts',(14.9360126444255,1.38402539194953,1125.44411764706));
#154714=CARTESIAN_POINT('Ctrl Pts',(15.0642614837351,2.76725994113625E-15,
1123.95));
#154715=CARTESIAN_POINT('Ctrl Pts',(14.9360126444255,-1.38402539194952,
1122.45588235294));
#154716=CARTESIAN_POINT('Ctrl Pts',(14.8077638051159,-2.76805078389906,
1120.96176470588));
#154717=CARTESIAN_POINT('Ctrl Pts',(14.4273846475923,-4.10494485108124,
1119.46764705882));
#154718=CARTESIAN_POINT('Ctrl Pts',(14.0470054900687,-5.44183891826342,
1117.97352941176));
#154719=CARTESIAN_POINT('Ctrl Pts',(13.4274493703259,-6.68607533664808,
1116.47941176471));
#154720=CARTESIAN_POINT('Ctrl Pts',(12.8078932505832,-7.93031175503273,
1114.98529411765));
#154721=CARTESIAN_POINT('Ctrl Pts',(11.9702584092036,-9.03951954568884,
1113.49117647059));
#154722=CARTESIAN_POINT('Ctrl Pts',(11.132623567824,-10.148727336345,1111.99705882353));
#154723=CARTESIAN_POINT('Ctrl Pts',(10.1054346546984,-11.0851337583099,
1110.50294117647));
#154724=CARTESIAN_POINT('Ctrl Pts',(9.07824574157275,-12.0215401802748,
1109.00882352941));
#154725=CARTESIAN_POINT('Ctrl Pts',(7.89648244316034,-12.7532570359442,
1107.51470588235));
#154726=CARTESIAN_POINT('Ctrl Pts',(6.71471914474792,-13.4849738916136,
1106.02058823529));
#154727=CARTESIAN_POINT('Ctrl Pts',(5.4186249928073,-13.9870834410653,1104.52647058824));
#154728=CARTESIAN_POINT('Ctrl Pts',(4.12253084086667,-14.4891929905171,
1103.03235294118));
#154729=CARTESIAN_POINT('Ctrl Pts',(2.75624276724855,-14.7445964952585,
1101.53823529412));
#154730=CARTESIAN_POINT('Ctrl Pts',(1.38995469363045,-15.,1100.04411764706));
#154731=CARTESIAN_POINT('Ctrl Pts',(0.,-15.,1098.55));
#154732=CARTESIAN_POINT('Ctrl Pts',(-1.38995469363045,-15.,1097.05588235294));
#154733=CARTESIAN_POINT('Ctrl Pts',(-2.75624276724856,-14.7445964952585,
1095.56176470588));
#154734=CARTESIAN_POINT('Ctrl Pts',(-4.12253084086666,-14.4891929905171,
1094.06764705882));
#154735=CARTESIAN_POINT('Ctrl Pts',(-5.41862499280729,-13.9870834410653,
1092.57352941176));
#154736=CARTESIAN_POINT('Ctrl Pts',(-6.71471914474793,-13.4849738916136,
1091.07941176471));
#154737=CARTESIAN_POINT('Ctrl Pts',(-7.89648244316034,-12.7532570359442,
1089.58529411765));
#154738=CARTESIAN_POINT('Ctrl Pts',(-9.07824574157275,-12.0215401802748,
1088.09117647059));
#154739=CARTESIAN_POINT('Ctrl Pts',(-10.1054346546984,-11.0851337583099,
1086.59705882353));
#154740=CARTESIAN_POINT('Ctrl Pts',(-11.132623567824,-10.148727336345,1085.10294117647));
#154741=CARTESIAN_POINT('Ctrl Pts',(-11.9702584092036,-9.03951954568885,
1083.60882352941));
#154742=CARTESIAN_POINT('Ctrl Pts',(-12.8078932505832,-7.93031175503273,
1082.11470588235));
#154743=CARTESIAN_POINT('Ctrl Pts',(-13.4274493703259,-6.68607533664808,
1080.62058823529));
#154744=CARTESIAN_POINT('Ctrl Pts',(-14.0470054900687,-5.44183891826343,
1079.12647058824));
#154745=CARTESIAN_POINT('Ctrl Pts',(-14.4273846475923,-4.10494485108124,
1077.63235294118));
#154746=CARTESIAN_POINT('Ctrl Pts',(-14.8077638051159,-2.76805078389906,
1076.13823529412));
#154747=CARTESIAN_POINT('Ctrl Pts',(-14.9360126444255,-1.38402539194953,
1074.64411764706));
#154748=CARTESIAN_POINT('Ctrl Pts',(-15.0642614837351,-9.22419980378748E-16,
1073.15));
#154749=CARTESIAN_POINT('Ctrl Pts',(-14.9360126444255,1.38402539194953,
1071.65588235294));
#154750=CARTESIAN_POINT('Ctrl Pts',(-14.8077638051159,2.76805078389906,
1070.16176470588));
#154751=CARTESIAN_POINT('Ctrl Pts',(-14.4273846475923,4.10494485108124,
1068.66764705882));
#154752=CARTESIAN_POINT('Ctrl Pts',(-14.0470054900687,5.44183891826343,
1067.17352941176));
#154753=CARTESIAN_POINT('Ctrl Pts',(-13.4274493703259,6.68607533664807,
1065.67941176471));
#154754=CARTESIAN_POINT('Ctrl Pts',(-12.8078932505832,7.93031175503273,
1064.18529411765));
#154755=CARTESIAN_POINT('Ctrl Pts',(-11.9702584092036,9.03951954568884,
1062.69117647059));
#154756=CARTESIAN_POINT('Ctrl Pts',(-11.132623567824,10.148727336345,1061.19705882353));
#154757=CARTESIAN_POINT('Ctrl Pts',(-10.1054346546984,11.0851337583099,
1059.70294117647));
#154758=CARTESIAN_POINT('Ctrl Pts',(-9.07824574157275,12.0215401802748,
1058.20882352941));
#154759=CARTESIAN_POINT('Ctrl Pts',(-7.89648244316034,12.7532570359442,
1056.71470588235));
#154760=CARTESIAN_POINT('Ctrl Pts',(-6.71471914474793,13.4849738916136,
1055.22058823529));
#154761=CARTESIAN_POINT('Ctrl Pts',(-5.41862499280729,13.9870834410653,
1053.72647058824));
#154762=CARTESIAN_POINT('Ctrl Pts',(-4.12253084086667,14.4891929905171,
1052.23235294118));
#154763=CARTESIAN_POINT('Ctrl Pts',(-2.75624276724856,14.7445964952585,
1050.73823529412));
#154764=CARTESIAN_POINT('Ctrl Pts',(-1.38995469363044,15.,1049.24411764706));
#154765=CARTESIAN_POINT('Ctrl Pts',(-1.83697019872103E-15,15.,1047.75));
#154766=CARTESIAN_POINT('Ctrl Pts',(1.38995469363045,15.,1046.25588235294));
#154767=CARTESIAN_POINT('Ctrl Pts',(2.75624276724855,14.7445964952585,1044.76176470588));
#154768=CARTESIAN_POINT('Ctrl Pts',(4.12253084086666,14.4891929905171,1043.26764705882));
#154769=CARTESIAN_POINT('Ctrl Pts',(5.4186249928073,13.9870834410653,1041.77352941176));
#154770=CARTESIAN_POINT('Ctrl Pts',(6.71471914474792,13.4849738916136,1040.27941176471));
#154771=CARTESIAN_POINT('Ctrl Pts',(7.89648244316034,12.7532570359442,1038.78529411765));
#154772=CARTESIAN_POINT('Ctrl Pts',(9.07824574157275,12.0215401802748,1037.29117647059));
#154773=CARTESIAN_POINT('Ctrl Pts',(10.1054346546984,11.0851337583099,1035.79705882353));
#154774=CARTESIAN_POINT('Ctrl Pts',(11.132623567824,10.148727336345,1034.30294117647));
#154775=CARTESIAN_POINT('Ctrl Pts',(11.9702584092036,9.03951954568885,1032.80882352941));
#154776=CARTESIAN_POINT('Ctrl Pts',(12.8078932505832,7.93031175503273,1031.31470588235));
#154777=CARTESIAN_POINT('Ctrl Pts',(13.4274493703259,6.68607533664807,1029.82058823529));
#154778=CARTESIAN_POINT('Ctrl Pts',(14.0470054900687,5.44183891826343,1028.32647058824));
#154779=CARTESIAN_POINT('Ctrl Pts',(14.4273846475923,4.10494485108125,1026.83235294118));
#154780=CARTESIAN_POINT('Ctrl Pts',(14.8077638051159,2.76805078389905,1025.33823529412));
#154781=CARTESIAN_POINT('Ctrl Pts',(14.9360126444255,1.38402539194953,1023.84411764706));
#154782=CARTESIAN_POINT('Ctrl Pts',(15.0642614837351,2.76725994113625E-15,
1022.35));
#154783=CARTESIAN_POINT('Ctrl Pts',(14.9360126444255,-1.38402539194952,
1020.85588235294));
#154784=CARTESIAN_POINT('Ctrl Pts',(14.8077638051159,-2.76805078389906,
1019.36176470588));
#154785=CARTESIAN_POINT('Ctrl Pts',(14.4273846475923,-4.10494485108124,
1017.86764705882));
#154786=CARTESIAN_POINT('Ctrl Pts',(14.0470054900687,-5.44183891826342,
1016.37352941176));
#154787=CARTESIAN_POINT('Ctrl Pts',(13.4274493703259,-6.68607533664808,
1014.87941176471));
#154788=CARTESIAN_POINT('Ctrl Pts',(12.8078932505832,-7.93031175503273,
1013.38529411765));
#154789=CARTESIAN_POINT('Ctrl Pts',(11.9702584092036,-9.03951954568884,
1011.89117647059));
#154790=CARTESIAN_POINT('Ctrl Pts',(11.132623567824,-10.148727336345,1010.39705882353));
#154791=CARTESIAN_POINT('Ctrl Pts',(10.1054346546984,-11.0851337583099,
1008.90294117647));
#154792=CARTESIAN_POINT('Ctrl Pts',(9.07824574157275,-12.0215401802748,
1007.40882352941));
#154793=CARTESIAN_POINT('Ctrl Pts',(7.89648244316034,-12.7532570359442,
1005.91470588235));
#154794=CARTESIAN_POINT('Ctrl Pts',(6.71471914474792,-13.4849738916136,
1004.42058823529));
#154795=CARTESIAN_POINT('Ctrl Pts',(5.4186249928073,-13.9870834410653,1002.92647058824));
#154796=CARTESIAN_POINT('Ctrl Pts',(4.12253084086667,-14.4891929905171,
1001.43235294118));
#154797=CARTESIAN_POINT('Ctrl Pts',(2.75624276724855,-14.7445964952585,
999.938235294118));
#154798=CARTESIAN_POINT('Ctrl Pts',(1.38995469363045,-15.,998.444117647059));
#154799=CARTESIAN_POINT('Ctrl Pts',(0.,-15.,996.95));
#154800=CARTESIAN_POINT('Ctrl Pts',(-1.38995469363045,-15.,995.455882352941));
#154801=CARTESIAN_POINT('Ctrl Pts',(-2.75624276724856,-14.7445964952585,
993.961764705882));
#154802=CARTESIAN_POINT('Ctrl Pts',(-4.12253084086666,-14.4891929905171,
992.467647058824));
#154803=CARTESIAN_POINT('Ctrl Pts',(-5.41862499280729,-13.9870834410653,
990.973529411765));
#154804=CARTESIAN_POINT('Ctrl Pts',(-6.71471914474793,-13.4849738916136,
989.479411764706));
#154805=CARTESIAN_POINT('Ctrl Pts',(-7.89648244316034,-12.7532570359442,
987.985294117647));
#154806=CARTESIAN_POINT('Ctrl Pts',(-9.07824574157275,-12.0215401802748,
986.491176470588));
#154807=CARTESIAN_POINT('Ctrl Pts',(-10.1054346546984,-11.0851337583099,
984.997058823529));
#154808=CARTESIAN_POINT('Ctrl Pts',(-11.132623567824,-10.148727336345,983.502941176471));
#154809=CARTESIAN_POINT('Ctrl Pts',(-11.9702584092036,-9.03951954568885,
982.008823529412));
#154810=CARTESIAN_POINT('Ctrl Pts',(-12.8078932505832,-7.93031175503273,
980.514705882353));
#154811=CARTESIAN_POINT('Ctrl Pts',(-13.4274493703259,-6.68607533664808,
979.020588235294));
#154812=CARTESIAN_POINT('Ctrl Pts',(-14.0470054900687,-5.44183891826343,
977.526470588235));
#154813=CARTESIAN_POINT('Ctrl Pts',(-14.4273846475923,-4.10494485108124,
976.032352941177));
#154814=CARTESIAN_POINT('Ctrl Pts',(-14.8077638051159,-2.76805078389906,
974.538235294118));
#154815=CARTESIAN_POINT('Ctrl Pts',(-14.9360126444255,-1.38402539194953,
973.044117647059));
#154816=CARTESIAN_POINT('Ctrl Pts',(-15.0642614837351,-9.22419980378748E-16,
971.55));
#154817=CARTESIAN_POINT('Ctrl Pts',(-14.9360126444255,1.38402539194953,
970.055882352941));
#154818=CARTESIAN_POINT('Ctrl Pts',(-14.8077638051159,2.76805078389906,
968.561764705882));
#154819=CARTESIAN_POINT('Ctrl Pts',(-14.4273846475923,4.10494485108124,
967.067647058824));
#154820=CARTESIAN_POINT('Ctrl Pts',(-14.0470054900687,5.44183891826343,
965.573529411765));
#154821=CARTESIAN_POINT('Ctrl Pts',(-13.4274493703259,6.68607533664807,
964.079411764706));
#154822=CARTESIAN_POINT('Ctrl Pts',(-12.8078932505832,7.93031175503273,
962.585294117647));
#154823=CARTESIAN_POINT('Ctrl Pts',(-11.9702584092036,9.03951954568884,
961.091176470588));
#154824=CARTESIAN_POINT('Ctrl Pts',(-11.132623567824,10.148727336345,959.59705882353));
#154825=CARTESIAN_POINT('Ctrl Pts',(-10.1054346546984,11.0851337583099,
958.102941176471));
#154826=CARTESIAN_POINT('Ctrl Pts',(-9.07824574157275,12.0215401802748,
956.608823529412));
#154827=CARTESIAN_POINT('Ctrl Pts',(-7.89648244316034,12.7532570359442,
955.114705882353));
#154828=CARTESIAN_POINT('Ctrl Pts',(-6.71471914474793,13.4849738916136,
953.620588235294));
#154829=CARTESIAN_POINT('Ctrl Pts',(-5.41862499280729,13.9870834410653,
952.126470588235));
#154830=CARTESIAN_POINT('Ctrl Pts',(-4.12253084086667,14.4891929905171,
950.632352941177));
#154831=CARTESIAN_POINT('Ctrl Pts',(-2.75624276724856,14.7445964952585,
949.138235294118));
#154832=CARTESIAN_POINT('Ctrl Pts',(-1.38995469363044,15.,947.644117647059));
#154833=CARTESIAN_POINT('Ctrl Pts',(-1.83697019872103E-15,15.,946.15));
#154834=CARTESIAN_POINT('Ctrl Pts',(1.38995469363045,15.,944.655882352941));
#154835=CARTESIAN_POINT('Ctrl Pts',(2.75624276724855,14.7445964952585,943.161764705882));
#154836=CARTESIAN_POINT('Ctrl Pts',(4.12253084086666,14.4891929905171,941.667647058824));
#154837=CARTESIAN_POINT('Ctrl Pts',(5.4186249928073,13.9870834410653,940.173529411765));
#154838=CARTESIAN_POINT('Ctrl Pts',(6.71471914474792,13.4849738916136,938.679411764706));
#154839=CARTESIAN_POINT('Ctrl Pts',(7.89648244316034,12.7532570359442,937.185294117647));
#154840=CARTESIAN_POINT('Ctrl Pts',(9.07824574157275,12.0215401802748,935.691176470589));
#154841=CARTESIAN_POINT('Ctrl Pts',(10.1054346546984,11.0851337583099,934.19705882353));
#154842=CARTESIAN_POINT('Ctrl Pts',(11.132623567824,10.148727336345,932.702941176471));
#154843=CARTESIAN_POINT('Ctrl Pts',(11.9702584092036,9.03951954568885,931.208823529412));
#154844=CARTESIAN_POINT('Ctrl Pts',(12.8078932505832,7.93031175503273,929.714705882353));
#154845=CARTESIAN_POINT('Ctrl Pts',(13.4274493703259,6.68607533664807,928.220588235294));
#154846=CARTESIAN_POINT('Ctrl Pts',(14.0470054900687,5.44183891826343,926.726470588235));
#154847=CARTESIAN_POINT('Ctrl Pts',(14.4273846475923,4.10494485108125,925.232352941176));
#154848=CARTESIAN_POINT('Ctrl Pts',(14.8077638051159,2.76805078389905,923.738235294118));
#154849=CARTESIAN_POINT('Ctrl Pts',(14.9360126444255,1.38402539194953,922.244117647059));
#154850=CARTESIAN_POINT('Ctrl Pts',(15.0642614837351,2.76725994113625E-15,
920.75));
#154851=CARTESIAN_POINT('Ctrl Pts',(14.9360126444255,-1.38402539194952,
919.255882352941));
#154852=CARTESIAN_POINT('Ctrl Pts',(14.8077638051159,-2.76805078389906,
917.761764705882));
#154853=CARTESIAN_POINT('Ctrl Pts',(14.4273846475923,-4.10494485108124,
916.267647058824));
#154854=CARTESIAN_POINT('Ctrl Pts',(14.0470054900687,-5.44183891826342,
914.773529411765));
#154855=CARTESIAN_POINT('Ctrl Pts',(13.4274493703259,-6.68607533664808,
913.279411764706));
#154856=CARTESIAN_POINT('Ctrl Pts',(12.8078932505832,-7.93031175503273,
911.785294117647));
#154857=CARTESIAN_POINT('Ctrl Pts',(11.9702584092036,-9.03951954568884,
910.291176470588));
#154858=CARTESIAN_POINT('Ctrl Pts',(11.132623567824,-10.148727336345,908.797058823529));
#154859=CARTESIAN_POINT('Ctrl Pts',(10.1054346546984,-11.0851337583099,
907.302941176471));
#154860=CARTESIAN_POINT('Ctrl Pts',(9.07824574157275,-12.0215401802748,
905.808823529412));
#154861=CARTESIAN_POINT('Ctrl Pts',(7.89648244316034,-12.7532570359442,
904.314705882353));
#154862=CARTESIAN_POINT('Ctrl Pts',(6.71471914474792,-13.4849738916136,
902.820588235294));
#154863=CARTESIAN_POINT('Ctrl Pts',(5.4186249928073,-13.9870834410653,901.326470588235));
#154864=CARTESIAN_POINT('Ctrl Pts',(4.12253084086667,-14.4891929905171,
899.832352941177));
#154865=CARTESIAN_POINT('Ctrl Pts',(2.75624276724855,-14.7445964952585,
898.338235294118));
#154866=CARTESIAN_POINT('Ctrl Pts',(1.38995469363045,-15.,896.844117647059));
#154867=CARTESIAN_POINT('Ctrl Pts',(0.,-15.,895.35));
#154868=CARTESIAN_POINT('Ctrl Pts',(-1.38995469363045,-15.,893.855882352941));
#154869=CARTESIAN_POINT('Ctrl Pts',(-2.75624276724856,-14.7445964952585,
892.361764705882));
#154870=CARTESIAN_POINT('Ctrl Pts',(-4.12253084086666,-14.4891929905171,
890.867647058824));
#154871=CARTESIAN_POINT('Ctrl Pts',(-5.41862499280729,-13.9870834410653,
889.373529411765));
#154872=CARTESIAN_POINT('Ctrl Pts',(-6.71471914474793,-13.4849738916136,
887.879411764706));
#154873=CARTESIAN_POINT('Ctrl Pts',(-7.89648244316034,-12.7532570359442,
886.385294117647));
#154874=CARTESIAN_POINT('Ctrl Pts',(-9.07824574157275,-12.0215401802748,
884.891176470588));
#154875=CARTESIAN_POINT('Ctrl Pts',(-10.1054346546984,-11.0851337583099,
883.39705882353));
#154876=CARTESIAN_POINT('Ctrl Pts',(-11.132623567824,-10.148727336345,881.902941176471));
#154877=CARTESIAN_POINT('Ctrl Pts',(-11.9702584092036,-9.03951954568885,
880.408823529412));
#154878=CARTESIAN_POINT('Ctrl Pts',(-12.8078932505832,-7.93031175503273,
878.914705882353));
#154879=CARTESIAN_POINT('Ctrl Pts',(-13.4274493703259,-6.68607533664808,
877.420588235294));
#154880=CARTESIAN_POINT('Ctrl Pts',(-14.0470054900687,-5.44183891826343,
875.926470588235));
#154881=CARTESIAN_POINT('Ctrl Pts',(-14.4273846475923,-4.10494485108124,
874.432352941177));
#154882=CARTESIAN_POINT('Ctrl Pts',(-14.8077638051159,-2.76805078389906,
872.938235294118));
#154883=CARTESIAN_POINT('Ctrl Pts',(-14.9360126444255,-1.38402539194953,
871.444117647059));
#154884=CARTESIAN_POINT('Ctrl Pts',(-15.0642614837351,-9.22419980378748E-16,
869.95));
#154885=CARTESIAN_POINT('Ctrl Pts',(-14.9360126444255,1.38402539194953,
868.455882352941));
#154886=CARTESIAN_POINT('Ctrl Pts',(-14.8077638051159,2.76805078389906,
866.961764705882));
#154887=CARTESIAN_POINT('Ctrl Pts',(-14.4273846475923,4.10494485108124,
865.467647058824));
#154888=CARTESIAN_POINT('Ctrl Pts',(-14.0470054900687,5.44183891826343,
863.973529411765));
#154889=CARTESIAN_POINT('Ctrl Pts',(-13.4274493703259,6.68607533664807,
862.479411764706));
#154890=CARTESIAN_POINT('Ctrl Pts',(-12.8078932505832,7.93031175503273,
860.985294117647));
#154891=CARTESIAN_POINT('Ctrl Pts',(-11.9702584092036,9.03951954568884,
859.491176470588));
#154892=CARTESIAN_POINT('Ctrl Pts',(-11.132623567824,10.148727336345,857.997058823529));
#154893=CARTESIAN_POINT('Ctrl Pts',(-10.1054346546984,11.0851337583099,
856.502941176471));
#154894=CARTESIAN_POINT('Ctrl Pts',(-9.07824574157275,12.0215401802748,
855.008823529412));
#154895=CARTESIAN_POINT('Ctrl Pts',(-7.89648244316034,12.7532570359442,
853.514705882353));
#154896=CARTESIAN_POINT('Ctrl Pts',(-6.71471914474793,13.4849738916136,
852.020588235294));
#154897=CARTESIAN_POINT('Ctrl Pts',(-5.41862499280729,13.9870834410653,
850.526470588235));
#154898=CARTESIAN_POINT('Ctrl Pts',(-4.12253084086667,14.4891929905171,
849.032352941177));
#154899=CARTESIAN_POINT('Ctrl Pts',(-2.75624276724856,14.7445964952585,
847.538235294118));
#154900=CARTESIAN_POINT('Ctrl Pts',(-1.38995469363044,15.,846.044117647059));
#154901=CARTESIAN_POINT('Ctrl Pts',(-1.83697019872103E-15,15.,844.55));
#154902=CARTESIAN_POINT('Ctrl Pts',(1.38995469363045,15.,843.055882352941));
#154903=CARTESIAN_POINT('Ctrl Pts',(2.75624276724855,14.7445964952585,841.561764705883));
#154904=CARTESIAN_POINT('Ctrl Pts',(4.12253084086666,14.4891929905171,840.067647058824));
#154905=CARTESIAN_POINT('Ctrl Pts',(5.4186249928073,13.9870834410653,838.573529411765));
#154906=CARTESIAN_POINT('Ctrl Pts',(6.71471914474792,13.4849738916136,837.079411764706));
#154907=CARTESIAN_POINT('Ctrl Pts',(7.89648244316034,12.7532570359442,835.585294117647));
#154908=CARTESIAN_POINT('Ctrl Pts',(9.07824574157275,12.0215401802748,834.091176470588));
#154909=CARTESIAN_POINT('Ctrl Pts',(10.1054346546984,11.0851337583099,832.597058823529));
#154910=CARTESIAN_POINT('Ctrl Pts',(11.132623567824,10.148727336345,831.102941176471));
#154911=CARTESIAN_POINT('Ctrl Pts',(11.9702584092036,9.03951954568885,829.608823529412));
#154912=CARTESIAN_POINT('Ctrl Pts',(12.8078932505832,7.93031175503273,828.114705882353));
#154913=CARTESIAN_POINT('Ctrl Pts',(13.4274493703259,6.68607533664807,826.620588235294));
#154914=CARTESIAN_POINT('Ctrl Pts',(14.0470054900687,5.44183891826343,825.126470588235));
#154915=CARTESIAN_POINT('Ctrl Pts',(14.4273846475923,4.10494485108125,823.632352941177));
#154916=CARTESIAN_POINT('Ctrl Pts',(14.8077638051159,2.76805078389905,822.138235294118));
#154917=CARTESIAN_POINT('Ctrl Pts',(14.9360126444255,1.38402539194953,820.644117647059));
#154918=CARTESIAN_POINT('Ctrl Pts',(15.0642614837351,2.76725994113625E-15,
819.15));
#154919=CARTESIAN_POINT('Ctrl Pts',(14.9360126444255,-1.38402539194952,
817.655882352941));
#154920=CARTESIAN_POINT('Ctrl Pts',(14.8077638051159,-2.76805078389906,
816.161764705882));
#154921=CARTESIAN_POINT('Ctrl Pts',(14.4273846475923,-4.10494485108124,
814.667647058824));
#154922=CARTESIAN_POINT('Ctrl Pts',(14.0470054900687,-5.44183891826342,
813.173529411765));
#154923=CARTESIAN_POINT('Ctrl Pts',(13.4274493703259,-6.68607533664808,
811.679411764706));
#154924=CARTESIAN_POINT('Ctrl Pts',(12.8078932505832,-7.93031175503273,
810.185294117647));
#154925=CARTESIAN_POINT('Ctrl Pts',(11.9702584092036,-9.03951954568884,
808.691176470588));
#154926=CARTESIAN_POINT('Ctrl Pts',(11.132623567824,-10.148727336345,807.197058823529));
#154927=CARTESIAN_POINT('Ctrl Pts',(10.1054346546984,-11.0851337583099,
805.702941176471));
#154928=CARTESIAN_POINT('Ctrl Pts',(9.07824574157275,-12.0215401802748,
804.208823529412));
#154929=CARTESIAN_POINT('Ctrl Pts',(7.89648244316034,-12.7532570359442,
802.714705882353));
#154930=CARTESIAN_POINT('Ctrl Pts',(6.71471914474792,-13.4849738916136,
801.220588235294));
#154931=CARTESIAN_POINT('Ctrl Pts',(5.4186249928073,-13.9870834410653,799.726470588235));
#154932=CARTESIAN_POINT('Ctrl Pts',(4.12253084086667,-14.4891929905171,
798.232352941176));
#154933=CARTESIAN_POINT('Ctrl Pts',(2.75624276724855,-14.7445964952585,
796.738235294118));
#154934=CARTESIAN_POINT('Ctrl Pts',(1.38995469363045,-15.,795.244117647059));
#154935=CARTESIAN_POINT('Ctrl Pts',(0.,-15.,793.75));
#154936=CARTESIAN_POINT('Ctrl Pts',(-1.38995469363045,-15.,792.255882352941));
#154937=CARTESIAN_POINT('Ctrl Pts',(-2.75624276724856,-14.7445964952585,
790.761764705882));
#154938=CARTESIAN_POINT('Ctrl Pts',(-4.12253084086666,-14.4891929905171,
789.267647058824));
#154939=CARTESIAN_POINT('Ctrl Pts',(-5.41862499280729,-13.9870834410653,
787.773529411765));
#154940=CARTESIAN_POINT('Ctrl Pts',(-6.71471914474793,-13.4849738916136,
786.279411764706));
#154941=CARTESIAN_POINT('Ctrl Pts',(-7.89648244316034,-12.7532570359442,
784.785294117647));
#154942=CARTESIAN_POINT('Ctrl Pts',(-9.07824574157275,-12.0215401802748,
783.291176470588));
#154943=CARTESIAN_POINT('Ctrl Pts',(-10.1054346546984,-11.0851337583099,
781.797058823529));
#154944=CARTESIAN_POINT('Ctrl Pts',(-11.132623567824,-10.148727336345,780.302941176471));
#154945=CARTESIAN_POINT('Ctrl Pts',(-11.9702584092036,-9.03951954568885,
778.808823529412));
#154946=CARTESIAN_POINT('Ctrl Pts',(-12.8078932505832,-7.93031175503273,
777.314705882353));
#154947=CARTESIAN_POINT('Ctrl Pts',(-13.4274493703259,-6.68607533664808,
775.820588235294));
#154948=CARTESIAN_POINT('Ctrl Pts',(-14.0470054900687,-5.44183891826343,
774.326470588235));
#154949=CARTESIAN_POINT('Ctrl Pts',(-14.4273846475923,-4.10494485108124,
772.832352941177));
#154950=CARTESIAN_POINT('Ctrl Pts',(-14.8077638051159,-2.76805078389906,
771.338235294118));
#154951=CARTESIAN_POINT('Ctrl Pts',(-14.9360126444255,-1.38402539194953,
769.844117647059));
#154952=CARTESIAN_POINT('Ctrl Pts',(-15.0642614837351,-9.22419980378748E-16,
768.35));
#154953=CARTESIAN_POINT('Ctrl Pts',(-14.9360126444255,1.38402539194953,
766.855882352941));
#154954=CARTESIAN_POINT('Ctrl Pts',(-14.8077638051159,2.76805078389906,
765.361764705882));
#154955=CARTESIAN_POINT('Ctrl Pts',(-14.4273846475923,4.10494485108124,
763.867647058824));
#154956=CARTESIAN_POINT('Ctrl Pts',(-14.0470054900687,5.44183891826343,
762.373529411765));
#154957=CARTESIAN_POINT('Ctrl Pts',(-13.4274493703259,6.68607533664807,
760.879411764706));
#154958=CARTESIAN_POINT('Ctrl Pts',(-12.8078932505832,7.93031175503273,
759.385294117647));
#154959=CARTESIAN_POINT('Ctrl Pts',(-11.9702584092036,9.03951954568884,
757.891176470588));
#154960=CARTESIAN_POINT('Ctrl Pts',(-11.132623567824,10.148727336345,756.397058823529));
#154961=CARTESIAN_POINT('Ctrl Pts',(-10.1054346546984,11.0851337583099,
754.902941176471));
#154962=CARTESIAN_POINT('Ctrl Pts',(-9.07824574157275,12.0215401802748,
753.408823529412));
#154963=CARTESIAN_POINT('Ctrl Pts',(-7.89648244316034,12.7532570359442,
751.914705882353));
#154964=CARTESIAN_POINT('Ctrl Pts',(-6.71471914474793,13.4849738916136,
750.420588235294));
#154965=CARTESIAN_POINT('Ctrl Pts',(-5.41862499280729,13.9870834410653,
748.926470588235));
#154966=CARTESIAN_POINT('Ctrl Pts',(-4.12253084086667,14.4891929905171,
747.432352941176));
#154967=CARTESIAN_POINT('Ctrl Pts',(-2.75624276724856,14.7445964952585,
745.938235294118));
#154968=CARTESIAN_POINT('Ctrl Pts',(-1.38995469363044,15.,744.444117647059));
#154969=CARTESIAN_POINT('Ctrl Pts',(-1.83697019872103E-15,15.,742.95));
#154970=CARTESIAN_POINT('Ctrl Pts',(1.38995469363045,15.,741.455882352941));
#154971=CARTESIAN_POINT('Ctrl Pts',(2.75624276724855,14.7445964952585,739.961764705882));
#154972=CARTESIAN_POINT('Ctrl Pts',(4.12253084086666,14.4891929905171,738.467647058824));
#154973=CARTESIAN_POINT('Ctrl Pts',(5.4186249928073,13.9870834410653,736.973529411765));
#154974=CARTESIAN_POINT('Ctrl Pts',(6.71471914474792,13.4849738916136,735.479411764706));
#154975=CARTESIAN_POINT('Ctrl Pts',(7.89648244316034,12.7532570359442,733.985294117647));
#154976=CARTESIAN_POINT('Ctrl Pts',(9.07824574157275,12.0215401802748,732.491176470588));
#154977=CARTESIAN_POINT('Ctrl Pts',(10.1054346546984,11.0851337583099,730.99705882353));
#154978=CARTESIAN_POINT('Ctrl Pts',(11.132623567824,10.148727336345,729.502941176471));
#154979=CARTESIAN_POINT('Ctrl Pts',(11.9702584092036,9.03951954568885,728.008823529412));
#154980=CARTESIAN_POINT('Ctrl Pts',(12.8078932505832,7.93031175503273,726.514705882353));
#154981=CARTESIAN_POINT('Ctrl Pts',(13.4274493703259,6.68607533664807,725.020588235294));
#154982=CARTESIAN_POINT('Ctrl Pts',(14.0470054900687,5.44183891826343,723.526470588235));
#154983=CARTESIAN_POINT('Ctrl Pts',(14.4273846475923,4.10494485108125,722.032352941177));
#154984=CARTESIAN_POINT('Ctrl Pts',(14.8077638051159,2.76805078389905,720.538235294118));
#154985=CARTESIAN_POINT('Ctrl Pts',(14.9360126444255,1.38402539194953,719.044117647059));
#154986=CARTESIAN_POINT('Ctrl Pts',(15.0642614837351,2.76725994113625E-15,
717.55));
#154987=CARTESIAN_POINT('Ctrl Pts',(14.9360126444255,-1.38402539194952,
716.055882352941));
#154988=CARTESIAN_POINT('Ctrl Pts',(14.8077638051159,-2.76805078389906,
714.561764705882));
#154989=CARTESIAN_POINT('Ctrl Pts',(14.4273846475923,-4.10494485108124,
713.067647058824));
#154990=CARTESIAN_POINT('Ctrl Pts',(14.0470054900687,-5.44183891826342,
711.573529411765));
#154991=CARTESIAN_POINT('Ctrl Pts',(13.4274493703259,-6.68607533664808,
710.079411764706));
#154992=CARTESIAN_POINT('Ctrl Pts',(12.8078932505832,-7.93031175503273,
708.585294117647));
#154993=CARTESIAN_POINT('Ctrl Pts',(11.9702584092036,-9.03951954568884,
707.091176470588));
#154994=CARTESIAN_POINT('Ctrl Pts',(11.132623567824,-10.148727336345,705.597058823529));
#154995=CARTESIAN_POINT('Ctrl Pts',(10.1054346546984,-11.0851337583099,
704.102941176471));
#154996=CARTESIAN_POINT('Ctrl Pts',(9.07824574157275,-12.0215401802748,
702.608823529412));
#154997=CARTESIAN_POINT('Ctrl Pts',(7.89648244316034,-12.7532570359442,
701.114705882353));
#154998=CARTESIAN_POINT('Ctrl Pts',(6.71471914474792,-13.4849738916136,
699.620588235294));
#154999=CARTESIAN_POINT('Ctrl Pts',(5.4186249928073,-13.9870834410653,698.126470588235));
#155000=CARTESIAN_POINT('Ctrl Pts',(4.12253084086667,-14.4891929905171,
696.632352941177));
#155001=CARTESIAN_POINT('Ctrl Pts',(2.75624276724855,-14.7445964952585,
695.138235294118));
#155002=CARTESIAN_POINT('Ctrl Pts',(1.38995469363045,-15.,693.644117647059));
#155003=CARTESIAN_POINT('Ctrl Pts',(0.,-15.,692.15));
#155004=CARTESIAN_POINT('Ctrl Pts',(-1.38995469363045,-15.,690.655882352941));
#155005=CARTESIAN_POINT('Ctrl Pts',(-2.75624276724856,-14.7445964952585,
689.161764705882));
#155006=CARTESIAN_POINT('Ctrl Pts',(-4.12253084086666,-14.4891929905171,
687.667647058824));
#155007=CARTESIAN_POINT('Ctrl Pts',(-5.41862499280729,-13.9870834410653,
686.173529411765));
#155008=CARTESIAN_POINT('Ctrl Pts',(-6.71471914474793,-13.4849738916136,
684.679411764706));
#155009=CARTESIAN_POINT('Ctrl Pts',(-7.89648244316034,-12.7532570359442,
683.185294117647));
#155010=CARTESIAN_POINT('Ctrl Pts',(-9.07824574157275,-12.0215401802748,
681.691176470588));
#155011=CARTESIAN_POINT('Ctrl Pts',(-10.1054346546984,-11.0851337583099,
680.197058823529));
#155012=CARTESIAN_POINT('Ctrl Pts',(-11.132623567824,-10.148727336345,678.702941176471));
#155013=CARTESIAN_POINT('Ctrl Pts',(-11.9702584092036,-9.03951954568885,
677.208823529412));
#155014=CARTESIAN_POINT('Ctrl Pts',(-12.8078932505832,-7.93031175503273,
675.714705882353));
#155015=CARTESIAN_POINT('Ctrl Pts',(-13.4274493703259,-6.68607533664808,
674.220588235294));
#155016=CARTESIAN_POINT('Ctrl Pts',(-14.0470054900687,-5.44183891826343,
672.726470588236));
#155017=CARTESIAN_POINT('Ctrl Pts',(-14.4273846475923,-4.10494485108124,
671.232352941176));
#155018=CARTESIAN_POINT('Ctrl Pts',(-14.8077638051159,-2.76805078389906,
669.738235294118));
#155019=CARTESIAN_POINT('Ctrl Pts',(-14.9360126444255,-1.38402539194953,
668.244117647059));
#155020=CARTESIAN_POINT('Ctrl Pts',(-15.0642614837351,-9.22419980378748E-16,
666.75));
#155021=CARTESIAN_POINT('Ctrl Pts',(-14.9360126444255,1.38402539194953,
665.255882352941));
#155022=CARTESIAN_POINT('Ctrl Pts',(-14.8077638051159,2.76805078389906,
663.761764705882));
#155023=CARTESIAN_POINT('Ctrl Pts',(-14.4273846475923,4.10494485108124,
662.267647058824));
#155024=CARTESIAN_POINT('Ctrl Pts',(-14.0470054900687,5.44183891826343,
660.773529411765));
#155025=CARTESIAN_POINT('Ctrl Pts',(-13.4274493703259,6.68607533664807,
659.279411764706));
#155026=CARTESIAN_POINT('Ctrl Pts',(-12.8078932505832,7.93031175503273,
657.785294117647));
#155027=CARTESIAN_POINT('Ctrl Pts',(-11.9702584092036,9.03951954568884,
656.291176470588));
#155028=CARTESIAN_POINT('Ctrl Pts',(-11.132623567824,10.148727336345,654.797058823529));
#155029=CARTESIAN_POINT('Ctrl Pts',(-10.1054346546984,11.0851337583099,
653.302941176471));
#155030=CARTESIAN_POINT('Ctrl Pts',(-9.07824574157275,12.0215401802748,
651.808823529412));
#155031=CARTESIAN_POINT('Ctrl Pts',(-7.89648244316034,12.7532570359442,
650.314705882353));
#155032=CARTESIAN_POINT('Ctrl Pts',(-6.71471914474793,13.4849738916136,
648.820588235294));
#155033=CARTESIAN_POINT('Ctrl Pts',(-5.41862499280729,13.9870834410653,
647.326470588235));
#155034=CARTESIAN_POINT('Ctrl Pts',(-4.12253084086667,14.4891929905171,
645.832352941176));
#155035=CARTESIAN_POINT('Ctrl Pts',(-2.75624276724856,14.7445964952585,
644.338235294118));
#155036=CARTESIAN_POINT('Ctrl Pts',(-1.38995469363044,15.,642.844117647059));
#155037=CARTESIAN_POINT('Ctrl Pts',(-1.83697019872103E-15,15.,641.35));
#155038=CARTESIAN_POINT('Ctrl Pts',(1.38995469363045,15.,639.855882352941));
#155039=CARTESIAN_POINT('Ctrl Pts',(2.75624276724855,14.7445964952585,638.361764705882));
#155040=CARTESIAN_POINT('Ctrl Pts',(4.12253084086666,14.4891929905171,636.867647058824));
#155041=CARTESIAN_POINT('Ctrl Pts',(5.4186249928073,13.9870834410653,635.373529411765));
#155042=CARTESIAN_POINT('Ctrl Pts',(6.71471914474792,13.4849738916136,633.879411764706));
#155043=CARTESIAN_POINT('Ctrl Pts',(7.89648244316034,12.7532570359442,632.385294117647));
#155044=CARTESIAN_POINT('Ctrl Pts',(9.07824574157275,12.0215401802748,630.891176470588));
#155045=CARTESIAN_POINT('Ctrl Pts',(10.1054346546984,11.0851337583099,629.39705882353));
#155046=CARTESIAN_POINT('Ctrl Pts',(11.132623567824,10.148727336345,627.902941176471));
#155047=CARTESIAN_POINT('Ctrl Pts',(11.9702584092036,9.03951954568885,626.408823529412));
#155048=CARTESIAN_POINT('Ctrl Pts',(12.8078932505832,7.93031175503273,624.914705882353));
#155049=CARTESIAN_POINT('Ctrl Pts',(13.4274493703259,6.68607533664807,623.420588235294));
#155050=CARTESIAN_POINT('Ctrl Pts',(14.0470054900687,5.44183891826343,621.926470588235));
#155051=CARTESIAN_POINT('Ctrl Pts',(14.4273846475923,4.10494485108125,620.432352941177));
#155052=CARTESIAN_POINT('Ctrl Pts',(14.8077638051159,2.76805078389905,618.938235294118));
#155053=CARTESIAN_POINT('Ctrl Pts',(14.9360126444255,1.38402539194953,617.444117647059));
#155054=CARTESIAN_POINT('Ctrl Pts',(15.0642614837351,2.76725994113625E-15,
615.95));
#155055=CARTESIAN_POINT('Ctrl Pts',(14.9360126444255,-1.38402539194952,
614.455882352941));
#155056=CARTESIAN_POINT('Ctrl Pts',(14.8077638051159,-2.76805078389906,
612.961764705883));
#155057=CARTESIAN_POINT('Ctrl Pts',(14.4273846475923,-4.10494485108124,
611.467647058824));
#155058=CARTESIAN_POINT('Ctrl Pts',(14.0470054900687,-5.44183891826342,
609.973529411765));
#155059=CARTESIAN_POINT('Ctrl Pts',(13.4274493703259,-6.68607533664808,
608.479411764706));
#155060=CARTESIAN_POINT('Ctrl Pts',(12.8078932505832,-7.93031175503273,
606.985294117647));
#155061=CARTESIAN_POINT('Ctrl Pts',(11.9702584092036,-9.03951954568884,
605.491176470588));
#155062=CARTESIAN_POINT('Ctrl Pts',(11.132623567824,-10.148727336345,603.997058823529));
#155063=CARTESIAN_POINT('Ctrl Pts',(10.1054346546984,-11.0851337583099,
602.502941176471));
#155064=CARTESIAN_POINT('Ctrl Pts',(9.07824574157275,-12.0215401802748,
601.008823529412));
#155065=CARTESIAN_POINT('Ctrl Pts',(7.89648244316034,-12.7532570359442,
599.514705882353));
#155066=CARTESIAN_POINT('Ctrl Pts',(6.71471914474792,-13.4849738916136,
598.020588235294));
#155067=CARTESIAN_POINT('Ctrl Pts',(5.4186249928073,-13.9870834410653,596.526470588235));
#155068=CARTESIAN_POINT('Ctrl Pts',(4.12253084086667,-14.4891929905171,
595.032352941176));
#155069=CARTESIAN_POINT('Ctrl Pts',(2.75624276724855,-14.7445964952585,
593.538235294118));
#155070=CARTESIAN_POINT('Ctrl Pts',(1.38995469363045,-15.,592.044117647059));
#155071=CARTESIAN_POINT('Ctrl Pts',(0.,-15.,590.55));
#155072=CARTESIAN_POINT('Ctrl Pts',(-1.38995469363045,-15.,589.055882352941));
#155073=CARTESIAN_POINT('Ctrl Pts',(-2.75624276724856,-14.7445964952585,
587.561764705882));
#155074=CARTESIAN_POINT('Ctrl Pts',(-4.12253084086666,-14.4891929905171,
586.067647058823));
#155075=CARTESIAN_POINT('Ctrl Pts',(-5.41862499280729,-13.9870834410653,
584.573529411765));
#155076=CARTESIAN_POINT('Ctrl Pts',(-6.71471914474793,-13.4849738916136,
583.079411764706));
#155077=CARTESIAN_POINT('Ctrl Pts',(-7.89648244316034,-12.7532570359442,
581.585294117647));
#155078=CARTESIAN_POINT('Ctrl Pts',(-9.07824574157275,-12.0215401802748,
580.091176470588));
#155079=CARTESIAN_POINT('Ctrl Pts',(-10.1054346546984,-11.0851337583099,
578.597058823529));
#155080=CARTESIAN_POINT('Ctrl Pts',(-11.132623567824,-10.148727336345,577.102941176471));
#155081=CARTESIAN_POINT('Ctrl Pts',(-11.9702584092036,-9.03951954568885,
575.608823529412));
#155082=CARTESIAN_POINT('Ctrl Pts',(-12.8078932505832,-7.93031175503273,
574.114705882353));
#155083=CARTESIAN_POINT('Ctrl Pts',(-13.4274493703259,-6.68607533664808,
572.620588235294));
#155084=CARTESIAN_POINT('Ctrl Pts',(-14.0470054900687,-5.44183891826343,
571.126470588235));
#155085=CARTESIAN_POINT('Ctrl Pts',(-14.4273846475923,-4.10494485108124,
569.632352941177));
#155086=CARTESIAN_POINT('Ctrl Pts',(-14.8077638051159,-2.76805078389906,
568.138235294118));
#155087=CARTESIAN_POINT('Ctrl Pts',(-14.9360126444255,-1.38402539194953,
566.644117647059));
#155088=CARTESIAN_POINT('Ctrl Pts',(-15.0642614837351,-9.22419980378748E-16,
565.15));
#155089=CARTESIAN_POINT('Ctrl Pts',(-14.9360126444255,1.38402539194953,
563.655882352941));
#155090=CARTESIAN_POINT('Ctrl Pts',(-14.8077638051159,2.76805078389906,
562.161764705883));
#155091=CARTESIAN_POINT('Ctrl Pts',(-14.4273846475923,4.10494485108124,
560.667647058824));
#155092=CARTESIAN_POINT('Ctrl Pts',(-14.0470054900687,5.44183891826343,
559.173529411765));
#155093=CARTESIAN_POINT('Ctrl Pts',(-13.4274493703259,6.68607533664807,
557.679411764706));
#155094=CARTESIAN_POINT('Ctrl Pts',(-12.8078932505832,7.93031175503273,
556.185294117647));
#155095=CARTESIAN_POINT('Ctrl Pts',(-11.9702584092036,9.03951954568884,
554.691176470588));
#155096=CARTESIAN_POINT('Ctrl Pts',(-11.132623567824,10.148727336345,553.19705882353));
#155097=CARTESIAN_POINT('Ctrl Pts',(-10.1054346546984,11.0851337583099,
551.702941176471));
#155098=CARTESIAN_POINT('Ctrl Pts',(-9.07824574157275,12.0215401802748,
550.208823529412));
#155099=CARTESIAN_POINT('Ctrl Pts',(-7.89648244316034,12.7532570359442,
548.714705882353));
#155100=CARTESIAN_POINT('Ctrl Pts',(-6.71471914474793,13.4849738916136,
547.220588235294));
#155101=CARTESIAN_POINT('Ctrl Pts',(-5.41862499280729,13.9870834410653,
545.726470588235));
#155102=CARTESIAN_POINT('Ctrl Pts',(-4.12253084086667,14.4891929905171,
544.232352941176));
#155103=CARTESIAN_POINT('Ctrl Pts',(-2.75624276724856,14.7445964952585,
542.738235294118));
#155104=CARTESIAN_POINT('Ctrl Pts',(-1.38995469363044,15.,541.244117647059));
#155105=CARTESIAN_POINT('Ctrl Pts',(-1.83697019872103E-15,15.,539.75));
#155106=CARTESIAN_POINT('Ctrl Pts',(1.38995469363045,15.,538.255882352941));
#155107=CARTESIAN_POINT('Ctrl Pts',(2.75624276724855,14.7445964952585,536.761764705882));
#155108=CARTESIAN_POINT('Ctrl Pts',(4.12253084086666,14.4891929905171,535.267647058824));
#155109=CARTESIAN_POINT('Ctrl Pts',(5.4186249928073,13.9870834410653,533.773529411765));
#155110=CARTESIAN_POINT('Ctrl Pts',(6.71471914474792,13.4849738916136,532.279411764706));
#155111=CARTESIAN_POINT('Ctrl Pts',(7.89648244316034,12.7532570359442,530.785294117647));
#155112=CARTESIAN_POINT('Ctrl Pts',(9.07824574157275,12.0215401802748,529.291176470588));
#155113=CARTESIAN_POINT('Ctrl Pts',(10.1054346546984,11.0851337583099,527.797058823529));
#155114=CARTESIAN_POINT('Ctrl Pts',(11.132623567824,10.148727336345,526.302941176471));
#155115=CARTESIAN_POINT('Ctrl Pts',(11.9702584092036,9.03951954568885,524.808823529412));
#155116=CARTESIAN_POINT('Ctrl Pts',(12.8078932505832,7.93031175503273,523.314705882353));
#155117=CARTESIAN_POINT('Ctrl Pts',(13.4274493703259,6.68607533664807,521.820588235294));
#155118=CARTESIAN_POINT('Ctrl Pts',(14.0470054900687,5.44183891826343,520.326470588235));
#155119=CARTESIAN_POINT('Ctrl Pts',(14.4273846475923,4.10494485108125,518.832352941177));
#155120=CARTESIAN_POINT('Ctrl Pts',(14.8077638051159,2.76805078389905,517.338235294118));
#155121=CARTESIAN_POINT('Ctrl Pts',(14.9360126444255,1.38402539194953,515.844117647059));
#155122=CARTESIAN_POINT('Ctrl Pts',(15.0642614837351,2.76725994113625E-15,
514.35));
#155123=CARTESIAN_POINT('Ctrl Pts',(14.9360126444255,-1.38402539194952,
512.855882352941));
#155124=CARTESIAN_POINT('Ctrl Pts',(14.8077638051159,-2.76805078389906,
511.361764705882));
#155125=CARTESIAN_POINT('Ctrl Pts',(14.4273846475923,-4.10494485108124,
509.867647058824));
#155126=CARTESIAN_POINT('Ctrl Pts',(14.0470054900687,-5.44183891826342,
508.373529411765));
#155127=CARTESIAN_POINT('Ctrl Pts',(13.4274493703259,-6.68607533664808,
506.879411764706));
#155128=CARTESIAN_POINT('Ctrl Pts',(12.8078932505832,-7.93031175503273,
505.385294117647));
#155129=CARTESIAN_POINT('Ctrl Pts',(11.9702584092036,-9.03951954568884,
503.891176470588));
#155130=CARTESIAN_POINT('Ctrl Pts',(11.132623567824,-10.148727336345,502.39705882353));
#155131=CARTESIAN_POINT('Ctrl Pts',(10.1054346546984,-11.0851337583099,
500.902941176471));
#155132=CARTESIAN_POINT('Ctrl Pts',(9.07824574157275,-12.0215401802748,
499.408823529412));
#155133=CARTESIAN_POINT('Ctrl Pts',(7.89648244316034,-12.7532570359442,
497.914705882353));
#155134=CARTESIAN_POINT('Ctrl Pts',(6.71471914474792,-13.4849738916136,
496.420588235294));
#155135=CARTESIAN_POINT('Ctrl Pts',(5.4186249928073,-13.9870834410653,494.926470588235));
#155136=CARTESIAN_POINT('Ctrl Pts',(4.12253084086667,-14.4891929905171,
493.432352941177));
#155137=CARTESIAN_POINT('Ctrl Pts',(2.75624276724855,-14.7445964952585,
491.938235294118));
#155138=CARTESIAN_POINT('Ctrl Pts',(1.38995469363045,-15.,490.444117647059));
#155139=CARTESIAN_POINT('Ctrl Pts',(0.,-15.,488.95));
#155140=CARTESIAN_POINT('Ctrl Pts',(-1.38995469363045,-15.,487.455882352941));
#155141=CARTESIAN_POINT('Ctrl Pts',(-2.75624276724856,-14.7445964952585,
485.961764705883));
#155142=CARTESIAN_POINT('Ctrl Pts',(-4.12253084086666,-14.4891929905171,
484.467647058824));
#155143=CARTESIAN_POINT('Ctrl Pts',(-5.41862499280729,-13.9870834410653,
482.973529411765));
#155144=CARTESIAN_POINT('Ctrl Pts',(-6.71471914474793,-13.4849738916136,
481.479411764706));
#155145=CARTESIAN_POINT('Ctrl Pts',(-7.89648244316034,-12.7532570359442,
479.985294117647));
#155146=CARTESIAN_POINT('Ctrl Pts',(-9.07824574157275,-12.0215401802748,
478.491176470588));
#155147=CARTESIAN_POINT('Ctrl Pts',(-10.1054346546984,-11.0851337583099,
476.99705882353));
#155148=CARTESIAN_POINT('Ctrl Pts',(-11.132623567824,-10.148727336345,475.502941176471));
#155149=CARTESIAN_POINT('Ctrl Pts',(-11.9702584092036,-9.03951954568885,
474.008823529412));
#155150=CARTESIAN_POINT('Ctrl Pts',(-12.8078932505832,-7.93031175503273,
472.514705882353));
#155151=CARTESIAN_POINT('Ctrl Pts',(-13.4274493703259,-6.68607533664808,
471.020588235294));
#155152=CARTESIAN_POINT('Ctrl Pts',(-14.0470054900687,-5.44183891826343,
469.526470588235));
#155153=CARTESIAN_POINT('Ctrl Pts',(-14.4273846475923,-4.10494485108124,
468.032352941177));
#155154=CARTESIAN_POINT('Ctrl Pts',(-14.8077638051159,-2.76805078389906,
466.538235294118));
#155155=CARTESIAN_POINT('Ctrl Pts',(-14.9360126444255,-1.38402539194953,
465.044117647059));
#155156=CARTESIAN_POINT('Ctrl Pts',(-15.0642614837351,-9.22419980378748E-16,
463.55));
#155157=CARTESIAN_POINT('Ctrl Pts',(-14.9360126444255,1.38402539194953,
462.055882352941));
#155158=CARTESIAN_POINT('Ctrl Pts',(-14.8077638051159,2.76805078389906,
460.561764705882));
#155159=CARTESIAN_POINT('Ctrl Pts',(-14.4273846475923,4.10494485108124,
459.067647058824));
#155160=CARTESIAN_POINT('Ctrl Pts',(-14.0470054900687,5.44183891826343,
457.573529411765));
#155161=CARTESIAN_POINT('Ctrl Pts',(-13.4274493703259,6.68607533664807,
456.079411764706));
#155162=CARTESIAN_POINT('Ctrl Pts',(-12.8078932505832,7.93031175503273,
454.585294117647));
#155163=CARTESIAN_POINT('Ctrl Pts',(-11.9702584092036,9.03951954568884,
453.091176470588));
#155164=CARTESIAN_POINT('Ctrl Pts',(-11.132623567824,10.148727336345,451.597058823529));
#155165=CARTESIAN_POINT('Ctrl Pts',(-10.1054346546984,11.0851337583099,
450.102941176471));
#155166=CARTESIAN_POINT('Ctrl Pts',(-9.07824574157275,12.0215401802748,
448.608823529412));
#155167=CARTESIAN_POINT('Ctrl Pts',(-7.89648244316034,12.7532570359442,
447.114705882353));
#155168=CARTESIAN_POINT('Ctrl Pts',(-6.71471914474793,13.4849738916136,
445.620588235294));
#155169=CARTESIAN_POINT('Ctrl Pts',(-5.41862499280729,13.9870834410653,
444.126470588235));
#155170=CARTESIAN_POINT('Ctrl Pts',(-4.12253084086667,14.4891929905171,
442.632352941176));
#155171=CARTESIAN_POINT('Ctrl Pts',(-2.75624276724856,14.7445964952585,
441.138235294118));
#155172=CARTESIAN_POINT('Ctrl Pts',(-1.38995469363044,15.,439.644117647059));
#155173=CARTESIAN_POINT('Ctrl Pts',(-1.83697019872103E-15,15.,438.15));
#155174=CARTESIAN_POINT('Ctrl Pts',(1.38995469363045,15.,436.655882352941));
#155175=CARTESIAN_POINT('Ctrl Pts',(2.75624276724855,14.7445964952585,435.161764705882));
#155176=CARTESIAN_POINT('Ctrl Pts',(4.12253084086666,14.4891929905171,433.667647058824));
#155177=CARTESIAN_POINT('Ctrl Pts',(5.4186249928073,13.9870834410653,432.173529411765));
#155178=CARTESIAN_POINT('Ctrl Pts',(6.71471914474792,13.4849738916136,430.679411764706));
#155179=CARTESIAN_POINT('Ctrl Pts',(7.89648244316034,12.7532570359442,429.185294117647));
#155180=CARTESIAN_POINT('Ctrl Pts',(9.07824574157275,12.0215401802748,427.691176470588));
#155181=CARTESIAN_POINT('Ctrl Pts',(10.1054346546984,11.0851337583099,426.19705882353));
#155182=CARTESIAN_POINT('Ctrl Pts',(11.132623567824,10.148727336345,424.702941176471));
#155183=CARTESIAN_POINT('Ctrl Pts',(11.9702584092036,9.03951954568885,423.208823529412));
#155184=CARTESIAN_POINT('Ctrl Pts',(12.8078932505832,7.93031175503273,421.714705882353));
#155185=CARTESIAN_POINT('Ctrl Pts',(13.4274493703259,6.68607533664807,420.220588235294));
#155186=CARTESIAN_POINT('Ctrl Pts',(14.0470054900687,5.44183891826343,418.726470588235));
#155187=CARTESIAN_POINT('Ctrl Pts',(14.4273846475923,4.10494485108125,417.232352941177));
#155188=CARTESIAN_POINT('Ctrl Pts',(14.8077638051159,2.76805078389905,415.738235294118));
#155189=CARTESIAN_POINT('Ctrl Pts',(14.9360126444255,1.38402539194953,414.244117647059));
#155190=CARTESIAN_POINT('Ctrl Pts',(15.0642614837351,2.76725994113625E-15,
412.75));
#155191=CARTESIAN_POINT('Ctrl Pts',(14.9360126444255,-1.38402539194952,
411.255882352941));
#155192=CARTESIAN_POINT('Ctrl Pts',(14.8077638051159,-2.76805078389906,
409.761764705883));
#155193=CARTESIAN_POINT('Ctrl Pts',(14.4273846475923,-4.10494485108124,
408.267647058824));
#155194=CARTESIAN_POINT('Ctrl Pts',(14.0470054900687,-5.44183891826342,
406.773529411765));
#155195=CARTESIAN_POINT('Ctrl Pts',(13.4274493703259,-6.68607533664808,
405.279411764706));
#155196=CARTESIAN_POINT('Ctrl Pts',(12.8078932505832,-7.93031175503273,
403.785294117647));
#155197=CARTESIAN_POINT('Ctrl Pts',(11.9702584092036,-9.03951954568884,
402.291176470588));
#155198=CARTESIAN_POINT('Ctrl Pts',(11.132623567824,-10.148727336345,400.797058823529));
#155199=CARTESIAN_POINT('Ctrl Pts',(10.1054346546984,-11.0851337583099,
399.302941176471));
#155200=CARTESIAN_POINT('Ctrl Pts',(9.07824574157275,-12.0215401802748,
397.808823529412));
#155201=CARTESIAN_POINT('Ctrl Pts',(7.89648244316034,-12.7532570359442,
396.314705882353));
#155202=CARTESIAN_POINT('Ctrl Pts',(6.71471914474792,-13.4849738916136,
394.820588235294));
#155203=CARTESIAN_POINT('Ctrl Pts',(5.4186249928073,-13.9870834410653,393.326470588235));
#155204=CARTESIAN_POINT('Ctrl Pts',(4.12253084086667,-14.4891929905171,
391.832352941177));
#155205=CARTESIAN_POINT('Ctrl Pts',(2.75624276724855,-14.7445964952585,
390.338235294118));
#155206=CARTESIAN_POINT('Ctrl Pts',(1.38995469363045,-15.,388.844117647059));
#155207=CARTESIAN_POINT('Ctrl Pts',(0.,-15.,387.35));
#155208=CARTESIAN_POINT('Ctrl Pts',(-1.38995469363045,-15.,385.855882352941));
#155209=CARTESIAN_POINT('Ctrl Pts',(-2.75624276724856,-14.7445964952585,
384.361764705882));
#155210=CARTESIAN_POINT('Ctrl Pts',(-4.12253084086666,-14.4891929905171,
382.867647058824));
#155211=CARTESIAN_POINT('Ctrl Pts',(-5.41862499280729,-13.9870834410653,
381.373529411765));
#155212=CARTESIAN_POINT('Ctrl Pts',(-6.71471914474793,-13.4849738916136,
379.879411764706));
#155213=CARTESIAN_POINT('Ctrl Pts',(-7.89648244316034,-12.7532570359442,
378.385294117647));
#155214=CARTESIAN_POINT('Ctrl Pts',(-9.07824574157275,-12.0215401802748,
376.891176470588));
#155215=CARTESIAN_POINT('Ctrl Pts',(-10.1054346546984,-11.0851337583099,
375.397058823529));
#155216=CARTESIAN_POINT('Ctrl Pts',(-11.132623567824,-10.148727336345,373.902941176471));
#155217=CARTESIAN_POINT('Ctrl Pts',(-11.9702584092036,-9.03951954568885,
372.408823529412));
#155218=CARTESIAN_POINT('Ctrl Pts',(-12.8078932505832,-7.93031175503273,
370.914705882353));
#155219=CARTESIAN_POINT('Ctrl Pts',(-13.4274493703259,-6.68607533664808,
369.420588235294));
#155220=CARTESIAN_POINT('Ctrl Pts',(-14.0470054900687,-5.44183891826343,
367.926470588235));
#155221=CARTESIAN_POINT('Ctrl Pts',(-14.4273846475923,-4.10494485108124,
366.432352941177));
#155222=CARTESIAN_POINT('Ctrl Pts',(-14.8077638051159,-2.76805078389906,
364.938235294118));
#155223=CARTESIAN_POINT('Ctrl Pts',(-14.9360126444255,-1.38402539194953,
363.444117647059));
#155224=CARTESIAN_POINT('Ctrl Pts',(-15.0642614837351,-9.22419980378748E-16,
361.95));
#155225=CARTESIAN_POINT('Ctrl Pts',(-14.9360126444255,1.38402539194953,
360.455882352941));
#155226=CARTESIAN_POINT('Ctrl Pts',(-14.8077638051159,2.76805078389906,
358.961764705882));
#155227=CARTESIAN_POINT('Ctrl Pts',(-14.4273846475923,4.10494485108124,
357.467647058824));
#155228=CARTESIAN_POINT('Ctrl Pts',(-14.0470054900687,5.44183891826343,
355.973529411765));
#155229=CARTESIAN_POINT('Ctrl Pts',(-13.4274493703259,6.68607533664807,
354.479411764706));
#155230=CARTESIAN_POINT('Ctrl Pts',(-12.8078932505832,7.93031175503273,
352.985294117647));
#155231=CARTESIAN_POINT('Ctrl Pts',(-11.9702584092036,9.03951954568884,
351.491176470588));
#155232=CARTESIAN_POINT('Ctrl Pts',(-11.132623567824,10.148727336345,349.99705882353));
#155233=CARTESIAN_POINT('Ctrl Pts',(-10.1054346546984,11.0851337583099,
348.502941176471));
#155234=CARTESIAN_POINT('Ctrl Pts',(-9.07824574157275,12.0215401802748,
347.008823529412));
#155235=CARTESIAN_POINT('Ctrl Pts',(-7.89648244316034,12.7532570359442,
345.514705882353));
#155236=CARTESIAN_POINT('Ctrl Pts',(-6.71471914474793,13.4849738916136,
344.020588235294));
#155237=CARTESIAN_POINT('Ctrl Pts',(-5.41862499280729,13.9870834410653,
342.526470588235));
#155238=CARTESIAN_POINT('Ctrl Pts',(-4.12253084086667,14.4891929905171,
341.032352941177));
#155239=CARTESIAN_POINT('Ctrl Pts',(-2.75624276724856,14.7445964952585,
339.538235294118));
#155240=CARTESIAN_POINT('Ctrl Pts',(-1.38995469363044,15.,338.044117647059));
#155241=CARTESIAN_POINT('Ctrl Pts',(-1.83697019872103E-15,15.,336.55));
#155242=CARTESIAN_POINT('Ctrl Pts',(1.38995469363045,15.,335.055882352941));
#155243=CARTESIAN_POINT('Ctrl Pts',(2.75624276724855,14.7445964952585,333.561764705882));
#155244=CARTESIAN_POINT('Ctrl Pts',(4.12253084086666,14.4891929905171,332.067647058824));
#155245=CARTESIAN_POINT('Ctrl Pts',(5.4186249928073,13.9870834410653,330.573529411765));
#155246=CARTESIAN_POINT('Ctrl Pts',(6.71471914474792,13.4849738916136,329.079411764706));
#155247=CARTESIAN_POINT('Ctrl Pts',(7.89648244316034,12.7532570359442,327.585294117647));
#155248=CARTESIAN_POINT('Ctrl Pts',(9.07824574157275,12.0215401802748,326.091176470588));
#155249=CARTESIAN_POINT('Ctrl Pts',(10.1054346546984,11.0851337583099,324.597058823529));
#155250=CARTESIAN_POINT('Ctrl Pts',(11.132623567824,10.148727336345,323.102941176471));
#155251=CARTESIAN_POINT('Ctrl Pts',(11.9702584092036,9.03951954568885,321.608823529412));
#155252=CARTESIAN_POINT('Ctrl Pts',(12.8078932505832,7.93031175503273,320.114705882353));
#155253=CARTESIAN_POINT('Ctrl Pts',(13.4274493703259,6.68607533664807,318.620588235294));
#155254=CARTESIAN_POINT('Ctrl Pts',(14.0470054900687,5.44183891826343,317.126470588235));
#155255=CARTESIAN_POINT('Ctrl Pts',(14.4273846475923,4.10494485108125,315.632352941176));
#155256=CARTESIAN_POINT('Ctrl Pts',(14.8077638051159,2.76805078389905,314.138235294118));
#155257=CARTESIAN_POINT('Ctrl Pts',(14.9360126444255,1.38402539194953,312.644117647059));
#155258=CARTESIAN_POINT('Ctrl Pts',(15.0642614837351,2.76725994113625E-15,
311.15));
#155259=CARTESIAN_POINT('Ctrl Pts',(14.9360126444255,-1.38402539194952,
309.655882352941));
#155260=CARTESIAN_POINT('Ctrl Pts',(14.8077638051159,-2.76805078389906,
308.161764705882));
#155261=CARTESIAN_POINT('Ctrl Pts',(14.4273846475923,-4.10494485108124,
306.667647058824));
#155262=CARTESIAN_POINT('Ctrl Pts',(14.0470054900687,-5.44183891826342,
305.173529411765));
#155263=CARTESIAN_POINT('Ctrl Pts',(13.4274493703259,-6.68607533664808,
303.679411764706));
#155264=CARTESIAN_POINT('Ctrl Pts',(12.8078932505832,-7.93031175503273,
302.185294117647));
#155265=CARTESIAN_POINT('Ctrl Pts',(11.9702584092036,-9.03951954568884,
300.691176470588));
#155266=CARTESIAN_POINT('Ctrl Pts',(11.132623567824,-10.148727336345,299.19705882353));
#155267=CARTESIAN_POINT('Ctrl Pts',(10.1054346546984,-11.0851337583099,
297.702941176471));
#155268=CARTESIAN_POINT('Ctrl Pts',(9.07824574157275,-12.0215401802748,
296.208823529412));
#155269=CARTESIAN_POINT('Ctrl Pts',(7.89648244316034,-12.7532570359442,
294.714705882353));
#155270=CARTESIAN_POINT('Ctrl Pts',(6.71471914474792,-13.4849738916136,
293.220588235294));
#155271=CARTESIAN_POINT('Ctrl Pts',(5.4186249928073,-13.9870834410653,291.726470588235));
#155272=CARTESIAN_POINT('Ctrl Pts',(4.12253084086667,-14.4891929905171,
290.232352941176));
#155273=CARTESIAN_POINT('Ctrl Pts',(2.75624276724855,-14.7445964952585,
288.738235294118));
#155274=CARTESIAN_POINT('Ctrl Pts',(1.38995469363045,-15.,287.244117647059));
#155275=CARTESIAN_POINT('Ctrl Pts',(0.,-15.,285.75));
#155276=CARTESIAN_POINT('Ctrl Pts',(-1.38995469363045,-15.,284.255882352941));
#155277=CARTESIAN_POINT('Ctrl Pts',(-2.75624276724856,-14.7445964952585,
282.761764705882));
#155278=CARTESIAN_POINT('Ctrl Pts',(-4.12253084086666,-14.4891929905171,
281.267647058824));
#155279=CARTESIAN_POINT('Ctrl Pts',(-5.41862499280729,-13.9870834410653,
279.773529411765));
#155280=CARTESIAN_POINT('Ctrl Pts',(-6.71471914474793,-13.4849738916136,
278.279411764706));
#155281=CARTESIAN_POINT('Ctrl Pts',(-7.89648244316034,-12.7532570359442,
276.785294117647));
#155282=CARTESIAN_POINT('Ctrl Pts',(-9.07824574157275,-12.0215401802748,
275.291176470588));
#155283=CARTESIAN_POINT('Ctrl Pts',(-10.1054346546984,-11.0851337583099,
273.797058823529));
#155284=CARTESIAN_POINT('Ctrl Pts',(-11.132623567824,-10.148727336345,272.302941176471));
#155285=CARTESIAN_POINT('Ctrl Pts',(-11.9702584092036,-9.03951954568885,
270.808823529412));
#155286=CARTESIAN_POINT('Ctrl Pts',(-12.8078932505832,-7.93031175503273,
269.314705882353));
#155287=CARTESIAN_POINT('Ctrl Pts',(-13.4274493703259,-6.68607533664808,
267.820588235294));
#155288=CARTESIAN_POINT('Ctrl Pts',(-14.0470054900687,-5.44183891826343,
266.326470588235));
#155289=CARTESIAN_POINT('Ctrl Pts',(-14.4273846475923,-4.10494485108124,
264.832352941177));
#155290=CARTESIAN_POINT('Ctrl Pts',(-14.8077638051159,-2.76805078389906,
263.338235294118));
#155291=CARTESIAN_POINT('Ctrl Pts',(-14.9360126444255,-1.38402539194953,
261.844117647059));
#155292=CARTESIAN_POINT('Ctrl Pts',(-15.0642614837351,-9.22419980378748E-16,
260.35));
#155293=CARTESIAN_POINT('Ctrl Pts',(-14.9360126444255,1.38402539194953,
258.855882352941));
#155294=CARTESIAN_POINT('Ctrl Pts',(-14.8077638051159,2.76805078389906,
257.361764705882));
#155295=CARTESIAN_POINT('Ctrl Pts',(-14.4273846475923,4.10494485108124,
255.867647058823));
#155296=CARTESIAN_POINT('Ctrl Pts',(-14.0470054900687,5.44183891826343,
254.373529411765));
#155297=CARTESIAN_POINT('Ctrl Pts',(-13.4274493703259,6.68607533664807,
252.879411764706));
#155298=CARTESIAN_POINT('Ctrl Pts',(-12.8078932505832,7.93031175503273,
251.385294117647));
#155299=CARTESIAN_POINT('Ctrl Pts',(-11.9702584092036,9.03951954568884,
249.891176470588));
#155300=CARTESIAN_POINT('Ctrl Pts',(-11.132623567824,10.148727336345,248.397058823529));
#155301=CARTESIAN_POINT('Ctrl Pts',(-10.1054346546984,11.0851337583099,
246.902941176471));
#155302=CARTESIAN_POINT('Ctrl Pts',(-9.07824574157275,12.0215401802748,
245.408823529412));
#155303=CARTESIAN_POINT('Ctrl Pts',(-7.89648244316034,12.7532570359442,
243.914705882353));
#155304=CARTESIAN_POINT('Ctrl Pts',(-6.71471914474793,13.4849738916136,
242.420588235294));
#155305=CARTESIAN_POINT('Ctrl Pts',(-5.41862499280729,13.9870834410653,
240.926470588235));
#155306=CARTESIAN_POINT('Ctrl Pts',(-4.12253084086667,14.4891929905171,
239.432352941177));
#155307=CARTESIAN_POINT('Ctrl Pts',(-2.75624276724856,14.7445964952585,
237.938235294118));
#155308=CARTESIAN_POINT('Ctrl Pts',(-1.38995469363044,15.,236.444117647059));
#155309=CARTESIAN_POINT('Ctrl Pts',(-1.83697019872103E-15,15.,234.95));
#155310=CARTESIAN_POINT('Ctrl Pts',(1.38995469363045,15.,233.455882352941));
#155311=CARTESIAN_POINT('Ctrl Pts',(2.75624276724855,14.7445964952585,231.961764705883));
#155312=CARTESIAN_POINT('Ctrl Pts',(4.12253084086666,14.4891929905171,230.467647058824));
#155313=CARTESIAN_POINT('Ctrl Pts',(5.4186249928073,13.9870834410653,228.973529411765));
#155314=CARTESIAN_POINT('Ctrl Pts',(6.71471914474792,13.4849738916136,227.479411764706));
#155315=CARTESIAN_POINT('Ctrl Pts',(7.89648244316034,12.7532570359442,225.985294117647));
#155316=CARTESIAN_POINT('Ctrl Pts',(9.07824574157275,12.0215401802748,224.491176470588));
#155317=CARTESIAN_POINT('Ctrl Pts',(10.1054346546984,11.0851337583099,222.99705882353));
#155318=CARTESIAN_POINT('Ctrl Pts',(11.132623567824,10.148727336345,221.502941176471));
#155319=CARTESIAN_POINT('Ctrl Pts',(11.9702584092036,9.03951954568885,220.008823529412));
#155320=CARTESIAN_POINT('Ctrl Pts',(12.8078932505832,7.93031175503273,218.514705882353));
#155321=CARTESIAN_POINT('Ctrl Pts',(13.4274493703259,6.68607533664807,217.020588235294));
#155322=CARTESIAN_POINT('Ctrl Pts',(14.0470054900687,5.44183891826343,215.526470588235));
#155323=CARTESIAN_POINT('Ctrl Pts',(14.4273846475923,4.10494485108125,214.032352941176));
#155324=CARTESIAN_POINT('Ctrl Pts',(14.8077638051159,2.76805078389905,212.538235294118));
#155325=CARTESIAN_POINT('Ctrl Pts',(14.9360126444255,1.38402539194953,211.044117647059));
#155326=CARTESIAN_POINT('Ctrl Pts',(15.0642614837351,2.76725994113625E-15,
209.55));
#155327=CARTESIAN_POINT('Ctrl Pts',(14.9360126444255,-1.38402539194952,
208.055882352941));
#155328=CARTESIAN_POINT('Ctrl Pts',(14.8077638051159,-2.76805078389906,
206.561764705882));
#155329=CARTESIAN_POINT('Ctrl Pts',(14.4273846475923,-4.10494485108124,
205.067647058824));
#155330=CARTESIAN_POINT('Ctrl Pts',(14.0470054900687,-5.44183891826342,
203.573529411765));
#155331=CARTESIAN_POINT('Ctrl Pts',(13.4274493703259,-6.68607533664808,
202.079411764706));
#155332=CARTESIAN_POINT('Ctrl Pts',(12.8078932505832,-7.93031175503273,
200.585294117647));
#155333=CARTESIAN_POINT('Ctrl Pts',(11.9702584092036,-9.03951954568884,
199.091176470588));
#155334=CARTESIAN_POINT('Ctrl Pts',(11.132623567824,-10.148727336345,197.597058823529));
#155335=CARTESIAN_POINT('Ctrl Pts',(10.1054346546984,-11.0851337583099,
196.102941176471));
#155336=CARTESIAN_POINT('Ctrl Pts',(9.07824574157275,-12.0215401802748,
194.608823529412));
#155337=CARTESIAN_POINT('Ctrl Pts',(7.89648244316034,-12.7532570359442,
193.114705882353));
#155338=CARTESIAN_POINT('Ctrl Pts',(6.71471914474792,-13.4849738916136,
191.620588235294));
#155339=CARTESIAN_POINT('Ctrl Pts',(5.4186249928073,-13.9870834410653,190.126470588235));
#155340=CARTESIAN_POINT('Ctrl Pts',(4.12253084086667,-14.4891929905171,
188.632352941176));
#155341=CARTESIAN_POINT('Ctrl Pts',(2.75624276724855,-14.7445964952585,
187.138235294118));
#155342=CARTESIAN_POINT('Ctrl Pts',(1.38995469363045,-15.,185.644117647059));
#155343=CARTESIAN_POINT('Ctrl Pts',(0.,-15.,184.15));
#155344=CARTESIAN_POINT('Ctrl Pts',(-1.38995469363045,-15.,182.655882352941));
#155345=CARTESIAN_POINT('Ctrl Pts',(-2.75624276724856,-14.7445964952585,
181.161764705882));
#155346=CARTESIAN_POINT('Ctrl Pts',(-4.12253084086666,-14.4891929905171,
179.667647058824));
#155347=CARTESIAN_POINT('Ctrl Pts',(-5.41862499280729,-13.9870834410653,
178.173529411765));
#155348=CARTESIAN_POINT('Ctrl Pts',(-6.71471914474793,-13.4849738916136,
176.679411764706));
#155349=CARTESIAN_POINT('Ctrl Pts',(-7.89648244316034,-12.7532570359442,
175.185294117647));
#155350=CARTESIAN_POINT('Ctrl Pts',(-9.07824574157275,-12.0215401802748,
173.691176470588));
#155351=CARTESIAN_POINT('Ctrl Pts',(-10.1054346546984,-11.0851337583099,
172.19705882353));
#155352=CARTESIAN_POINT('Ctrl Pts',(-11.132623567824,-10.148727336345,170.702941176471));
#155353=CARTESIAN_POINT('Ctrl Pts',(-11.9702584092036,-9.03951954568885,
169.208823529412));
#155354=CARTESIAN_POINT('Ctrl Pts',(-12.8078932505832,-7.93031175503273,
167.714705882353));
#155355=CARTESIAN_POINT('Ctrl Pts',(-13.4274493703259,-6.68607533664808,
166.220588235294));
#155356=CARTESIAN_POINT('Ctrl Pts',(-14.0470054900687,-5.44183891826343,
164.726470588235));
#155357=CARTESIAN_POINT('Ctrl Pts',(-14.4273846475923,-4.10494485108124,
163.232352941177));
#155358=CARTESIAN_POINT('Ctrl Pts',(-14.8077638051159,-2.76805078389906,
161.738235294118));
#155359=CARTESIAN_POINT('Ctrl Pts',(-14.9360126444255,-1.38402539194953,
160.244117647059));
#155360=CARTESIAN_POINT('Ctrl Pts',(-15.0642614837351,-9.22419980378748E-16,
158.75));
#155361=CARTESIAN_POINT('Ctrl Pts',(-14.9360126444255,1.38402539194953,
157.255882352941));
#155362=CARTESIAN_POINT('Ctrl Pts',(-14.8077638051159,2.76805078389906,
155.761764705882));
#155363=CARTESIAN_POINT('Ctrl Pts',(-14.4273846475923,4.10494485108124,
154.267647058824));
#155364=CARTESIAN_POINT('Ctrl Pts',(-14.0470054900687,5.44183891826343,
152.773529411765));
#155365=CARTESIAN_POINT('Ctrl Pts',(-13.4274493703259,6.68607533664807,
151.279411764706));
#155366=CARTESIAN_POINT('Ctrl Pts',(-12.8078932505832,7.93031175503273,
149.785294117647));
#155367=CARTESIAN_POINT('Ctrl Pts',(-11.9702584092036,9.03951954568884,
148.291176470588));
#155368=CARTESIAN_POINT('Ctrl Pts',(-11.132623567824,10.148727336345,146.79705882353));
#155369=CARTESIAN_POINT('Ctrl Pts',(-10.1054346546984,11.0851337583099,
145.302941176471));
#155370=CARTESIAN_POINT('Ctrl Pts',(-9.07824574157275,12.0215401802748,
143.808823529412));
#155371=CARTESIAN_POINT('Ctrl Pts',(-7.89648244316034,12.7532570359442,
142.314705882353));
#155372=CARTESIAN_POINT('Ctrl Pts',(-6.71471914474793,13.4849738916136,
140.820588235294));
#155373=CARTESIAN_POINT('Ctrl Pts',(-5.41862499280729,13.9870834410653,
139.326470588235));
#155374=CARTESIAN_POINT('Ctrl Pts',(-4.12253084086667,14.4891929905171,
137.832352941177));
#155375=CARTESIAN_POINT('Ctrl Pts',(-2.75624276724856,14.7445964952585,
136.338235294118));
#155376=CARTESIAN_POINT('Ctrl Pts',(-1.38995469363044,15.,134.844117647059));
#155377=CARTESIAN_POINT('Ctrl Pts',(-1.83697019872103E-15,15.,133.35));
#155378=CARTESIAN_POINT('Ctrl Pts',(1.38995469363045,15.,131.855882352941));
#155379=CARTESIAN_POINT('Ctrl Pts',(2.75624276724855,14.7445964952585,130.361764705882));
#155380=CARTESIAN_POINT('Ctrl Pts',(4.12253084086666,14.4891929905171,128.867647058824));
#155381=CARTESIAN_POINT('Ctrl Pts',(5.4186249928073,13.9870834410653,127.373529411765));
#155382=CARTESIAN_POINT('Ctrl Pts',(6.71471914474792,13.4849738916136,125.879411764706));
#155383=CARTESIAN_POINT('Ctrl Pts',(7.89648244316034,12.7532570359442,124.385294117647));
#155384=CARTESIAN_POINT('Ctrl Pts',(9.07824574157275,12.0215401802748,122.891176470588));
#155385=CARTESIAN_POINT('Ctrl Pts',(10.1054346546984,11.0851337583099,121.397058823529));
#155386=CARTESIAN_POINT('Ctrl Pts',(11.132623567824,10.148727336345,119.902941176471));
#155387=CARTESIAN_POINT('Ctrl Pts',(11.9702584092036,9.03951954568885,118.408823529412));
#155388=CARTESIAN_POINT('Ctrl Pts',(12.8078932505832,7.93031175503273,116.914705882353));
#155389=CARTESIAN_POINT('Ctrl Pts',(13.4274493703259,6.68607533664807,115.420588235294));
#155390=CARTESIAN_POINT('Ctrl Pts',(14.0470054900687,5.44183891826343,113.926470588235));
#155391=CARTESIAN_POINT('Ctrl Pts',(14.4273846475923,4.10494485108125,112.432352941177));
#155392=CARTESIAN_POINT('Ctrl Pts',(14.8077638051159,2.76805078389905,110.938235294118));
#155393=CARTESIAN_POINT('Ctrl Pts',(14.9360126444255,1.38402539194953,109.444117647059));
#155394=CARTESIAN_POINT('Ctrl Pts',(15.0642614837351,2.76725994113625E-15,
107.95));
#155395=CARTESIAN_POINT('Ctrl Pts',(14.9360126444255,-1.38402539194952,
106.455882352941));
#155396=CARTESIAN_POINT('Ctrl Pts',(14.8077638051159,-2.76805078389906,
104.961764705882));
#155397=CARTESIAN_POINT('Ctrl Pts',(14.4273846475923,-4.10494485108124,
103.467647058824));
#155398=CARTESIAN_POINT('Ctrl Pts',(14.0470054900687,-5.44183891826342,
101.973529411765));
#155399=CARTESIAN_POINT('Ctrl Pts',(13.4274493703259,-6.68607533664808,
100.479411764706));
#155400=CARTESIAN_POINT('Ctrl Pts',(12.8078932505832,-7.93031175503273,
98.985294117647));
#155401=CARTESIAN_POINT('Ctrl Pts',(11.9702584092036,-9.03951954568884,
97.4911764705884));
#155402=CARTESIAN_POINT('Ctrl Pts',(11.132623567824,-10.148727336345,95.9970588235295));
#155403=CARTESIAN_POINT('Ctrl Pts',(10.1054346546984,-11.0851337583099,
94.5029411764706));
#155404=CARTESIAN_POINT('Ctrl Pts',(9.07824574157275,-12.0215401802748,
93.0088235294117));
#155405=CARTESIAN_POINT('Ctrl Pts',(7.89648244316034,-12.7532570359442,
91.5147058823529));
#155406=CARTESIAN_POINT('Ctrl Pts',(6.71471914474792,-13.4849738916136,
90.0205882352942));
#155407=CARTESIAN_POINT('Ctrl Pts',(5.4186249928073,-13.9870834410653,88.5264705882354));
#155408=CARTESIAN_POINT('Ctrl Pts',(4.12253084086667,-14.4891929905171,
87.0323529411765));
#155409=CARTESIAN_POINT('Ctrl Pts',(2.75624276724855,-14.7445964952585,
85.5382352941176));
#155410=CARTESIAN_POINT('Ctrl Pts',(1.38995469363045,-15.,84.0441176470588));
#155411=CARTESIAN_POINT('Ctrl Pts',(0.,-15.,82.5500000000001));
#155412=CARTESIAN_POINT('Ctrl Pts',(-1.38995469363045,-15.,81.0558823529413));
#155413=CARTESIAN_POINT('Ctrl Pts',(-2.75624276724856,-14.7445964952585,
79.5617647058824));
#155414=CARTESIAN_POINT('Ctrl Pts',(-4.12253084086666,-14.4891929905171,
78.0676470588235));
#155415=CARTESIAN_POINT('Ctrl Pts',(-5.41862499280729,-13.9870834410653,
76.5735294117647));
#155416=CARTESIAN_POINT('Ctrl Pts',(-6.71471914474793,-13.4849738916136,
75.079411764706));
#155417=CARTESIAN_POINT('Ctrl Pts',(-7.89648244316034,-12.7532570359442,
73.5852941176471));
#155418=CARTESIAN_POINT('Ctrl Pts',(-9.07824574157275,-12.0215401802748,
72.0911764705883));
#155419=CARTESIAN_POINT('Ctrl Pts',(-10.1054346546984,-11.0851337583099,
70.5970588235294));
#155420=CARTESIAN_POINT('Ctrl Pts',(-11.132623567824,-10.148727336345,69.1029411764705));
#155421=CARTESIAN_POINT('Ctrl Pts',(-11.9702584092036,-9.03951954568885,
67.6088235294119));
#155422=CARTESIAN_POINT('Ctrl Pts',(-12.8078932505832,-7.93031175503273,
66.114705882353));
#155423=CARTESIAN_POINT('Ctrl Pts',(-13.4274493703259,-6.68607533664808,
64.6205882352942));
#155424=CARTESIAN_POINT('Ctrl Pts',(-14.0470054900687,-5.44183891826343,
63.1264705882353));
#155425=CARTESIAN_POINT('Ctrl Pts',(-14.4273846475923,-4.10494485108124,
61.6323529411764));
#155426=CARTESIAN_POINT('Ctrl Pts',(-14.8077638051159,-2.76805078389906,
60.1382352941178));
#155427=CARTESIAN_POINT('Ctrl Pts',(-14.9360126444255,-1.38402539194953,
58.6441176470589));
#155428=CARTESIAN_POINT('Ctrl Pts',(-15.0642614837351,-9.22419980378748E-16,
57.15));
#155429=CARTESIAN_POINT('Ctrl Pts',(-14.9360126444255,1.38402539194953,
55.6558823529412));
#155430=CARTESIAN_POINT('Ctrl Pts',(-14.8077638051159,2.76805078389906,
54.1617647058823));
#155431=CARTESIAN_POINT('Ctrl Pts',(-14.4273846475923,4.10494485108124,
52.6676470588237));
#155432=CARTESIAN_POINT('Ctrl Pts',(-14.0470054900687,5.44183891826343,
51.1735294117648));
#155433=CARTESIAN_POINT('Ctrl Pts',(-13.4274493703259,6.68607533664807,
49.6794117647059));
#155434=CARTESIAN_POINT('Ctrl Pts',(-12.8078932505832,7.93031175503273,
48.185294117647));
#155435=CARTESIAN_POINT('Ctrl Pts',(-11.9702584092036,9.03951954568884,
46.6911764705882));
#155436=CARTESIAN_POINT('Ctrl Pts',(-11.132623567824,10.148727336345,45.1970588235295));
#155437=CARTESIAN_POINT('Ctrl Pts',(-10.1054346546984,11.0851337583099,
43.7029411764707));
#155438=CARTESIAN_POINT('Ctrl Pts',(-9.07824574157275,12.0215401802748,
42.2088235294118));
#155439=CARTESIAN_POINT('Ctrl Pts',(-7.89648244316034,12.7532570359442,
40.7147058823529));
#155440=CARTESIAN_POINT('Ctrl Pts',(-6.71471914474793,13.4849738916136,
39.2205882352941));
#155441=CARTESIAN_POINT('Ctrl Pts',(-5.41862499280729,13.9870834410653,
37.7264705882354));
#155442=CARTESIAN_POINT('Ctrl Pts',(-4.12253084086667,14.4891929905171,
36.2323529411766));
#155443=CARTESIAN_POINT('Ctrl Pts',(-2.75624276724856,14.7445964952585,
34.7382352941177));
#155444=CARTESIAN_POINT('Ctrl Pts',(-1.38995469363044,15.,33.2441176470588));
#155445=CARTESIAN_POINT('Ctrl Pts',(-1.83697019872103E-15,15.,31.7499999999999));
#155446=CARTESIAN_POINT('Ctrl Pts',(1.38995469363045,15.,30.2558823529413));
#155447=CARTESIAN_POINT('Ctrl Pts',(2.75624276724855,14.7445964952585,28.7617647058824));
#155448=CARTESIAN_POINT('Ctrl Pts',(4.12253084086666,14.4891929905171,27.2676470588236));
#155449=CARTESIAN_POINT('Ctrl Pts',(5.4186249928073,13.9870834410653,25.7735294117647));
#155450=CARTESIAN_POINT('Ctrl Pts',(6.71471914474792,13.4849738916136,24.2794117647058));
#155451=CARTESIAN_POINT('Ctrl Pts',(7.89648244316034,12.7532570359442,22.7852941176472));
#155452=CARTESIAN_POINT('Ctrl Pts',(9.07824574157275,12.0215401802748,21.2911764705883));
#155453=CARTESIAN_POINT('Ctrl Pts',(10.1054346546984,11.0851337583099,19.7970588235294));
#155454=CARTESIAN_POINT('Ctrl Pts',(11.132623567824,10.148727336345,18.3029411764706));
#155455=CARTESIAN_POINT('Ctrl Pts',(11.9702584092036,9.03951954568885,16.8088235294117));
#155456=CARTESIAN_POINT('Ctrl Pts',(12.8078932505832,7.93031175503273,15.3147058823531));
#155457=CARTESIAN_POINT('Ctrl Pts',(13.4274493703259,6.68607533664807,13.8205882352942));
#155458=CARTESIAN_POINT('Ctrl Pts',(14.0470054900687,5.44183891826343,12.3264705882353));
#155459=CARTESIAN_POINT('Ctrl Pts',(14.4273846475923,4.10494485108125,10.8323529411765));
#155460=CARTESIAN_POINT('Ctrl Pts',(14.8077638051159,2.76805078389905,9.33823529411759));
#155461=CARTESIAN_POINT('Ctrl Pts',(14.9360126444255,1.38402539194953,7.84411764705895));
#155462=CARTESIAN_POINT('Ctrl Pts',(15.0642614837351,2.76725994113625E-15,
6.35000000000008));
#155463=CARTESIAN_POINT('Ctrl Pts',(14.9360126444255,-1.38402539194952,
4.85588235294121));
#155464=CARTESIAN_POINT('Ctrl Pts',(14.8077638051159,-2.76805078389906,
3.36176470588234));
#155465=CARTESIAN_POINT('Ctrl Pts',(14.4273846475923,-4.10494485108124,
1.86764705882347));
#155466=CARTESIAN_POINT('Ctrl Pts',(14.0470054900687,-5.44183891826342,
0.373529411764828));
#155467=CARTESIAN_POINT('Ctrl Pts',(13.4274493703259,-6.68607533664808,
-1.12058823529404));
#155468=CARTESIAN_POINT('Ctrl Pts',(12.8078932505832,-7.93031175503273,
-2.61470588235291));
#155469=CARTESIAN_POINT('Ctrl Pts',(11.9702584092036,-9.03951954568884,
-4.10882352941178));
#155470=CARTESIAN_POINT('Ctrl Pts',(11.132623567824,-10.148727336345,-5.60294117647064));
#155471=CARTESIAN_POINT('Ctrl Pts',(10.1054346546984,-11.0851337583099,
-7.09705882352929));
#155472=CARTESIAN_POINT('Ctrl Pts',(9.07824574157275,-12.0215401802748,
-8.59117647058816));
#155473=CARTESIAN_POINT('Ctrl Pts',(7.89648244316034,-12.7532570359442,
-10.085294117647));
#155474=CARTESIAN_POINT('Ctrl Pts',(6.71471914474792,-13.4849738916136,
-11.5794117647059));
#155475=CARTESIAN_POINT('Ctrl Pts',(5.4186249928073,-13.9870834410653,-13.0735294117648));
#155476=CARTESIAN_POINT('Ctrl Pts',(4.12253084086667,-14.4891929905171,
-14.5676470588234));
#155477=CARTESIAN_POINT('Ctrl Pts',(2.75624276724855,-14.7445964952585,
-16.0617647058823));
#155478=CARTESIAN_POINT('Ctrl Pts',(1.38995469363045,-15.,-17.5558823529411));
#155479=CARTESIAN_POINT('Ctrl Pts',(0.,-15.,-19.05));
#155480=CARTESIAN_POINT('Ctrl Pts',(-1.38995469363045,-15.,-20.5441176470589));
#155481=CARTESIAN_POINT('Ctrl Pts',(-2.75624276724856,-14.7445964952585,
-22.0382352941175));
#155482=CARTESIAN_POINT('Ctrl Pts',(-4.12253084086666,-14.4891929905171,
-23.5323529411764));
#155483=CARTESIAN_POINT('Ctrl Pts',(-5.41862499280729,-13.9870834410653,
-25.0264705882353));
#155484=CARTESIAN_POINT('Ctrl Pts',(-6.71471914474793,-13.4849738916136,
-26.5205882352941));
#155485=CARTESIAN_POINT('Ctrl Pts',(-7.89648244316034,-12.7532570359442,
-28.014705882353));
#155486=CARTESIAN_POINT('Ctrl Pts',(-9.07824574157275,-12.0215401802748,
-29.5088235294116));
#155487=CARTESIAN_POINT('Ctrl Pts',(-10.1054346546984,-11.0851337583099,
-31.0029411764705));
#155488=CARTESIAN_POINT('Ctrl Pts',(-11.132623567824,-10.148727336345,-32.4970588235294));
#155489=CARTESIAN_POINT('Ctrl Pts',(-11.9702584092036,-9.03951954568885,
-33.9911764705882));
#155490=CARTESIAN_POINT('Ctrl Pts',(-12.8078932505832,-7.93031175503273,
-35.4852941176471));
#155491=CARTESIAN_POINT('Ctrl Pts',(-13.4274493703259,-6.68607533664808,
-36.9794117647058));
#155492=CARTESIAN_POINT('Ctrl Pts',(-14.0470054900687,-5.44183891826343,
-38.4735294117646));
#155493=CARTESIAN_POINT('Ctrl Pts',(-14.4273846475923,-4.10494485108124,
-39.9676470588235));
#155494=CARTESIAN_POINT('Ctrl Pts',(-14.8077638051159,-2.76805078389906,
-41.4617647058824));
#155495=CARTESIAN_POINT('Ctrl Pts',(-14.9360126444255,-1.38402539194953,
-42.9558823529412));
#155496=CARTESIAN_POINT('Ctrl Pts',(-15.0642614837351,-9.22419980378748E-16,
-44.4499999999999));
#155497=CARTESIAN_POINT('Ctrl Pts',(-14.9360126444255,1.38402539194953,
-45.9441176470587));
#155498=CARTESIAN_POINT('Ctrl Pts',(-14.8077638051159,2.76805078389906,
-47.4382352941176));
#155499=CARTESIAN_POINT('Ctrl Pts',(-14.4273846475923,4.10494485108124,
-48.9323529411765));
#155500=CARTESIAN_POINT('Ctrl Pts',(-14.0470054900687,5.44183891826343,
-50.4264705882354));
#155501=CARTESIAN_POINT('Ctrl Pts',(-13.4274493703259,6.68607533664807,
-51.920588235294));
#155502=CARTESIAN_POINT('Ctrl Pts',(-12.8078932505832,7.93031175503273,
-53.4147058823529));
#155503=CARTESIAN_POINT('Ctrl Pts',(-11.9702584092036,9.03951954568884,
-54.9088235294117));
#155504=CARTESIAN_POINT('Ctrl Pts',(-11.132623567824,10.148727336345,-56.4029411764706));
#155505=CARTESIAN_POINT('Ctrl Pts',(-10.1054346546984,11.0851337583099,
-57.8970588235295));
#155506=CARTESIAN_POINT('Ctrl Pts',(-9.07824574157275,12.0215401802748,
-59.3911764705881));
#155507=CARTESIAN_POINT('Ctrl Pts',(-7.89648244316034,12.7532570359442,
-60.885294117647));
#155508=CARTESIAN_POINT('Ctrl Pts',(-6.71471914474793,13.4849738916136,
-62.3794117647059));
#155509=CARTESIAN_POINT('Ctrl Pts',(-5.41862499280729,13.9870834410653,
-63.8735294117647));
#155510=CARTESIAN_POINT('Ctrl Pts',(-4.12253084086667,14.4891929905171,
-65.3676470588236));
#155511=CARTESIAN_POINT('Ctrl Pts',(-2.75624276724856,14.7445964952585,
-66.8617647058822));
#155512=CARTESIAN_POINT('Ctrl Pts',(-1.38995469363044,15.,-68.3558823529411));
#155513=CARTESIAN_POINT('Ctrl Pts',(-1.83697019872103E-15,15.,-69.85));
#155514=CARTESIAN_POINT('Ctrl Pts',(1.38995469363045,15.,-71.3441176470589));
#155515=CARTESIAN_POINT('Ctrl Pts',(2.75624276724855,14.7445964952585,-72.8382352941177));
#155516=CARTESIAN_POINT('Ctrl Pts',(4.12253084086666,14.4891929905171,-74.3323529411764));
#155517=CARTESIAN_POINT('Ctrl Pts',(5.4186249928073,13.9870834410653,-75.8264705882352));
#155518=CARTESIAN_POINT('Ctrl Pts',(6.71471914474792,13.4849738916136,-77.3205882352941));
#155519=CARTESIAN_POINT('Ctrl Pts',(7.89648244316034,12.7532570359442,-78.814705882353));
#155520=CARTESIAN_POINT('Ctrl Pts',(9.07824574157275,12.0215401802748,-80.3088235294118));
#155521=CARTESIAN_POINT('Ctrl Pts',(10.1054346546984,11.0851337583099,-81.8029411764705));
#155522=CARTESIAN_POINT('Ctrl Pts',(11.132623567824,10.148727336345,-83.2970588235294));
#155523=CARTESIAN_POINT('Ctrl Pts',(11.9702584092036,9.03951954568885,-84.7911764705882));
#155524=CARTESIAN_POINT('Ctrl Pts',(12.8078932505832,7.93031175503273,-86.2852941176471));
#155525=CARTESIAN_POINT('Ctrl Pts',(13.4274493703259,6.68607533664807,-87.7794117647059));
#155526=CARTESIAN_POINT('Ctrl Pts',(14.0470054900687,5.44183891826343,-89.2735294117646));
#155527=CARTESIAN_POINT('Ctrl Pts',(14.4273846475923,4.10494485108125,-90.7676470588235));
#155528=CARTESIAN_POINT('Ctrl Pts',(14.8077638051159,2.76805078389905,-92.2617647058823));
#155529=CARTESIAN_POINT('Ctrl Pts',(14.9360126444255,1.38402539194953,-93.7558823529412));
#155530=CARTESIAN_POINT('Ctrl Pts',(15.0642614837351,2.76725994113625E-15,
-95.2500000000001));
#155531=CARTESIAN_POINT('Ctrl Pts',(14.9360126444255,-1.38402539194952,
-96.7441176470587));
#155532=CARTESIAN_POINT('Ctrl Pts',(14.8077638051159,-2.76805078389906,
-98.2382352941176));
#155533=CARTESIAN_POINT('Ctrl Pts',(14.4273846475923,-4.10494485108124,
-99.7323529411764));
#155534=CARTESIAN_POINT('Ctrl Pts',(14.0470054900687,-5.44183891826342,
-101.226470588235));
#155535=CARTESIAN_POINT('Ctrl Pts',(13.4274493703259,-6.68607533664808,
-102.720588235294));
#155536=CARTESIAN_POINT('Ctrl Pts',(12.8078932505832,-7.93031175503273,
-104.214705882353));
#155537=CARTESIAN_POINT('Ctrl Pts',(11.9702584092036,-9.03951954568884,
-105.708823529412));
#155538=CARTESIAN_POINT('Ctrl Pts',(11.132623567824,-10.148727336345,-107.202941176471));
#155539=CARTESIAN_POINT('Ctrl Pts',(10.1054346546984,-11.0851337583099,
-108.697058823529));
#155540=CARTESIAN_POINT('Ctrl Pts',(9.07824574157275,-12.0215401802748,
-110.191176470588));
#155541=CARTESIAN_POINT('Ctrl Pts',(7.89648244316034,-12.7532570359442,
-111.685294117647));
#155542=CARTESIAN_POINT('Ctrl Pts',(6.71471914474792,-13.4849738916136,
-113.179411764706));
#155543=CARTESIAN_POINT('Ctrl Pts',(5.4186249928073,-13.9870834410653,-114.673529411765));
#155544=CARTESIAN_POINT('Ctrl Pts',(4.12253084086667,-14.4891929905171,
-116.167647058824));
#155545=CARTESIAN_POINT('Ctrl Pts',(2.75624276724855,-14.7445964952585,
-117.661764705882));
#155546=CARTESIAN_POINT('Ctrl Pts',(1.38995469363045,-15.,-119.155882352941));
#155547=CARTESIAN_POINT('Ctrl Pts',(0.,-15.,-120.65));
#155548=CARTESIAN_POINT('Ctrl Pts',(-1.38995469363045,-15.,-122.144117647059));
#155549=CARTESIAN_POINT('Ctrl Pts',(-2.75624276724856,-14.7445964952585,
-123.638235294118));
#155550=CARTESIAN_POINT('Ctrl Pts',(-4.12253084086666,-14.4891929905171,
-125.132352941177));
#155551=CARTESIAN_POINT('Ctrl Pts',(-5.41862499280729,-13.9870834410653,
-126.626470588235));
#155552=CARTESIAN_POINT('Ctrl Pts',(-6.71471914474793,-13.4849738916136,
-128.120588235294));
#155553=CARTESIAN_POINT('Ctrl Pts',(-7.89648244316034,-12.7532570359442,
-129.614705882353));
#155554=CARTESIAN_POINT('Ctrl Pts',(-9.07824574157275,-12.0215401802748,
-131.108823529412));
#155555=CARTESIAN_POINT('Ctrl Pts',(-10.1054346546984,-11.0851337583099,
-132.602941176471));
#155556=CARTESIAN_POINT('Ctrl Pts',(-11.132623567824,-10.148727336345,-134.097058823529));
#155557=CARTESIAN_POINT('Ctrl Pts',(-11.9702584092036,-9.03951954568885,
-135.591176470588));
#155558=CARTESIAN_POINT('Ctrl Pts',(-12.8078932505832,-7.93031175503273,
-137.085294117647));
#155559=CARTESIAN_POINT('Ctrl Pts',(-13.4274493703259,-6.68607533664808,
-138.579411764706));
#155560=CARTESIAN_POINT('Ctrl Pts',(-14.0470054900687,-5.44183891826343,
-140.073529411765));
#155561=CARTESIAN_POINT('Ctrl Pts',(-14.4273846475923,-4.10494485108124,
-141.567647058823));
#155562=CARTESIAN_POINT('Ctrl Pts',(-14.8077638051159,-2.76805078389906,
-143.061764705882));
#155563=CARTESIAN_POINT('Ctrl Pts',(-14.9360126444255,-1.38402539194953,
-144.555882352941));
#155564=CARTESIAN_POINT('Ctrl Pts',(-15.0642614837351,-9.22419980378748E-16,
-146.05));
#155565=CARTESIAN_POINT('Ctrl Pts',(-14.9360126444255,1.38402539194953,
-147.544117647059));
#155566=CARTESIAN_POINT('Ctrl Pts',(-14.8077638051159,2.76805078389906,
-149.038235294118));
#155567=CARTESIAN_POINT('Ctrl Pts',(-14.4273846475923,4.10494485108124,
-150.532352941176));
#155568=CARTESIAN_POINT('Ctrl Pts',(-14.0470054900687,5.44183891826343,
-152.026470588235));
#155569=CARTESIAN_POINT('Ctrl Pts',(-13.4274493703259,6.68607533664807,
-153.520588235294));
#155570=CARTESIAN_POINT('Ctrl Pts',(-12.8078932505832,7.93031175503273,
-155.014705882353));
#155571=CARTESIAN_POINT('Ctrl Pts',(-11.9702584092036,9.03951954568884,
-156.508823529412));
#155572=CARTESIAN_POINT('Ctrl Pts',(-11.132623567824,10.148727336345,-158.002941176471));
#155573=CARTESIAN_POINT('Ctrl Pts',(-10.1054346546984,11.0851337583099,
-159.497058823529));
#155574=CARTESIAN_POINT('Ctrl Pts',(-9.07824574157275,12.0215401802748,
-160.991176470588));
#155575=CARTESIAN_POINT('Ctrl Pts',(-7.89648244316034,12.7532570359442,
-162.485294117647));
#155576=CARTESIAN_POINT('Ctrl Pts',(-6.71471914474793,13.4849738916136,
-163.979411764706));
#155577=CARTESIAN_POINT('Ctrl Pts',(-5.41862499280729,13.9870834410653,
-165.473529411765));
#155578=CARTESIAN_POINT('Ctrl Pts',(-4.12253084086667,14.4891929905171,
-166.967647058824));
#155579=CARTESIAN_POINT('Ctrl Pts',(-2.75624276724856,14.7445964952585,
-168.461764705882));
#155580=CARTESIAN_POINT('Ctrl Pts',(-1.38995469363044,15.,-169.955882352941));
#155581=CARTESIAN_POINT('Ctrl Pts',(-1.83697019872103E-15,15.,-171.45));
#155582=CARTESIAN_POINT('Ctrl Pts',(1.38995469363045,15.,-172.944117647059));
#155583=CARTESIAN_POINT('Ctrl Pts',(2.75624276724855,14.7445964952585,-174.438235294118));
#155584=CARTESIAN_POINT('Ctrl Pts',(4.12253084086666,14.4891929905171,-175.932352941176));
#155585=CARTESIAN_POINT('Ctrl Pts',(5.4186249928073,13.9870834410653,-177.426470588235));
#155586=CARTESIAN_POINT('Ctrl Pts',(6.71471914474792,13.4849738916136,-178.920588235294));
#155587=CARTESIAN_POINT('Ctrl Pts',(7.89648244316034,12.7532570359442,-180.414705882353));
#155588=CARTESIAN_POINT('Ctrl Pts',(9.07824574157275,12.0215401802748,-181.908823529412));
#155589=CARTESIAN_POINT('Ctrl Pts',(10.1054346546984,11.0851337583099,-183.402941176471));
#155590=CARTESIAN_POINT('Ctrl Pts',(11.132623567824,10.148727336345,-184.897058823529));
#155591=CARTESIAN_POINT('Ctrl Pts',(11.9702584092036,9.03951954568885,-186.391176470588));
#155592=CARTESIAN_POINT('Ctrl Pts',(12.8078932505832,7.93031175503273,-187.885294117647));
#155593=CARTESIAN_POINT('Ctrl Pts',(13.4274493703259,6.68607533664807,-189.379411764706));
#155594=CARTESIAN_POINT('Ctrl Pts',(14.0470054900687,5.44183891826343,-190.873529411765));
#155595=CARTESIAN_POINT('Ctrl Pts',(14.4273846475923,4.10494485108125,-192.367647058824));
#155596=CARTESIAN_POINT('Ctrl Pts',(14.8077638051159,2.76805078389905,-193.861764705882));
#155597=CARTESIAN_POINT('Ctrl Pts',(14.9360126444255,1.38402539194953,-195.355882352941));
#155598=CARTESIAN_POINT('Ctrl Pts',(15.0642614837351,2.76725994113625E-15,
-196.85));
#155599=CARTESIAN_POINT('Ctrl Pts',(14.9360126444255,-1.38402539194952,
-198.344117647059));
#155600=CARTESIAN_POINT('Ctrl Pts',(14.8077638051159,-2.76805078389906,
-199.838235294118));
#155601=CARTESIAN_POINT('Ctrl Pts',(14.4273846475923,-4.10494485108124,
-201.332352941176));
#155602=CARTESIAN_POINT('Ctrl Pts',(14.0470054900687,-5.44183891826342,
-202.826470588235));
#155603=CARTESIAN_POINT('Ctrl Pts',(13.4274493703259,-6.68607533664808,
-204.320588235294));
#155604=CARTESIAN_POINT('Ctrl Pts',(12.8078932505832,-7.93031175503273,
-205.814705882353));
#155605=CARTESIAN_POINT('Ctrl Pts',(11.9702584092036,-9.03951954568884,
-207.308823529412));
#155606=CARTESIAN_POINT('Ctrl Pts',(11.132623567824,-10.148727336345,-208.80294117647));
#155607=CARTESIAN_POINT('Ctrl Pts',(10.1054346546984,-11.0851337583099,
-210.297058823529));
#155608=CARTESIAN_POINT('Ctrl Pts',(9.07824574157275,-12.0215401802748,
-211.791176470588));
#155609=CARTESIAN_POINT('Ctrl Pts',(7.89648244316034,-12.7532570359442,
-213.285294117647));
#155610=CARTESIAN_POINT('Ctrl Pts',(6.71471914474792,-13.4849738916136,
-214.779411764706));
#155611=CARTESIAN_POINT('Ctrl Pts',(5.4186249928073,-13.9870834410653,-216.273529411765));
#155612=CARTESIAN_POINT('Ctrl Pts',(4.12253084086667,-14.4891929905171,
-217.767647058823));
#155613=CARTESIAN_POINT('Ctrl Pts',(2.75624276724855,-14.7445964952585,
-219.261764705882));
#155614=CARTESIAN_POINT('Ctrl Pts',(1.38995469363045,-15.,-220.755882352941));
#155615=CARTESIAN_POINT('Ctrl Pts',(0.,-15.,-222.25));
#155616=CARTESIAN_POINT('Ctrl Pts',(-1.38995469363045,-15.,-223.744117647059));
#155617=CARTESIAN_POINT('Ctrl Pts',(-2.75624276724856,-14.7445964952585,
-225.238235294118));
#155618=CARTESIAN_POINT('Ctrl Pts',(-4.12253084086666,-14.4891929905171,
-226.732352941176));
#155619=CARTESIAN_POINT('Ctrl Pts',(-5.41862499280729,-13.9870834410653,
-228.226470588235));
#155620=CARTESIAN_POINT('Ctrl Pts',(-6.71471914474793,-13.4849738916136,
-229.720588235294));
#155621=CARTESIAN_POINT('Ctrl Pts',(-7.89648244316034,-12.7532570359442,
-231.214705882353));
#155622=CARTESIAN_POINT('Ctrl Pts',(-9.07824574157275,-12.0215401802748,
-232.708823529412));
#155623=CARTESIAN_POINT('Ctrl Pts',(-10.1054346546984,-11.0851337583099,
-234.202941176471));
#155624=CARTESIAN_POINT('Ctrl Pts',(-11.132623567824,-10.148727336345,-235.697058823529));
#155625=CARTESIAN_POINT('Ctrl Pts',(-11.9702584092036,-9.03951954568885,
-237.191176470588));
#155626=CARTESIAN_POINT('Ctrl Pts',(-12.8078932505832,-7.93031175503273,
-238.685294117647));
#155627=CARTESIAN_POINT('Ctrl Pts',(-13.4274493703259,-6.68607533664808,
-240.179411764706));
#155628=CARTESIAN_POINT('Ctrl Pts',(-14.0470054900687,-5.44183891826343,
-241.673529411765));
#155629=CARTESIAN_POINT('Ctrl Pts',(-14.4273846475923,-4.10494485108124,
-243.167647058824));
#155630=CARTESIAN_POINT('Ctrl Pts',(-14.8077638051159,-2.76805078389906,
-244.661764705882));
#155631=CARTESIAN_POINT('Ctrl Pts',(-14.9360126444255,-1.38402539194953,
-246.155882352941));
#155632=CARTESIAN_POINT('Ctrl Pts',(-15.0642614837351,-9.22419980378748E-16,
-247.65));
#155633=CARTESIAN_POINT('Ctrl Pts',(-14.9360126444255,1.38402539194953,
-249.144117647059));
#155634=CARTESIAN_POINT('Ctrl Pts',(-14.8077638051159,2.76805078389906,
-250.638235294118));
#155635=CARTESIAN_POINT('Ctrl Pts',(-14.4273846475923,4.10494485108124,
-252.132352941177));
#155636=CARTESIAN_POINT('Ctrl Pts',(-14.0470054900687,5.44183891826343,
-253.626470588235));
#155637=CARTESIAN_POINT('Ctrl Pts',(-13.4274493703259,6.68607533664807,
-255.120588235294));
#155638=CARTESIAN_POINT('Ctrl Pts',(-12.8078932505832,7.93031175503273,
-256.614705882353));
#155639=CARTESIAN_POINT('Ctrl Pts',(-11.9702584092036,9.03951954568884,
-258.108823529412));
#155640=CARTESIAN_POINT('Ctrl Pts',(-11.132623567824,10.148727336345,-259.602941176471));
#155641=CARTESIAN_POINT('Ctrl Pts',(-10.1054346546984,11.0851337583099,
-261.097058823529));
#155642=CARTESIAN_POINT('Ctrl Pts',(-9.07824574157275,12.0215401802748,
-262.591176470588));
#155643=CARTESIAN_POINT('Ctrl Pts',(-7.89648244316034,12.7532570359442,
-264.085294117647));
#155644=CARTESIAN_POINT('Ctrl Pts',(-6.71471914474793,13.4849738916136,
-265.579411764706));
#155645=CARTESIAN_POINT('Ctrl Pts',(-5.41862499280729,13.9870834410653,
-267.073529411765));
#155646=CARTESIAN_POINT('Ctrl Pts',(-4.12253084086667,14.4891929905171,
-268.567647058823));
#155647=CARTESIAN_POINT('Ctrl Pts',(-2.75624276724856,14.7445964952585,
-270.061764705882));
#155648=CARTESIAN_POINT('Ctrl Pts',(-1.38995469363044,15.,-271.555882352941));
#155649=CARTESIAN_POINT('Ctrl Pts',(-1.83697019872103E-15,15.,-273.05));
#155650=CARTESIAN_POINT('Ctrl Pts',(1.38995469363045,15.,-274.544117647059));
#155651=CARTESIAN_POINT('Ctrl Pts',(2.75624276724855,14.7445964952585,-276.038235294118));
#155652=CARTESIAN_POINT('Ctrl Pts',(4.12253084086666,14.4891929905171,-277.532352941176));
#155653=CARTESIAN_POINT('Ctrl Pts',(5.4186249928073,13.9870834410653,-279.026470588235));
#155654=CARTESIAN_POINT('Ctrl Pts',(6.71471914474792,13.4849738916136,-280.520588235294));
#155655=CARTESIAN_POINT('Ctrl Pts',(7.89648244316034,12.7532570359442,-282.014705882353));
#155656=CARTESIAN_POINT('Ctrl Pts',(9.07824574157275,12.0215401802748,-283.508823529412));
#155657=CARTESIAN_POINT('Ctrl Pts',(10.1054346546984,11.0851337583099,-285.002941176471));
#155658=CARTESIAN_POINT('Ctrl Pts',(11.132623567824,10.148727336345,-286.497058823529));
#155659=CARTESIAN_POINT('Ctrl Pts',(11.9702584092036,9.03951954568885,-287.991176470588));
#155660=CARTESIAN_POINT('Ctrl Pts',(12.8078932505832,7.93031175503273,-289.485294117647));
#155661=CARTESIAN_POINT('Ctrl Pts',(13.4274493703259,6.68607533664807,-290.979411764706));
#155662=CARTESIAN_POINT('Ctrl Pts',(14.0470054900687,5.44183891826343,-292.473529411765));
#155663=CARTESIAN_POINT('Ctrl Pts',(14.4273846475923,4.10494485108125,-293.967647058824));
#155664=CARTESIAN_POINT('Ctrl Pts',(14.8077638051159,2.76805078389905,-295.461764705882));
#155665=CARTESIAN_POINT('Ctrl Pts',(14.9360126444255,1.38402539194953,-296.955882352941));
#155666=CARTESIAN_POINT('Ctrl Pts',(15.0642614837351,2.76725994113625E-15,
-298.45));
#155667=CARTESIAN_POINT('Ctrl Pts',(14.9360126444255,-1.38402539194952,
-299.944117647059));
#155668=CARTESIAN_POINT('Ctrl Pts',(14.8077638051159,-2.76805078389906,
-301.438235294118));
#155669=CARTESIAN_POINT('Ctrl Pts',(14.4273846475923,-4.10494485108124,
-302.932352941177));
#155670=CARTESIAN_POINT('Ctrl Pts',(14.0470054900687,-5.44183891826342,
-304.426470588235));
#155671=CARTESIAN_POINT('Ctrl Pts',(13.4274493703259,-6.68607533664808,
-305.920588235294));
#155672=CARTESIAN_POINT('Ctrl Pts',(12.8078932505832,-7.93031175503273,
-307.414705882353));
#155673=CARTESIAN_POINT('Ctrl Pts',(11.9702584092036,-9.03951954568884,
-308.908823529412));
#155674=CARTESIAN_POINT('Ctrl Pts',(11.132623567824,-10.148727336345,-310.402941176471));
#155675=CARTESIAN_POINT('Ctrl Pts',(10.1054346546984,-11.0851337583099,
-311.897058823529));
#155676=CARTESIAN_POINT('Ctrl Pts',(9.07824574157275,-12.0215401802748,
-313.391176470588));
#155677=CARTESIAN_POINT('Ctrl Pts',(7.89648244316034,-12.7532570359442,
-314.885294117647));
#155678=CARTESIAN_POINT('Ctrl Pts',(6.71471914474792,-13.4849738916136,
-316.379411764706));
#155679=CARTESIAN_POINT('Ctrl Pts',(5.4186249928073,-13.9870834410653,-317.873529411765));
#155680=CARTESIAN_POINT('Ctrl Pts',(4.12253084086667,-14.4891929905171,
-319.367647058824));
#155681=CARTESIAN_POINT('Ctrl Pts',(2.75624276724855,-14.7445964952585,
-320.861764705882));
#155682=CARTESIAN_POINT('Ctrl Pts',(1.38995469363045,-15.,-322.355882352941));
#155683=CARTESIAN_POINT('Ctrl Pts',(0.,-15.,-323.85));
#155684=CARTESIAN_POINT('Ctrl Pts',(-1.38995469363045,-15.,-325.344117647059));
#155685=CARTESIAN_POINT('Ctrl Pts',(-2.75624276724856,-14.7445964952585,
-326.838235294118));
#155686=CARTESIAN_POINT('Ctrl Pts',(-4.12253084086666,-14.4891929905171,
-328.332352941176));
#155687=CARTESIAN_POINT('Ctrl Pts',(-5.41862499280729,-13.9870834410653,
-329.826470588235));
#155688=CARTESIAN_POINT('Ctrl Pts',(-6.71471914474793,-13.4849738916136,
-331.320588235294));
#155689=CARTESIAN_POINT('Ctrl Pts',(-7.89648244316034,-12.7532570359442,
-332.814705882353));
#155690=CARTESIAN_POINT('Ctrl Pts',(-9.07824574157275,-12.0215401802748,
-334.308823529412));
#155691=CARTESIAN_POINT('Ctrl Pts',(-10.1054346546984,-11.0851337583099,
-335.80294117647));
#155692=CARTESIAN_POINT('Ctrl Pts',(-11.132623567824,-10.148727336345,-337.297058823529));
#155693=CARTESIAN_POINT('Ctrl Pts',(-11.9702584092036,-9.03951954568885,
-338.791176470588));
#155694=CARTESIAN_POINT('Ctrl Pts',(-12.8078932505832,-7.93031175503273,
-340.285294117647));
#155695=CARTESIAN_POINT('Ctrl Pts',(-13.4274493703259,-6.68607533664808,
-341.779411764706));
#155696=CARTESIAN_POINT('Ctrl Pts',(-14.0470054900687,-5.44183891826343,
-343.273529411765));
#155697=CARTESIAN_POINT('Ctrl Pts',(-14.4273846475923,-4.10494485108124,
-344.767647058823));
#155698=CARTESIAN_POINT('Ctrl Pts',(-14.8077638051159,-2.76805078389906,
-346.261764705882));
#155699=CARTESIAN_POINT('Ctrl Pts',(-14.9360126444255,-1.38402539194953,
-347.755882352941));
#155700=CARTESIAN_POINT('Ctrl Pts',(-15.0642614837351,-9.22419980378748E-16,
-349.25));
#155701=CARTESIAN_POINT('Ctrl Pts',(-14.9360126444255,1.38402539194953,
-350.744117647059));
#155702=CARTESIAN_POINT('Ctrl Pts',(-14.8077638051159,2.76805078389906,
-352.238235294118));
#155703=CARTESIAN_POINT('Ctrl Pts',(-14.4273846475923,4.10494485108124,
-353.732352941176));
#155704=CARTESIAN_POINT('Ctrl Pts',(-14.0470054900687,5.44183891826343,
-355.226470588235));
#155705=CARTESIAN_POINT('Ctrl Pts',(-13.4274493703259,6.68607533664807,
-356.720588235294));
#155706=CARTESIAN_POINT('Ctrl Pts',(-12.8078932505832,7.93031175503273,
-358.214705882353));
#155707=CARTESIAN_POINT('Ctrl Pts',(-11.9702584092036,9.03951954568884,
-359.708823529412));
#155708=CARTESIAN_POINT('Ctrl Pts',(-11.132623567824,10.148727336345,-361.202941176471));
#155709=CARTESIAN_POINT('Ctrl Pts',(-10.1054346546984,11.0851337583099,
-362.697058823529));
#155710=CARTESIAN_POINT('Ctrl Pts',(-9.07824574157275,12.0215401802748,
-364.191176470588));
#155711=CARTESIAN_POINT('Ctrl Pts',(-7.89648244316034,12.7532570359442,
-365.685294117647));
#155712=CARTESIAN_POINT('Ctrl Pts',(-6.71471914474793,13.4849738916136,
-367.179411764706));
#155713=CARTESIAN_POINT('Ctrl Pts',(-5.41862499280729,13.9870834410653,
-368.673529411765));
#155714=CARTESIAN_POINT('Ctrl Pts',(-4.12253084086667,14.4891929905171,
-370.167647058824));
#155715=CARTESIAN_POINT('Ctrl Pts',(-2.75624276724856,14.7445964952585,
-371.661764705882));
#155716=CARTESIAN_POINT('Ctrl Pts',(-1.38995469363044,15.,-373.155882352941));
#155717=CARTESIAN_POINT('Ctrl Pts',(-1.83697019872103E-15,15.,-374.65));
#155718=CARTESIAN_POINT('Ctrl Pts',(1.38995469363045,15.,-376.144117647059));
#155719=CARTESIAN_POINT('Ctrl Pts',(2.75624276724855,14.7445964952585,-377.638235294118));
#155720=CARTESIAN_POINT('Ctrl Pts',(4.12253084086666,14.4891929905171,-379.132352941177));
#155721=CARTESIAN_POINT('Ctrl Pts',(5.4186249928073,13.9870834410653,-380.626470588235));
#155722=CARTESIAN_POINT('Ctrl Pts',(6.71471914474792,13.4849738916136,-382.120588235294));
#155723=CARTESIAN_POINT('Ctrl Pts',(7.89648244316034,12.7532570359442,-383.614705882353));
#155724=CARTESIAN_POINT('Ctrl Pts',(9.07824574157275,12.0215401802748,-385.108823529412));
#155725=CARTESIAN_POINT('Ctrl Pts',(10.1054346546984,11.0851337583099,-386.602941176471));
#155726=CARTESIAN_POINT('Ctrl Pts',(11.132623567824,10.148727336345,-388.097058823529));
#155727=CARTESIAN_POINT('Ctrl Pts',(11.9702584092036,9.03951954568885,-389.591176470588));
#155728=CARTESIAN_POINT('Ctrl Pts',(12.8078932505832,7.93031175503273,-391.085294117647));
#155729=CARTESIAN_POINT('Ctrl Pts',(13.4274493703259,6.68607533664807,-392.579411764706));
#155730=CARTESIAN_POINT('Ctrl Pts',(14.0470054900687,5.44183891826343,-394.073529411765));
#155731=CARTESIAN_POINT('Ctrl Pts',(14.4273846475923,4.10494485108125,-395.567647058823));
#155732=CARTESIAN_POINT('Ctrl Pts',(14.8077638051159,2.76805078389905,-397.061764705882));
#155733=CARTESIAN_POINT('Ctrl Pts',(14.9360126444255,1.38402539194953,-398.555882352941));
#155734=CARTESIAN_POINT('Ctrl Pts',(15.0642614837351,2.76725994113625E-15,
-400.05));
#155735=CARTESIAN_POINT('Ctrl Pts',(14.9360126444255,-1.38402539194952,
-401.544117647059));
#155736=CARTESIAN_POINT('Ctrl Pts',(14.8077638051159,-2.76805078389906,
-403.038235294118));
#155737=CARTESIAN_POINT('Ctrl Pts',(14.4273846475923,-4.10494485108124,
-404.532352941176));
#155738=CARTESIAN_POINT('Ctrl Pts',(14.0470054900687,-5.44183891826342,
-406.026470588235));
#155739=CARTESIAN_POINT('Ctrl Pts',(13.4274493703259,-6.68607533664808,
-407.520588235294));
#155740=CARTESIAN_POINT('Ctrl Pts',(12.8078932505832,-7.93031175503273,
-409.014705882353));
#155741=CARTESIAN_POINT('Ctrl Pts',(11.9702584092036,-9.03951954568884,
-410.508823529412));
#155742=CARTESIAN_POINT('Ctrl Pts',(11.132623567824,-10.148727336345,-412.002941176471));
#155743=CARTESIAN_POINT('Ctrl Pts',(10.1054346546984,-11.0851337583099,
-413.497058823529));
#155744=CARTESIAN_POINT('Ctrl Pts',(9.07824574157275,-12.0215401802748,
-414.991176470588));
#155745=CARTESIAN_POINT('Ctrl Pts',(7.89648244316034,-12.7532570359442,
-416.485294117647));
#155746=CARTESIAN_POINT('Ctrl Pts',(6.71471914474792,-13.4849738916136,
-417.979411764706));
#155747=CARTESIAN_POINT('Ctrl Pts',(5.4186249928073,-13.9870834410653,-419.473529411765));
#155748=CARTESIAN_POINT('Ctrl Pts',(4.12253084086667,-14.4891929905171,
-420.967647058824));
#155749=CARTESIAN_POINT('Ctrl Pts',(2.75624276724855,-14.7445964952585,
-422.461764705882));
#155750=CARTESIAN_POINT('Ctrl Pts',(1.38995469363045,-15.,-423.955882352941));
#155751=CARTESIAN_POINT('Ctrl Pts',(0.,-15.,-425.45));
#155752=CARTESIAN_POINT('Ctrl Pts',(-1.38995469363045,-15.,-426.944117647059));
#155753=CARTESIAN_POINT('Ctrl Pts',(-2.75624276724856,-14.7445964952585,
-428.438235294118));
#155754=CARTESIAN_POINT('Ctrl Pts',(-4.12253084086666,-14.4891929905171,
-429.932352941177));
#155755=CARTESIAN_POINT('Ctrl Pts',(-5.41862499280729,-13.9870834410653,
-431.426470588235));
#155756=CARTESIAN_POINT('Ctrl Pts',(-6.71471914474793,-13.4849738916136,
-432.920588235294));
#155757=CARTESIAN_POINT('Ctrl Pts',(-7.89648244316034,-12.7532570359442,
-434.414705882353));
#155758=CARTESIAN_POINT('Ctrl Pts',(-9.07824574157275,-12.0215401802748,
-435.908823529412));
#155759=CARTESIAN_POINT('Ctrl Pts',(-10.1054346546984,-11.0851337583099,
-437.402941176471));
#155760=CARTESIAN_POINT('Ctrl Pts',(-11.132623567824,-10.148727336345,-438.89705882353));
#155761=CARTESIAN_POINT('Ctrl Pts',(-11.9702584092036,-9.03951954568885,
-440.391176470588));
#155762=CARTESIAN_POINT('Ctrl Pts',(-12.8078932505832,-7.93031175503273,
-441.885294117647));
#155763=CARTESIAN_POINT('Ctrl Pts',(-13.4274493703259,-6.68607533664808,
-443.379411764706));
#155764=CARTESIAN_POINT('Ctrl Pts',(-14.0470054900687,-5.44183891826343,
-444.873529411765));
#155765=CARTESIAN_POINT('Ctrl Pts',(-14.4273846475923,-4.10494485108124,
-446.367647058824));
#155766=CARTESIAN_POINT('Ctrl Pts',(-14.8077638051159,-2.76805078389906,
-447.861764705882));
#155767=CARTESIAN_POINT('Ctrl Pts',(-14.9360126444255,-1.38402539194953,
-449.355882352941));
#155768=CARTESIAN_POINT('Ctrl Pts',(-15.0642614837351,-9.22419980378748E-16,
-450.85));
#155769=CARTESIAN_POINT('Ctrl Pts',(-14.9360126444255,1.38402539194953,
-452.344117647059));
#155770=CARTESIAN_POINT('Ctrl Pts',(-14.8077638051159,2.76805078389906,
-453.838235294118));
#155771=CARTESIAN_POINT('Ctrl Pts',(-14.4273846475923,4.10494485108124,
-455.332352941176));
#155772=CARTESIAN_POINT('Ctrl Pts',(-14.0470054900687,5.44183891826343,
-456.826470588235));
#155773=CARTESIAN_POINT('Ctrl Pts',(-13.4274493703259,6.68607533664807,
-458.320588235294));
#155774=CARTESIAN_POINT('Ctrl Pts',(-12.8078932505832,7.93031175503273,
-459.814705882353));
#155775=CARTESIAN_POINT('Ctrl Pts',(-11.9702584092036,9.03951954568884,
-461.308823529412));
#155776=CARTESIAN_POINT('Ctrl Pts',(-11.132623567824,10.148727336345,-462.802941176471));
#155777=CARTESIAN_POINT('Ctrl Pts',(-10.1054346546984,11.0851337583099,
-464.297058823529));
#155778=CARTESIAN_POINT('Ctrl Pts',(-9.07824574157275,12.0215401802748,
-465.791176470588));
#155779=CARTESIAN_POINT('Ctrl Pts',(-7.89648244316034,12.7532570359442,
-467.285294117647));
#155780=CARTESIAN_POINT('Ctrl Pts',(-6.71471914474793,13.4849738916136,
-468.779411764706));
#155781=CARTESIAN_POINT('Ctrl Pts',(-5.41862499280729,13.9870834410653,
-470.273529411765));
#155782=CARTESIAN_POINT('Ctrl Pts',(-4.12253084086667,14.4891929905171,
-471.767647058824));
#155783=CARTESIAN_POINT('Ctrl Pts',(-2.75624276724856,14.7445964952585,
-473.261764705882));
#155784=CARTESIAN_POINT('Ctrl Pts',(-1.38995469363044,15.,-474.755882352941));
#155785=CARTESIAN_POINT('Ctrl Pts',(-1.83697019872103E-15,15.,-476.25));
#155786=CARTESIAN_POINT('Ctrl Pts',(1.38995469363045,15.,-477.744117647059));
#155787=CARTESIAN_POINT('Ctrl Pts',(2.75624276724855,14.7445964952585,-479.238235294118));
#155788=CARTESIAN_POINT('Ctrl Pts',(4.12253084086666,14.4891929905171,-480.732352941176));
#155789=CARTESIAN_POINT('Ctrl Pts',(5.4186249928073,13.9870834410653,-482.226470588235));
#155790=CARTESIAN_POINT('Ctrl Pts',(6.71471914474792,13.4849738916136,-483.720588235294));
#155791=CARTESIAN_POINT('Ctrl Pts',(7.89648244316034,12.7532570359442,-485.214705882353));
#155792=CARTESIAN_POINT('Ctrl Pts',(9.07824574157275,12.0215401802748,-486.708823529412));
#155793=CARTESIAN_POINT('Ctrl Pts',(10.1054346546984,11.0851337583099,-488.202941176471));
#155794=CARTESIAN_POINT('Ctrl Pts',(11.132623567824,10.148727336345,-489.697058823529));
#155795=CARTESIAN_POINT('Ctrl Pts',(11.9702584092036,9.03951954568885,-491.191176470588));
#155796=CARTESIAN_POINT('Ctrl Pts',(12.8078932505832,7.93031175503273,-492.685294117647));
#155797=CARTESIAN_POINT('Ctrl Pts',(13.4274493703259,6.68607533664807,-494.179411764706));
#155798=CARTESIAN_POINT('Ctrl Pts',(14.0470054900687,5.44183891826343,-495.673529411765));
#155799=CARTESIAN_POINT('Ctrl Pts',(14.4273846475923,4.10494485108125,-497.167647058824));
#155800=CARTESIAN_POINT('Ctrl Pts',(14.8077638051159,2.76805078389905,-498.661764705882));
#155801=CARTESIAN_POINT('Ctrl Pts',(14.9360126444255,1.38402539194953,-500.155882352941));
#155802=CARTESIAN_POINT('Ctrl Pts',(15.0642614837351,2.76725994113625E-15,
-501.65));
#155803=CARTESIAN_POINT('Ctrl Pts',(14.9360126444255,-1.38402539194952,
-503.144117647059));
#155804=CARTESIAN_POINT('Ctrl Pts',(14.8077638051159,-2.76805078389906,
-504.638235294118));
#155805=CARTESIAN_POINT('Ctrl Pts',(14.4273846475923,-4.10494485108124,
-506.132352941176));
#155806=CARTESIAN_POINT('Ctrl Pts',(14.0470054900687,-5.44183891826342,
-507.626470588235));
#155807=CARTESIAN_POINT('Ctrl Pts',(13.4274493703259,-6.68607533664808,
-509.120588235294));
#155808=CARTESIAN_POINT('Ctrl Pts',(12.8078932505832,-7.93031175503273,
-510.614705882353));
#155809=CARTESIAN_POINT('Ctrl Pts',(11.9702584092036,-9.03951954568884,
-512.108823529412));
#155810=CARTESIAN_POINT('Ctrl Pts',(11.132623567824,-10.148727336345,-513.602941176471));
#155811=CARTESIAN_POINT('Ctrl Pts',(10.1054346546984,-11.0851337583099,
-515.09705882353));
#155812=CARTESIAN_POINT('Ctrl Pts',(9.07824574157275,-12.0215401802748,
-516.591176470588));
#155813=CARTESIAN_POINT('Ctrl Pts',(7.89648244316034,-12.7532570359442,
-518.085294117647));
#155814=CARTESIAN_POINT('Ctrl Pts',(6.71471914474792,-13.4849738916136,
-519.579411764706));
#155815=CARTESIAN_POINT('Ctrl Pts',(5.4186249928073,-13.9870834410653,-521.073529411765));
#155816=CARTESIAN_POINT('Ctrl Pts',(4.12253084086667,-14.4891929905171,
-522.567647058823));
#155817=CARTESIAN_POINT('Ctrl Pts',(2.75624276724855,-14.7445964952585,
-524.061764705882));
#155818=CARTESIAN_POINT('Ctrl Pts',(1.38995469363045,-15.,-525.555882352941));
#155819=CARTESIAN_POINT('Ctrl Pts',(0.,-15.,-527.05));
#155820=CARTESIAN_POINT('Ctrl Pts',(-1.38995469363045,-15.,-528.544117647059));
#155821=CARTESIAN_POINT('Ctrl Pts',(-2.75624276724856,-14.7445964952585,
-530.038235294118));
#155822=CARTESIAN_POINT('Ctrl Pts',(-4.12253084086666,-14.4891929905171,
-531.532352941177));
#155823=CARTESIAN_POINT('Ctrl Pts',(-5.41862499280729,-13.9870834410653,
-533.026470588235));
#155824=CARTESIAN_POINT('Ctrl Pts',(-6.71471914474793,-13.4849738916136,
-534.520588235294));
#155825=CARTESIAN_POINT('Ctrl Pts',(-7.89648244316034,-12.7532570359442,
-536.014705882353));
#155826=CARTESIAN_POINT('Ctrl Pts',(-9.07824574157275,-12.0215401802748,
-537.508823529412));
#155827=CARTESIAN_POINT('Ctrl Pts',(-10.1054346546984,-11.0851337583099,
-539.00294117647));
#155828=CARTESIAN_POINT('Ctrl Pts',(-11.132623567824,-10.148727336345,-540.49705882353));
#155829=CARTESIAN_POINT('Ctrl Pts',(-11.9702584092036,-9.03951954568885,
-541.991176470588));
#155830=CARTESIAN_POINT('Ctrl Pts',(-12.8078932505832,-7.93031175503273,
-543.485294117647));
#155831=CARTESIAN_POINT('Ctrl Pts',(-13.4274493703259,-6.68607533664808,
-544.979411764706));
#155832=CARTESIAN_POINT('Ctrl Pts',(-14.0470054900687,-5.44183891826343,
-546.473529411765));
#155833=CARTESIAN_POINT('Ctrl Pts',(-14.4273846475923,-4.10494485108124,
-547.967647058823));
#155834=CARTESIAN_POINT('Ctrl Pts',(-14.8077638051159,-2.76805078389906,
-549.461764705882));
#155835=CARTESIAN_POINT('Ctrl Pts',(-14.9360126444255,-1.38402539194953,
-550.955882352941));
#155836=CARTESIAN_POINT('Ctrl Pts',(-15.0642614837351,-9.22419980378748E-16,
-552.45));
#155837=CARTESIAN_POINT('Ctrl Pts',(-14.9360126444255,1.38402539194953,
-553.944117647059));
#155838=CARTESIAN_POINT('Ctrl Pts',(-14.8077638051159,2.76805078389906,
-555.438235294118));
#155839=CARTESIAN_POINT('Ctrl Pts',(-14.4273846475923,4.10494485108124,
-556.932352941177));
#155840=CARTESIAN_POINT('Ctrl Pts',(-14.0470054900687,5.44183891826343,
-558.426470588235));
#155841=CARTESIAN_POINT('Ctrl Pts',(-13.4274493703259,6.68607533664807,
-559.920588235294));
#155842=CARTESIAN_POINT('Ctrl Pts',(-12.8078932505832,7.93031175503273,
-561.414705882353));
#155843=CARTESIAN_POINT('Ctrl Pts',(-11.9702584092036,9.03951954568884,
-562.908823529412));
#155844=CARTESIAN_POINT('Ctrl Pts',(-11.132623567824,10.148727336345,-564.402941176471));
#155845=CARTESIAN_POINT('Ctrl Pts',(-10.1054346546984,11.0851337583099,
-565.897058823529));
#155846=CARTESIAN_POINT('Ctrl Pts',(-9.07824574157275,12.0215401802748,
-567.391176470588));
#155847=CARTESIAN_POINT('Ctrl Pts',(-7.89648244316034,12.7532570359442,
-568.885294117647));
#155848=CARTESIAN_POINT('Ctrl Pts',(-6.71471914474793,13.4849738916136,
-570.379411764706));
#155849=CARTESIAN_POINT('Ctrl Pts',(-5.41862499280729,13.9870834410653,
-571.873529411765));
#155850=CARTESIAN_POINT('Ctrl Pts',(-4.12253084086667,14.4891929905171,
-573.367647058824));
#155851=CARTESIAN_POINT('Ctrl Pts',(-2.75624276724856,14.7445964952585,
-574.861764705882));
#155852=CARTESIAN_POINT('Ctrl Pts',(-1.38995469363044,15.,-576.355882352941));
#155853=CARTESIAN_POINT('Ctrl Pts',(-1.83697019872103E-15,15.,-577.85));
#155854=CARTESIAN_POINT('Ctrl Pts',(1.38995469363045,15.,-579.344117647059));
#155855=CARTESIAN_POINT('Ctrl Pts',(2.75624276724855,14.7445964952585,-580.838235294117));
#155856=CARTESIAN_POINT('Ctrl Pts',(4.12253084086666,14.4891929905171,-582.332352941176));
#155857=CARTESIAN_POINT('Ctrl Pts',(5.4186249928073,13.9870834410653,-583.826470588235));
#155858=CARTESIAN_POINT('Ctrl Pts',(6.71471914474792,13.4849738916136,-585.320588235294));
#155859=CARTESIAN_POINT('Ctrl Pts',(7.89648244316034,12.7532570359442,-586.814705882353));
#155860=CARTESIAN_POINT('Ctrl Pts',(9.07824574157275,12.0215401802748,-588.308823529412));
#155861=CARTESIAN_POINT('Ctrl Pts',(10.1054346546984,11.0851337583099,-589.802941176471));
#155862=CARTESIAN_POINT('Ctrl Pts',(11.132623567824,10.148727336345,-591.297058823529));
#155863=CARTESIAN_POINT('Ctrl Pts',(11.9702584092036,9.03951954568885,-592.791176470588));
#155864=CARTESIAN_POINT('Ctrl Pts',(12.8078932505832,7.93031175503273,-594.285294117647));
#155865=CARTESIAN_POINT('Ctrl Pts',(13.4274493703259,6.68607533664807,-595.779411764706));
#155866=CARTESIAN_POINT('Ctrl Pts',(14.0470054900687,5.44183891826343,-597.273529411765));
#155867=CARTESIAN_POINT('Ctrl Pts',(14.4273846475923,4.10494485108125,-598.767647058824));
#155868=CARTESIAN_POINT('Ctrl Pts',(14.8077638051159,2.76805078389905,-600.261764705882));
#155869=CARTESIAN_POINT('Ctrl Pts',(14.9360126444255,1.38402539194953,-601.755882352941));
#155870=CARTESIAN_POINT('Ctrl Pts',(15.0642614837351,2.76725994113625E-15,
-603.25));
#155871=CARTESIAN_POINT('Ctrl Pts',(14.9360126444255,-1.38402539194952,
-604.744117647059));
#155872=CARTESIAN_POINT('Ctrl Pts',(14.8077638051159,-2.76805078389906,
-606.238235294118));
#155873=CARTESIAN_POINT('Ctrl Pts',(14.4273846475923,-4.10494485108124,
-607.732352941176));
#155874=CARTESIAN_POINT('Ctrl Pts',(14.0470054900687,-5.44183891826342,
-609.226470588235));
#155875=CARTESIAN_POINT('Ctrl Pts',(13.4274493703259,-6.68607533664808,
-610.720588235294));
#155876=CARTESIAN_POINT('Ctrl Pts',(12.8078932505832,-7.93031175503273,
-612.214705882353));
#155877=CARTESIAN_POINT('Ctrl Pts',(11.9702584092036,-9.03951954568884,
-613.708823529412));
#155878=CARTESIAN_POINT('Ctrl Pts',(11.132623567824,-10.148727336345,-615.202941176471));
#155879=CARTESIAN_POINT('Ctrl Pts',(10.1054346546984,-11.0851337583099,
-616.697058823529));
#155880=CARTESIAN_POINT('Ctrl Pts',(9.07824574157275,-12.0215401802748,
-618.191176470588));
#155881=CARTESIAN_POINT('Ctrl Pts',(7.89648244316034,-12.7532570359442,
-619.685294117647));
#155882=CARTESIAN_POINT('Ctrl Pts',(6.71471914474792,-13.4849738916136,
-621.179411764706));
#155883=CARTESIAN_POINT('Ctrl Pts',(5.4186249928073,-13.9870834410653,-622.673529411764));
#155884=CARTESIAN_POINT('Ctrl Pts',(4.12253084086667,-14.4891929905171,
-624.167647058823));
#155885=CARTESIAN_POINT('Ctrl Pts',(2.75624276724855,-14.7445964952585,
-625.661764705882));
#155886=CARTESIAN_POINT('Ctrl Pts',(1.38995469363045,-15.,-627.155882352941));
#155887=CARTESIAN_POINT('Ctrl Pts',(0.,-15.,-628.65));
#155888=CARTESIAN_POINT('Ctrl Pts',(-1.38995469363045,-15.,-630.144117647059));
#155889=CARTESIAN_POINT('Ctrl Pts',(-2.75624276724856,-14.7445964952585,
-631.638235294118));
#155890=CARTESIAN_POINT('Ctrl Pts',(-4.12253084086666,-14.4891929905171,
-633.132352941176));
#155891=CARTESIAN_POINT('Ctrl Pts',(-5.41862499280729,-13.9870834410653,
-634.626470588235));
#155892=CARTESIAN_POINT('Ctrl Pts',(-6.71471914474793,-13.4849738916136,
-636.120588235294));
#155893=CARTESIAN_POINT('Ctrl Pts',(-7.89648244316034,-12.7532570359442,
-637.614705882353));
#155894=CARTESIAN_POINT('Ctrl Pts',(-9.07824574157275,-12.0215401802748,
-639.108823529412));
#155895=CARTESIAN_POINT('Ctrl Pts',(-10.1054346546984,-11.0851337583099,
-640.60294117647));
#155896=CARTESIAN_POINT('Ctrl Pts',(-11.132623567824,-10.148727336345,-642.097058823529));
#155897=CARTESIAN_POINT('Ctrl Pts',(-11.9702584092036,-9.03951954568885,
-643.591176470588));
#155898=CARTESIAN_POINT('Ctrl Pts',(-12.8078932505832,-7.93031175503273,
-645.085294117647));
#155899=CARTESIAN_POINT('Ctrl Pts',(-13.4274493703259,-6.68607533664808,
-646.579411764706));
#155900=CARTESIAN_POINT('Ctrl Pts',(-14.0470054900687,-5.44183891826343,
-648.073529411765));
#155901=CARTESIAN_POINT('Ctrl Pts',(-14.4273846475923,-4.10494485108124,
-649.567647058824));
#155902=CARTESIAN_POINT('Ctrl Pts',(-14.8077638051159,-2.76805078389906,
-651.061764705883));
#155903=CARTESIAN_POINT('Ctrl Pts',(-14.9360126444255,-1.38402539194953,
-652.555882352941));
#155904=CARTESIAN_POINT('Ctrl Pts',(-15.0642614837351,-9.22419980378748E-16,
-654.05));
#155905=CARTESIAN_POINT('Ctrl Pts',(-14.9360126444255,1.38402539194953,
-655.544117647059));
#155906=CARTESIAN_POINT('Ctrl Pts',(-14.8077638051159,2.76805078389906,
-657.038235294117));
#155907=CARTESIAN_POINT('Ctrl Pts',(-14.4273846475923,4.10494485108124,
-658.532352941177));
#155908=CARTESIAN_POINT('Ctrl Pts',(-14.0470054900687,5.44183891826343,
-660.026470588235));
#155909=CARTESIAN_POINT('Ctrl Pts',(-13.4274493703259,6.68607533664807,
-661.520588235294));
#155910=CARTESIAN_POINT('Ctrl Pts',(-12.8078932505832,7.93031175503273,
-663.014705882353));
#155911=CARTESIAN_POINT('Ctrl Pts',(-11.9702584092036,9.03951954568884,
-664.508823529412));
#155912=CARTESIAN_POINT('Ctrl Pts',(-11.132623567824,10.148727336345,-666.002941176471));
#155913=CARTESIAN_POINT('Ctrl Pts',(-10.1054346546984,11.0851337583099,
-667.497058823529));
#155914=CARTESIAN_POINT('Ctrl Pts',(-9.07824574157275,12.0215401802748,
-668.991176470588));
#155915=CARTESIAN_POINT('Ctrl Pts',(-7.89648244316034,12.7532570359442,
-670.485294117647));
#155916=CARTESIAN_POINT('Ctrl Pts',(-6.71471914474793,13.4849738916136,
-671.979411764706));
#155917=CARTESIAN_POINT('Ctrl Pts',(-5.41862499280729,13.9870834410653,
-673.473529411765));
#155918=CARTESIAN_POINT('Ctrl Pts',(-4.12253084086667,14.4891929905171,
-674.967647058824));
#155919=CARTESIAN_POINT('Ctrl Pts',(-2.75624276724856,14.7445964952585,
-676.461764705882));
#155920=CARTESIAN_POINT('Ctrl Pts',(-1.38995469363044,15.,-677.955882352941));
#155921=CARTESIAN_POINT('Ctrl Pts',(-1.83697019872103E-15,15.,-679.45));
#155922=CARTESIAN_POINT('Ctrl Pts',(1.38995469363045,15.,-680.944117647059));
#155923=CARTESIAN_POINT('Ctrl Pts',(2.75624276724855,14.7445964952585,-682.438235294117));
#155924=CARTESIAN_POINT('Ctrl Pts',(4.12253084086666,14.4891929905171,-683.932352941176));
#155925=CARTESIAN_POINT('Ctrl Pts',(5.4186249928073,13.9870834410653,-685.426470588235));
#155926=CARTESIAN_POINT('Ctrl Pts',(6.71471914474792,13.4849738916136,-686.920588235294));
#155927=CARTESIAN_POINT('Ctrl Pts',(7.89648244316034,12.7532570359442,-688.414705882353));
#155928=CARTESIAN_POINT('Ctrl Pts',(9.07824574157275,12.0215401802748,-689.908823529412));
#155929=CARTESIAN_POINT('Ctrl Pts',(10.1054346546984,11.0851337583099,-691.402941176471));
#155930=CARTESIAN_POINT('Ctrl Pts',(11.132623567824,10.148727336345,-692.89705882353));
#155931=CARTESIAN_POINT('Ctrl Pts',(11.9702584092036,9.03951954568885,-694.391176470588));
#155932=CARTESIAN_POINT('Ctrl Pts',(12.8078932505832,7.93031175503273,-695.885294117647));
#155933=CARTESIAN_POINT('Ctrl Pts',(13.4274493703259,6.68607533664807,-697.379411764706));
#155934=CARTESIAN_POINT('Ctrl Pts',(14.0470054900687,5.44183891826343,-698.873529411764));
#155935=CARTESIAN_POINT('Ctrl Pts',(14.4273846475923,4.10494485108125,-700.367647058823));
#155936=CARTESIAN_POINT('Ctrl Pts',(14.8077638051159,2.76805078389905,-701.861764705882));
#155937=CARTESIAN_POINT('Ctrl Pts',(14.9360126444255,1.38402539194953,-703.355882352941));
#155938=CARTESIAN_POINT('Ctrl Pts',(15.0642614837351,2.76725994113625E-15,
-704.85));
#155939=CARTESIAN_POINT('Ctrl Pts',(14.9360126444255,-1.38402539194952,
-706.344117647059));
#155940=CARTESIAN_POINT('Ctrl Pts',(14.8077638051159,-2.76805078389906,
-707.838235294118));
#155941=CARTESIAN_POINT('Ctrl Pts',(14.4273846475923,-4.10494485108124,
-709.332352941177));
#155942=CARTESIAN_POINT('Ctrl Pts',(14.0470054900687,-5.44183891826342,
-710.826470588236));
#155943=CARTESIAN_POINT('Ctrl Pts',(13.4274493703259,-6.68607533664808,
-712.320588235294));
#155944=CARTESIAN_POINT('Ctrl Pts',(12.8078932505832,-7.93031175503273,
-713.814705882353));
#155945=CARTESIAN_POINT('Ctrl Pts',(11.9702584092036,-9.03951954568884,
-715.308823529412));
#155946=CARTESIAN_POINT('Ctrl Pts',(11.132623567824,-10.148727336345,-716.802941176471));
#155947=CARTESIAN_POINT('Ctrl Pts',(10.1054346546984,-11.0851337583099,
-718.297058823529));
#155948=CARTESIAN_POINT('Ctrl Pts',(9.07824574157275,-12.0215401802748,
-719.791176470588));
#155949=CARTESIAN_POINT('Ctrl Pts',(7.89648244316034,-12.7532570359442,
-721.285294117647));
#155950=CARTESIAN_POINT('Ctrl Pts',(6.71471914474792,-13.4849738916136,
-722.779411764706));
#155951=CARTESIAN_POINT('Ctrl Pts',(5.4186249928073,-13.9870834410653,-724.273529411765));
#155952=CARTESIAN_POINT('Ctrl Pts',(4.12253084086667,-14.4891929905171,
-725.767647058824));
#155953=CARTESIAN_POINT('Ctrl Pts',(2.75624276724855,-14.7445964952585,
-727.261764705882));
#155954=CARTESIAN_POINT('Ctrl Pts',(1.38995469363045,-15.,-728.755882352941));
#155955=CARTESIAN_POINT('Ctrl Pts',(0.,-15.,-730.25));
#155956=CARTESIAN_POINT('Ctrl Pts',(-1.38995469363045,-15.,-731.744117647059));
#155957=CARTESIAN_POINT('Ctrl Pts',(-2.75624276724856,-14.7445964952585,
-733.238235294118));
#155958=CARTESIAN_POINT('Ctrl Pts',(-4.12253084086666,-14.4891929905171,
-734.732352941177));
#155959=CARTESIAN_POINT('Ctrl Pts',(-5.41862499280729,-13.9870834410653,
-736.226470588235));
#155960=CARTESIAN_POINT('Ctrl Pts',(-6.71471914474793,-13.4849738916136,
-737.720588235294));
#155961=CARTESIAN_POINT('Ctrl Pts',(-7.89648244316034,-12.7532570359442,
-739.214705882353));
#155962=CARTESIAN_POINT('Ctrl Pts',(-9.07824574157275,-12.0215401802748,
-740.708823529412));
#155963=CARTESIAN_POINT('Ctrl Pts',(-10.1054346546984,-11.0851337583099,
-742.20294117647));
#155964=CARTESIAN_POINT('Ctrl Pts',(-11.132623567824,-10.148727336345,-743.697058823529));
#155965=CARTESIAN_POINT('Ctrl Pts',(-11.9702584092036,-9.03951954568885,
-745.191176470588));
#155966=CARTESIAN_POINT('Ctrl Pts',(-12.8078932505832,-7.93031175503273,
-746.685294117647));
#155967=CARTESIAN_POINT('Ctrl Pts',(-13.4274493703259,-6.68607533664808,
-748.179411764706));
#155968=CARTESIAN_POINT('Ctrl Pts',(-14.0470054900687,-5.44183891826343,
-749.673529411765));
#155969=CARTESIAN_POINT('Ctrl Pts',(-14.4273846475923,-4.10494485108124,
-751.167647058824));
#155970=CARTESIAN_POINT('Ctrl Pts',(-14.8077638051159,-2.76805078389906,
-752.661764705882));
#155971=CARTESIAN_POINT('Ctrl Pts',(-14.9360126444255,-1.38402539194953,
-754.155882352941));
#155972=CARTESIAN_POINT('Ctrl Pts',(-15.0642614837351,-9.22419980378748E-16,
-755.65));
#155973=CARTESIAN_POINT('Ctrl Pts',(-14.9360126444255,1.38402539194953,
-757.144117647059));
#155974=CARTESIAN_POINT('Ctrl Pts',(-14.8077638051159,2.76805078389906,
-758.638235294118));
#155975=CARTESIAN_POINT('Ctrl Pts',(-14.4273846475923,4.10494485108124,
-760.132352941176));
#155976=CARTESIAN_POINT('Ctrl Pts',(-14.0470054900687,5.44183891826343,
-761.626470588235));
#155977=CARTESIAN_POINT('Ctrl Pts',(-13.4274493703259,6.68607533664807,
-763.120588235294));
#155978=CARTESIAN_POINT('Ctrl Pts',(-12.8078932505832,7.93031175503273,
-764.614705882353));
#155979=CARTESIAN_POINT('Ctrl Pts',(-11.9702584092036,9.03951954568884,
-766.108823529412));
#155980=CARTESIAN_POINT('Ctrl Pts',(-11.132623567824,10.148727336345,-767.602941176471));
#155981=CARTESIAN_POINT('Ctrl Pts',(-10.1054346546984,11.0851337583099,
-769.09705882353));
#155982=CARTESIAN_POINT('Ctrl Pts',(-9.07824574157275,12.0215401802748,
-770.591176470589));
#155983=CARTESIAN_POINT('Ctrl Pts',(-7.89648244316034,12.7532570359442,
-772.085294117647));
#155984=CARTESIAN_POINT('Ctrl Pts',(-6.71471914474793,13.4849738916136,
-773.579411764706));
#155985=CARTESIAN_POINT('Ctrl Pts',(-5.41862499280729,13.9870834410653,
-775.073529411765));
#155986=CARTESIAN_POINT('Ctrl Pts',(-4.12253084086667,14.4891929905171,
-776.567647058824));
#155987=CARTESIAN_POINT('Ctrl Pts',(-2.75624276724856,14.7445964952585,
-778.061764705882));
#155988=CARTESIAN_POINT('Ctrl Pts',(-1.38995469363044,15.,-779.555882352941));
#155989=CARTESIAN_POINT('Ctrl Pts',(-1.83697019872103E-15,15.,-781.05));
#155990=CARTESIAN_POINT('Ctrl Pts',(1.38995469363045,15.,-782.544117647059));
#155991=CARTESIAN_POINT('Ctrl Pts',(2.75624276724855,14.7445964952585,-784.038235294118));
#155992=CARTESIAN_POINT('Ctrl Pts',(4.12253084086666,14.4891929905171,-785.532352941177));
#155993=CARTESIAN_POINT('Ctrl Pts',(5.4186249928073,13.9870834410653,-787.026470588235));
#155994=CARTESIAN_POINT('Ctrl Pts',(6.71471914474792,13.4849738916136,-788.520588235294));
#155995=CARTESIAN_POINT('Ctrl Pts',(7.89648244316034,12.7532570359442,-790.014705882353));
#155996=CARTESIAN_POINT('Ctrl Pts',(9.07824574157275,12.0215401802748,-791.508823529412));
#155997=CARTESIAN_POINT('Ctrl Pts',(10.1054346546984,11.0851337583099,-793.002941176471));
#155998=CARTESIAN_POINT('Ctrl Pts',(11.132623567824,10.148727336345,-794.497058823529));
#155999=CARTESIAN_POINT('Ctrl Pts',(11.9702584092036,9.03951954568885,-795.991176470588));
#156000=CARTESIAN_POINT('Ctrl Pts',(12.8078932505832,7.93031175503273,-797.485294117647));
#156001=CARTESIAN_POINT('Ctrl Pts',(13.4274493703259,6.68607533664807,-798.979411764706));
#156002=CARTESIAN_POINT('Ctrl Pts',(14.0470054900687,5.44183891826343,-800.473529411765));
#156003=CARTESIAN_POINT('Ctrl Pts',(14.4273846475923,4.10494485108125,-801.967647058823));
#156004=CARTESIAN_POINT('Ctrl Pts',(14.8077638051159,2.76805078389905,-803.461764705882));
#156005=CARTESIAN_POINT('Ctrl Pts',(14.9360126444255,1.38402539194953,-804.955882352941));
#156006=CARTESIAN_POINT('Ctrl Pts',(15.0642614837351,2.76725994113625E-15,
-806.45));
#156007=CARTESIAN_POINT('Ctrl Pts',(14.9360126444255,-1.38402539194952,
-807.944117647059));
#156008=CARTESIAN_POINT('Ctrl Pts',(14.8077638051159,-2.76805078389906,
-809.438235294118));
#156009=CARTESIAN_POINT('Ctrl Pts',(14.4273846475923,-4.10494485108124,
-810.932352941177));
#156010=CARTESIAN_POINT('Ctrl Pts',(14.0470054900687,-5.44183891826342,
-812.426470588235));
#156011=CARTESIAN_POINT('Ctrl Pts',(13.4274493703259,-6.68607533664808,
-813.920588235294));
#156012=CARTESIAN_POINT('Ctrl Pts',(12.8078932505832,-7.93031175503273,
-815.414705882353));
#156013=CARTESIAN_POINT('Ctrl Pts',(11.9702584092036,-9.03951954568884,
-816.908823529412));
#156014=CARTESIAN_POINT('Ctrl Pts',(11.132623567824,-10.148727336345,-818.40294117647));
#156015=CARTESIAN_POINT('Ctrl Pts',(10.1054346546984,-11.0851337583099,
-819.897058823529));
#156016=CARTESIAN_POINT('Ctrl Pts',(9.07824574157275,-12.0215401802748,
-821.391176470588));
#156017=CARTESIAN_POINT('Ctrl Pts',(7.89648244316034,-12.7532570359442,
-822.885294117647));
#156018=CARTESIAN_POINT('Ctrl Pts',(6.71471914474792,-13.4849738916136,
-824.379411764706));
#156019=CARTESIAN_POINT('Ctrl Pts',(5.4186249928073,-13.9870834410653,-825.873529411765));
#156020=CARTESIAN_POINT('Ctrl Pts',(4.12253084086667,-14.4891929905171,
-827.367647058824));
#156021=CARTESIAN_POINT('Ctrl Pts',(2.75624276724855,-14.7445964952585,
-828.861764705882));
#156022=CARTESIAN_POINT('Ctrl Pts',(1.38995469363045,-15.,-830.355882352941));
#156023=CARTESIAN_POINT('Ctrl Pts',(0.,-15.,-831.85));
#156024=CARTESIAN_POINT('Ctrl Pts',(-1.38995469363045,-15.,-833.344117647059));
#156025=CARTESIAN_POINT('Ctrl Pts',(-2.75624276724856,-14.7445964952585,
-834.838235294118));
#156026=CARTESIAN_POINT('Ctrl Pts',(-4.12253084086666,-14.4891929905171,
-836.332352941177));
#156027=CARTESIAN_POINT('Ctrl Pts',(-5.41862499280729,-13.9870834410653,
-837.826470588235));
#156028=CARTESIAN_POINT('Ctrl Pts',(-6.71471914474793,-13.4849738916136,
-839.320588235294));
#156029=CARTESIAN_POINT('Ctrl Pts',(-7.89648244316034,-12.7532570359442,
-840.814705882353));
#156030=CARTESIAN_POINT('Ctrl Pts',(-9.07824574157275,-12.0215401802748,
-842.308823529412));
#156031=CARTESIAN_POINT('Ctrl Pts',(-10.1054346546984,-11.0851337583099,
-843.802941176471));
#156032=CARTESIAN_POINT('Ctrl Pts',(-11.132623567824,-10.148727336345,-845.29705882353));
#156033=CARTESIAN_POINT('Ctrl Pts',(-11.9702584092036,-9.03951954568885,
-846.791176470588));
#156034=CARTESIAN_POINT('Ctrl Pts',(-12.8078932505832,-7.93031175503273,
-848.285294117647));
#156035=CARTESIAN_POINT('Ctrl Pts',(-13.4274493703259,-6.68607533664808,
-849.779411764706));
#156036=CARTESIAN_POINT('Ctrl Pts',(-14.0470054900687,-5.44183891826343,
-851.273529411765));
#156037=CARTESIAN_POINT('Ctrl Pts',(-14.4273846475923,-4.10494485108124,
-852.767647058824));
#156038=CARTESIAN_POINT('Ctrl Pts',(-14.8077638051159,-2.76805078389906,
-854.261764705882));
#156039=CARTESIAN_POINT('Ctrl Pts',(-14.9360126444255,-1.38402539194953,
-855.755882352941));
#156040=CARTESIAN_POINT('Ctrl Pts',(-15.0642614837351,-9.22419980378748E-16,
-857.25));
#156041=CARTESIAN_POINT('Ctrl Pts',(-14.9360126444255,1.38402539194953,
-858.744117647059));
#156042=CARTESIAN_POINT('Ctrl Pts',(-14.8077638051159,2.76805078389906,
-860.238235294118));
#156043=CARTESIAN_POINT('Ctrl Pts',(-14.4273846475923,4.10494485108124,
-861.732352941176));
#156044=CARTESIAN_POINT('Ctrl Pts',(-14.0470054900687,5.44183891826343,
-863.226470588235));
#156045=CARTESIAN_POINT('Ctrl Pts',(-13.4274493703259,6.68607533664807,
-864.720588235294));
#156046=CARTESIAN_POINT('Ctrl Pts',(-12.8078932505832,7.93031175503273,
-866.214705882353));
#156047=CARTESIAN_POINT('Ctrl Pts',(-11.9702584092036,9.03951954568884,
-867.708823529412));
#156048=CARTESIAN_POINT('Ctrl Pts',(-11.132623567824,10.148727336345,-869.202941176471));
#156049=CARTESIAN_POINT('Ctrl Pts',(-10.1054346546984,11.0851337583099,
-870.697058823529));
#156050=CARTESIAN_POINT('Ctrl Pts',(-9.07824574157275,12.0215401802748,
-872.191176470589));
#156051=CARTESIAN_POINT('Ctrl Pts',(-7.89648244316034,12.7532570359442,
-873.685294117647));
#156052=CARTESIAN_POINT('Ctrl Pts',(-6.71471914474793,13.4849738916136,
-875.179411764706));
#156053=CARTESIAN_POINT('Ctrl Pts',(-5.41862499280729,13.9870834410653,
-876.673529411764));
#156054=CARTESIAN_POINT('Ctrl Pts',(-4.12253084086667,14.4891929905171,
-878.167647058823));
#156055=CARTESIAN_POINT('Ctrl Pts',(-2.75624276724856,14.7445964952585,
-879.661764705882));
#156056=CARTESIAN_POINT('Ctrl Pts',(-1.38995469363044,15.,-881.155882352941));
#156057=CARTESIAN_POINT('Ctrl Pts',(-1.83697019872103E-15,15.,-882.65));
#156058=CARTESIAN_POINT('Ctrl Pts',(1.38995469363045,15.,-884.144117647059));
#156059=CARTESIAN_POINT('Ctrl Pts',(2.75624276724855,14.7445964952585,-885.638235294118));
#156060=CARTESIAN_POINT('Ctrl Pts',(4.12253084086666,14.4891929905171,-887.132352941177));
#156061=CARTESIAN_POINT('Ctrl Pts',(5.4186249928073,13.9870834410653,-888.626470588235));
#156062=CARTESIAN_POINT('Ctrl Pts',(6.71471914474792,13.4849738916136,-890.120588235294));
#156063=CARTESIAN_POINT('Ctrl Pts',(7.89648244316034,12.7532570359442,-891.614705882353));
#156064=CARTESIAN_POINT('Ctrl Pts',(9.07824574157275,12.0215401802748,-893.108823529412));
#156065=CARTESIAN_POINT('Ctrl Pts',(10.1054346546984,11.0851337583099,-894.60294117647));
#156066=CARTESIAN_POINT('Ctrl Pts',(11.132623567824,10.148727336345,-896.09705882353));
#156067=CARTESIAN_POINT('Ctrl Pts',(11.9702584092036,9.03951954568885,-897.591176470588));
#156068=CARTESIAN_POINT('Ctrl Pts',(12.8078932505832,7.93031175503273,-899.085294117647));
#156069=CARTESIAN_POINT('Ctrl Pts',(13.4274493703259,6.68607533664807,-900.579411764706));
#156070=CARTESIAN_POINT('Ctrl Pts',(14.0470054900687,5.44183891826343,-902.073529411765));
#156071=CARTESIAN_POINT('Ctrl Pts',(14.4273846475923,4.10494485108125,-903.567647058824));
#156072=CARTESIAN_POINT('Ctrl Pts',(14.8077638051159,2.76805078389905,-905.061764705883));
#156073=CARTESIAN_POINT('Ctrl Pts',(14.9360126444255,1.38402539194953,-906.555882352941));
#156074=CARTESIAN_POINT('Ctrl Pts',(15.0642614837351,2.76725994113625E-15,
-908.05));
#156075=CARTESIAN_POINT('Ctrl Pts',(14.9360126444255,-1.38402539194952,
-909.544117647059));
#156076=CARTESIAN_POINT('Ctrl Pts',(14.8077638051159,-2.76805078389906,
-911.038235294118));
#156077=CARTESIAN_POINT('Ctrl Pts',(14.4273846475923,-4.10494485108124,
-912.532352941176));
#156078=CARTESIAN_POINT('Ctrl Pts',(14.0470054900687,-5.44183891826342,
-914.026470588235));
#156079=CARTESIAN_POINT('Ctrl Pts',(13.4274493703259,-6.68607533664808,
-915.520588235294));
#156080=CARTESIAN_POINT('Ctrl Pts',(12.8078932505832,-7.93031175503273,
-917.014705882353));
#156081=CARTESIAN_POINT('Ctrl Pts',(11.9702584092036,-9.03951954568884,
-918.508823529412));
#156082=CARTESIAN_POINT('Ctrl Pts',(11.132623567824,-10.148727336345,-920.002941176471));
#156083=CARTESIAN_POINT('Ctrl Pts',(10.1054346546984,-11.0851337583099,
-921.497058823529));
#156084=CARTESIAN_POINT('Ctrl Pts',(9.07824574157275,-12.0215401802748,
-922.991176470588));
#156085=CARTESIAN_POINT('Ctrl Pts',(7.89648244316034,-12.7532570359442,
-924.485294117647));
#156086=CARTESIAN_POINT('Ctrl Pts',(6.71471914474792,-13.4849738916136,
-925.979411764706));
#156087=CARTESIAN_POINT('Ctrl Pts',(5.4186249928073,-13.9870834410653,-927.473529411765));
#156088=CARTESIAN_POINT('Ctrl Pts',(4.12253084086667,-14.4891929905171,
-928.967647058823));
#156089=CARTESIAN_POINT('Ctrl Pts',(2.75624276724855,-14.7445964952585,
-930.461764705883));
#156090=CARTESIAN_POINT('Ctrl Pts',(1.38995469363045,-15.,-931.955882352941));
#156091=CARTESIAN_POINT('Ctrl Pts',(0.,-15.,-933.45));
#156092=CARTESIAN_POINT('Ctrl Pts',(-1.38995469363045,-15.,-934.944117647059));
#156093=CARTESIAN_POINT('Ctrl Pts',(-2.75624276724856,-14.7445964952585,
-936.438235294117));
#156094=CARTESIAN_POINT('Ctrl Pts',(-4.12253084086666,-14.4891929905171,
-937.932352941177));
#156095=CARTESIAN_POINT('Ctrl Pts',(-5.41862499280729,-13.9870834410653,
-939.426470588235));
#156096=CARTESIAN_POINT('Ctrl Pts',(-6.71471914474793,-13.4849738916136,
-940.920588235294));
#156097=CARTESIAN_POINT('Ctrl Pts',(-7.89648244316034,-12.7532570359442,
-942.414705882353));
#156098=CARTESIAN_POINT('Ctrl Pts',(-9.07824574157275,-12.0215401802748,
-943.908823529412));
#156099=CARTESIAN_POINT('Ctrl Pts',(-10.1054346546984,-11.0851337583099,
-945.402941176471));
#156100=CARTESIAN_POINT('Ctrl Pts',(-11.132623567824,-10.148727336345,-946.89705882353));
#156101=CARTESIAN_POINT('Ctrl Pts',(-11.9702584092036,-9.03951954568885,
-948.391176470588));
#156102=CARTESIAN_POINT('Ctrl Pts',(-12.8078932505832,-7.93031175503273,
-949.885294117647));
#156103=CARTESIAN_POINT('Ctrl Pts',(-13.4274493703259,-6.68607533664808,
-951.379411764706));
#156104=CARTESIAN_POINT('Ctrl Pts',(-14.0470054900687,-5.44183891826343,
-952.873529411765));
#156105=CARTESIAN_POINT('Ctrl Pts',(-14.4273846475923,-4.10494485108124,
-954.367647058824));
#156106=CARTESIAN_POINT('Ctrl Pts',(-14.8077638051159,-2.76805078389906,
-955.861764705882));
#156107=CARTESIAN_POINT('Ctrl Pts',(-14.9360126444255,-1.38402539194953,
-957.355882352941));
#156108=CARTESIAN_POINT('Ctrl Pts',(-15.0642614837351,-9.22419980378748E-16,
-958.85));
#156109=CARTESIAN_POINT('Ctrl Pts',(-14.9360126444255,1.38402539194953,
-960.344117647059));
#156110=CARTESIAN_POINT('Ctrl Pts',(-14.8077638051159,2.76805078389906,
-961.838235294118));
#156111=CARTESIAN_POINT('Ctrl Pts',(-14.4273846475923,4.10494485108124,
-963.332352941177));
#156112=CARTESIAN_POINT('Ctrl Pts',(-14.0470054900687,5.44183891826343,
-964.826470588235));
#156113=CARTESIAN_POINT('Ctrl Pts',(-13.4274493703259,6.68607533664807,
-966.320588235294));
#156114=CARTESIAN_POINT('Ctrl Pts',(-12.8078932505832,7.93031175503273,
-967.814705882353));
#156115=CARTESIAN_POINT('Ctrl Pts',(-11.9702584092036,9.03951954568884,
-969.308823529412));
#156116=CARTESIAN_POINT('Ctrl Pts',(-11.132623567824,10.148727336345,-970.80294117647));
#156117=CARTESIAN_POINT('Ctrl Pts',(-10.1054346546984,11.0851337583099,
-972.297058823529));
#156118=CARTESIAN_POINT('Ctrl Pts',(-9.07824574157275,12.0215401802748,
-973.791176470588));
#156119=CARTESIAN_POINT('Ctrl Pts',(-7.89648244316034,12.7532570359442,
-975.285294117647));
#156120=CARTESIAN_POINT('Ctrl Pts',(-6.71471914474793,13.4849738916136,
-976.779411764706));
#156121=CARTESIAN_POINT('Ctrl Pts',(-5.41862499280729,13.9870834410653,
-978.273529411765));
#156122=CARTESIAN_POINT('Ctrl Pts',(-4.12253084086667,14.4891929905171,
-979.767647058824));
#156123=CARTESIAN_POINT('Ctrl Pts',(-2.75624276724856,14.7445964952585,
-981.261764705882));
#156124=CARTESIAN_POINT('Ctrl Pts',(-1.38995469363044,15.,-982.755882352941));
#156125=CARTESIAN_POINT('Ctrl Pts',(-1.83697019872103E-15,15.,-984.25));
#156126=CARTESIAN_POINT('Ctrl Pts',(1.38995469363045,15.,-985.744117647059));
#156127=CARTESIAN_POINT('Ctrl Pts',(2.75624276724855,14.7445964952585,-987.238235294118));
#156128=CARTESIAN_POINT('Ctrl Pts',(4.12253084086666,14.4891929905171,-988.732352941177));
#156129=CARTESIAN_POINT('Ctrl Pts',(5.4186249928073,13.9870834410653,-990.226470588235));
#156130=CARTESIAN_POINT('Ctrl Pts',(6.71471914474792,13.4849738916136,-991.720588235294));
#156131=CARTESIAN_POINT('Ctrl Pts',(7.89648244316034,12.7532570359442,-993.214705882353));
#156132=CARTESIAN_POINT('Ctrl Pts',(9.07824574157275,12.0215401802748,-994.708823529412));
#156133=CARTESIAN_POINT('Ctrl Pts',(10.1054346546984,11.0851337583099,-996.202941176471));
#156134=CARTESIAN_POINT('Ctrl Pts',(11.132623567824,10.148727336345,-997.697058823529));
#156135=CARTESIAN_POINT('Ctrl Pts',(11.9702584092036,9.03951954568885,-999.191176470588));
#156136=CARTESIAN_POINT('Ctrl Pts',(12.8078932505832,7.93031175503273,-1000.68529411765));
#156137=CARTESIAN_POINT('Ctrl Pts',(13.4274493703259,6.68607533664807,-1002.17941176471));
#156138=CARTESIAN_POINT('Ctrl Pts',(14.0470054900687,5.44183891826343,-1003.67352941176));
#156139=CARTESIAN_POINT('Ctrl Pts',(14.4273846475923,4.10494485108125,-1005.16764705882));
#156140=CARTESIAN_POINT('Ctrl Pts',(14.8077638051159,2.76805078389905,-1006.66176470588));
#156141=CARTESIAN_POINT('Ctrl Pts',(14.9360126444255,1.38402539194953,-1008.15588235294));
#156142=CARTESIAN_POINT('Ctrl Pts',(15.0642614837351,2.76725994113625E-15,
-1009.65));
#156143=CARTESIAN_POINT('Ctrl Pts',(14.9360126444255,-1.38402539194952,
-1011.14411764706));
#156144=CARTESIAN_POINT('Ctrl Pts',(14.8077638051159,-2.76805078389906,
-1012.63823529412));
#156145=CARTESIAN_POINT('Ctrl Pts',(14.4273846475923,-4.10494485108124,
-1014.13235294118));
#156146=CARTESIAN_POINT('Ctrl Pts',(14.0470054900687,-5.44183891826342,
-1015.62647058824));
#156147=CARTESIAN_POINT('Ctrl Pts',(13.4274493703259,-6.68607533664808,
-1017.12058823529));
#156148=CARTESIAN_POINT('Ctrl Pts',(12.8078932505832,-7.93031175503273,
-1018.61470588235));
#156149=CARTESIAN_POINT('Ctrl Pts',(11.9702584092036,-9.03951954568884,
-1020.10882352941));
#156150=CARTESIAN_POINT('Ctrl Pts',(11.132623567824,-10.148727336345,-1021.60294117647));
#156151=CARTESIAN_POINT('Ctrl Pts',(10.1054346546984,-11.0851337583099,
-1023.09705882353));
#156152=CARTESIAN_POINT('Ctrl Pts',(9.07824574157275,-12.0215401802748,
-1024.59117647059));
#156153=CARTESIAN_POINT('Ctrl Pts',(7.89648244316034,-12.7532570359442,
-1026.08529411765));
#156154=CARTESIAN_POINT('Ctrl Pts',(6.71471914474792,-13.4849738916136,
-1027.57941176471));
#156155=CARTESIAN_POINT('Ctrl Pts',(5.4186249928073,-13.9870834410653,-1029.07352941176));
#156156=CARTESIAN_POINT('Ctrl Pts',(4.12253084086667,-14.4891929905171,
-1030.56764705882));
#156157=CARTESIAN_POINT('Ctrl Pts',(2.75624276724855,-14.7445964952585,
-1032.06176470588));
#156158=CARTESIAN_POINT('Ctrl Pts',(1.38995469363045,-15.,-1033.55588235294));
#156159=CARTESIAN_POINT('Ctrl Pts',(0.,-15.,-1035.05));
#156160=CARTESIAN_POINT('Ctrl Pts',(-1.38995469363045,-15.,-1036.54411764706));
#156161=CARTESIAN_POINT('Ctrl Pts',(-2.75624276724856,-14.7445964952585,
-1038.03823529412));
#156162=CARTESIAN_POINT('Ctrl Pts',(-4.12253084086666,-14.4891929905171,
-1039.53235294118));
#156163=CARTESIAN_POINT('Ctrl Pts',(-5.41862499280729,-13.9870834410653,
-1041.02647058824));
#156164=CARTESIAN_POINT('Ctrl Pts',(-6.71471914474793,-13.4849738916136,
-1042.52058823529));
#156165=CARTESIAN_POINT('Ctrl Pts',(-7.89648244316034,-12.7532570359442,
-1044.01470588235));
#156166=CARTESIAN_POINT('Ctrl Pts',(-9.07824574157275,-12.0215401802748,
-1045.50882352941));
#156167=CARTESIAN_POINT('Ctrl Pts',(-10.1054346546984,-11.0851337583099,
-1047.00294117647));
#156168=CARTESIAN_POINT('Ctrl Pts',(-11.132623567824,-10.148727336345,-1048.49705882353));
#156169=CARTESIAN_POINT('Ctrl Pts',(-11.9702584092036,-9.03951954568885,
-1049.99117647059));
#156170=CARTESIAN_POINT('Ctrl Pts',(-12.8078932505832,-7.93031175503273,
-1051.48529411765));
#156171=CARTESIAN_POINT('Ctrl Pts',(-13.4274493703259,-6.68607533664808,
-1052.97941176471));
#156172=CARTESIAN_POINT('Ctrl Pts',(-14.0470054900687,-5.44183891826343,
-1054.47352941176));
#156173=CARTESIAN_POINT('Ctrl Pts',(-14.4273846475923,-4.10494485108124,
-1055.96764705882));
#156174=CARTESIAN_POINT('Ctrl Pts',(-14.8077638051159,-2.76805078389906,
-1057.46176470588));
#156175=CARTESIAN_POINT('Ctrl Pts',(-14.9360126444255,-1.38402539194953,
-1058.95588235294));
#156176=CARTESIAN_POINT('Ctrl Pts',(-15.0642614837351,-9.22419980378748E-16,
-1060.45));
#156177=CARTESIAN_POINT('Ctrl Pts',(-14.9360126444255,1.38402539194953,
-1061.94411764706));
#156178=CARTESIAN_POINT('Ctrl Pts',(-14.8077638051159,2.76805078389906,
-1063.43823529412));
#156179=CARTESIAN_POINT('Ctrl Pts',(-14.4273846475923,4.10494485108124,
-1064.93235294118));
#156180=CARTESIAN_POINT('Ctrl Pts',(-14.0470054900687,5.44183891826343,
-1066.42647058824));
#156181=CARTESIAN_POINT('Ctrl Pts',(-13.4274493703259,6.68607533664807,
-1067.92058823529));
#156182=CARTESIAN_POINT('Ctrl Pts',(-12.8078932505832,7.93031175503273,
-1069.41470588235));
#156183=CARTESIAN_POINT('Ctrl Pts',(-11.9702584092036,9.03951954568884,
-1070.90882352941));
#156184=CARTESIAN_POINT('Ctrl Pts',(-11.132623567824,10.148727336345,-1072.40294117647));
#156185=CARTESIAN_POINT('Ctrl Pts',(-10.1054346546984,11.0851337583099,
-1073.89705882353));
#156186=CARTESIAN_POINT('Ctrl Pts',(-9.07824574157275,12.0215401802748,
-1075.39117647059));
#156187=CARTESIAN_POINT('Ctrl Pts',(-7.89648244316034,12.7532570359442,
-1076.88529411765));
#156188=CARTESIAN_POINT('Ctrl Pts',(-6.71471914474793,13.4849738916136,
-1078.37941176471));
#156189=CARTESIAN_POINT('Ctrl Pts',(-5.41862499280729,13.9870834410653,
-1079.87352941176));
#156190=CARTESIAN_POINT('Ctrl Pts',(-4.12253084086667,14.4891929905171,
-1081.36764705882));
#156191=CARTESIAN_POINT('Ctrl Pts',(-2.75624276724856,14.7445964952585,
-1082.86176470588));
#156192=CARTESIAN_POINT('Ctrl Pts',(-1.38995469363044,15.,-1084.35588235294));
#156193=CARTESIAN_POINT('Ctrl Pts',(-1.83697019872103E-15,15.,-1085.85));
#156194=CARTESIAN_POINT('Ctrl Pts',(1.38995469363045,15.,-1087.34411764706));
#156195=CARTESIAN_POINT('Ctrl Pts',(2.75624276724855,14.7445964952585,-1088.83823529412));
#156196=CARTESIAN_POINT('Ctrl Pts',(4.12253084086666,14.4891929905171,-1090.33235294118));
#156197=CARTESIAN_POINT('Ctrl Pts',(5.4186249928073,13.9870834410653,-1091.82647058824));
#156198=CARTESIAN_POINT('Ctrl Pts',(6.71471914474792,13.4849738916136,-1093.32058823529));
#156199=CARTESIAN_POINT('Ctrl Pts',(7.89648244316034,12.7532570359442,-1094.81470588235));
#156200=CARTESIAN_POINT('Ctrl Pts',(9.07824574157275,12.0215401802748,-1096.30882352941));
#156201=CARTESIAN_POINT('Ctrl Pts',(10.1054346546984,11.0851337583099,-1097.80294117647));
#156202=CARTESIAN_POINT('Ctrl Pts',(11.132623567824,10.148727336345,-1099.29705882353));
#156203=CARTESIAN_POINT('Ctrl Pts',(11.9702584092036,9.03951954568885,-1100.79117647059));
#156204=CARTESIAN_POINT('Ctrl Pts',(12.8078932505832,7.93031175503273,-1102.28529411765));
#156205=CARTESIAN_POINT('Ctrl Pts',(13.4274493703259,6.68607533664807,-1103.77941176471));
#156206=CARTESIAN_POINT('Ctrl Pts',(14.0470054900687,5.44183891826343,-1105.27352941176));
#156207=CARTESIAN_POINT('Ctrl Pts',(14.4273846475923,4.10494485108125,-1106.76764705882));
#156208=CARTESIAN_POINT('Ctrl Pts',(14.8077638051159,2.76805078389905,-1108.26176470588));
#156209=CARTESIAN_POINT('Ctrl Pts',(14.9360126444255,1.38402539194953,-1109.75588235294));
#156210=CARTESIAN_POINT('Ctrl Pts',(15.0642614837351,2.76725994113625E-15,
-1111.25));
#156211=CARTESIAN_POINT('Ctrl Pts',(14.9360126444255,-1.38402539194952,
-1112.74411764706));
#156212=CARTESIAN_POINT('Ctrl Pts',(14.8077638051159,-2.76805078389906,
-1114.23823529412));
#156213=CARTESIAN_POINT('Ctrl Pts',(14.4273846475923,-4.10494485108124,
-1115.73235294118));
#156214=CARTESIAN_POINT('Ctrl Pts',(14.0470054900687,-5.44183891826342,
-1117.22647058824));
#156215=CARTESIAN_POINT('Ctrl Pts',(13.4274493703259,-6.68607533664808,
-1118.72058823529));
#156216=CARTESIAN_POINT('Ctrl Pts',(12.8078932505832,-7.93031175503273,
-1120.21470588235));
#156217=CARTESIAN_POINT('Ctrl Pts',(11.9702584092036,-9.03951954568884,
-1121.70882352941));
#156218=CARTESIAN_POINT('Ctrl Pts',(11.132623567824,-10.148727336345,-1123.20294117647));
#156219=CARTESIAN_POINT('Ctrl Pts',(10.1054346546984,-11.0851337583099,
-1124.69705882353));
#156220=CARTESIAN_POINT('Ctrl Pts',(9.07824574157275,-12.0215401802748,
-1126.19117647059));
#156221=CARTESIAN_POINT('Ctrl Pts',(7.89648244316034,-12.7532570359442,
-1127.68529411765));
#156222=CARTESIAN_POINT('Ctrl Pts',(6.71471914474792,-13.4849738916136,
-1129.17941176471));
#156223=CARTESIAN_POINT('Ctrl Pts',(5.4186249928073,-13.9870834410653,-1130.67352941176));
#156224=CARTESIAN_POINT('Ctrl Pts',(4.12253084086667,-14.4891929905171,
-1132.16764705882));
#156225=CARTESIAN_POINT('Ctrl Pts',(2.75624276724855,-14.7445964952585,
-1133.66176470588));
#156226=CARTESIAN_POINT('Ctrl Pts',(1.38995469363045,-15.,-1135.15588235294));
#156227=CARTESIAN_POINT('Ctrl Pts',(0.,-15.,-1136.65));
#156228=CARTESIAN_POINT('Ctrl Pts',(-1.38995469363045,-15.,-1138.14411764706));
#156229=CARTESIAN_POINT('Ctrl Pts',(-2.75624276724856,-14.7445964952585,
-1139.63823529412));
#156230=CARTESIAN_POINT('Ctrl Pts',(-4.12253084086666,-14.4891929905171,
-1141.13235294118));
#156231=CARTESIAN_POINT('Ctrl Pts',(-5.41862499280729,-13.9870834410653,
-1142.62647058824));
#156232=CARTESIAN_POINT('Ctrl Pts',(-6.71471914474793,-13.4849738916136,
-1144.12058823529));
#156233=CARTESIAN_POINT('Ctrl Pts',(-7.89648244316034,-12.7532570359442,
-1145.61470588235));
#156234=CARTESIAN_POINT('Ctrl Pts',(-9.07824574157275,-12.0215401802748,
-1147.10882352941));
#156235=CARTESIAN_POINT('Ctrl Pts',(-10.1054346546984,-11.0851337583099,
-1148.60294117647));
#156236=CARTESIAN_POINT('Ctrl Pts',(-11.132623567824,-10.148727336345,-1150.09705882353));
#156237=CARTESIAN_POINT('Ctrl Pts',(-11.9702584092036,-9.03951954568885,
-1151.59117647059));
#156238=CARTESIAN_POINT('Ctrl Pts',(-12.8078932505832,-7.93031175503273,
-1153.08529411765));
#156239=CARTESIAN_POINT('Ctrl Pts',(-13.4274493703259,-6.68607533664808,
-1154.57941176471));
#156240=CARTESIAN_POINT('Ctrl Pts',(-14.0470054900687,-5.44183891826343,
-1156.07352941176));
#156241=CARTESIAN_POINT('Ctrl Pts',(-14.4273846475923,-4.10494485108124,
-1157.56764705882));
#156242=CARTESIAN_POINT('Ctrl Pts',(-14.8077638051159,-2.76805078389906,
-1159.06176470588));
#156243=CARTESIAN_POINT('Ctrl Pts',(-14.9360126444255,-1.38402539194953,
-1160.55588235294));
#156244=CARTESIAN_POINT('Ctrl Pts',(-15.0642614837351,-9.22419980378748E-16,
-1162.05));
#156245=CARTESIAN_POINT('Ctrl Pts',(-14.9360126444255,1.38402539194953,
-1163.54411764706));
#156246=CARTESIAN_POINT('Ctrl Pts',(-14.8077638051159,2.76805078389906,
-1165.03823529412));
#156247=CARTESIAN_POINT('Ctrl Pts',(-14.4273846475923,4.10494485108124,
-1166.53235294118));
#156248=CARTESIAN_POINT('Ctrl Pts',(-14.0470054900687,5.44183891826343,
-1168.02647058824));
#156249=CARTESIAN_POINT('Ctrl Pts',(-13.4274493703259,6.68607533664807,
-1169.52058823529));
#156250=CARTESIAN_POINT('Ctrl Pts',(-12.8078932505832,7.93031175503273,
-1171.01470588235));
#156251=CARTESIAN_POINT('Ctrl Pts',(-11.9702584092036,9.03951954568884,
-1172.50882352941));
#156252=CARTESIAN_POINT('Ctrl Pts',(-11.132623567824,10.148727336345,-1174.00294117647));
#156253=CARTESIAN_POINT('Ctrl Pts',(-10.1054346546984,11.0851337583099,
-1175.49705882353));
#156254=CARTESIAN_POINT('Ctrl Pts',(-9.07824574157275,12.0215401802748,
-1176.99117647059));
#156255=CARTESIAN_POINT('Ctrl Pts',(-7.89648244316034,12.7532570359442,
-1178.48529411765));
#156256=CARTESIAN_POINT('Ctrl Pts',(-6.71471914474793,13.4849738916136,
-1179.97941176471));
#156257=CARTESIAN_POINT('Ctrl Pts',(-5.41862499280729,13.9870834410653,
-1181.47352941176));
#156258=CARTESIAN_POINT('Ctrl Pts',(-4.12253084086667,14.4891929905171,
-1182.96764705882));
#156259=CARTESIAN_POINT('Ctrl Pts',(-2.75624276724856,14.7445964952585,
-1184.46176470588));
#156260=CARTESIAN_POINT('Ctrl Pts',(-1.38995469363044,15.,-1185.95588235294));
#156261=CARTESIAN_POINT('Ctrl Pts',(-1.83697019872103E-15,15.,-1187.45));
#156262=CARTESIAN_POINT('Ctrl Pts',(1.38995469363045,15.,-1188.94411764706));
#156263=CARTESIAN_POINT('Ctrl Pts',(2.75624276724855,14.7445964952585,-1190.43823529412));
#156264=CARTESIAN_POINT('Ctrl Pts',(4.12253084086666,14.4891929905171,-1191.93235294118));
#156265=CARTESIAN_POINT('Ctrl Pts',(5.4186249928073,13.9870834410653,-1193.42647058824));
#156266=CARTESIAN_POINT('Ctrl Pts',(6.71471914474792,13.4849738916136,-1194.92058823529));
#156267=CARTESIAN_POINT('Ctrl Pts',(7.89648244316034,12.7532570359442,-1196.41470588235));
#156268=CARTESIAN_POINT('Ctrl Pts',(9.07824574157275,12.0215401802748,-1197.90882352941));
#156269=CARTESIAN_POINT('Ctrl Pts',(10.1054346546984,11.0851337583099,-1199.40294117647));
#156270=CARTESIAN_POINT('Ctrl Pts',(11.132623567824,10.148727336345,-1200.89705882353));
#156271=CARTESIAN_POINT('Ctrl Pts',(11.9702584092036,9.03951954568885,-1202.39117647059));
#156272=CARTESIAN_POINT('Ctrl Pts',(12.8078932505832,7.93031175503273,-1203.88529411765));
#156273=CARTESIAN_POINT('Ctrl Pts',(13.4274493703259,6.68607533664807,-1205.37941176471));
#156274=CARTESIAN_POINT('Ctrl Pts',(14.0470054900687,5.44183891826343,-1206.87352941176));
#156275=CARTESIAN_POINT('Ctrl Pts',(14.4273846475923,4.10494485108125,-1208.36764705882));
#156276=CARTESIAN_POINT('Ctrl Pts',(14.8077638051159,2.76805078389905,-1209.86176470588));
#156277=CARTESIAN_POINT('Ctrl Pts',(14.9360126444255,1.38402539194953,-1211.35588235294));
#156278=CARTESIAN_POINT('Ctrl Pts',(15.0642614837351,2.76725994113625E-15,
-1212.85));
#156279=CARTESIAN_POINT('Ctrl Pts',(14.9360126444255,-1.38402539194952,
-1214.34411764706));
#156280=CARTESIAN_POINT('Ctrl Pts',(14.8077638051159,-2.76805078389906,
-1215.83823529412));
#156281=CARTESIAN_POINT('Ctrl Pts',(14.4273846475923,-4.10494485108124,
-1217.33235294118));
#156282=CARTESIAN_POINT('Ctrl Pts',(14.0470054900687,-5.44183891826342,
-1218.82647058824));
#156283=CARTESIAN_POINT('Ctrl Pts',(13.4274493703259,-6.68607533664808,
-1220.32058823529));
#156284=CARTESIAN_POINT('Ctrl Pts',(12.8078932505832,-7.93031175503273,
-1221.81470588235));
#156285=CARTESIAN_POINT('Ctrl Pts',(11.9702584092036,-9.03951954568884,
-1223.30882352941));
#156286=CARTESIAN_POINT('Ctrl Pts',(11.132623567824,-10.148727336345,-1224.80294117647));
#156287=CARTESIAN_POINT('Ctrl Pts',(10.1054346546984,-11.0851337583099,
-1226.29705882353));
#156288=CARTESIAN_POINT('Ctrl Pts',(9.07824574157275,-12.0215401802748,
-1227.79117647059));
#156289=CARTESIAN_POINT('Ctrl Pts',(7.89648244316034,-12.7532570359442,
-1229.28529411765));
#156290=CARTESIAN_POINT('Ctrl Pts',(6.71471914474792,-13.4849738916136,
-1230.77941176471));
#156291=CARTESIAN_POINT('Ctrl Pts',(5.4186249928073,-13.9870834410653,-1232.27352941176));
#156292=CARTESIAN_POINT('Ctrl Pts',(4.12253084086667,-14.4891929905171,
-1233.76764705882));
#156293=CARTESIAN_POINT('Ctrl Pts',(2.75624276724855,-14.7445964952585,
-1235.26176470588));
#156294=CARTESIAN_POINT('Ctrl Pts',(1.38995469363045,-15.,-1236.75588235294));
#156295=CARTESIAN_POINT('Ctrl Pts',(0.,-15.,-1238.25));
#156296=CARTESIAN_POINT('Ctrl Pts',(-1.38995469363045,-15.,-1239.74411764706));
#156297=CARTESIAN_POINT('Ctrl Pts',(-2.75624276724856,-14.7445964952585,
-1241.23823529412));
#156298=CARTESIAN_POINT('Ctrl Pts',(-4.12253084086666,-14.4891929905171,
-1242.73235294118));
#156299=CARTESIAN_POINT('Ctrl Pts',(-5.41862499280729,-13.9870834410653,
-1244.22647058824));
#156300=CARTESIAN_POINT('Ctrl Pts',(-6.71471914474793,-13.4849738916136,
-1245.72058823529));
#156301=CARTESIAN_POINT('Ctrl Pts',(-7.89648244316034,-12.7532570359442,
-1247.21470588235));
#156302=CARTESIAN_POINT('Ctrl Pts',(-9.07824574157275,-12.0215401802748,
-1248.70882352941));
#156303=CARTESIAN_POINT('Ctrl Pts',(-10.1054346546984,-11.0851337583099,
-1250.20294117647));
#156304=CARTESIAN_POINT('Ctrl Pts',(-11.132623567824,-10.148727336345,-1251.69705882353));
#156305=CARTESIAN_POINT('Ctrl Pts',(-11.9702584092036,-9.03951954568885,
-1253.19117647059));
#156306=CARTESIAN_POINT('Ctrl Pts',(-12.8078932505832,-7.93031175503273,
-1254.68529411765));
#156307=CARTESIAN_POINT('Ctrl Pts',(-13.4274493703259,-6.68607533664808,
-1256.17941176471));
#156308=CARTESIAN_POINT('Ctrl Pts',(-14.0470054900687,-5.44183891826343,
-1257.67352941176));
#156309=CARTESIAN_POINT('Ctrl Pts',(-14.4273846475923,-4.10494485108124,
-1259.16764705882));
#156310=CARTESIAN_POINT('Ctrl Pts',(-14.8077638051159,-2.76805078389906,
-1260.66176470588));
#156311=CARTESIAN_POINT('Ctrl Pts',(-14.9360126444255,-1.38402539194953,
-1262.15588235294));
#156312=CARTESIAN_POINT('Ctrl Pts',(-15.0642614837351,-9.22419980378748E-16,
-1263.65));
#156313=CARTESIAN_POINT('Ctrl Pts',(-14.9360126444255,1.38402539194953,
-1265.14411764706));
#156314=CARTESIAN_POINT('Ctrl Pts',(-14.8077638051159,2.76805078389906,
-1266.63823529412));
#156315=CARTESIAN_POINT('Ctrl Pts',(-14.4273846475923,4.10494485108124,
-1268.13235294118));
#156316=CARTESIAN_POINT('Ctrl Pts',(-14.0470054900687,5.44183891826343,
-1269.62647058824));
#156317=CARTESIAN_POINT('Ctrl Pts',(-13.4274493703259,6.68607533664807,
-1271.12058823529));
#156318=CARTESIAN_POINT('Ctrl Pts',(-12.8078932505832,7.93031175503273,
-1272.61470588235));
#156319=CARTESIAN_POINT('Ctrl Pts',(-11.9702584092036,9.03951954568884,
-1274.10882352941));
#156320=CARTESIAN_POINT('Ctrl Pts',(-11.132623567824,10.148727336345,-1275.60294117647));
#156321=CARTESIAN_POINT('Ctrl Pts',(-10.1054346546984,11.0851337583099,
-1277.09705882353));
#156322=CARTESIAN_POINT('Ctrl Pts',(-9.07824574157275,12.0215401802748,
-1278.59117647059));
#156323=CARTESIAN_POINT('Ctrl Pts',(-7.89648244316034,12.7532570359442,
-1280.08529411765));
#156324=CARTESIAN_POINT('Ctrl Pts',(-6.71471914474793,13.4849738916136,
-1281.57941176471));
#156325=CARTESIAN_POINT('Ctrl Pts',(-5.41862499280729,13.9870834410653,
-1283.07352941176));
#156326=CARTESIAN_POINT('Ctrl Pts',(-4.12253084086667,14.4891929905171,
-1284.56764705882));
#156327=CARTESIAN_POINT('Ctrl Pts',(-2.75624276724856,14.7445964952585,
-1286.06176470588));
#156328=CARTESIAN_POINT('Ctrl Pts',(-1.38995469363044,15.,-1287.55588235294));
#156329=CARTESIAN_POINT('Ctrl Pts',(-1.83697019872103E-15,15.,-1289.05));
#156330=CARTESIAN_POINT('Ctrl Pts',(1.38995469363045,15.,-1290.54411764706));
#156331=CARTESIAN_POINT('Ctrl Pts',(2.75624276724855,14.7445964952585,-1292.03823529412));
#156332=CARTESIAN_POINT('Ctrl Pts',(4.12253084086666,14.4891929905171,-1293.53235294118));
#156333=CARTESIAN_POINT('Ctrl Pts',(5.4186249928073,13.9870834410653,-1295.02647058824));
#156334=CARTESIAN_POINT('Ctrl Pts',(6.71471914474792,13.4849738916136,-1296.52058823529));
#156335=CARTESIAN_POINT('Ctrl Pts',(7.89648244316034,12.7532570359442,-1298.01470588235));
#156336=CARTESIAN_POINT('Ctrl Pts',(9.07824574157275,12.0215401802748,-1299.50882352941));
#156337=CARTESIAN_POINT('Ctrl Pts',(10.1054346546984,11.0851337583099,-1301.00294117647));
#156338=CARTESIAN_POINT('Ctrl Pts',(11.132623567824,10.148727336345,-1302.49705882353));
#156339=CARTESIAN_POINT('Ctrl Pts',(11.9702584092036,9.03951954568885,-1303.99117647059));
#156340=CARTESIAN_POINT('Ctrl Pts',(12.8078932505832,7.93031175503273,-1305.48529411765));
#156341=CARTESIAN_POINT('Ctrl Pts',(13.4274493703259,6.68607533664807,-1306.97941176471));
#156342=CARTESIAN_POINT('Ctrl Pts',(14.0470054900687,5.44183891826343,-1308.47352941176));
#156343=CARTESIAN_POINT('Ctrl Pts',(14.4273846475923,4.10494485108125,-1309.96764705882));
#156344=CARTESIAN_POINT('Ctrl Pts',(14.8077638051159,2.76805078389905,-1311.46176470588));
#156345=CARTESIAN_POINT('Ctrl Pts',(14.9360126444255,1.38402539194953,-1312.95588235294));
#156346=CARTESIAN_POINT('Ctrl Pts',(15.0642614837351,2.76725994113625E-15,
-1314.45));
#156347=CARTESIAN_POINT('Ctrl Pts',(14.9360126444255,-1.38402539194952,
-1315.94411764706));
#156348=CARTESIAN_POINT('Ctrl Pts',(14.8077638051159,-2.76805078389906,
-1317.43823529412));
#156349=CARTESIAN_POINT('Ctrl Pts',(14.4273846475923,-4.10494485108124,
-1318.93235294118));
#156350=CARTESIAN_POINT('Ctrl Pts',(14.0470054900687,-5.44183891826342,
-1320.42647058824));
#156351=CARTESIAN_POINT('Ctrl Pts',(13.4274493703259,-6.68607533664808,
-1321.92058823529));
#156352=CARTESIAN_POINT('Ctrl Pts',(12.8078932505832,-7.93031175503273,
-1323.41470588235));
#156353=CARTESIAN_POINT('Ctrl Pts',(11.9702584092036,-9.03951954568884,
-1324.90882352941));
#156354=CARTESIAN_POINT('Ctrl Pts',(11.132623567824,-10.148727336345,-1326.40294117647));
#156355=CARTESIAN_POINT('Ctrl Pts',(10.1054346546984,-11.0851337583099,
-1327.89705882353));
#156356=CARTESIAN_POINT('Ctrl Pts',(9.07824574157275,-12.0215401802748,
-1329.39117647059));
#156357=CARTESIAN_POINT('Ctrl Pts',(7.89648244316034,-12.7532570359442,
-1330.88529411765));
#156358=CARTESIAN_POINT('Ctrl Pts',(6.71471914474792,-13.4849738916136,
-1332.37941176471));
#156359=CARTESIAN_POINT('Ctrl Pts',(5.4186249928073,-13.9870834410653,-1333.87352941176));
#156360=CARTESIAN_POINT('Ctrl Pts',(4.12253084086667,-14.4891929905171,
-1335.36764705882));
#156361=CARTESIAN_POINT('Ctrl Pts',(2.75624276724855,-14.7445964952585,
-1336.86176470588));
#156362=CARTESIAN_POINT('Ctrl Pts',(1.38995469363045,-15.,-1338.35588235294));
#156363=CARTESIAN_POINT('Ctrl Pts',(0.,-15.,-1339.85));
#156364=CARTESIAN_POINT('Ctrl Pts',(-1.38995469363045,-15.,-1341.34411764706));
#156365=CARTESIAN_POINT('Ctrl Pts',(-2.75624276724856,-14.7445964952585,
-1342.83823529412));
#156366=CARTESIAN_POINT('Ctrl Pts',(-4.12253084086666,-14.4891929905171,
-1344.33235294118));
#156367=CARTESIAN_POINT('Ctrl Pts',(-5.41862499280729,-13.9870834410653,
-1345.82647058824));
#156368=CARTESIAN_POINT('Ctrl Pts',(-6.71471914474793,-13.4849738916136,
-1347.32058823529));
#156369=CARTESIAN_POINT('Ctrl Pts',(-7.89648244316034,-12.7532570359442,
-1348.81470588235));
#156370=CARTESIAN_POINT('Ctrl Pts',(-9.07824574157275,-12.0215401802748,
-1350.30882352941));
#156371=CARTESIAN_POINT('Ctrl Pts',(-10.1054346546984,-11.0851337583099,
-1351.80294117647));
#156372=CARTESIAN_POINT('Ctrl Pts',(-11.132623567824,-10.148727336345,-1353.29705882353));
#156373=CARTESIAN_POINT('Ctrl Pts',(-11.9702584092036,-9.03951954568885,
-1354.79117647059));
#156374=CARTESIAN_POINT('Ctrl Pts',(-12.8078932505832,-7.93031175503273,
-1356.28529411765));
#156375=CARTESIAN_POINT('Ctrl Pts',(-13.4274493703259,-6.68607533664808,
-1357.77941176471));
#156376=CARTESIAN_POINT('Ctrl Pts',(-14.0470054900687,-5.44183891826343,
-1359.27352941176));
#156377=CARTESIAN_POINT('Ctrl Pts',(-14.4273846475923,-4.10494485108124,
-1360.76764705882));
#156378=CARTESIAN_POINT('Ctrl Pts',(-14.8077638051159,-2.76805078389906,
-1362.26176470588));
#156379=CARTESIAN_POINT('Ctrl Pts',(-14.9360126444255,-1.38402539194953,
-1363.75588235294));
#156380=CARTESIAN_POINT('Ctrl Pts',(-15.0642614837351,-9.22419980378748E-16,
-1365.25));
#156381=CARTESIAN_POINT('Ctrl Pts',(-14.9360126444255,1.38402539194953,
-1366.74411764706));
#156382=CARTESIAN_POINT('Ctrl Pts',(-14.8077638051159,2.76805078389906,
-1368.23823529412));
#156383=CARTESIAN_POINT('Ctrl Pts',(-14.4273846475923,4.10494485108124,
-1369.73235294118));
#156384=CARTESIAN_POINT('Ctrl Pts',(-14.0470054900687,5.44183891826343,
-1371.22647058824));
#156385=CARTESIAN_POINT('Ctrl Pts',(-13.4274493703259,6.68607533664807,
-1372.72058823529));
#156386=CARTESIAN_POINT('Ctrl Pts',(-12.8078932505832,7.93031175503273,
-1374.21470588235));
#156387=CARTESIAN_POINT('Ctrl Pts',(-11.9702584092036,9.03951954568884,
-1375.70882352941));
#156388=CARTESIAN_POINT('Ctrl Pts',(-11.132623567824,10.148727336345,-1377.20294117647));
#156389=CARTESIAN_POINT('Ctrl Pts',(-10.1054346546984,11.0851337583099,
-1378.69705882353));
#156390=CARTESIAN_POINT('Ctrl Pts',(-9.07824574157275,12.0215401802748,
-1380.19117647059));
#156391=CARTESIAN_POINT('Ctrl Pts',(-7.89648244316034,12.7532570359442,
-1381.68529411765));
#156392=CARTESIAN_POINT('Ctrl Pts',(-6.71471914474793,13.4849738916136,
-1383.17941176471));
#156393=CARTESIAN_POINT('Ctrl Pts',(-5.41862499280729,13.9870834410653,
-1384.67352941176));
#156394=CARTESIAN_POINT('Ctrl Pts',(-4.12253084086667,14.4891929905171,
-1386.16764705882));
#156395=CARTESIAN_POINT('Ctrl Pts',(-2.75624276724856,14.7445964952585,
-1387.66176470588));
#156396=CARTESIAN_POINT('Ctrl Pts',(-1.38995469363044,15.,-1389.15588235294));
#156397=CARTESIAN_POINT('Ctrl Pts',(-1.83697019872103E-15,15.,-1390.65));
#156398=CARTESIAN_POINT('Ctrl Pts',(1.38995469363045,15.,-1392.14411764706));
#156399=CARTESIAN_POINT('Ctrl Pts',(2.75624276724855,14.7445964952585,-1393.63823529412));
#156400=CARTESIAN_POINT('Ctrl Pts',(4.12253084086666,14.4891929905171,-1395.13235294118));
#156401=CARTESIAN_POINT('Ctrl Pts',(5.4186249928073,13.9870834410653,-1396.62647058824));
#156402=CARTESIAN_POINT('Ctrl Pts',(6.71471914474792,13.4849738916136,-1398.12058823529));
#156403=CARTESIAN_POINT('Ctrl Pts',(7.89648244316034,12.7532570359442,-1399.61470588235));
#156404=CARTESIAN_POINT('Ctrl Pts',(9.07824574157275,12.0215401802748,-1401.10882352941));
#156405=CARTESIAN_POINT('Ctrl Pts',(10.1054346546984,11.0851337583099,-1402.60294117647));
#156406=CARTESIAN_POINT('Ctrl Pts',(11.132623567824,10.148727336345,-1404.09705882353));
#156407=CARTESIAN_POINT('Ctrl Pts',(11.9702584092036,9.03951954568885,-1405.59117647059));
#156408=CARTESIAN_POINT('Ctrl Pts',(12.8078932505832,7.93031175503273,-1407.08529411765));
#156409=CARTESIAN_POINT('Ctrl Pts',(13.4274493703259,6.68607533664807,-1408.57941176471));
#156410=CARTESIAN_POINT('Ctrl Pts',(14.0470054900687,5.44183891826343,-1410.07352941176));
#156411=CARTESIAN_POINT('Ctrl Pts',(14.4273846475923,4.10494485108125,-1411.56764705882));
#156412=CARTESIAN_POINT('Ctrl Pts',(14.8077638051159,2.76805078389905,-1413.06176470588));
#156413=CARTESIAN_POINT('Ctrl Pts',(14.9360126444255,1.38402539194953,-1414.55588235294));
#156414=CARTESIAN_POINT('Ctrl Pts',(15.0642614837351,2.76725994113625E-15,
-1416.05));
#156415=CARTESIAN_POINT('Ctrl Pts',(14.9360126444255,-1.38402539194952,
-1417.54411764706));
#156416=CARTESIAN_POINT('Ctrl Pts',(14.8077638051159,-2.76805078389906,
-1419.03823529412));
#156417=CARTESIAN_POINT('Ctrl Pts',(14.4273846475923,-4.10494485108124,
-1420.53235294118));
#156418=CARTESIAN_POINT('Ctrl Pts',(14.0470054900687,-5.44183891826342,
-1422.02647058824));
#156419=CARTESIAN_POINT('Ctrl Pts',(13.4274493703259,-6.68607533664808,
-1423.52058823529));
#156420=CARTESIAN_POINT('Ctrl Pts',(12.8078932505832,-7.93031175503273,
-1425.01470588235));
#156421=CARTESIAN_POINT('Ctrl Pts',(11.9702584092036,-9.03951954568884,
-1426.50882352941));
#156422=CARTESIAN_POINT('Ctrl Pts',(11.132623567824,-10.148727336345,-1428.00294117647));
#156423=CARTESIAN_POINT('Ctrl Pts',(10.1054346546984,-11.0851337583099,
-1429.49705882353));
#156424=CARTESIAN_POINT('Ctrl Pts',(9.07824574157275,-12.0215401802748,
-1430.99117647059));
#156425=CARTESIAN_POINT('Ctrl Pts',(7.89648244316034,-12.7532570359442,
-1432.48529411765));
#156426=CARTESIAN_POINT('Ctrl Pts',(6.71471914474792,-13.4849738916136,
-1433.97941176471));
#156427=CARTESIAN_POINT('Ctrl Pts',(5.4186249928073,-13.9870834410653,-1435.47352941176));
#156428=CARTESIAN_POINT('Ctrl Pts',(4.12253084086667,-14.4891929905171,
-1436.96764705882));
#156429=CARTESIAN_POINT('Ctrl Pts',(2.75624276724855,-14.7445964952585,
-1438.46176470588));
#156430=CARTESIAN_POINT('Ctrl Pts',(1.38995469363045,-15.,-1439.95588235294));
#156431=CARTESIAN_POINT('Ctrl Pts',(0.,-15.,-1441.45));
#156432=CARTESIAN_POINT('Ctrl Pts',(-1.38995469363045,-15.,-1442.94411764706));
#156433=CARTESIAN_POINT('Ctrl Pts',(-2.75624276724856,-14.7445964952585,
-1444.43823529412));
#156434=CARTESIAN_POINT('Ctrl Pts',(-4.12253084086666,-14.4891929905171,
-1445.93235294118));
#156435=CARTESIAN_POINT('Ctrl Pts',(-5.41862499280729,-13.9870834410653,
-1447.42647058824));
#156436=CARTESIAN_POINT('Ctrl Pts',(-6.71471914474793,-13.4849738916136,
-1448.92058823529));
#156437=CARTESIAN_POINT('Ctrl Pts',(-7.89648244316034,-12.7532570359442,
-1450.41470588235));
#156438=CARTESIAN_POINT('Ctrl Pts',(-9.07824574157275,-12.0215401802748,
-1451.90882352941));
#156439=CARTESIAN_POINT('Ctrl Pts',(-10.1054346546984,-11.0851337583099,
-1453.40294117647));
#156440=CARTESIAN_POINT('Ctrl Pts',(-11.132623567824,-10.148727336345,-1454.89705882353));
#156441=CARTESIAN_POINT('Ctrl Pts',(-11.9702584092036,-9.03951954568885,
-1456.39117647059));
#156442=CARTESIAN_POINT('Ctrl Pts',(-12.8078932505832,-7.93031175503273,
-1457.88529411765));
#156443=CARTESIAN_POINT('Ctrl Pts',(-13.4274493703259,-6.68607533664808,
-1459.37941176471));
#156444=CARTESIAN_POINT('Ctrl Pts',(-14.0470054900687,-5.44183891826343,
-1460.87352941176));
#156445=CARTESIAN_POINT('Ctrl Pts',(-14.4273846475923,-4.10494485108124,
-1462.36764705882));
#156446=CARTESIAN_POINT('Ctrl Pts',(-14.8077638051159,-2.76805078389906,
-1463.86176470588));
#156447=CARTESIAN_POINT('Ctrl Pts',(-14.9360126444255,-1.38402539194953,
-1465.35588235294));
#156448=CARTESIAN_POINT('Ctrl Pts',(-15.0642614837351,-9.22419980378748E-16,
-1466.85));
#156449=CARTESIAN_POINT('Ctrl Pts',(-14.9360126444255,1.38402539194953,
-1468.34411764706));
#156450=CARTESIAN_POINT('Ctrl Pts',(-14.8077638051159,2.76805078389906,
-1469.83823529412));
#156451=CARTESIAN_POINT('Ctrl Pts',(-14.4273846475923,4.10494485108124,
-1471.33235294118));
#156452=CARTESIAN_POINT('Ctrl Pts',(-14.0470054900687,5.44183891826343,
-1472.82647058824));
#156453=CARTESIAN_POINT('Ctrl Pts',(-13.4274493703259,6.68607533664807,
-1474.32058823529));
#156454=CARTESIAN_POINT('Ctrl Pts',(-12.8078932505832,7.93031175503273,
-1475.81470588235));
#156455=CARTESIAN_POINT('Ctrl Pts',(-11.9702584092036,9.03951954568884,
-1477.30882352941));
#156456=CARTESIAN_POINT('Ctrl Pts',(-11.132623567824,10.148727336345,-1478.80294117647));
#156457=CARTESIAN_POINT('Ctrl Pts',(-10.1054346546984,11.0851337583099,
-1480.29705882353));
#156458=CARTESIAN_POINT('Ctrl Pts',(-9.07824574157275,12.0215401802748,
-1481.79117647059));
#156459=CARTESIAN_POINT('Ctrl Pts',(-7.89648244316034,12.7532570359442,
-1483.28529411765));
#156460=CARTESIAN_POINT('Ctrl Pts',(-6.71471914474793,13.4849738916136,
-1484.77941176471));
#156461=CARTESIAN_POINT('Ctrl Pts',(-5.41862499280729,13.9870834410653,
-1486.27352941176));
#156462=CARTESIAN_POINT('Ctrl Pts',(-4.12253084086667,14.4891929905171,
-1487.76764705882));
#156463=CARTESIAN_POINT('Ctrl Pts',(-2.75624276724856,14.7445964952585,
-1489.26176470588));
#156464=CARTESIAN_POINT('Ctrl Pts',(-1.38995469363044,15.,-1490.75588235294));
#156465=CARTESIAN_POINT('Ctrl Pts',(-1.83697019872103E-15,15.,-1492.25));
#156466=CARTESIAN_POINT('Ctrl Pts',(1.38995469363045,15.,-1493.74411764706));
#156467=CARTESIAN_POINT('Ctrl Pts',(2.75624276724855,14.7445964952585,-1495.23823529412));
#156468=CARTESIAN_POINT('Ctrl Pts',(4.12253084086666,14.4891929905171,-1496.73235294118));
#156469=CARTESIAN_POINT('Ctrl Pts',(5.4186249928073,13.9870834410653,-1498.22647058824));
#156470=CARTESIAN_POINT('Ctrl Pts',(6.26766581794969,13.6581632730821,-1499.20523195215));
#156471=CARTESIAN_POINT('Ctrl Pts',(7.0706872023049,13.228959992651,-1500.18777724595));
#156472=CARTESIAN_POINT('Ctrl Pts',(19.3695474754025,6.6553975974033,-1515.23617759469));
#156473=CARTESIAN_POINT('Ctrl Pts',(31.6684077485001,0.0818352021555714,
-1530.28457794343));
#156474=CARTESIAN_POINT('Ctrl Pts',(0.,-18.048,1504.95));
#156475=CARTESIAN_POINT('Ctrl Pts',(-1.67239348737615,-18.048,1503.45588235294));
#156476=CARTESIAN_POINT('Ctrl Pts',(-3.31631129755346,-17.7406985030951,
1501.96176470588));
#156477=CARTESIAN_POINT('Ctrl Pts',(-4.96022910773077,-17.4333970061901,
1500.46764705882));
#156478=CARTESIAN_POINT('Ctrl Pts',(-6.51968959134574,-16.8292587962898,
1498.97352941176));
#156479=CARTESIAN_POINT('Ctrl Pts',(-8.07915007496071,-16.2251205863895,
1497.47941176471));
#156480=CARTESIAN_POINT('Ctrl Pts',(-9.50104767561052,-15.3447188656481,
1495.98529411765));
#156481=CARTESIAN_POINT('Ctrl Pts',(-10.9229452762603,-14.4643171449067,
1494.49117647059));
#156482=CARTESIAN_POINT('Ctrl Pts',(-12.1588589765331,-13.3376329379985,
1492.99705882353));
#156483=CARTESIAN_POINT('Ctrl Pts',(-13.3947726768058,-12.2109487310903,
1491.50294117647));
#156484=CARTESIAN_POINT('Ctrl Pts',(-14.4026149179538,-10.8763499173728,
1490.00882352941));
#156485=CARTESIAN_POINT('Ctrl Pts',(-15.4104571591017,-9.54175110365538,
1488.51470588235));
#156486=CARTESIAN_POINT('Ctrl Pts',(-16.1559070823762,-8.04468584505497,
1487.02058823529));
#156487=CARTESIAN_POINT('Ctrl Pts',(-16.9013570056506,-6.54762058645456,
1485.52647058824));
#156488=CARTESIAN_POINT('Ctrl Pts',(-17.3590292079831,-4.93906964482095,
1484.03235294118));
#156489=CARTESIAN_POINT('Ctrl Pts',(-17.8167014103155,-3.33051870318735,
1482.53823529412));
#156490=CARTESIAN_POINT('Ctrl Pts',(-17.9710104137728,-1.66525935159368,
1481.04411764706));
#156491=CARTESIAN_POINT('Ctrl Pts',(-18.1253194172301,-1.10985572039171E-15,
1479.55));
#156492=CARTESIAN_POINT('Ctrl Pts',(-17.9710104137728,1.66525935159367,
1478.05588235294));
#156493=CARTESIAN_POINT('Ctrl Pts',(-17.8167014103155,3.33051870318735,
1476.56176470588));
#156494=CARTESIAN_POINT('Ctrl Pts',(-17.3590292079831,4.93906964482096,
1475.06764705882));
#156495=CARTESIAN_POINT('Ctrl Pts',(-16.9013570056506,6.54762058645456,
1473.57352941176));
#156496=CARTESIAN_POINT('Ctrl Pts',(-16.1559070823762,8.04468584505497,
1472.07941176471));
#156497=CARTESIAN_POINT('Ctrl Pts',(-15.4104571591017,9.54175110365538,
1470.58529411765));
#156498=CARTESIAN_POINT('Ctrl Pts',(-14.4026149179538,10.8763499173728,
1469.09117647059));
#156499=CARTESIAN_POINT('Ctrl Pts',(-13.3947726768058,12.2109487310903,
1467.59705882353));
#156500=CARTESIAN_POINT('Ctrl Pts',(-12.1588589765331,13.3376329379985,
1466.10294117647));
#156501=CARTESIAN_POINT('Ctrl Pts',(-10.9229452762603,14.4643171449067,
1464.60882352941));
#156502=CARTESIAN_POINT('Ctrl Pts',(-9.50104767561052,15.3447188656481,
1463.11470588235));
#156503=CARTESIAN_POINT('Ctrl Pts',(-8.07915007496071,16.2251205863895,
1461.62058823529));
#156504=CARTESIAN_POINT('Ctrl Pts',(-6.51968959134574,16.8292587962898,
1460.12647058824));
#156505=CARTESIAN_POINT('Ctrl Pts',(-4.96022910773078,17.4333970061901,
1458.63235294118));
#156506=CARTESIAN_POINT('Ctrl Pts',(-3.31631129755346,17.7406985030951,
1457.13823529412));
#156507=CARTESIAN_POINT('Ctrl Pts',(-1.67239348737615,18.048,1455.64411764706));
#156508=CARTESIAN_POINT('Ctrl Pts',(-2.21024254310115E-15,18.048,1454.15));
#156509=CARTESIAN_POINT('Ctrl Pts',(1.67239348737616,18.048,1452.65588235294));
#156510=CARTESIAN_POINT('Ctrl Pts',(3.31631129755346,17.7406985030951,1451.16176470588));
#156511=CARTESIAN_POINT('Ctrl Pts',(4.96022910773077,17.4333970061901,1449.66764705882));
#156512=CARTESIAN_POINT('Ctrl Pts',(6.51968959134575,16.8292587962898,1448.17352941177));
#156513=CARTESIAN_POINT('Ctrl Pts',(8.07915007496071,16.2251205863895,1446.67941176471));
#156514=CARTESIAN_POINT('Ctrl Pts',(9.50104767561053,15.3447188656481,1445.18529411765));
#156515=CARTESIAN_POINT('Ctrl Pts',(10.9229452762603,14.4643171449067,1443.69117647059));
#156516=CARTESIAN_POINT('Ctrl Pts',(12.1588589765331,13.3376329379985,1442.19705882353));
#156517=CARTESIAN_POINT('Ctrl Pts',(13.3947726768058,12.2109487310903,1440.70294117647));
#156518=CARTESIAN_POINT('Ctrl Pts',(14.4026149179538,10.8763499173728,1439.20882352941));
#156519=CARTESIAN_POINT('Ctrl Pts',(15.4104571591017,9.54175110365538,1437.71470588235));
#156520=CARTESIAN_POINT('Ctrl Pts',(16.1559070823762,8.04468584505496,1436.22058823529));
#156521=CARTESIAN_POINT('Ctrl Pts',(16.9013570056506,6.54762058645456,1434.72647058824));
#156522=CARTESIAN_POINT('Ctrl Pts',(17.3590292079831,4.93906964482096,1433.23235294118));
#156523=CARTESIAN_POINT('Ctrl Pts',(17.8167014103155,3.33051870318735,1431.73823529412));
#156524=CARTESIAN_POINT('Ctrl Pts',(17.9710104137728,1.66525935159367,1430.24411764706));
#156525=CARTESIAN_POINT('Ctrl Pts',(18.1253194172301,3.32956716117513E-15,
1428.75));
#156526=CARTESIAN_POINT('Ctrl Pts',(17.9710104137728,-1.66525935159367,
1427.25588235294));
#156527=CARTESIAN_POINT('Ctrl Pts',(17.8167014103155,-3.33051870318736,
1425.76176470588));
#156528=CARTESIAN_POINT('Ctrl Pts',(17.3590292079831,-4.93906964482095,
1424.26764705882));
#156529=CARTESIAN_POINT('Ctrl Pts',(16.9013570056506,-6.54762058645456,
1422.77352941176));
#156530=CARTESIAN_POINT('Ctrl Pts',(16.1559070823762,-8.04468584505497,
1421.27941176471));
#156531=CARTESIAN_POINT('Ctrl Pts',(15.4104571591017,-9.54175110365538,
1419.78529411765));
#156532=CARTESIAN_POINT('Ctrl Pts',(14.4026149179538,-10.8763499173728,
1418.29117647059));
#156533=CARTESIAN_POINT('Ctrl Pts',(13.3947726768058,-12.2109487310903,
1416.79705882353));
#156534=CARTESIAN_POINT('Ctrl Pts',(12.1588589765331,-13.3376329379985,
1415.30294117647));
#156535=CARTESIAN_POINT('Ctrl Pts',(10.9229452762603,-14.4643171449067,
1413.80882352941));
#156536=CARTESIAN_POINT('Ctrl Pts',(9.50104767561053,-15.3447188656481,
1412.31470588235));
#156537=CARTESIAN_POINT('Ctrl Pts',(8.07915007496071,-16.2251205863895,
1410.82058823529));
#156538=CARTESIAN_POINT('Ctrl Pts',(6.51968959134574,-16.8292587962898,
1409.32647058824));
#156539=CARTESIAN_POINT('Ctrl Pts',(4.96022910773078,-17.4333970061901,
1407.83235294118));
#156540=CARTESIAN_POINT('Ctrl Pts',(3.31631129755346,-17.7406985030951,
1406.33823529412));
#156541=CARTESIAN_POINT('Ctrl Pts',(1.67239348737615,-18.048,1404.84411764706));
#156542=CARTESIAN_POINT('Ctrl Pts',(0.,-18.048,1403.35));
#156543=CARTESIAN_POINT('Ctrl Pts',(-1.67239348737615,-18.048,1401.85588235294));
#156544=CARTESIAN_POINT('Ctrl Pts',(-3.31631129755346,-17.7406985030951,
1400.36176470588));
#156545=CARTESIAN_POINT('Ctrl Pts',(-4.96022910773077,-17.4333970061901,
1398.86764705882));
#156546=CARTESIAN_POINT('Ctrl Pts',(-6.51968959134574,-16.8292587962898,
1397.37352941176));
#156547=CARTESIAN_POINT('Ctrl Pts',(-8.07915007496071,-16.2251205863895,
1395.87941176471));
#156548=CARTESIAN_POINT('Ctrl Pts',(-9.50104767561052,-15.3447188656481,
1394.38529411765));
#156549=CARTESIAN_POINT('Ctrl Pts',(-10.9229452762603,-14.4643171449067,
1392.89117647059));
#156550=CARTESIAN_POINT('Ctrl Pts',(-12.1588589765331,-13.3376329379985,
1391.39705882353));
#156551=CARTESIAN_POINT('Ctrl Pts',(-13.3947726768058,-12.2109487310903,
1389.90294117647));
#156552=CARTESIAN_POINT('Ctrl Pts',(-14.4026149179538,-10.8763499173728,
1388.40882352941));
#156553=CARTESIAN_POINT('Ctrl Pts',(-15.4104571591017,-9.54175110365538,
1386.91470588235));
#156554=CARTESIAN_POINT('Ctrl Pts',(-16.1559070823762,-8.04468584505497,
1385.42058823529));
#156555=CARTESIAN_POINT('Ctrl Pts',(-16.9013570056506,-6.54762058645456,
1383.92647058824));
#156556=CARTESIAN_POINT('Ctrl Pts',(-17.3590292079831,-4.93906964482095,
1382.43235294118));
#156557=CARTESIAN_POINT('Ctrl Pts',(-17.8167014103155,-3.33051870318735,
1380.93823529412));
#156558=CARTESIAN_POINT('Ctrl Pts',(-17.9710104137728,-1.66525935159368,
1379.44411764706));
#156559=CARTESIAN_POINT('Ctrl Pts',(-18.1253194172301,-1.10985572039171E-15,
1377.95));
#156560=CARTESIAN_POINT('Ctrl Pts',(-17.9710104137728,1.66525935159367,
1376.45588235294));
#156561=CARTESIAN_POINT('Ctrl Pts',(-17.8167014103155,3.33051870318735,
1374.96176470588));
#156562=CARTESIAN_POINT('Ctrl Pts',(-17.3590292079831,4.93906964482096,
1373.46764705882));
#156563=CARTESIAN_POINT('Ctrl Pts',(-16.9013570056506,6.54762058645456,
1371.97352941176));
#156564=CARTESIAN_POINT('Ctrl Pts',(-16.1559070823762,8.04468584505497,
1370.47941176471));
#156565=CARTESIAN_POINT('Ctrl Pts',(-15.4104571591017,9.54175110365538,
1368.98529411765));
#156566=CARTESIAN_POINT('Ctrl Pts',(-14.4026149179538,10.8763499173728,
1367.49117647059));
#156567=CARTESIAN_POINT('Ctrl Pts',(-13.3947726768058,12.2109487310903,
1365.99705882353));
#156568=CARTESIAN_POINT('Ctrl Pts',(-12.1588589765331,13.3376329379985,
1364.50294117647));
#156569=CARTESIAN_POINT('Ctrl Pts',(-10.9229452762603,14.4643171449067,
1363.00882352941));
#156570=CARTESIAN_POINT('Ctrl Pts',(-9.50104767561052,15.3447188656481,
1361.51470588235));
#156571=CARTESIAN_POINT('Ctrl Pts',(-8.07915007496071,16.2251205863895,
1360.02058823529));
#156572=CARTESIAN_POINT('Ctrl Pts',(-6.51968959134574,16.8292587962898,
1358.52647058824));
#156573=CARTESIAN_POINT('Ctrl Pts',(-4.96022910773078,17.4333970061901,
1357.03235294118));
#156574=CARTESIAN_POINT('Ctrl Pts',(-3.31631129755346,17.7406985030951,
1355.53823529412));
#156575=CARTESIAN_POINT('Ctrl Pts',(-1.67239348737615,18.048,1354.04411764706));
#156576=CARTESIAN_POINT('Ctrl Pts',(-2.21024254310115E-15,18.048,1352.55));
#156577=CARTESIAN_POINT('Ctrl Pts',(1.67239348737616,18.048,1351.05588235294));
#156578=CARTESIAN_POINT('Ctrl Pts',(3.31631129755346,17.7406985030951,1349.56176470588));
#156579=CARTESIAN_POINT('Ctrl Pts',(4.96022910773077,17.4333970061901,1348.06764705882));
#156580=CARTESIAN_POINT('Ctrl Pts',(6.51968959134575,16.8292587962898,1346.57352941176));
#156581=CARTESIAN_POINT('Ctrl Pts',(8.07915007496071,16.2251205863895,1345.07941176471));
#156582=CARTESIAN_POINT('Ctrl Pts',(9.50104767561053,15.3447188656481,1343.58529411765));
#156583=CARTESIAN_POINT('Ctrl Pts',(10.9229452762603,14.4643171449067,1342.09117647059));
#156584=CARTESIAN_POINT('Ctrl Pts',(12.1588589765331,13.3376329379985,1340.59705882353));
#156585=CARTESIAN_POINT('Ctrl Pts',(13.3947726768058,12.2109487310903,1339.10294117647));
#156586=CARTESIAN_POINT('Ctrl Pts',(14.4026149179538,10.8763499173728,1337.60882352941));
#156587=CARTESIAN_POINT('Ctrl Pts',(15.4104571591017,9.54175110365538,1336.11470588235));
#156588=CARTESIAN_POINT('Ctrl Pts',(16.1559070823762,8.04468584505496,1334.62058823529));
#156589=CARTESIAN_POINT('Ctrl Pts',(16.9013570056506,6.54762058645456,1333.12647058824));
#156590=CARTESIAN_POINT('Ctrl Pts',(17.3590292079831,4.93906964482096,1331.63235294118));
#156591=CARTESIAN_POINT('Ctrl Pts',(17.8167014103155,3.33051870318735,1330.13823529412));
#156592=CARTESIAN_POINT('Ctrl Pts',(17.9710104137728,1.66525935159367,1328.64411764706));
#156593=CARTESIAN_POINT('Ctrl Pts',(18.1253194172301,3.32956716117513E-15,
1327.15));
#156594=CARTESIAN_POINT('Ctrl Pts',(17.9710104137728,-1.66525935159367,
1325.65588235294));
#156595=CARTESIAN_POINT('Ctrl Pts',(17.8167014103155,-3.33051870318736,
1324.16176470588));
#156596=CARTESIAN_POINT('Ctrl Pts',(17.3590292079831,-4.93906964482095,
1322.66764705882));
#156597=CARTESIAN_POINT('Ctrl Pts',(16.9013570056506,-6.54762058645456,
1321.17352941176));
#156598=CARTESIAN_POINT('Ctrl Pts',(16.1559070823762,-8.04468584505497,
1319.67941176471));
#156599=CARTESIAN_POINT('Ctrl Pts',(15.4104571591017,-9.54175110365538,
1318.18529411765));
#156600=CARTESIAN_POINT('Ctrl Pts',(14.4026149179538,-10.8763499173728,
1316.69117647059));
#156601=CARTESIAN_POINT('Ctrl Pts',(13.3947726768058,-12.2109487310903,
1315.19705882353));
#156602=CARTESIAN_POINT('Ctrl Pts',(12.1588589765331,-13.3376329379985,
1313.70294117647));
#156603=CARTESIAN_POINT('Ctrl Pts',(10.9229452762603,-14.4643171449067,
1312.20882352941));
#156604=CARTESIAN_POINT('Ctrl Pts',(9.50104767561053,-15.3447188656481,
1310.71470588235));
#156605=CARTESIAN_POINT('Ctrl Pts',(8.07915007496071,-16.2251205863895,
1309.22058823529));
#156606=CARTESIAN_POINT('Ctrl Pts',(6.51968959134574,-16.8292587962898,
1307.72647058824));
#156607=CARTESIAN_POINT('Ctrl Pts',(4.96022910773078,-17.4333970061901,
1306.23235294118));
#156608=CARTESIAN_POINT('Ctrl Pts',(3.31631129755346,-17.7406985030951,
1304.73823529412));
#156609=CARTESIAN_POINT('Ctrl Pts',(1.67239348737615,-18.048,1303.24411764706));
#156610=CARTESIAN_POINT('Ctrl Pts',(0.,-18.048,1301.75));
#156611=CARTESIAN_POINT('Ctrl Pts',(-1.67239348737615,-18.048,1300.25588235294));
#156612=CARTESIAN_POINT('Ctrl Pts',(-3.31631129755346,-17.7406985030951,
1298.76176470588));
#156613=CARTESIAN_POINT('Ctrl Pts',(-4.96022910773077,-17.4333970061901,
1297.26764705882));
#156614=CARTESIAN_POINT('Ctrl Pts',(-6.51968959134574,-16.8292587962898,
1295.77352941176));
#156615=CARTESIAN_POINT('Ctrl Pts',(-8.07915007496071,-16.2251205863895,
1294.27941176471));
#156616=CARTESIAN_POINT('Ctrl Pts',(-9.50104767561052,-15.3447188656481,
1292.78529411765));
#156617=CARTESIAN_POINT('Ctrl Pts',(-10.9229452762603,-14.4643171449067,
1291.29117647059));
#156618=CARTESIAN_POINT('Ctrl Pts',(-12.1588589765331,-13.3376329379985,
1289.79705882353));
#156619=CARTESIAN_POINT('Ctrl Pts',(-13.3947726768058,-12.2109487310903,
1288.30294117647));
#156620=CARTESIAN_POINT('Ctrl Pts',(-14.4026149179538,-10.8763499173728,
1286.80882352941));
#156621=CARTESIAN_POINT('Ctrl Pts',(-15.4104571591017,-9.54175110365538,
1285.31470588235));
#156622=CARTESIAN_POINT('Ctrl Pts',(-16.1559070823762,-8.04468584505497,
1283.82058823529));
#156623=CARTESIAN_POINT('Ctrl Pts',(-16.9013570056506,-6.54762058645456,
1282.32647058824));
#156624=CARTESIAN_POINT('Ctrl Pts',(-17.3590292079831,-4.93906964482095,
1280.83235294118));
#156625=CARTESIAN_POINT('Ctrl Pts',(-17.8167014103155,-3.33051870318735,
1279.33823529412));
#156626=CARTESIAN_POINT('Ctrl Pts',(-17.9710104137728,-1.66525935159368,
1277.84411764706));
#156627=CARTESIAN_POINT('Ctrl Pts',(-18.1253194172301,-1.10985572039171E-15,
1276.35));
#156628=CARTESIAN_POINT('Ctrl Pts',(-17.9710104137728,1.66525935159367,
1274.85588235294));
#156629=CARTESIAN_POINT('Ctrl Pts',(-17.8167014103155,3.33051870318735,
1273.36176470588));
#156630=CARTESIAN_POINT('Ctrl Pts',(-17.3590292079831,4.93906964482096,
1271.86764705882));
#156631=CARTESIAN_POINT('Ctrl Pts',(-16.9013570056506,6.54762058645456,
1270.37352941176));
#156632=CARTESIAN_POINT('Ctrl Pts',(-16.1559070823762,8.04468584505497,
1268.87941176471));
#156633=CARTESIAN_POINT('Ctrl Pts',(-15.4104571591017,9.54175110365538,
1267.38529411765));
#156634=CARTESIAN_POINT('Ctrl Pts',(-14.4026149179538,10.8763499173728,
1265.89117647059));
#156635=CARTESIAN_POINT('Ctrl Pts',(-13.3947726768058,12.2109487310903,
1264.39705882353));
#156636=CARTESIAN_POINT('Ctrl Pts',(-12.1588589765331,13.3376329379985,
1262.90294117647));
#156637=CARTESIAN_POINT('Ctrl Pts',(-10.9229452762603,14.4643171449067,
1261.40882352941));
#156638=CARTESIAN_POINT('Ctrl Pts',(-9.50104767561052,15.3447188656481,
1259.91470588235));
#156639=CARTESIAN_POINT('Ctrl Pts',(-8.07915007496071,16.2251205863895,
1258.42058823529));
#156640=CARTESIAN_POINT('Ctrl Pts',(-6.51968959134574,16.8292587962898,
1256.92647058824));
#156641=CARTESIAN_POINT('Ctrl Pts',(-4.96022910773078,17.4333970061901,
1255.43235294118));
#156642=CARTESIAN_POINT('Ctrl Pts',(-3.31631129755346,17.7406985030951,
1253.93823529412));
#156643=CARTESIAN_POINT('Ctrl Pts',(-1.67239348737615,18.048,1252.44411764706));
#156644=CARTESIAN_POINT('Ctrl Pts',(-2.21024254310115E-15,18.048,1250.95));
#156645=CARTESIAN_POINT('Ctrl Pts',(1.67239348737616,18.048,1249.45588235294));
#156646=CARTESIAN_POINT('Ctrl Pts',(3.31631129755346,17.7406985030951,1247.96176470588));
#156647=CARTESIAN_POINT('Ctrl Pts',(4.96022910773077,17.4333970061901,1246.46764705882));
#156648=CARTESIAN_POINT('Ctrl Pts',(6.51968959134575,16.8292587962898,1244.97352941176));
#156649=CARTESIAN_POINT('Ctrl Pts',(8.07915007496071,16.2251205863895,1243.47941176471));
#156650=CARTESIAN_POINT('Ctrl Pts',(9.50104767561053,15.3447188656481,1241.98529411765));
#156651=CARTESIAN_POINT('Ctrl Pts',(10.9229452762603,14.4643171449067,1240.49117647059));
#156652=CARTESIAN_POINT('Ctrl Pts',(12.1588589765331,13.3376329379985,1238.99705882353));
#156653=CARTESIAN_POINT('Ctrl Pts',(13.3947726768058,12.2109487310903,1237.50294117647));
#156654=CARTESIAN_POINT('Ctrl Pts',(14.4026149179538,10.8763499173728,1236.00882352941));
#156655=CARTESIAN_POINT('Ctrl Pts',(15.4104571591017,9.54175110365538,1234.51470588235));
#156656=CARTESIAN_POINT('Ctrl Pts',(16.1559070823762,8.04468584505496,1233.02058823529));
#156657=CARTESIAN_POINT('Ctrl Pts',(16.9013570056506,6.54762058645456,1231.52647058824));
#156658=CARTESIAN_POINT('Ctrl Pts',(17.3590292079831,4.93906964482096,1230.03235294118));
#156659=CARTESIAN_POINT('Ctrl Pts',(17.8167014103155,3.33051870318735,1228.53823529412));
#156660=CARTESIAN_POINT('Ctrl Pts',(17.9710104137728,1.66525935159367,1227.04411764706));
#156661=CARTESIAN_POINT('Ctrl Pts',(18.1253194172301,3.32956716117513E-15,
1225.55));
#156662=CARTESIAN_POINT('Ctrl Pts',(17.9710104137728,-1.66525935159367,
1224.05588235294));
#156663=CARTESIAN_POINT('Ctrl Pts',(17.8167014103155,-3.33051870318736,
1222.56176470588));
#156664=CARTESIAN_POINT('Ctrl Pts',(17.3590292079831,-4.93906964482095,
1221.06764705882));
#156665=CARTESIAN_POINT('Ctrl Pts',(16.9013570056506,-6.54762058645456,
1219.57352941176));
#156666=CARTESIAN_POINT('Ctrl Pts',(16.1559070823762,-8.04468584505497,
1218.07941176471));
#156667=CARTESIAN_POINT('Ctrl Pts',(15.4104571591017,-9.54175110365538,
1216.58529411765));
#156668=CARTESIAN_POINT('Ctrl Pts',(14.4026149179538,-10.8763499173728,
1215.09117647059));
#156669=CARTESIAN_POINT('Ctrl Pts',(13.3947726768058,-12.2109487310903,
1213.59705882353));
#156670=CARTESIAN_POINT('Ctrl Pts',(12.1588589765331,-13.3376329379985,
1212.10294117647));
#156671=CARTESIAN_POINT('Ctrl Pts',(10.9229452762603,-14.4643171449067,
1210.60882352941));
#156672=CARTESIAN_POINT('Ctrl Pts',(9.50104767561053,-15.3447188656481,
1209.11470588235));
#156673=CARTESIAN_POINT('Ctrl Pts',(8.07915007496071,-16.2251205863895,
1207.62058823529));
#156674=CARTESIAN_POINT('Ctrl Pts',(6.51968959134574,-16.8292587962898,
1206.12647058824));
#156675=CARTESIAN_POINT('Ctrl Pts',(4.96022910773078,-17.4333970061901,
1204.63235294118));
#156676=CARTESIAN_POINT('Ctrl Pts',(3.31631129755346,-17.7406985030951,
1203.13823529412));
#156677=CARTESIAN_POINT('Ctrl Pts',(1.67239348737615,-18.048,1201.64411764706));
#156678=CARTESIAN_POINT('Ctrl Pts',(0.,-18.048,1200.15));
#156679=CARTESIAN_POINT('Ctrl Pts',(-1.67239348737615,-18.048,1198.65588235294));
#156680=CARTESIAN_POINT('Ctrl Pts',(-3.31631129755346,-17.7406985030951,
1197.16176470588));
#156681=CARTESIAN_POINT('Ctrl Pts',(-4.96022910773077,-17.4333970061901,
1195.66764705882));
#156682=CARTESIAN_POINT('Ctrl Pts',(-6.51968959134574,-16.8292587962898,
1194.17352941176));
#156683=CARTESIAN_POINT('Ctrl Pts',(-8.07915007496071,-16.2251205863895,
1192.67941176471));
#156684=CARTESIAN_POINT('Ctrl Pts',(-9.50104767561052,-15.3447188656481,
1191.18529411765));
#156685=CARTESIAN_POINT('Ctrl Pts',(-10.9229452762603,-14.4643171449067,
1189.69117647059));
#156686=CARTESIAN_POINT('Ctrl Pts',(-12.1588589765331,-13.3376329379985,
1188.19705882353));
#156687=CARTESIAN_POINT('Ctrl Pts',(-13.3947726768058,-12.2109487310903,
1186.70294117647));
#156688=CARTESIAN_POINT('Ctrl Pts',(-14.4026149179538,-10.8763499173728,
1185.20882352941));
#156689=CARTESIAN_POINT('Ctrl Pts',(-15.4104571591017,-9.54175110365538,
1183.71470588235));
#156690=CARTESIAN_POINT('Ctrl Pts',(-16.1559070823762,-8.04468584505497,
1182.22058823529));
#156691=CARTESIAN_POINT('Ctrl Pts',(-16.9013570056506,-6.54762058645456,
1180.72647058824));
#156692=CARTESIAN_POINT('Ctrl Pts',(-17.3590292079831,-4.93906964482095,
1179.23235294118));
#156693=CARTESIAN_POINT('Ctrl Pts',(-17.8167014103155,-3.33051870318735,
1177.73823529412));
#156694=CARTESIAN_POINT('Ctrl Pts',(-17.9710104137728,-1.66525935159368,
1176.24411764706));
#156695=CARTESIAN_POINT('Ctrl Pts',(-18.1253194172301,-1.10985572039171E-15,
1174.75));
#156696=CARTESIAN_POINT('Ctrl Pts',(-17.9710104137728,1.66525935159367,
1173.25588235294));
#156697=CARTESIAN_POINT('Ctrl Pts',(-17.8167014103155,3.33051870318735,
1171.76176470588));
#156698=CARTESIAN_POINT('Ctrl Pts',(-17.3590292079831,4.93906964482096,
1170.26764705882));
#156699=CARTESIAN_POINT('Ctrl Pts',(-16.9013570056506,6.54762058645456,
1168.77352941176));
#156700=CARTESIAN_POINT('Ctrl Pts',(-16.1559070823762,8.04468584505497,
1167.27941176471));
#156701=CARTESIAN_POINT('Ctrl Pts',(-15.4104571591017,9.54175110365538,
1165.78529411765));
#156702=CARTESIAN_POINT('Ctrl Pts',(-14.4026149179538,10.8763499173728,
1164.29117647059));
#156703=CARTESIAN_POINT('Ctrl Pts',(-13.3947726768058,12.2109487310903,
1162.79705882353));
#156704=CARTESIAN_POINT('Ctrl Pts',(-12.1588589765331,13.3376329379985,
1161.30294117647));
#156705=CARTESIAN_POINT('Ctrl Pts',(-10.9229452762603,14.4643171449067,
1159.80882352941));
#156706=CARTESIAN_POINT('Ctrl Pts',(-9.50104767561052,15.3447188656481,
1158.31470588235));
#156707=CARTESIAN_POINT('Ctrl Pts',(-8.07915007496071,16.2251205863895,
1156.82058823529));
#156708=CARTESIAN_POINT('Ctrl Pts',(-6.51968959134574,16.8292587962898,
1155.32647058824));
#156709=CARTESIAN_POINT('Ctrl Pts',(-4.96022910773078,17.4333970061901,
1153.83235294118));
#156710=CARTESIAN_POINT('Ctrl Pts',(-3.31631129755346,17.7406985030951,
1152.33823529412));
#156711=CARTESIAN_POINT('Ctrl Pts',(-1.67239348737615,18.048,1150.84411764706));
#156712=CARTESIAN_POINT('Ctrl Pts',(-2.21024254310115E-15,18.048,1149.35));
#156713=CARTESIAN_POINT('Ctrl Pts',(1.67239348737616,18.048,1147.85588235294));
#156714=CARTESIAN_POINT('Ctrl Pts',(3.31631129755346,17.7406985030951,1146.36176470588));
#156715=CARTESIAN_POINT('Ctrl Pts',(4.96022910773077,17.4333970061901,1144.86764705882));
#156716=CARTESIAN_POINT('Ctrl Pts',(6.51968959134575,16.8292587962898,1143.37352941176));
#156717=CARTESIAN_POINT('Ctrl Pts',(8.07915007496071,16.2251205863895,1141.87941176471));
#156718=CARTESIAN_POINT('Ctrl Pts',(9.50104767561053,15.3447188656481,1140.38529411765));
#156719=CARTESIAN_POINT('Ctrl Pts',(10.9229452762603,14.4643171449067,1138.89117647059));
#156720=CARTESIAN_POINT('Ctrl Pts',(12.1588589765331,13.3376329379985,1137.39705882353));
#156721=CARTESIAN_POINT('Ctrl Pts',(13.3947726768058,12.2109487310903,1135.90294117647));
#156722=CARTESIAN_POINT('Ctrl Pts',(14.4026149179538,10.8763499173728,1134.40882352941));
#156723=CARTESIAN_POINT('Ctrl Pts',(15.4104571591017,9.54175110365538,1132.91470588235));
#156724=CARTESIAN_POINT('Ctrl Pts',(16.1559070823762,8.04468584505496,1131.42058823529));
#156725=CARTESIAN_POINT('Ctrl Pts',(16.9013570056506,6.54762058645456,1129.92647058824));
#156726=CARTESIAN_POINT('Ctrl Pts',(17.3590292079831,4.93906964482096,1128.43235294118));
#156727=CARTESIAN_POINT('Ctrl Pts',(17.8167014103155,3.33051870318735,1126.93823529412));
#156728=CARTESIAN_POINT('Ctrl Pts',(17.9710104137728,1.66525935159367,1125.44411764706));
#156729=CARTESIAN_POINT('Ctrl Pts',(18.1253194172301,3.32956716117513E-15,
1123.95));
#156730=CARTESIAN_POINT('Ctrl Pts',(17.9710104137728,-1.66525935159367,
1122.45588235294));
#156731=CARTESIAN_POINT('Ctrl Pts',(17.8167014103155,-3.33051870318736,
1120.96176470588));
#156732=CARTESIAN_POINT('Ctrl Pts',(17.3590292079831,-4.93906964482095,
1119.46764705882));
#156733=CARTESIAN_POINT('Ctrl Pts',(16.9013570056506,-6.54762058645456,
1117.97352941176));
#156734=CARTESIAN_POINT('Ctrl Pts',(16.1559070823762,-8.04468584505497,
1116.47941176471));
#156735=CARTESIAN_POINT('Ctrl Pts',(15.4104571591017,-9.54175110365538,
1114.98529411765));
#156736=CARTESIAN_POINT('Ctrl Pts',(14.4026149179538,-10.8763499173728,
1113.49117647059));
#156737=CARTESIAN_POINT('Ctrl Pts',(13.3947726768058,-12.2109487310903,
1111.99705882353));
#156738=CARTESIAN_POINT('Ctrl Pts',(12.1588589765331,-13.3376329379985,
1110.50294117647));
#156739=CARTESIAN_POINT('Ctrl Pts',(10.9229452762603,-14.4643171449067,
1109.00882352941));
#156740=CARTESIAN_POINT('Ctrl Pts',(9.50104767561053,-15.3447188656481,
1107.51470588235));
#156741=CARTESIAN_POINT('Ctrl Pts',(8.07915007496071,-16.2251205863895,
1106.02058823529));
#156742=CARTESIAN_POINT('Ctrl Pts',(6.51968959134574,-16.8292587962898,
1104.52647058824));
#156743=CARTESIAN_POINT('Ctrl Pts',(4.96022910773078,-17.4333970061901,
1103.03235294118));
#156744=CARTESIAN_POINT('Ctrl Pts',(3.31631129755346,-17.7406985030951,
1101.53823529412));
#156745=CARTESIAN_POINT('Ctrl Pts',(1.67239348737615,-18.048,1100.04411764706));
#156746=CARTESIAN_POINT('Ctrl Pts',(0.,-18.048,1098.55));
#156747=CARTESIAN_POINT('Ctrl Pts',(-1.67239348737615,-18.048,1097.05588235294));
#156748=CARTESIAN_POINT('Ctrl Pts',(-3.31631129755346,-17.7406985030951,
1095.56176470588));
#156749=CARTESIAN_POINT('Ctrl Pts',(-4.96022910773077,-17.4333970061901,
1094.06764705882));
#156750=CARTESIAN_POINT('Ctrl Pts',(-6.51968959134574,-16.8292587962898,
1092.57352941176));
#156751=CARTESIAN_POINT('Ctrl Pts',(-8.07915007496071,-16.2251205863895,
1091.07941176471));
#156752=CARTESIAN_POINT('Ctrl Pts',(-9.50104767561052,-15.3447188656481,
1089.58529411765));
#156753=CARTESIAN_POINT('Ctrl Pts',(-10.9229452762603,-14.4643171449067,
1088.09117647059));
#156754=CARTESIAN_POINT('Ctrl Pts',(-12.1588589765331,-13.3376329379985,
1086.59705882353));
#156755=CARTESIAN_POINT('Ctrl Pts',(-13.3947726768058,-12.2109487310903,
1085.10294117647));
#156756=CARTESIAN_POINT('Ctrl Pts',(-14.4026149179538,-10.8763499173728,
1083.60882352941));
#156757=CARTESIAN_POINT('Ctrl Pts',(-15.4104571591017,-9.54175110365538,
1082.11470588235));
#156758=CARTESIAN_POINT('Ctrl Pts',(-16.1559070823762,-8.04468584505497,
1080.62058823529));
#156759=CARTESIAN_POINT('Ctrl Pts',(-16.9013570056506,-6.54762058645456,
1079.12647058824));
#156760=CARTESIAN_POINT('Ctrl Pts',(-17.3590292079831,-4.93906964482095,
1077.63235294118));
#156761=CARTESIAN_POINT('Ctrl Pts',(-17.8167014103155,-3.33051870318735,
1076.13823529412));
#156762=CARTESIAN_POINT('Ctrl Pts',(-17.9710104137728,-1.66525935159368,
1074.64411764706));
#156763=CARTESIAN_POINT('Ctrl Pts',(-18.1253194172301,-1.10985572039171E-15,
1073.15));
#156764=CARTESIAN_POINT('Ctrl Pts',(-17.9710104137728,1.66525935159367,
1071.65588235294));
#156765=CARTESIAN_POINT('Ctrl Pts',(-17.8167014103155,3.33051870318735,
1070.16176470588));
#156766=CARTESIAN_POINT('Ctrl Pts',(-17.3590292079831,4.93906964482096,
1068.66764705882));
#156767=CARTESIAN_POINT('Ctrl Pts',(-16.9013570056506,6.54762058645456,
1067.17352941176));
#156768=CARTESIAN_POINT('Ctrl Pts',(-16.1559070823762,8.04468584505497,
1065.67941176471));
#156769=CARTESIAN_POINT('Ctrl Pts',(-15.4104571591017,9.54175110365538,
1064.18529411765));
#156770=CARTESIAN_POINT('Ctrl Pts',(-14.4026149179538,10.8763499173728,
1062.69117647059));
#156771=CARTESIAN_POINT('Ctrl Pts',(-13.3947726768058,12.2109487310903,
1061.19705882353));
#156772=CARTESIAN_POINT('Ctrl Pts',(-12.1588589765331,13.3376329379985,
1059.70294117647));
#156773=CARTESIAN_POINT('Ctrl Pts',(-10.9229452762603,14.4643171449067,
1058.20882352941));
#156774=CARTESIAN_POINT('Ctrl Pts',(-9.50104767561052,15.3447188656481,
1056.71470588235));
#156775=CARTESIAN_POINT('Ctrl Pts',(-8.07915007496071,16.2251205863895,
1055.22058823529));
#156776=CARTESIAN_POINT('Ctrl Pts',(-6.51968959134574,16.8292587962898,
1053.72647058824));
#156777=CARTESIAN_POINT('Ctrl Pts',(-4.96022910773078,17.4333970061901,
1052.23235294118));
#156778=CARTESIAN_POINT('Ctrl Pts',(-3.31631129755346,17.7406985030951,
1050.73823529412));
#156779=CARTESIAN_POINT('Ctrl Pts',(-1.67239348737615,18.048,1049.24411764706));
#156780=CARTESIAN_POINT('Ctrl Pts',(-2.21024254310115E-15,18.048,1047.75));
#156781=CARTESIAN_POINT('Ctrl Pts',(1.67239348737616,18.048,1046.25588235294));
#156782=CARTESIAN_POINT('Ctrl Pts',(3.31631129755346,17.7406985030951,1044.76176470588));
#156783=CARTESIAN_POINT('Ctrl Pts',(4.96022910773077,17.4333970061901,1043.26764705882));
#156784=CARTESIAN_POINT('Ctrl Pts',(6.51968959134575,16.8292587962898,1041.77352941176));
#156785=CARTESIAN_POINT('Ctrl Pts',(8.07915007496071,16.2251205863895,1040.27941176471));
#156786=CARTESIAN_POINT('Ctrl Pts',(9.50104767561053,15.3447188656481,1038.78529411765));
#156787=CARTESIAN_POINT('Ctrl Pts',(10.9229452762603,14.4643171449067,1037.29117647059));
#156788=CARTESIAN_POINT('Ctrl Pts',(12.1588589765331,13.3376329379985,1035.79705882353));
#156789=CARTESIAN_POINT('Ctrl Pts',(13.3947726768058,12.2109487310903,1034.30294117647));
#156790=CARTESIAN_POINT('Ctrl Pts',(14.4026149179538,10.8763499173728,1032.80882352941));
#156791=CARTESIAN_POINT('Ctrl Pts',(15.4104571591017,9.54175110365538,1031.31470588235));
#156792=CARTESIAN_POINT('Ctrl Pts',(16.1559070823762,8.04468584505496,1029.82058823529));
#156793=CARTESIAN_POINT('Ctrl Pts',(16.9013570056506,6.54762058645456,1028.32647058824));
#156794=CARTESIAN_POINT('Ctrl Pts',(17.3590292079831,4.93906964482096,1026.83235294118));
#156795=CARTESIAN_POINT('Ctrl Pts',(17.8167014103155,3.33051870318735,1025.33823529412));
#156796=CARTESIAN_POINT('Ctrl Pts',(17.9710104137728,1.66525935159367,1023.84411764706));
#156797=CARTESIAN_POINT('Ctrl Pts',(18.1253194172301,3.32956716117513E-15,
1022.35));
#156798=CARTESIAN_POINT('Ctrl Pts',(17.9710104137728,-1.66525935159367,
1020.85588235294));
#156799=CARTESIAN_POINT('Ctrl Pts',(17.8167014103155,-3.33051870318736,
1019.36176470588));
#156800=CARTESIAN_POINT('Ctrl Pts',(17.3590292079831,-4.93906964482095,
1017.86764705882));
#156801=CARTESIAN_POINT('Ctrl Pts',(16.9013570056506,-6.54762058645456,
1016.37352941176));
#156802=CARTESIAN_POINT('Ctrl Pts',(16.1559070823762,-8.04468584505497,
1014.87941176471));
#156803=CARTESIAN_POINT('Ctrl Pts',(15.4104571591017,-9.54175110365538,
1013.38529411765));
#156804=CARTESIAN_POINT('Ctrl Pts',(14.4026149179538,-10.8763499173728,
1011.89117647059));
#156805=CARTESIAN_POINT('Ctrl Pts',(13.3947726768058,-12.2109487310903,
1010.39705882353));
#156806=CARTESIAN_POINT('Ctrl Pts',(12.1588589765331,-13.3376329379985,
1008.90294117647));
#156807=CARTESIAN_POINT('Ctrl Pts',(10.9229452762603,-14.4643171449067,
1007.40882352941));
#156808=CARTESIAN_POINT('Ctrl Pts',(9.50104767561053,-15.3447188656481,
1005.91470588235));
#156809=CARTESIAN_POINT('Ctrl Pts',(8.07915007496071,-16.2251205863895,
1004.42058823529));
#156810=CARTESIAN_POINT('Ctrl Pts',(6.51968959134574,-16.8292587962898,
1002.92647058824));
#156811=CARTESIAN_POINT('Ctrl Pts',(4.96022910773078,-17.4333970061901,
1001.43235294118));
#156812=CARTESIAN_POINT('Ctrl Pts',(3.31631129755346,-17.7406985030951,
999.938235294118));
#156813=CARTESIAN_POINT('Ctrl Pts',(1.67239348737615,-18.048,998.444117647059));
#156814=CARTESIAN_POINT('Ctrl Pts',(0.,-18.048,996.95));
#156815=CARTESIAN_POINT('Ctrl Pts',(-1.67239348737615,-18.048,995.455882352941));
#156816=CARTESIAN_POINT('Ctrl Pts',(-3.31631129755346,-17.7406985030951,
993.961764705882));
#156817=CARTESIAN_POINT('Ctrl Pts',(-4.96022910773077,-17.4333970061901,
992.467647058824));
#156818=CARTESIAN_POINT('Ctrl Pts',(-6.51968959134574,-16.8292587962898,
990.973529411765));
#156819=CARTESIAN_POINT('Ctrl Pts',(-8.07915007496071,-16.2251205863895,
989.479411764706));
#156820=CARTESIAN_POINT('Ctrl Pts',(-9.50104767561052,-15.3447188656481,
987.985294117647));
#156821=CARTESIAN_POINT('Ctrl Pts',(-10.9229452762603,-14.4643171449067,
986.491176470588));
#156822=CARTESIAN_POINT('Ctrl Pts',(-12.1588589765331,-13.3376329379985,
984.997058823529));
#156823=CARTESIAN_POINT('Ctrl Pts',(-13.3947726768058,-12.2109487310903,
983.502941176471));
#156824=CARTESIAN_POINT('Ctrl Pts',(-14.4026149179538,-10.8763499173728,
982.008823529412));
#156825=CARTESIAN_POINT('Ctrl Pts',(-15.4104571591017,-9.54175110365538,
980.514705882353));
#156826=CARTESIAN_POINT('Ctrl Pts',(-16.1559070823762,-8.04468584505497,
979.020588235294));
#156827=CARTESIAN_POINT('Ctrl Pts',(-16.9013570056506,-6.54762058645456,
977.526470588235));
#156828=CARTESIAN_POINT('Ctrl Pts',(-17.3590292079831,-4.93906964482095,
976.032352941177));
#156829=CARTESIAN_POINT('Ctrl Pts',(-17.8167014103155,-3.33051870318735,
974.538235294118));
#156830=CARTESIAN_POINT('Ctrl Pts',(-17.9710104137728,-1.66525935159368,
973.044117647059));
#156831=CARTESIAN_POINT('Ctrl Pts',(-18.1253194172301,-1.10985572039171E-15,
971.55));
#156832=CARTESIAN_POINT('Ctrl Pts',(-17.9710104137728,1.66525935159367,
970.055882352941));
#156833=CARTESIAN_POINT('Ctrl Pts',(-17.8167014103155,3.33051870318735,
968.561764705882));
#156834=CARTESIAN_POINT('Ctrl Pts',(-17.3590292079831,4.93906964482096,
967.067647058824));
#156835=CARTESIAN_POINT('Ctrl Pts',(-16.9013570056506,6.54762058645456,
965.573529411765));
#156836=CARTESIAN_POINT('Ctrl Pts',(-16.1559070823762,8.04468584505497,
964.079411764706));
#156837=CARTESIAN_POINT('Ctrl Pts',(-15.4104571591017,9.54175110365538,
962.585294117647));
#156838=CARTESIAN_POINT('Ctrl Pts',(-14.4026149179538,10.8763499173728,
961.091176470588));
#156839=CARTESIAN_POINT('Ctrl Pts',(-13.3947726768058,12.2109487310903,
959.59705882353));
#156840=CARTESIAN_POINT('Ctrl Pts',(-12.1588589765331,13.3376329379985,
958.102941176471));
#156841=CARTESIAN_POINT('Ctrl Pts',(-10.9229452762603,14.4643171449067,
956.608823529412));
#156842=CARTESIAN_POINT('Ctrl Pts',(-9.50104767561052,15.3447188656481,
955.114705882353));
#156843=CARTESIAN_POINT('Ctrl Pts',(-8.07915007496071,16.2251205863895,
953.620588235294));
#156844=CARTESIAN_POINT('Ctrl Pts',(-6.51968959134574,16.8292587962898,
952.126470588235));
#156845=CARTESIAN_POINT('Ctrl Pts',(-4.96022910773078,17.4333970061901,
950.632352941177));
#156846=CARTESIAN_POINT('Ctrl Pts',(-3.31631129755346,17.7406985030951,
949.138235294118));
#156847=CARTESIAN_POINT('Ctrl Pts',(-1.67239348737615,18.048,947.644117647059));
#156848=CARTESIAN_POINT('Ctrl Pts',(-2.21024254310115E-15,18.048,946.15));
#156849=CARTESIAN_POINT('Ctrl Pts',(1.67239348737616,18.048,944.655882352941));
#156850=CARTESIAN_POINT('Ctrl Pts',(3.31631129755346,17.7406985030951,943.161764705882));
#156851=CARTESIAN_POINT('Ctrl Pts',(4.96022910773077,17.4333970061901,941.667647058824));
#156852=CARTESIAN_POINT('Ctrl Pts',(6.51968959134575,16.8292587962898,940.173529411765));
#156853=CARTESIAN_POINT('Ctrl Pts',(8.07915007496071,16.2251205863895,938.679411764706));
#156854=CARTESIAN_POINT('Ctrl Pts',(9.50104767561053,15.3447188656481,937.185294117647));
#156855=CARTESIAN_POINT('Ctrl Pts',(10.9229452762603,14.4643171449067,935.691176470589));
#156856=CARTESIAN_POINT('Ctrl Pts',(12.1588589765331,13.3376329379985,934.19705882353));
#156857=CARTESIAN_POINT('Ctrl Pts',(13.3947726768058,12.2109487310903,932.702941176471));
#156858=CARTESIAN_POINT('Ctrl Pts',(14.4026149179538,10.8763499173728,931.208823529412));
#156859=CARTESIAN_POINT('Ctrl Pts',(15.4104571591017,9.54175110365538,929.714705882353));
#156860=CARTESIAN_POINT('Ctrl Pts',(16.1559070823762,8.04468584505496,928.220588235294));
#156861=CARTESIAN_POINT('Ctrl Pts',(16.9013570056506,6.54762058645456,926.726470588235));
#156862=CARTESIAN_POINT('Ctrl Pts',(17.3590292079831,4.93906964482096,925.232352941176));
#156863=CARTESIAN_POINT('Ctrl Pts',(17.8167014103155,3.33051870318735,923.738235294118));
#156864=CARTESIAN_POINT('Ctrl Pts',(17.9710104137728,1.66525935159367,922.244117647059));
#156865=CARTESIAN_POINT('Ctrl Pts',(18.1253194172301,3.32956716117513E-15,
920.75));
#156866=CARTESIAN_POINT('Ctrl Pts',(17.9710104137728,-1.66525935159367,
919.255882352941));
#156867=CARTESIAN_POINT('Ctrl Pts',(17.8167014103155,-3.33051870318736,
917.761764705882));
#156868=CARTESIAN_POINT('Ctrl Pts',(17.3590292079831,-4.93906964482095,
916.267647058824));
#156869=CARTESIAN_POINT('Ctrl Pts',(16.9013570056506,-6.54762058645456,
914.773529411765));
#156870=CARTESIAN_POINT('Ctrl Pts',(16.1559070823762,-8.04468584505497,
913.279411764706));
#156871=CARTESIAN_POINT('Ctrl Pts',(15.4104571591017,-9.54175110365538,
911.785294117647));
#156872=CARTESIAN_POINT('Ctrl Pts',(14.4026149179538,-10.8763499173728,
910.291176470588));
#156873=CARTESIAN_POINT('Ctrl Pts',(13.3947726768058,-12.2109487310903,
908.797058823529));
#156874=CARTESIAN_POINT('Ctrl Pts',(12.1588589765331,-13.3376329379985,
907.302941176471));
#156875=CARTESIAN_POINT('Ctrl Pts',(10.9229452762603,-14.4643171449067,
905.808823529412));
#156876=CARTESIAN_POINT('Ctrl Pts',(9.50104767561053,-15.3447188656481,
904.314705882353));
#156877=CARTESIAN_POINT('Ctrl Pts',(8.07915007496071,-16.2251205863895,
902.820588235294));
#156878=CARTESIAN_POINT('Ctrl Pts',(6.51968959134574,-16.8292587962898,
901.326470588235));
#156879=CARTESIAN_POINT('Ctrl Pts',(4.96022910773078,-17.4333970061901,
899.832352941177));
#156880=CARTESIAN_POINT('Ctrl Pts',(3.31631129755346,-17.7406985030951,
898.338235294118));
#156881=CARTESIAN_POINT('Ctrl Pts',(1.67239348737615,-18.048,896.844117647059));
#156882=CARTESIAN_POINT('Ctrl Pts',(0.,-18.048,895.35));
#156883=CARTESIAN_POINT('Ctrl Pts',(-1.67239348737615,-18.048,893.855882352941));
#156884=CARTESIAN_POINT('Ctrl Pts',(-3.31631129755346,-17.7406985030951,
892.361764705882));
#156885=CARTESIAN_POINT('Ctrl Pts',(-4.96022910773077,-17.4333970061901,
890.867647058824));
#156886=CARTESIAN_POINT('Ctrl Pts',(-6.51968959134574,-16.8292587962898,
889.373529411765));
#156887=CARTESIAN_POINT('Ctrl Pts',(-8.07915007496071,-16.2251205863895,
887.879411764706));
#156888=CARTESIAN_POINT('Ctrl Pts',(-9.50104767561052,-15.3447188656481,
886.385294117647));
#156889=CARTESIAN_POINT('Ctrl Pts',(-10.9229452762603,-14.4643171449067,
884.891176470588));
#156890=CARTESIAN_POINT('Ctrl Pts',(-12.1588589765331,-13.3376329379985,
883.39705882353));
#156891=CARTESIAN_POINT('Ctrl Pts',(-13.3947726768058,-12.2109487310903,
881.902941176471));
#156892=CARTESIAN_POINT('Ctrl Pts',(-14.4026149179538,-10.8763499173728,
880.408823529412));
#156893=CARTESIAN_POINT('Ctrl Pts',(-15.4104571591017,-9.54175110365538,
878.914705882353));
#156894=CARTESIAN_POINT('Ctrl Pts',(-16.1559070823762,-8.04468584505497,
877.420588235294));
#156895=CARTESIAN_POINT('Ctrl Pts',(-16.9013570056506,-6.54762058645456,
875.926470588235));
#156896=CARTESIAN_POINT('Ctrl Pts',(-17.3590292079831,-4.93906964482095,
874.432352941177));
#156897=CARTESIAN_POINT('Ctrl Pts',(-17.8167014103155,-3.33051870318735,
872.938235294118));
#156898=CARTESIAN_POINT('Ctrl Pts',(-17.9710104137728,-1.66525935159368,
871.444117647059));
#156899=CARTESIAN_POINT('Ctrl Pts',(-18.1253194172301,-1.10985572039171E-15,
869.95));
#156900=CARTESIAN_POINT('Ctrl Pts',(-17.9710104137728,1.66525935159367,
868.455882352941));
#156901=CARTESIAN_POINT('Ctrl Pts',(-17.8167014103155,3.33051870318735,
866.961764705882));
#156902=CARTESIAN_POINT('Ctrl Pts',(-17.3590292079831,4.93906964482096,
865.467647058824));
#156903=CARTESIAN_POINT('Ctrl Pts',(-16.9013570056506,6.54762058645456,
863.973529411765));
#156904=CARTESIAN_POINT('Ctrl Pts',(-16.1559070823762,8.04468584505497,
862.479411764706));
#156905=CARTESIAN_POINT('Ctrl Pts',(-15.4104571591017,9.54175110365538,
860.985294117647));
#156906=CARTESIAN_POINT('Ctrl Pts',(-14.4026149179538,10.8763499173728,
859.491176470588));
#156907=CARTESIAN_POINT('Ctrl Pts',(-13.3947726768058,12.2109487310903,
857.997058823529));
#156908=CARTESIAN_POINT('Ctrl Pts',(-12.1588589765331,13.3376329379985,
856.502941176471));
#156909=CARTESIAN_POINT('Ctrl Pts',(-10.9229452762603,14.4643171449067,
855.008823529412));
#156910=CARTESIAN_POINT('Ctrl Pts',(-9.50104767561052,15.3447188656481,
853.514705882353));
#156911=CARTESIAN_POINT('Ctrl Pts',(-8.07915007496071,16.2251205863895,
852.020588235294));
#156912=CARTESIAN_POINT('Ctrl Pts',(-6.51968959134574,16.8292587962898,
850.526470588235));
#156913=CARTESIAN_POINT('Ctrl Pts',(-4.96022910773078,17.4333970061901,
849.032352941177));
#156914=CARTESIAN_POINT('Ctrl Pts',(-3.31631129755346,17.7406985030951,
847.538235294118));
#156915=CARTESIAN_POINT('Ctrl Pts',(-1.67239348737615,18.048,846.044117647059));
#156916=CARTESIAN_POINT('Ctrl Pts',(-2.21024254310115E-15,18.048,844.55));
#156917=CARTESIAN_POINT('Ctrl Pts',(1.67239348737616,18.048,843.055882352941));
#156918=CARTESIAN_POINT('Ctrl Pts',(3.31631129755346,17.7406985030951,841.561764705883));
#156919=CARTESIAN_POINT('Ctrl Pts',(4.96022910773077,17.4333970061901,840.067647058824));
#156920=CARTESIAN_POINT('Ctrl Pts',(6.51968959134575,16.8292587962898,838.573529411765));
#156921=CARTESIAN_POINT('Ctrl Pts',(8.07915007496071,16.2251205863895,837.079411764706));
#156922=CARTESIAN_POINT('Ctrl Pts',(9.50104767561053,15.3447188656481,835.585294117647));
#156923=CARTESIAN_POINT('Ctrl Pts',(10.9229452762603,14.4643171449067,834.091176470588));
#156924=CARTESIAN_POINT('Ctrl Pts',(12.1588589765331,13.3376329379985,832.597058823529));
#156925=CARTESIAN_POINT('Ctrl Pts',(13.3947726768058,12.2109487310903,831.102941176471));
#156926=CARTESIAN_POINT('Ctrl Pts',(14.4026149179538,10.8763499173728,829.608823529412));
#156927=CARTESIAN_POINT('Ctrl Pts',(15.4104571591017,9.54175110365538,828.114705882353));
#156928=CARTESIAN_POINT('Ctrl Pts',(16.1559070823762,8.04468584505496,826.620588235294));
#156929=CARTESIAN_POINT('Ctrl Pts',(16.9013570056506,6.54762058645456,825.126470588235));
#156930=CARTESIAN_POINT('Ctrl Pts',(17.3590292079831,4.93906964482096,823.632352941177));
#156931=CARTESIAN_POINT('Ctrl Pts',(17.8167014103155,3.33051870318735,822.138235294118));
#156932=CARTESIAN_POINT('Ctrl Pts',(17.9710104137728,1.66525935159367,820.644117647059));
#156933=CARTESIAN_POINT('Ctrl Pts',(18.1253194172301,3.32956716117513E-15,
819.15));
#156934=CARTESIAN_POINT('Ctrl Pts',(17.9710104137728,-1.66525935159367,
817.655882352941));
#156935=CARTESIAN_POINT('Ctrl Pts',(17.8167014103155,-3.33051870318736,
816.161764705882));
#156936=CARTESIAN_POINT('Ctrl Pts',(17.3590292079831,-4.93906964482095,
814.667647058824));
#156937=CARTESIAN_POINT('Ctrl Pts',(16.9013570056506,-6.54762058645456,
813.173529411765));
#156938=CARTESIAN_POINT('Ctrl Pts',(16.1559070823762,-8.04468584505497,
811.679411764706));
#156939=CARTESIAN_POINT('Ctrl Pts',(15.4104571591017,-9.54175110365538,
810.185294117647));
#156940=CARTESIAN_POINT('Ctrl Pts',(14.4026149179538,-10.8763499173728,
808.691176470588));
#156941=CARTESIAN_POINT('Ctrl Pts',(13.3947726768058,-12.2109487310903,
807.197058823529));
#156942=CARTESIAN_POINT('Ctrl Pts',(12.1588589765331,-13.3376329379985,
805.702941176471));
#156943=CARTESIAN_POINT('Ctrl Pts',(10.9229452762603,-14.4643171449067,
804.208823529412));
#156944=CARTESIAN_POINT('Ctrl Pts',(9.50104767561053,-15.3447188656481,
802.714705882353));
#156945=CARTESIAN_POINT('Ctrl Pts',(8.07915007496071,-16.2251205863895,
801.220588235294));
#156946=CARTESIAN_POINT('Ctrl Pts',(6.51968959134574,-16.8292587962898,
799.726470588235));
#156947=CARTESIAN_POINT('Ctrl Pts',(4.96022910773078,-17.4333970061901,
798.232352941176));
#156948=CARTESIAN_POINT('Ctrl Pts',(3.31631129755346,-17.7406985030951,
796.738235294118));
#156949=CARTESIAN_POINT('Ctrl Pts',(1.67239348737615,-18.048,795.244117647059));
#156950=CARTESIAN_POINT('Ctrl Pts',(0.,-18.048,793.75));
#156951=CARTESIAN_POINT('Ctrl Pts',(-1.67239348737615,-18.048,792.255882352941));
#156952=CARTESIAN_POINT('Ctrl Pts',(-3.31631129755346,-17.7406985030951,
790.761764705882));
#156953=CARTESIAN_POINT('Ctrl Pts',(-4.96022910773077,-17.4333970061901,
789.267647058824));
#156954=CARTESIAN_POINT('Ctrl Pts',(-6.51968959134574,-16.8292587962898,
787.773529411765));
#156955=CARTESIAN_POINT('Ctrl Pts',(-8.07915007496071,-16.2251205863895,
786.279411764706));
#156956=CARTESIAN_POINT('Ctrl Pts',(-9.50104767561052,-15.3447188656481,
784.785294117647));
#156957=CARTESIAN_POINT('Ctrl Pts',(-10.9229452762603,-14.4643171449067,
783.291176470588));
#156958=CARTESIAN_POINT('Ctrl Pts',(-12.1588589765331,-13.3376329379985,
781.797058823529));
#156959=CARTESIAN_POINT('Ctrl Pts',(-13.3947726768058,-12.2109487310903,
780.302941176471));
#156960=CARTESIAN_POINT('Ctrl Pts',(-14.4026149179538,-10.8763499173728,
778.808823529412));
#156961=CARTESIAN_POINT('Ctrl Pts',(-15.4104571591017,-9.54175110365538,
777.314705882353));
#156962=CARTESIAN_POINT('Ctrl Pts',(-16.1559070823762,-8.04468584505497,
775.820588235294));
#156963=CARTESIAN_POINT('Ctrl Pts',(-16.9013570056506,-6.54762058645456,
774.326470588235));
#156964=CARTESIAN_POINT('Ctrl Pts',(-17.3590292079831,-4.93906964482095,
772.832352941177));
#156965=CARTESIAN_POINT('Ctrl Pts',(-17.8167014103155,-3.33051870318735,
771.338235294118));
#156966=CARTESIAN_POINT('Ctrl Pts',(-17.9710104137728,-1.66525935159368,
769.844117647059));
#156967=CARTESIAN_POINT('Ctrl Pts',(-18.1253194172301,-1.10985572039171E-15,
768.35));
#156968=CARTESIAN_POINT('Ctrl Pts',(-17.9710104137728,1.66525935159367,
766.855882352941));
#156969=CARTESIAN_POINT('Ctrl Pts',(-17.8167014103155,3.33051870318735,
765.361764705882));
#156970=CARTESIAN_POINT('Ctrl Pts',(-17.3590292079831,4.93906964482096,
763.867647058824));
#156971=CARTESIAN_POINT('Ctrl Pts',(-16.9013570056506,6.54762058645456,
762.373529411765));
#156972=CARTESIAN_POINT('Ctrl Pts',(-16.1559070823762,8.04468584505497,
760.879411764706));
#156973=CARTESIAN_POINT('Ctrl Pts',(-15.4104571591017,9.54175110365538,
759.385294117647));
#156974=CARTESIAN_POINT('Ctrl Pts',(-14.4026149179538,10.8763499173728,
757.891176470588));
#156975=CARTESIAN_POINT('Ctrl Pts',(-13.3947726768058,12.2109487310903,
756.397058823529));
#156976=CARTESIAN_POINT('Ctrl Pts',(-12.1588589765331,13.3376329379985,
754.902941176471));
#156977=CARTESIAN_POINT('Ctrl Pts',(-10.9229452762603,14.4643171449067,
753.408823529412));
#156978=CARTESIAN_POINT('Ctrl Pts',(-9.50104767561052,15.3447188656481,
751.914705882353));
#156979=CARTESIAN_POINT('Ctrl Pts',(-8.07915007496071,16.2251205863895,
750.420588235294));
#156980=CARTESIAN_POINT('Ctrl Pts',(-6.51968959134574,16.8292587962898,
748.926470588235));
#156981=CARTESIAN_POINT('Ctrl Pts',(-4.96022910773078,17.4333970061901,
747.432352941176));
#156982=CARTESIAN_POINT('Ctrl Pts',(-3.31631129755346,17.7406985030951,
745.938235294118));
#156983=CARTESIAN_POINT('Ctrl Pts',(-1.67239348737615,18.048,744.444117647059));
#156984=CARTESIAN_POINT('Ctrl Pts',(-2.21024254310115E-15,18.048,742.95));
#156985=CARTESIAN_POINT('Ctrl Pts',(1.67239348737616,18.048,741.455882352941));
#156986=CARTESIAN_POINT('Ctrl Pts',(3.31631129755346,17.7406985030951,739.961764705882));
#156987=CARTESIAN_POINT('Ctrl Pts',(4.96022910773077,17.4333970061901,738.467647058824));
#156988=CARTESIAN_POINT('Ctrl Pts',(6.51968959134575,16.8292587962898,736.973529411765));
#156989=CARTESIAN_POINT('Ctrl Pts',(8.07915007496071,16.2251205863895,735.479411764706));
#156990=CARTESIAN_POINT('Ctrl Pts',(9.50104767561053,15.3447188656481,733.985294117647));
#156991=CARTESIAN_POINT('Ctrl Pts',(10.9229452762603,14.4643171449067,732.491176470588));
#156992=CARTESIAN_POINT('Ctrl Pts',(12.1588589765331,13.3376329379985,730.99705882353));
#156993=CARTESIAN_POINT('Ctrl Pts',(13.3947726768058,12.2109487310903,729.502941176471));
#156994=CARTESIAN_POINT('Ctrl Pts',(14.4026149179538,10.8763499173728,728.008823529412));
#156995=CARTESIAN_POINT('Ctrl Pts',(15.4104571591017,9.54175110365538,726.514705882353));
#156996=CARTESIAN_POINT('Ctrl Pts',(16.1559070823762,8.04468584505496,725.020588235294));
#156997=CARTESIAN_POINT('Ctrl Pts',(16.9013570056506,6.54762058645456,723.526470588235));
#156998=CARTESIAN_POINT('Ctrl Pts',(17.3590292079831,4.93906964482096,722.032352941177));
#156999=CARTESIAN_POINT('Ctrl Pts',(17.8167014103155,3.33051870318735,720.538235294118));
#157000=CARTESIAN_POINT('Ctrl Pts',(17.9710104137728,1.66525935159367,719.044117647059));
#157001=CARTESIAN_POINT('Ctrl Pts',(18.1253194172301,3.32956716117513E-15,
717.55));
#157002=CARTESIAN_POINT('Ctrl Pts',(17.9710104137728,-1.66525935159367,
716.055882352941));
#157003=CARTESIAN_POINT('Ctrl Pts',(17.8167014103155,-3.33051870318736,
714.561764705882));
#157004=CARTESIAN_POINT('Ctrl Pts',(17.3590292079831,-4.93906964482095,
713.067647058824));
#157005=CARTESIAN_POINT('Ctrl Pts',(16.9013570056506,-6.54762058645456,
711.573529411765));
#157006=CARTESIAN_POINT('Ctrl Pts',(16.1559070823762,-8.04468584505497,
710.079411764706));
#157007=CARTESIAN_POINT('Ctrl Pts',(15.4104571591017,-9.54175110365538,
708.585294117647));
#157008=CARTESIAN_POINT('Ctrl Pts',(14.4026149179538,-10.8763499173728,
707.091176470588));
#157009=CARTESIAN_POINT('Ctrl Pts',(13.3947726768058,-12.2109487310903,
705.597058823529));
#157010=CARTESIAN_POINT('Ctrl Pts',(12.1588589765331,-13.3376329379985,
704.102941176471));
#157011=CARTESIAN_POINT('Ctrl Pts',(10.9229452762603,-14.4643171449067,
702.608823529412));
#157012=CARTESIAN_POINT('Ctrl Pts',(9.50104767561053,-15.3447188656481,
701.114705882353));
#157013=CARTESIAN_POINT('Ctrl Pts',(8.07915007496071,-16.2251205863895,
699.620588235294));
#157014=CARTESIAN_POINT('Ctrl Pts',(6.51968959134574,-16.8292587962898,
698.126470588235));
#157015=CARTESIAN_POINT('Ctrl Pts',(4.96022910773078,-17.4333970061901,
696.632352941177));
#157016=CARTESIAN_POINT('Ctrl Pts',(3.31631129755346,-17.7406985030951,
695.138235294118));
#157017=CARTESIAN_POINT('Ctrl Pts',(1.67239348737615,-18.048,693.644117647059));
#157018=CARTESIAN_POINT('Ctrl Pts',(0.,-18.048,692.15));
#157019=CARTESIAN_POINT('Ctrl Pts',(-1.67239348737615,-18.048,690.655882352941));
#157020=CARTESIAN_POINT('Ctrl Pts',(-3.31631129755346,-17.7406985030951,
689.161764705882));
#157021=CARTESIAN_POINT('Ctrl Pts',(-4.96022910773077,-17.4333970061901,
687.667647058824));
#157022=CARTESIAN_POINT('Ctrl Pts',(-6.51968959134574,-16.8292587962898,
686.173529411765));
#157023=CARTESIAN_POINT('Ctrl Pts',(-8.07915007496071,-16.2251205863895,
684.679411764706));
#157024=CARTESIAN_POINT('Ctrl Pts',(-9.50104767561052,-15.3447188656481,
683.185294117647));
#157025=CARTESIAN_POINT('Ctrl Pts',(-10.9229452762603,-14.4643171449067,
681.691176470588));
#157026=CARTESIAN_POINT('Ctrl Pts',(-12.1588589765331,-13.3376329379985,
680.197058823529));
#157027=CARTESIAN_POINT('Ctrl Pts',(-13.3947726768058,-12.2109487310903,
678.702941176471));
#157028=CARTESIAN_POINT('Ctrl Pts',(-14.4026149179538,-10.8763499173728,
677.208823529412));
#157029=CARTESIAN_POINT('Ctrl Pts',(-15.4104571591017,-9.54175110365538,
675.714705882353));
#157030=CARTESIAN_POINT('Ctrl Pts',(-16.1559070823762,-8.04468584505497,
674.220588235294));
#157031=CARTESIAN_POINT('Ctrl Pts',(-16.9013570056506,-6.54762058645456,
672.726470588236));
#157032=CARTESIAN_POINT('Ctrl Pts',(-17.3590292079831,-4.93906964482095,
671.232352941176));
#157033=CARTESIAN_POINT('Ctrl Pts',(-17.8167014103155,-3.33051870318735,
669.738235294118));
#157034=CARTESIAN_POINT('Ctrl Pts',(-17.9710104137728,-1.66525935159368,
668.244117647059));
#157035=CARTESIAN_POINT('Ctrl Pts',(-18.1253194172301,-1.10985572039171E-15,
666.75));
#157036=CARTESIAN_POINT('Ctrl Pts',(-17.9710104137728,1.66525935159367,
665.255882352941));
#157037=CARTESIAN_POINT('Ctrl Pts',(-17.8167014103155,3.33051870318735,
663.761764705882));
#157038=CARTESIAN_POINT('Ctrl Pts',(-17.3590292079831,4.93906964482096,
662.267647058824));
#157039=CARTESIAN_POINT('Ctrl Pts',(-16.9013570056506,6.54762058645456,
660.773529411765));
#157040=CARTESIAN_POINT('Ctrl Pts',(-16.1559070823762,8.04468584505497,
659.279411764706));
#157041=CARTESIAN_POINT('Ctrl Pts',(-15.4104571591017,9.54175110365538,
657.785294117647));
#157042=CARTESIAN_POINT('Ctrl Pts',(-14.4026149179538,10.8763499173728,
656.291176470588));
#157043=CARTESIAN_POINT('Ctrl Pts',(-13.3947726768058,12.2109487310903,
654.797058823529));
#157044=CARTESIAN_POINT('Ctrl Pts',(-12.1588589765331,13.3376329379985,
653.302941176471));
#157045=CARTESIAN_POINT('Ctrl Pts',(-10.9229452762603,14.4643171449067,
651.808823529412));
#157046=CARTESIAN_POINT('Ctrl Pts',(-9.50104767561052,15.3447188656481,
650.314705882353));
#157047=CARTESIAN_POINT('Ctrl Pts',(-8.07915007496071,16.2251205863895,
648.820588235294));
#157048=CARTESIAN_POINT('Ctrl Pts',(-6.51968959134574,16.8292587962898,
647.326470588235));
#157049=CARTESIAN_POINT('Ctrl Pts',(-4.96022910773078,17.4333970061901,
645.832352941176));
#157050=CARTESIAN_POINT('Ctrl Pts',(-3.31631129755346,17.7406985030951,
644.338235294118));
#157051=CARTESIAN_POINT('Ctrl Pts',(-1.67239348737615,18.048,642.844117647059));
#157052=CARTESIAN_POINT('Ctrl Pts',(-2.21024254310115E-15,18.048,641.35));
#157053=CARTESIAN_POINT('Ctrl Pts',(1.67239348737616,18.048,639.855882352941));
#157054=CARTESIAN_POINT('Ctrl Pts',(3.31631129755346,17.7406985030951,638.361764705882));
#157055=CARTESIAN_POINT('Ctrl Pts',(4.96022910773077,17.4333970061901,636.867647058824));
#157056=CARTESIAN_POINT('Ctrl Pts',(6.51968959134575,16.8292587962898,635.373529411765));
#157057=CARTESIAN_POINT('Ctrl Pts',(8.07915007496071,16.2251205863895,633.879411764706));
#157058=CARTESIAN_POINT('Ctrl Pts',(9.50104767561053,15.3447188656481,632.385294117647));
#157059=CARTESIAN_POINT('Ctrl Pts',(10.9229452762603,14.4643171449067,630.891176470588));
#157060=CARTESIAN_POINT('Ctrl Pts',(12.1588589765331,13.3376329379985,629.39705882353));
#157061=CARTESIAN_POINT('Ctrl Pts',(13.3947726768058,12.2109487310903,627.902941176471));
#157062=CARTESIAN_POINT('Ctrl Pts',(14.4026149179538,10.8763499173728,626.408823529412));
#157063=CARTESIAN_POINT('Ctrl Pts',(15.4104571591017,9.54175110365538,624.914705882353));
#157064=CARTESIAN_POINT('Ctrl Pts',(16.1559070823762,8.04468584505496,623.420588235294));
#157065=CARTESIAN_POINT('Ctrl Pts',(16.9013570056506,6.54762058645456,621.926470588235));
#157066=CARTESIAN_POINT('Ctrl Pts',(17.3590292079831,4.93906964482096,620.432352941177));
#157067=CARTESIAN_POINT('Ctrl Pts',(17.8167014103155,3.33051870318735,618.938235294118));
#157068=CARTESIAN_POINT('Ctrl Pts',(17.9710104137728,1.66525935159367,617.444117647059));
#157069=CARTESIAN_POINT('Ctrl Pts',(18.1253194172301,3.32956716117513E-15,
615.95));
#157070=CARTESIAN_POINT('Ctrl Pts',(17.9710104137728,-1.66525935159367,
614.455882352941));
#157071=CARTESIAN_POINT('Ctrl Pts',(17.8167014103155,-3.33051870318736,
612.961764705883));
#157072=CARTESIAN_POINT('Ctrl Pts',(17.3590292079831,-4.93906964482095,
611.467647058824));
#157073=CARTESIAN_POINT('Ctrl Pts',(16.9013570056506,-6.54762058645456,
609.973529411765));
#157074=CARTESIAN_POINT('Ctrl Pts',(16.1559070823762,-8.04468584505497,
608.479411764706));
#157075=CARTESIAN_POINT('Ctrl Pts',(15.4104571591017,-9.54175110365538,
606.985294117647));
#157076=CARTESIAN_POINT('Ctrl Pts',(14.4026149179538,-10.8763499173728,
605.491176470588));
#157077=CARTESIAN_POINT('Ctrl Pts',(13.3947726768058,-12.2109487310903,
603.997058823529));
#157078=CARTESIAN_POINT('Ctrl Pts',(12.1588589765331,-13.3376329379985,
602.502941176471));
#157079=CARTESIAN_POINT('Ctrl Pts',(10.9229452762603,-14.4643171449067,
601.008823529412));
#157080=CARTESIAN_POINT('Ctrl Pts',(9.50104767561053,-15.3447188656481,
599.514705882353));
#157081=CARTESIAN_POINT('Ctrl Pts',(8.07915007496071,-16.2251205863895,
598.020588235294));
#157082=CARTESIAN_POINT('Ctrl Pts',(6.51968959134574,-16.8292587962898,
596.526470588235));
#157083=CARTESIAN_POINT('Ctrl Pts',(4.96022910773078,-17.4333970061901,
595.032352941176));
#157084=CARTESIAN_POINT('Ctrl Pts',(3.31631129755346,-17.7406985030951,
593.538235294118));
#157085=CARTESIAN_POINT('Ctrl Pts',(1.67239348737615,-18.048,592.044117647059));
#157086=CARTESIAN_POINT('Ctrl Pts',(0.,-18.048,590.55));
#157087=CARTESIAN_POINT('Ctrl Pts',(-1.67239348737615,-18.048,589.055882352941));
#157088=CARTESIAN_POINT('Ctrl Pts',(-3.31631129755346,-17.7406985030951,
587.561764705882));
#157089=CARTESIAN_POINT('Ctrl Pts',(-4.96022910773077,-17.4333970061901,
586.067647058823));
#157090=CARTESIAN_POINT('Ctrl Pts',(-6.51968959134574,-16.8292587962898,
584.573529411765));
#157091=CARTESIAN_POINT('Ctrl Pts',(-8.07915007496071,-16.2251205863895,
583.079411764706));
#157092=CARTESIAN_POINT('Ctrl Pts',(-9.50104767561052,-15.3447188656481,
581.585294117647));
#157093=CARTESIAN_POINT('Ctrl Pts',(-10.9229452762603,-14.4643171449067,
580.091176470588));
#157094=CARTESIAN_POINT('Ctrl Pts',(-12.1588589765331,-13.3376329379985,
578.597058823529));
#157095=CARTESIAN_POINT('Ctrl Pts',(-13.3947726768058,-12.2109487310903,
577.102941176471));
#157096=CARTESIAN_POINT('Ctrl Pts',(-14.4026149179538,-10.8763499173728,
575.608823529412));
#157097=CARTESIAN_POINT('Ctrl Pts',(-15.4104571591017,-9.54175110365538,
574.114705882353));
#157098=CARTESIAN_POINT('Ctrl Pts',(-16.1559070823762,-8.04468584505497,
572.620588235294));
#157099=CARTESIAN_POINT('Ctrl Pts',(-16.9013570056506,-6.54762058645456,
571.126470588235));
#157100=CARTESIAN_POINT('Ctrl Pts',(-17.3590292079831,-4.93906964482095,
569.632352941177));
#157101=CARTESIAN_POINT('Ctrl Pts',(-17.8167014103155,-3.33051870318735,
568.138235294118));
#157102=CARTESIAN_POINT('Ctrl Pts',(-17.9710104137728,-1.66525935159368,
566.644117647059));
#157103=CARTESIAN_POINT('Ctrl Pts',(-18.1253194172301,-1.10985572039171E-15,
565.15));
#157104=CARTESIAN_POINT('Ctrl Pts',(-17.9710104137728,1.66525935159367,
563.655882352941));
#157105=CARTESIAN_POINT('Ctrl Pts',(-17.8167014103155,3.33051870318735,
562.161764705883));
#157106=CARTESIAN_POINT('Ctrl Pts',(-17.3590292079831,4.93906964482096,
560.667647058824));
#157107=CARTESIAN_POINT('Ctrl Pts',(-16.9013570056506,6.54762058645456,
559.173529411765));
#157108=CARTESIAN_POINT('Ctrl Pts',(-16.1559070823762,8.04468584505497,
557.679411764706));
#157109=CARTESIAN_POINT('Ctrl Pts',(-15.4104571591017,9.54175110365538,
556.185294117647));
#157110=CARTESIAN_POINT('Ctrl Pts',(-14.4026149179538,10.8763499173728,
554.691176470588));
#157111=CARTESIAN_POINT('Ctrl Pts',(-13.3947726768058,12.2109487310903,
553.19705882353));
#157112=CARTESIAN_POINT('Ctrl Pts',(-12.1588589765331,13.3376329379985,
551.702941176471));
#157113=CARTESIAN_POINT('Ctrl Pts',(-10.9229452762603,14.4643171449067,
550.208823529412));
#157114=CARTESIAN_POINT('Ctrl Pts',(-9.50104767561052,15.3447188656481,
548.714705882353));
#157115=CARTESIAN_POINT('Ctrl Pts',(-8.07915007496071,16.2251205863895,
547.220588235294));
#157116=CARTESIAN_POINT('Ctrl Pts',(-6.51968959134574,16.8292587962898,
545.726470588235));
#157117=CARTESIAN_POINT('Ctrl Pts',(-4.96022910773078,17.4333970061901,
544.232352941176));
#157118=CARTESIAN_POINT('Ctrl Pts',(-3.31631129755346,17.7406985030951,
542.738235294118));
#157119=CARTESIAN_POINT('Ctrl Pts',(-1.67239348737615,18.048,541.244117647059));
#157120=CARTESIAN_POINT('Ctrl Pts',(-2.21024254310115E-15,18.048,539.75));
#157121=CARTESIAN_POINT('Ctrl Pts',(1.67239348737616,18.048,538.255882352941));
#157122=CARTESIAN_POINT('Ctrl Pts',(3.31631129755346,17.7406985030951,536.761764705882));
#157123=CARTESIAN_POINT('Ctrl Pts',(4.96022910773077,17.4333970061901,535.267647058824));
#157124=CARTESIAN_POINT('Ctrl Pts',(6.51968959134575,16.8292587962898,533.773529411765));
#157125=CARTESIAN_POINT('Ctrl Pts',(8.07915007496071,16.2251205863895,532.279411764706));
#157126=CARTESIAN_POINT('Ctrl Pts',(9.50104767561053,15.3447188656481,530.785294117647));
#157127=CARTESIAN_POINT('Ctrl Pts',(10.9229452762603,14.4643171449067,529.291176470588));
#157128=CARTESIAN_POINT('Ctrl Pts',(12.1588589765331,13.3376329379985,527.797058823529));
#157129=CARTESIAN_POINT('Ctrl Pts',(13.3947726768058,12.2109487310903,526.302941176471));
#157130=CARTESIAN_POINT('Ctrl Pts',(14.4026149179538,10.8763499173728,524.808823529412));
#157131=CARTESIAN_POINT('Ctrl Pts',(15.4104571591017,9.54175110365538,523.314705882353));
#157132=CARTESIAN_POINT('Ctrl Pts',(16.1559070823762,8.04468584505496,521.820588235294));
#157133=CARTESIAN_POINT('Ctrl Pts',(16.9013570056506,6.54762058645456,520.326470588235));
#157134=CARTESIAN_POINT('Ctrl Pts',(17.3590292079831,4.93906964482096,518.832352941177));
#157135=CARTESIAN_POINT('Ctrl Pts',(17.8167014103155,3.33051870318735,517.338235294118));
#157136=CARTESIAN_POINT('Ctrl Pts',(17.9710104137728,1.66525935159367,515.844117647059));
#157137=CARTESIAN_POINT('Ctrl Pts',(18.1253194172301,3.32956716117513E-15,
514.35));
#157138=CARTESIAN_POINT('Ctrl Pts',(17.9710104137728,-1.66525935159367,
512.855882352941));
#157139=CARTESIAN_POINT('Ctrl Pts',(17.8167014103155,-3.33051870318736,
511.361764705882));
#157140=CARTESIAN_POINT('Ctrl Pts',(17.3590292079831,-4.93906964482095,
509.867647058824));
#157141=CARTESIAN_POINT('Ctrl Pts',(16.9013570056506,-6.54762058645456,
508.373529411765));
#157142=CARTESIAN_POINT('Ctrl Pts',(16.1559070823762,-8.04468584505497,
506.879411764706));
#157143=CARTESIAN_POINT('Ctrl Pts',(15.4104571591017,-9.54175110365538,
505.385294117647));
#157144=CARTESIAN_POINT('Ctrl Pts',(14.4026149179538,-10.8763499173728,
503.891176470588));
#157145=CARTESIAN_POINT('Ctrl Pts',(13.3947726768058,-12.2109487310903,
502.39705882353));
#157146=CARTESIAN_POINT('Ctrl Pts',(12.1588589765331,-13.3376329379985,
500.902941176471));
#157147=CARTESIAN_POINT('Ctrl Pts',(10.9229452762603,-14.4643171449067,
499.408823529412));
#157148=CARTESIAN_POINT('Ctrl Pts',(9.50104767561053,-15.3447188656481,
497.914705882353));
#157149=CARTESIAN_POINT('Ctrl Pts',(8.07915007496071,-16.2251205863895,
496.420588235294));
#157150=CARTESIAN_POINT('Ctrl Pts',(6.51968959134574,-16.8292587962898,
494.926470588235));
#157151=CARTESIAN_POINT('Ctrl Pts',(4.96022910773078,-17.4333970061901,
493.432352941177));
#157152=CARTESIAN_POINT('Ctrl Pts',(3.31631129755346,-17.7406985030951,
491.938235294118));
#157153=CARTESIAN_POINT('Ctrl Pts',(1.67239348737615,-18.048,490.444117647059));
#157154=CARTESIAN_POINT('Ctrl Pts',(0.,-18.048,488.95));
#157155=CARTESIAN_POINT('Ctrl Pts',(-1.67239348737615,-18.048,487.455882352941));
#157156=CARTESIAN_POINT('Ctrl Pts',(-3.31631129755346,-17.7406985030951,
485.961764705883));
#157157=CARTESIAN_POINT('Ctrl Pts',(-4.96022910773077,-17.4333970061901,
484.467647058824));
#157158=CARTESIAN_POINT('Ctrl Pts',(-6.51968959134574,-16.8292587962898,
482.973529411765));
#157159=CARTESIAN_POINT('Ctrl Pts',(-8.07915007496071,-16.2251205863895,
481.479411764706));
#157160=CARTESIAN_POINT('Ctrl Pts',(-9.50104767561052,-15.3447188656481,
479.985294117647));
#157161=CARTESIAN_POINT('Ctrl Pts',(-10.9229452762603,-14.4643171449067,
478.491176470588));
#157162=CARTESIAN_POINT('Ctrl Pts',(-12.1588589765331,-13.3376329379985,
476.99705882353));
#157163=CARTESIAN_POINT('Ctrl Pts',(-13.3947726768058,-12.2109487310903,
475.502941176471));
#157164=CARTESIAN_POINT('Ctrl Pts',(-14.4026149179538,-10.8763499173728,
474.008823529412));
#157165=CARTESIAN_POINT('Ctrl Pts',(-15.4104571591017,-9.54175110365538,
472.514705882353));
#157166=CARTESIAN_POINT('Ctrl Pts',(-16.1559070823762,-8.04468584505497,
471.020588235294));
#157167=CARTESIAN_POINT('Ctrl Pts',(-16.9013570056506,-6.54762058645456,
469.526470588235));
#157168=CARTESIAN_POINT('Ctrl Pts',(-17.3590292079831,-4.93906964482095,
468.032352941177));
#157169=CARTESIAN_POINT('Ctrl Pts',(-17.8167014103155,-3.33051870318735,
466.538235294118));
#157170=CARTESIAN_POINT('Ctrl Pts',(-17.9710104137728,-1.66525935159368,
465.044117647059));
#157171=CARTESIAN_POINT('Ctrl Pts',(-18.1253194172301,-1.10985572039171E-15,
463.55));
#157172=CARTESIAN_POINT('Ctrl Pts',(-17.9710104137728,1.66525935159367,
462.055882352941));
#157173=CARTESIAN_POINT('Ctrl Pts',(-17.8167014103155,3.33051870318735,
460.561764705882));
#157174=CARTESIAN_POINT('Ctrl Pts',(-17.3590292079831,4.93906964482096,
459.067647058824));
#157175=CARTESIAN_POINT('Ctrl Pts',(-16.9013570056506,6.54762058645456,
457.573529411765));
#157176=CARTESIAN_POINT('Ctrl Pts',(-16.1559070823762,8.04468584505497,
456.079411764706));
#157177=CARTESIAN_POINT('Ctrl Pts',(-15.4104571591017,9.54175110365538,
454.585294117647));
#157178=CARTESIAN_POINT('Ctrl Pts',(-14.4026149179538,10.8763499173728,
453.091176470588));
#157179=CARTESIAN_POINT('Ctrl Pts',(-13.3947726768058,12.2109487310903,
451.597058823529));
#157180=CARTESIAN_POINT('Ctrl Pts',(-12.1588589765331,13.3376329379985,
450.102941176471));
#157181=CARTESIAN_POINT('Ctrl Pts',(-10.9229452762603,14.4643171449067,
448.608823529412));
#157182=CARTESIAN_POINT('Ctrl Pts',(-9.50104767561052,15.3447188656481,
447.114705882353));
#157183=CARTESIAN_POINT('Ctrl Pts',(-8.07915007496071,16.2251205863895,
445.620588235294));
#157184=CARTESIAN_POINT('Ctrl Pts',(-6.51968959134574,16.8292587962898,
444.126470588235));
#157185=CARTESIAN_POINT('Ctrl Pts',(-4.96022910773078,17.4333970061901,
442.632352941176));
#157186=CARTESIAN_POINT('Ctrl Pts',(-3.31631129755346,17.7406985030951,
441.138235294118));
#157187=CARTESIAN_POINT('Ctrl Pts',(-1.67239348737615,18.048,439.644117647059));
#157188=CARTESIAN_POINT('Ctrl Pts',(-2.21024254310115E-15,18.048,438.15));
#157189=CARTESIAN_POINT('Ctrl Pts',(1.67239348737616,18.048,436.655882352941));
#157190=CARTESIAN_POINT('Ctrl Pts',(3.31631129755346,17.7406985030951,435.161764705882));
#157191=CARTESIAN_POINT('Ctrl Pts',(4.96022910773077,17.4333970061901,433.667647058824));
#157192=CARTESIAN_POINT('Ctrl Pts',(6.51968959134575,16.8292587962898,432.173529411765));
#157193=CARTESIAN_POINT('Ctrl Pts',(8.07915007496071,16.2251205863895,430.679411764706));
#157194=CARTESIAN_POINT('Ctrl Pts',(9.50104767561053,15.3447188656481,429.185294117647));
#157195=CARTESIAN_POINT('Ctrl Pts',(10.9229452762603,14.4643171449067,427.691176470588));
#157196=CARTESIAN_POINT('Ctrl Pts',(12.1588589765331,13.3376329379985,426.19705882353));
#157197=CARTESIAN_POINT('Ctrl Pts',(13.3947726768058,12.2109487310903,424.702941176471));
#157198=CARTESIAN_POINT('Ctrl Pts',(14.4026149179538,10.8763499173728,423.208823529412));
#157199=CARTESIAN_POINT('Ctrl Pts',(15.4104571591017,9.54175110365538,421.714705882353));
#157200=CARTESIAN_POINT('Ctrl Pts',(16.1559070823762,8.04468584505496,420.220588235294));
#157201=CARTESIAN_POINT('Ctrl Pts',(16.9013570056506,6.54762058645456,418.726470588235));
#157202=CARTESIAN_POINT('Ctrl Pts',(17.3590292079831,4.93906964482096,417.232352941177));
#157203=CARTESIAN_POINT('Ctrl Pts',(17.8167014103155,3.33051870318735,415.738235294118));
#157204=CARTESIAN_POINT('Ctrl Pts',(17.9710104137728,1.66525935159367,414.244117647059));
#157205=CARTESIAN_POINT('Ctrl Pts',(18.1253194172301,3.32956716117513E-15,
412.75));
#157206=CARTESIAN_POINT('Ctrl Pts',(17.9710104137728,-1.66525935159367,
411.255882352941));
#157207=CARTESIAN_POINT('Ctrl Pts',(17.8167014103155,-3.33051870318736,
409.761764705883));
#157208=CARTESIAN_POINT('Ctrl Pts',(17.3590292079831,-4.93906964482095,
408.267647058824));
#157209=CARTESIAN_POINT('Ctrl Pts',(16.9013570056506,-6.54762058645456,
406.773529411765));
#157210=CARTESIAN_POINT('Ctrl Pts',(16.1559070823762,-8.04468584505497,
405.279411764706));
#157211=CARTESIAN_POINT('Ctrl Pts',(15.4104571591017,-9.54175110365538,
403.785294117647));
#157212=CARTESIAN_POINT('Ctrl Pts',(14.4026149179538,-10.8763499173728,
402.291176470588));
#157213=CARTESIAN_POINT('Ctrl Pts',(13.3947726768058,-12.2109487310903,
400.797058823529));
#157214=CARTESIAN_POINT('Ctrl Pts',(12.1588589765331,-13.3376329379985,
399.302941176471));
#157215=CARTESIAN_POINT('Ctrl Pts',(10.9229452762603,-14.4643171449067,
397.808823529412));
#157216=CARTESIAN_POINT('Ctrl Pts',(9.50104767561053,-15.3447188656481,
396.314705882353));
#157217=CARTESIAN_POINT('Ctrl Pts',(8.07915007496071,-16.2251205863895,
394.820588235294));
#157218=CARTESIAN_POINT('Ctrl Pts',(6.51968959134574,-16.8292587962898,
393.326470588235));
#157219=CARTESIAN_POINT('Ctrl Pts',(4.96022910773078,-17.4333970061901,
391.832352941177));
#157220=CARTESIAN_POINT('Ctrl Pts',(3.31631129755346,-17.7406985030951,
390.338235294118));
#157221=CARTESIAN_POINT('Ctrl Pts',(1.67239348737615,-18.048,388.844117647059));
#157222=CARTESIAN_POINT('Ctrl Pts',(0.,-18.048,387.35));
#157223=CARTESIAN_POINT('Ctrl Pts',(-1.67239348737615,-18.048,385.855882352941));
#157224=CARTESIAN_POINT('Ctrl Pts',(-3.31631129755346,-17.7406985030951,
384.361764705882));
#157225=CARTESIAN_POINT('Ctrl Pts',(-4.96022910773077,-17.4333970061901,
382.867647058824));
#157226=CARTESIAN_POINT('Ctrl Pts',(-6.51968959134574,-16.8292587962898,
381.373529411765));
#157227=CARTESIAN_POINT('Ctrl Pts',(-8.07915007496071,-16.2251205863895,
379.879411764706));
#157228=CARTESIAN_POINT('Ctrl Pts',(-9.50104767561052,-15.3447188656481,
378.385294117647));
#157229=CARTESIAN_POINT('Ctrl Pts',(-10.9229452762603,-14.4643171449067,
376.891176470588));
#157230=CARTESIAN_POINT('Ctrl Pts',(-12.1588589765331,-13.3376329379985,
375.397058823529));
#157231=CARTESIAN_POINT('Ctrl Pts',(-13.3947726768058,-12.2109487310903,
373.902941176471));
#157232=CARTESIAN_POINT('Ctrl Pts',(-14.4026149179538,-10.8763499173728,
372.408823529412));
#157233=CARTESIAN_POINT('Ctrl Pts',(-15.4104571591017,-9.54175110365538,
370.914705882353));
#157234=CARTESIAN_POINT('Ctrl Pts',(-16.1559070823762,-8.04468584505497,
369.420588235294));
#157235=CARTESIAN_POINT('Ctrl Pts',(-16.9013570056506,-6.54762058645456,
367.926470588235));
#157236=CARTESIAN_POINT('Ctrl Pts',(-17.3590292079831,-4.93906964482095,
366.432352941177));
#157237=CARTESIAN_POINT('Ctrl Pts',(-17.8167014103155,-3.33051870318735,
364.938235294118));
#157238=CARTESIAN_POINT('Ctrl Pts',(-17.9710104137728,-1.66525935159368,
363.444117647059));
#157239=CARTESIAN_POINT('Ctrl Pts',(-18.1253194172301,-1.10985572039171E-15,
361.95));
#157240=CARTESIAN_POINT('Ctrl Pts',(-17.9710104137728,1.66525935159367,
360.455882352941));
#157241=CARTESIAN_POINT('Ctrl Pts',(-17.8167014103155,3.33051870318735,
358.961764705882));
#157242=CARTESIAN_POINT('Ctrl Pts',(-17.3590292079831,4.93906964482096,
357.467647058824));
#157243=CARTESIAN_POINT('Ctrl Pts',(-16.9013570056506,6.54762058645456,
355.973529411765));
#157244=CARTESIAN_POINT('Ctrl Pts',(-16.1559070823762,8.04468584505497,
354.479411764706));
#157245=CARTESIAN_POINT('Ctrl Pts',(-15.4104571591017,9.54175110365538,
352.985294117647));
#157246=CARTESIAN_POINT('Ctrl Pts',(-14.4026149179538,10.8763499173728,
351.491176470588));
#157247=CARTESIAN_POINT('Ctrl Pts',(-13.3947726768058,12.2109487310903,
349.99705882353));
#157248=CARTESIAN_POINT('Ctrl Pts',(-12.1588589765331,13.3376329379985,
348.502941176471));
#157249=CARTESIAN_POINT('Ctrl Pts',(-10.9229452762603,14.4643171449067,
347.008823529412));
#157250=CARTESIAN_POINT('Ctrl Pts',(-9.50104767561052,15.3447188656481,
345.514705882353));
#157251=CARTESIAN_POINT('Ctrl Pts',(-8.07915007496071,16.2251205863895,
344.020588235294));
#157252=CARTESIAN_POINT('Ctrl Pts',(-6.51968959134574,16.8292587962898,
342.526470588235));
#157253=CARTESIAN_POINT('Ctrl Pts',(-4.96022910773078,17.4333970061901,
341.032352941177));
#157254=CARTESIAN_POINT('Ctrl Pts',(-3.31631129755346,17.7406985030951,
339.538235294118));
#157255=CARTESIAN_POINT('Ctrl Pts',(-1.67239348737615,18.048,338.044117647059));
#157256=CARTESIAN_POINT('Ctrl Pts',(-2.21024254310115E-15,18.048,336.55));
#157257=CARTESIAN_POINT('Ctrl Pts',(1.67239348737616,18.048,335.055882352941));
#157258=CARTESIAN_POINT('Ctrl Pts',(3.31631129755346,17.7406985030951,333.561764705882));
#157259=CARTESIAN_POINT('Ctrl Pts',(4.96022910773077,17.4333970061901,332.067647058824));
#157260=CARTESIAN_POINT('Ctrl Pts',(6.51968959134575,16.8292587962898,330.573529411765));
#157261=CARTESIAN_POINT('Ctrl Pts',(8.07915007496071,16.2251205863895,329.079411764706));
#157262=CARTESIAN_POINT('Ctrl Pts',(9.50104767561053,15.3447188656481,327.585294117647));
#157263=CARTESIAN_POINT('Ctrl Pts',(10.9229452762603,14.4643171449067,326.091176470588));
#157264=CARTESIAN_POINT('Ctrl Pts',(12.1588589765331,13.3376329379985,324.597058823529));
#157265=CARTESIAN_POINT('Ctrl Pts',(13.3947726768058,12.2109487310903,323.102941176471));
#157266=CARTESIAN_POINT('Ctrl Pts',(14.4026149179538,10.8763499173728,321.608823529412));
#157267=CARTESIAN_POINT('Ctrl Pts',(15.4104571591017,9.54175110365538,320.114705882353));
#157268=CARTESIAN_POINT('Ctrl Pts',(16.1559070823762,8.04468584505496,318.620588235294));
#157269=CARTESIAN_POINT('Ctrl Pts',(16.9013570056506,6.54762058645456,317.126470588235));
#157270=CARTESIAN_POINT('Ctrl Pts',(17.3590292079831,4.93906964482096,315.632352941176));
#157271=CARTESIAN_POINT('Ctrl Pts',(17.8167014103155,3.33051870318735,314.138235294118));
#157272=CARTESIAN_POINT('Ctrl Pts',(17.9710104137728,1.66525935159367,312.644117647059));
#157273=CARTESIAN_POINT('Ctrl Pts',(18.1253194172301,3.32956716117513E-15,
311.15));
#157274=CARTESIAN_POINT('Ctrl Pts',(17.9710104137728,-1.66525935159367,
309.655882352941));
#157275=CARTESIAN_POINT('Ctrl Pts',(17.8167014103155,-3.33051870318736,
308.161764705882));
#157276=CARTESIAN_POINT('Ctrl Pts',(17.3590292079831,-4.93906964482095,
306.667647058824));
#157277=CARTESIAN_POINT('Ctrl Pts',(16.9013570056506,-6.54762058645456,
305.173529411765));
#157278=CARTESIAN_POINT('Ctrl Pts',(16.1559070823762,-8.04468584505497,
303.679411764706));
#157279=CARTESIAN_POINT('Ctrl Pts',(15.4104571591017,-9.54175110365538,
302.185294117647));
#157280=CARTESIAN_POINT('Ctrl Pts',(14.4026149179538,-10.8763499173728,
300.691176470588));
#157281=CARTESIAN_POINT('Ctrl Pts',(13.3947726768058,-12.2109487310903,
299.19705882353));
#157282=CARTESIAN_POINT('Ctrl Pts',(12.1588589765331,-13.3376329379985,
297.702941176471));
#157283=CARTESIAN_POINT('Ctrl Pts',(10.9229452762603,-14.4643171449067,
296.208823529412));
#157284=CARTESIAN_POINT('Ctrl Pts',(9.50104767561053,-15.3447188656481,
294.714705882353));
#157285=CARTESIAN_POINT('Ctrl Pts',(8.07915007496071,-16.2251205863895,
293.220588235294));
#157286=CARTESIAN_POINT('Ctrl Pts',(6.51968959134574,-16.8292587962898,
291.726470588235));
#157287=CARTESIAN_POINT('Ctrl Pts',(4.96022910773078,-17.4333970061901,
290.232352941176));
#157288=CARTESIAN_POINT('Ctrl Pts',(3.31631129755346,-17.7406985030951,
288.738235294118));
#157289=CARTESIAN_POINT('Ctrl Pts',(1.67239348737615,-18.048,287.244117647059));
#157290=CARTESIAN_POINT('Ctrl Pts',(0.,-18.048,285.75));
#157291=CARTESIAN_POINT('Ctrl Pts',(-1.67239348737615,-18.048,284.255882352941));
#157292=CARTESIAN_POINT('Ctrl Pts',(-3.31631129755346,-17.7406985030951,
282.761764705882));
#157293=CARTESIAN_POINT('Ctrl Pts',(-4.96022910773077,-17.4333970061901,
281.267647058824));
#157294=CARTESIAN_POINT('Ctrl Pts',(-6.51968959134574,-16.8292587962898,
279.773529411765));
#157295=CARTESIAN_POINT('Ctrl Pts',(-8.07915007496071,-16.2251205863895,
278.279411764706));
#157296=CARTESIAN_POINT('Ctrl Pts',(-9.50104767561052,-15.3447188656481,
276.785294117647));
#157297=CARTESIAN_POINT('Ctrl Pts',(-10.9229452762603,-14.4643171449067,
275.291176470588));
#157298=CARTESIAN_POINT('Ctrl Pts',(-12.1588589765331,-13.3376329379985,
273.797058823529));
#157299=CARTESIAN_POINT('Ctrl Pts',(-13.3947726768058,-12.2109487310903,
272.302941176471));
#157300=CARTESIAN_POINT('Ctrl Pts',(-14.4026149179538,-10.8763499173728,
270.808823529412));
#157301=CARTESIAN_POINT('Ctrl Pts',(-15.4104571591017,-9.54175110365538,
269.314705882353));
#157302=CARTESIAN_POINT('Ctrl Pts',(-16.1559070823762,-8.04468584505497,
267.820588235294));
#157303=CARTESIAN_POINT('Ctrl Pts',(-16.9013570056506,-6.54762058645456,
266.326470588235));
#157304=CARTESIAN_POINT('Ctrl Pts',(-17.3590292079831,-4.93906964482095,
264.832352941177));
#157305=CARTESIAN_POINT('Ctrl Pts',(-17.8167014103155,-3.33051870318735,
263.338235294118));
#157306=CARTESIAN_POINT('Ctrl Pts',(-17.9710104137728,-1.66525935159368,
261.844117647059));
#157307=CARTESIAN_POINT('Ctrl Pts',(-18.1253194172301,-1.10985572039171E-15,
260.35));
#157308=CARTESIAN_POINT('Ctrl Pts',(-17.9710104137728,1.66525935159367,
258.855882352941));
#157309=CARTESIAN_POINT('Ctrl Pts',(-17.8167014103155,3.33051870318735,
257.361764705882));
#157310=CARTESIAN_POINT('Ctrl Pts',(-17.3590292079831,4.93906964482096,
255.867647058823));
#157311=CARTESIAN_POINT('Ctrl Pts',(-16.9013570056506,6.54762058645456,
254.373529411765));
#157312=CARTESIAN_POINT('Ctrl Pts',(-16.1559070823762,8.04468584505497,
252.879411764706));
#157313=CARTESIAN_POINT('Ctrl Pts',(-15.4104571591017,9.54175110365538,
251.385294117647));
#157314=CARTESIAN_POINT('Ctrl Pts',(-14.4026149179538,10.8763499173728,
249.891176470588));
#157315=CARTESIAN_POINT('Ctrl Pts',(-13.3947726768058,12.2109487310903,
248.397058823529));
#157316=CARTESIAN_POINT('Ctrl Pts',(-12.1588589765331,13.3376329379985,
246.902941176471));
#157317=CARTESIAN_POINT('Ctrl Pts',(-10.9229452762603,14.4643171449067,
245.408823529412));
#157318=CARTESIAN_POINT('Ctrl Pts',(-9.50104767561052,15.3447188656481,
243.914705882353));
#157319=CARTESIAN_POINT('Ctrl Pts',(-8.07915007496071,16.2251205863895,
242.420588235294));
#157320=CARTESIAN_POINT('Ctrl Pts',(-6.51968959134574,16.8292587962898,
240.926470588235));
#157321=CARTESIAN_POINT('Ctrl Pts',(-4.96022910773078,17.4333970061901,
239.432352941177));
#157322=CARTESIAN_POINT('Ctrl Pts',(-3.31631129755346,17.7406985030951,
237.938235294118));
#157323=CARTESIAN_POINT('Ctrl Pts',(-1.67239348737615,18.048,236.444117647059));
#157324=CARTESIAN_POINT('Ctrl Pts',(-2.21024254310115E-15,18.048,234.95));
#157325=CARTESIAN_POINT('Ctrl Pts',(1.67239348737616,18.048,233.455882352941));
#157326=CARTESIAN_POINT('Ctrl Pts',(3.31631129755346,17.7406985030951,231.961764705883));
#157327=CARTESIAN_POINT('Ctrl Pts',(4.96022910773077,17.4333970061901,230.467647058824));
#157328=CARTESIAN_POINT('Ctrl Pts',(6.51968959134575,16.8292587962898,228.973529411765));
#157329=CARTESIAN_POINT('Ctrl Pts',(8.07915007496071,16.2251205863895,227.479411764706));
#157330=CARTESIAN_POINT('Ctrl Pts',(9.50104767561053,15.3447188656481,225.985294117647));
#157331=CARTESIAN_POINT('Ctrl Pts',(10.9229452762603,14.4643171449067,224.491176470588));
#157332=CARTESIAN_POINT('Ctrl Pts',(12.1588589765331,13.3376329379985,222.99705882353));
#157333=CARTESIAN_POINT('Ctrl Pts',(13.3947726768058,12.2109487310903,221.502941176471));
#157334=CARTESIAN_POINT('Ctrl Pts',(14.4026149179538,10.8763499173728,220.008823529412));
#157335=CARTESIAN_POINT('Ctrl Pts',(15.4104571591017,9.54175110365538,218.514705882353));
#157336=CARTESIAN_POINT('Ctrl Pts',(16.1559070823762,8.04468584505496,217.020588235294));
#157337=CARTESIAN_POINT('Ctrl Pts',(16.9013570056506,6.54762058645456,215.526470588235));
#157338=CARTESIAN_POINT('Ctrl Pts',(17.3590292079831,4.93906964482096,214.032352941176));
#157339=CARTESIAN_POINT('Ctrl Pts',(17.8167014103155,3.33051870318735,212.538235294118));
#157340=CARTESIAN_POINT('Ctrl Pts',(17.9710104137728,1.66525935159367,211.044117647059));
#157341=CARTESIAN_POINT('Ctrl Pts',(18.1253194172301,3.32956716117513E-15,
209.55));
#157342=CARTESIAN_POINT('Ctrl Pts',(17.9710104137728,-1.66525935159367,
208.055882352941));
#157343=CARTESIAN_POINT('Ctrl Pts',(17.8167014103155,-3.33051870318736,
206.561764705882));
#157344=CARTESIAN_POINT('Ctrl Pts',(17.3590292079831,-4.93906964482095,
205.067647058824));
#157345=CARTESIAN_POINT('Ctrl Pts',(16.9013570056506,-6.54762058645456,
203.573529411765));
#157346=CARTESIAN_POINT('Ctrl Pts',(16.1559070823762,-8.04468584505497,
202.079411764706));
#157347=CARTESIAN_POINT('Ctrl Pts',(15.4104571591017,-9.54175110365538,
200.585294117647));
#157348=CARTESIAN_POINT('Ctrl Pts',(14.4026149179538,-10.8763499173728,
199.091176470588));
#157349=CARTESIAN_POINT('Ctrl Pts',(13.3947726768058,-12.2109487310903,
197.597058823529));
#157350=CARTESIAN_POINT('Ctrl Pts',(12.1588589765331,-13.3376329379985,
196.102941176471));
#157351=CARTESIAN_POINT('Ctrl Pts',(10.9229452762603,-14.4643171449067,
194.608823529412));
#157352=CARTESIAN_POINT('Ctrl Pts',(9.50104767561053,-15.3447188656481,
193.114705882353));
#157353=CARTESIAN_POINT('Ctrl Pts',(8.07915007496071,-16.2251205863895,
191.620588235294));
#157354=CARTESIAN_POINT('Ctrl Pts',(6.51968959134574,-16.8292587962898,
190.126470588235));
#157355=CARTESIAN_POINT('Ctrl Pts',(4.96022910773078,-17.4333970061901,
188.632352941176));
#157356=CARTESIAN_POINT('Ctrl Pts',(3.31631129755346,-17.7406985030951,
187.138235294118));
#157357=CARTESIAN_POINT('Ctrl Pts',(1.67239348737615,-18.048,185.644117647059));
#157358=CARTESIAN_POINT('Ctrl Pts',(0.,-18.048,184.15));
#157359=CARTESIAN_POINT('Ctrl Pts',(-1.67239348737615,-18.048,182.655882352941));
#157360=CARTESIAN_POINT('Ctrl Pts',(-3.31631129755346,-17.7406985030951,
181.161764705882));
#157361=CARTESIAN_POINT('Ctrl Pts',(-4.96022910773077,-17.4333970061901,
179.667647058824));
#157362=CARTESIAN_POINT('Ctrl Pts',(-6.51968959134574,-16.8292587962898,
178.173529411765));
#157363=CARTESIAN_POINT('Ctrl Pts',(-8.07915007496071,-16.2251205863895,
176.679411764706));
#157364=CARTESIAN_POINT('Ctrl Pts',(-9.50104767561052,-15.3447188656481,
175.185294117647));
#157365=CARTESIAN_POINT('Ctrl Pts',(-10.9229452762603,-14.4643171449067,
173.691176470588));
#157366=CARTESIAN_POINT('Ctrl Pts',(-12.1588589765331,-13.3376329379985,
172.19705882353));
#157367=CARTESIAN_POINT('Ctrl Pts',(-13.3947726768058,-12.2109487310903,
170.702941176471));
#157368=CARTESIAN_POINT('Ctrl Pts',(-14.4026149179538,-10.8763499173728,
169.208823529412));
#157369=CARTESIAN_POINT('Ctrl Pts',(-15.4104571591017,-9.54175110365538,
167.714705882353));
#157370=CARTESIAN_POINT('Ctrl Pts',(-16.1559070823762,-8.04468584505497,
166.220588235294));
#157371=CARTESIAN_POINT('Ctrl Pts',(-16.9013570056506,-6.54762058645456,
164.726470588235));
#157372=CARTESIAN_POINT('Ctrl Pts',(-17.3590292079831,-4.93906964482095,
163.232352941177));
#157373=CARTESIAN_POINT('Ctrl Pts',(-17.8167014103155,-3.33051870318735,
161.738235294118));
#157374=CARTESIAN_POINT('Ctrl Pts',(-17.9710104137728,-1.66525935159368,
160.244117647059));
#157375=CARTESIAN_POINT('Ctrl Pts',(-18.1253194172301,-1.10985572039171E-15,
158.75));
#157376=CARTESIAN_POINT('Ctrl Pts',(-17.9710104137728,1.66525935159367,
157.255882352941));
#157377=CARTESIAN_POINT('Ctrl Pts',(-17.8167014103155,3.33051870318735,
155.761764705882));
#157378=CARTESIAN_POINT('Ctrl Pts',(-17.3590292079831,4.93906964482096,
154.267647058824));
#157379=CARTESIAN_POINT('Ctrl Pts',(-16.9013570056506,6.54762058645456,
152.773529411765));
#157380=CARTESIAN_POINT('Ctrl Pts',(-16.1559070823762,8.04468584505497,
151.279411764706));
#157381=CARTESIAN_POINT('Ctrl Pts',(-15.4104571591017,9.54175110365538,
149.785294117647));
#157382=CARTESIAN_POINT('Ctrl Pts',(-14.4026149179538,10.8763499173728,
148.291176470588));
#157383=CARTESIAN_POINT('Ctrl Pts',(-13.3947726768058,12.2109487310903,
146.79705882353));
#157384=CARTESIAN_POINT('Ctrl Pts',(-12.1588589765331,13.3376329379985,
145.302941176471));
#157385=CARTESIAN_POINT('Ctrl Pts',(-10.9229452762603,14.4643171449067,
143.808823529412));
#157386=CARTESIAN_POINT('Ctrl Pts',(-9.50104767561052,15.3447188656481,
142.314705882353));
#157387=CARTESIAN_POINT('Ctrl Pts',(-8.07915007496071,16.2251205863895,
140.820588235294));
#157388=CARTESIAN_POINT('Ctrl Pts',(-6.51968959134574,16.8292587962898,
139.326470588235));
#157389=CARTESIAN_POINT('Ctrl Pts',(-4.96022910773078,17.4333970061901,
137.832352941177));
#157390=CARTESIAN_POINT('Ctrl Pts',(-3.31631129755346,17.7406985030951,
136.338235294118));
#157391=CARTESIAN_POINT('Ctrl Pts',(-1.67239348737615,18.048,134.844117647059));
#157392=CARTESIAN_POINT('Ctrl Pts',(-2.21024254310115E-15,18.048,133.35));
#157393=CARTESIAN_POINT('Ctrl Pts',(1.67239348737616,18.048,131.855882352941));
#157394=CARTESIAN_POINT('Ctrl Pts',(3.31631129755346,17.7406985030951,130.361764705882));
#157395=CARTESIAN_POINT('Ctrl Pts',(4.96022910773077,17.4333970061901,128.867647058824));
#157396=CARTESIAN_POINT('Ctrl Pts',(6.51968959134575,16.8292587962898,127.373529411765));
#157397=CARTESIAN_POINT('Ctrl Pts',(8.07915007496071,16.2251205863895,125.879411764706));
#157398=CARTESIAN_POINT('Ctrl Pts',(9.50104767561053,15.3447188656481,124.385294117647));
#157399=CARTESIAN_POINT('Ctrl Pts',(10.9229452762603,14.4643171449067,122.891176470588));
#157400=CARTESIAN_POINT('Ctrl Pts',(12.1588589765331,13.3376329379985,121.397058823529));
#157401=CARTESIAN_POINT('Ctrl Pts',(13.3947726768058,12.2109487310903,119.902941176471));
#157402=CARTESIAN_POINT('Ctrl Pts',(14.4026149179538,10.8763499173728,118.408823529412));
#157403=CARTESIAN_POINT('Ctrl Pts',(15.4104571591017,9.54175110365538,116.914705882353));
#157404=CARTESIAN_POINT('Ctrl Pts',(16.1559070823762,8.04468584505496,115.420588235294));
#157405=CARTESIAN_POINT('Ctrl Pts',(16.9013570056506,6.54762058645456,113.926470588235));
#157406=CARTESIAN_POINT('Ctrl Pts',(17.3590292079831,4.93906964482096,112.432352941177));
#157407=CARTESIAN_POINT('Ctrl Pts',(17.8167014103155,3.33051870318735,110.938235294118));
#157408=CARTESIAN_POINT('Ctrl Pts',(17.9710104137728,1.66525935159367,109.444117647059));
#157409=CARTESIAN_POINT('Ctrl Pts',(18.1253194172301,3.32956716117513E-15,
107.95));
#157410=CARTESIAN_POINT('Ctrl Pts',(17.9710104137728,-1.66525935159367,
106.455882352941));
#157411=CARTESIAN_POINT('Ctrl Pts',(17.8167014103155,-3.33051870318736,
104.961764705882));
#157412=CARTESIAN_POINT('Ctrl Pts',(17.3590292079831,-4.93906964482095,
103.467647058824));
#157413=CARTESIAN_POINT('Ctrl Pts',(16.9013570056506,-6.54762058645456,
101.973529411765));
#157414=CARTESIAN_POINT('Ctrl Pts',(16.1559070823762,-8.04468584505497,
100.479411764706));
#157415=CARTESIAN_POINT('Ctrl Pts',(15.4104571591017,-9.54175110365538,
98.985294117647));
#157416=CARTESIAN_POINT('Ctrl Pts',(14.4026149179538,-10.8763499173728,
97.4911764705884));
#157417=CARTESIAN_POINT('Ctrl Pts',(13.3947726768058,-12.2109487310903,
95.9970588235295));
#157418=CARTESIAN_POINT('Ctrl Pts',(12.1588589765331,-13.3376329379985,
94.5029411764706));
#157419=CARTESIAN_POINT('Ctrl Pts',(10.9229452762603,-14.4643171449067,
93.0088235294117));
#157420=CARTESIAN_POINT('Ctrl Pts',(9.50104767561053,-15.3447188656481,
91.5147058823529));
#157421=CARTESIAN_POINT('Ctrl Pts',(8.07915007496071,-16.2251205863895,
90.0205882352942));
#157422=CARTESIAN_POINT('Ctrl Pts',(6.51968959134574,-16.8292587962898,
88.5264705882354));
#157423=CARTESIAN_POINT('Ctrl Pts',(4.96022910773078,-17.4333970061901,
87.0323529411765));
#157424=CARTESIAN_POINT('Ctrl Pts',(3.31631129755346,-17.7406985030951,
85.5382352941176));
#157425=CARTESIAN_POINT('Ctrl Pts',(1.67239348737615,-18.048,84.0441176470588));
#157426=CARTESIAN_POINT('Ctrl Pts',(0.,-18.048,82.5500000000001));
#157427=CARTESIAN_POINT('Ctrl Pts',(-1.67239348737615,-18.048,81.0558823529413));
#157428=CARTESIAN_POINT('Ctrl Pts',(-3.31631129755346,-17.7406985030951,
79.5617647058824));
#157429=CARTESIAN_POINT('Ctrl Pts',(-4.96022910773077,-17.4333970061901,
78.0676470588235));
#157430=CARTESIAN_POINT('Ctrl Pts',(-6.51968959134574,-16.8292587962898,
76.5735294117647));
#157431=CARTESIAN_POINT('Ctrl Pts',(-8.07915007496071,-16.2251205863895,
75.079411764706));
#157432=CARTESIAN_POINT('Ctrl Pts',(-9.50104767561052,-15.3447188656481,
73.5852941176471));
#157433=CARTESIAN_POINT('Ctrl Pts',(-10.9229452762603,-14.4643171449067,
72.0911764705883));
#157434=CARTESIAN_POINT('Ctrl Pts',(-12.1588589765331,-13.3376329379985,
70.5970588235294));
#157435=CARTESIAN_POINT('Ctrl Pts',(-13.3947726768058,-12.2109487310903,
69.1029411764705));
#157436=CARTESIAN_POINT('Ctrl Pts',(-14.4026149179538,-10.8763499173728,
67.6088235294119));
#157437=CARTESIAN_POINT('Ctrl Pts',(-15.4104571591017,-9.54175110365538,
66.114705882353));
#157438=CARTESIAN_POINT('Ctrl Pts',(-16.1559070823762,-8.04468584505497,
64.6205882352942));
#157439=CARTESIAN_POINT('Ctrl Pts',(-16.9013570056506,-6.54762058645456,
63.1264705882353));
#157440=CARTESIAN_POINT('Ctrl Pts',(-17.3590292079831,-4.93906964482095,
61.6323529411764));
#157441=CARTESIAN_POINT('Ctrl Pts',(-17.8167014103155,-3.33051870318735,
60.1382352941178));
#157442=CARTESIAN_POINT('Ctrl Pts',(-17.9710104137728,-1.66525935159368,
58.6441176470589));
#157443=CARTESIAN_POINT('Ctrl Pts',(-18.1253194172301,-1.10985572039171E-15,
57.15));
#157444=CARTESIAN_POINT('Ctrl Pts',(-17.9710104137728,1.66525935159367,
55.6558823529412));
#157445=CARTESIAN_POINT('Ctrl Pts',(-17.8167014103155,3.33051870318735,
54.1617647058823));
#157446=CARTESIAN_POINT('Ctrl Pts',(-17.3590292079831,4.93906964482096,
52.6676470588237));
#157447=CARTESIAN_POINT('Ctrl Pts',(-16.9013570056506,6.54762058645456,
51.1735294117648));
#157448=CARTESIAN_POINT('Ctrl Pts',(-16.1559070823762,8.04468584505497,
49.6794117647059));
#157449=CARTESIAN_POINT('Ctrl Pts',(-15.4104571591017,9.54175110365538,
48.185294117647));
#157450=CARTESIAN_POINT('Ctrl Pts',(-14.4026149179538,10.8763499173728,
46.6911764705882));
#157451=CARTESIAN_POINT('Ctrl Pts',(-13.3947726768058,12.2109487310903,
45.1970588235295));
#157452=CARTESIAN_POINT('Ctrl Pts',(-12.1588589765331,13.3376329379985,
43.7029411764707));
#157453=CARTESIAN_POINT('Ctrl Pts',(-10.9229452762603,14.4643171449067,
42.2088235294118));
#157454=CARTESIAN_POINT('Ctrl Pts',(-9.50104767561052,15.3447188656481,
40.7147058823529));
#157455=CARTESIAN_POINT('Ctrl Pts',(-8.07915007496071,16.2251205863895,
39.2205882352941));
#157456=CARTESIAN_POINT('Ctrl Pts',(-6.51968959134574,16.8292587962898,
37.7264705882354));
#157457=CARTESIAN_POINT('Ctrl Pts',(-4.96022910773078,17.4333970061901,
36.2323529411766));
#157458=CARTESIAN_POINT('Ctrl Pts',(-3.31631129755346,17.7406985030951,
34.7382352941177));
#157459=CARTESIAN_POINT('Ctrl Pts',(-1.67239348737615,18.048,33.2441176470588));
#157460=CARTESIAN_POINT('Ctrl Pts',(-2.21024254310115E-15,18.048,31.7499999999999));
#157461=CARTESIAN_POINT('Ctrl Pts',(1.67239348737616,18.048,30.2558823529413));
#157462=CARTESIAN_POINT('Ctrl Pts',(3.31631129755346,17.7406985030951,28.7617647058824));
#157463=CARTESIAN_POINT('Ctrl Pts',(4.96022910773077,17.4333970061901,27.2676470588236));
#157464=CARTESIAN_POINT('Ctrl Pts',(6.51968959134575,16.8292587962898,25.7735294117647));
#157465=CARTESIAN_POINT('Ctrl Pts',(8.07915007496071,16.2251205863895,24.2794117647058));
#157466=CARTESIAN_POINT('Ctrl Pts',(9.50104767561053,15.3447188656481,22.7852941176472));
#157467=CARTESIAN_POINT('Ctrl Pts',(10.9229452762603,14.4643171449067,21.2911764705883));
#157468=CARTESIAN_POINT('Ctrl Pts',(12.1588589765331,13.3376329379985,19.7970588235294));
#157469=CARTESIAN_POINT('Ctrl Pts',(13.3947726768058,12.2109487310903,18.3029411764706));
#157470=CARTESIAN_POINT('Ctrl Pts',(14.4026149179538,10.8763499173728,16.8088235294117));
#157471=CARTESIAN_POINT('Ctrl Pts',(15.4104571591017,9.54175110365538,15.3147058823531));
#157472=CARTESIAN_POINT('Ctrl Pts',(16.1559070823762,8.04468584505496,13.8205882352942));
#157473=CARTESIAN_POINT('Ctrl Pts',(16.9013570056506,6.54762058645456,12.3264705882353));
#157474=CARTESIAN_POINT('Ctrl Pts',(17.3590292079831,4.93906964482096,10.8323529411765));
#157475=CARTESIAN_POINT('Ctrl Pts',(17.8167014103155,3.33051870318735,9.33823529411759));
#157476=CARTESIAN_POINT('Ctrl Pts',(17.9710104137728,1.66525935159367,7.84411764705895));
#157477=CARTESIAN_POINT('Ctrl Pts',(18.1253194172301,3.32956716117513E-15,
6.35000000000008));
#157478=CARTESIAN_POINT('Ctrl Pts',(17.9710104137728,-1.66525935159367,
4.85588235294121));
#157479=CARTESIAN_POINT('Ctrl Pts',(17.8167014103155,-3.33051870318736,
3.36176470588234));
#157480=CARTESIAN_POINT('Ctrl Pts',(17.3590292079831,-4.93906964482095,
1.86764705882347));
#157481=CARTESIAN_POINT('Ctrl Pts',(16.9013570056506,-6.54762058645456,
0.373529411764828));
#157482=CARTESIAN_POINT('Ctrl Pts',(16.1559070823762,-8.04468584505497,
-1.12058823529404));
#157483=CARTESIAN_POINT('Ctrl Pts',(15.4104571591017,-9.54175110365538,
-2.61470588235291));
#157484=CARTESIAN_POINT('Ctrl Pts',(14.4026149179538,-10.8763499173728,
-4.10882352941178));
#157485=CARTESIAN_POINT('Ctrl Pts',(13.3947726768058,-12.2109487310903,
-5.60294117647064));
#157486=CARTESIAN_POINT('Ctrl Pts',(12.1588589765331,-13.3376329379985,
-7.09705882352929));
#157487=CARTESIAN_POINT('Ctrl Pts',(10.9229452762603,-14.4643171449067,
-8.59117647058816));
#157488=CARTESIAN_POINT('Ctrl Pts',(9.50104767561053,-15.3447188656481,
-10.085294117647));
#157489=CARTESIAN_POINT('Ctrl Pts',(8.07915007496071,-16.2251205863895,
-11.5794117647059));
#157490=CARTESIAN_POINT('Ctrl Pts',(6.51968959134574,-16.8292587962898,
-13.0735294117648));
#157491=CARTESIAN_POINT('Ctrl Pts',(4.96022910773078,-17.4333970061901,
-14.5676470588234));
#157492=CARTESIAN_POINT('Ctrl Pts',(3.31631129755346,-17.7406985030951,
-16.0617647058823));
#157493=CARTESIAN_POINT('Ctrl Pts',(1.67239348737615,-18.048,-17.5558823529411));
#157494=CARTESIAN_POINT('Ctrl Pts',(0.,-18.048,-19.05));
#157495=CARTESIAN_POINT('Ctrl Pts',(-1.67239348737615,-18.048,-20.5441176470589));
#157496=CARTESIAN_POINT('Ctrl Pts',(-3.31631129755346,-17.7406985030951,
-22.0382352941175));
#157497=CARTESIAN_POINT('Ctrl Pts',(-4.96022910773077,-17.4333970061901,
-23.5323529411764));
#157498=CARTESIAN_POINT('Ctrl Pts',(-6.51968959134574,-16.8292587962898,
-25.0264705882353));
#157499=CARTESIAN_POINT('Ctrl Pts',(-8.07915007496071,-16.2251205863895,
-26.5205882352941));
#157500=CARTESIAN_POINT('Ctrl Pts',(-9.50104767561052,-15.3447188656481,
-28.014705882353));
#157501=CARTESIAN_POINT('Ctrl Pts',(-10.9229452762603,-14.4643171449067,
-29.5088235294116));
#157502=CARTESIAN_POINT('Ctrl Pts',(-12.1588589765331,-13.3376329379985,
-31.0029411764705));
#157503=CARTESIAN_POINT('Ctrl Pts',(-13.3947726768058,-12.2109487310903,
-32.4970588235294));
#157504=CARTESIAN_POINT('Ctrl Pts',(-14.4026149179538,-10.8763499173728,
-33.9911764705882));
#157505=CARTESIAN_POINT('Ctrl Pts',(-15.4104571591017,-9.54175110365538,
-35.4852941176471));
#157506=CARTESIAN_POINT('Ctrl Pts',(-16.1559070823762,-8.04468584505497,
-36.9794117647058));
#157507=CARTESIAN_POINT('Ctrl Pts',(-16.9013570056506,-6.54762058645456,
-38.4735294117646));
#157508=CARTESIAN_POINT('Ctrl Pts',(-17.3590292079831,-4.93906964482095,
-39.9676470588235));
#157509=CARTESIAN_POINT('Ctrl Pts',(-17.8167014103155,-3.33051870318735,
-41.4617647058824));
#157510=CARTESIAN_POINT('Ctrl Pts',(-17.9710104137728,-1.66525935159368,
-42.9558823529412));
#157511=CARTESIAN_POINT('Ctrl Pts',(-18.1253194172301,-1.10985572039171E-15,
-44.4499999999999));
#157512=CARTESIAN_POINT('Ctrl Pts',(-17.9710104137728,1.66525935159367,
-45.9441176470587));
#157513=CARTESIAN_POINT('Ctrl Pts',(-17.8167014103155,3.33051870318735,
-47.4382352941176));
#157514=CARTESIAN_POINT('Ctrl Pts',(-17.3590292079831,4.93906964482096,
-48.9323529411765));
#157515=CARTESIAN_POINT('Ctrl Pts',(-16.9013570056506,6.54762058645456,
-50.4264705882354));
#157516=CARTESIAN_POINT('Ctrl Pts',(-16.1559070823762,8.04468584505497,
-51.920588235294));
#157517=CARTESIAN_POINT('Ctrl Pts',(-15.4104571591017,9.54175110365538,
-53.4147058823529));
#157518=CARTESIAN_POINT('Ctrl Pts',(-14.4026149179538,10.8763499173728,
-54.9088235294117));
#157519=CARTESIAN_POINT('Ctrl Pts',(-13.3947726768058,12.2109487310903,
-56.4029411764706));
#157520=CARTESIAN_POINT('Ctrl Pts',(-12.1588589765331,13.3376329379985,
-57.8970588235295));
#157521=CARTESIAN_POINT('Ctrl Pts',(-10.9229452762603,14.4643171449067,
-59.3911764705881));
#157522=CARTESIAN_POINT('Ctrl Pts',(-9.50104767561052,15.3447188656481,
-60.885294117647));
#157523=CARTESIAN_POINT('Ctrl Pts',(-8.07915007496071,16.2251205863895,
-62.3794117647059));
#157524=CARTESIAN_POINT('Ctrl Pts',(-6.51968959134574,16.8292587962898,
-63.8735294117647));
#157525=CARTESIAN_POINT('Ctrl Pts',(-4.96022910773078,17.4333970061901,
-65.3676470588236));
#157526=CARTESIAN_POINT('Ctrl Pts',(-3.31631129755346,17.7406985030951,
-66.8617647058822));
#157527=CARTESIAN_POINT('Ctrl Pts',(-1.67239348737615,18.048,-68.3558823529411));
#157528=CARTESIAN_POINT('Ctrl Pts',(-2.21024254310115E-15,18.048,-69.85));
#157529=CARTESIAN_POINT('Ctrl Pts',(1.67239348737616,18.048,-71.3441176470589));
#157530=CARTESIAN_POINT('Ctrl Pts',(3.31631129755346,17.7406985030951,-72.8382352941177));
#157531=CARTESIAN_POINT('Ctrl Pts',(4.96022910773077,17.4333970061901,-74.3323529411764));
#157532=CARTESIAN_POINT('Ctrl Pts',(6.51968959134575,16.8292587962898,-75.8264705882352));
#157533=CARTESIAN_POINT('Ctrl Pts',(8.07915007496071,16.2251205863895,-77.3205882352941));
#157534=CARTESIAN_POINT('Ctrl Pts',(9.50104767561053,15.3447188656481,-78.814705882353));
#157535=CARTESIAN_POINT('Ctrl Pts',(10.9229452762603,14.4643171449067,-80.3088235294118));
#157536=CARTESIAN_POINT('Ctrl Pts',(12.1588589765331,13.3376329379985,-81.8029411764705));
#157537=CARTESIAN_POINT('Ctrl Pts',(13.3947726768058,12.2109487310903,-83.2970588235294));
#157538=CARTESIAN_POINT('Ctrl Pts',(14.4026149179538,10.8763499173728,-84.7911764705882));
#157539=CARTESIAN_POINT('Ctrl Pts',(15.4104571591017,9.54175110365538,-86.2852941176471));
#157540=CARTESIAN_POINT('Ctrl Pts',(16.1559070823762,8.04468584505496,-87.7794117647059));
#157541=CARTESIAN_POINT('Ctrl Pts',(16.9013570056506,6.54762058645456,-89.2735294117646));
#157542=CARTESIAN_POINT('Ctrl Pts',(17.3590292079831,4.93906964482096,-90.7676470588235));
#157543=CARTESIAN_POINT('Ctrl Pts',(17.8167014103155,3.33051870318735,-92.2617647058823));
#157544=CARTESIAN_POINT('Ctrl Pts',(17.9710104137728,1.66525935159367,-93.7558823529412));
#157545=CARTESIAN_POINT('Ctrl Pts',(18.1253194172301,3.32956716117513E-15,
-95.2500000000001));
#157546=CARTESIAN_POINT('Ctrl Pts',(17.9710104137728,-1.66525935159367,
-96.7441176470587));
#157547=CARTESIAN_POINT('Ctrl Pts',(17.8167014103155,-3.33051870318736,
-98.2382352941176));
#157548=CARTESIAN_POINT('Ctrl Pts',(17.3590292079831,-4.93906964482095,
-99.7323529411764));
#157549=CARTESIAN_POINT('Ctrl Pts',(16.9013570056506,-6.54762058645456,
-101.226470588235));
#157550=CARTESIAN_POINT('Ctrl Pts',(16.1559070823762,-8.04468584505497,
-102.720588235294));
#157551=CARTESIAN_POINT('Ctrl Pts',(15.4104571591017,-9.54175110365538,
-104.214705882353));
#157552=CARTESIAN_POINT('Ctrl Pts',(14.4026149179538,-10.8763499173728,
-105.708823529412));
#157553=CARTESIAN_POINT('Ctrl Pts',(13.3947726768058,-12.2109487310903,
-107.202941176471));
#157554=CARTESIAN_POINT('Ctrl Pts',(12.1588589765331,-13.3376329379985,
-108.697058823529));
#157555=CARTESIAN_POINT('Ctrl Pts',(10.9229452762603,-14.4643171449067,
-110.191176470588));
#157556=CARTESIAN_POINT('Ctrl Pts',(9.50104767561053,-15.3447188656481,
-111.685294117647));
#157557=CARTESIAN_POINT('Ctrl Pts',(8.07915007496071,-16.2251205863895,
-113.179411764706));
#157558=CARTESIAN_POINT('Ctrl Pts',(6.51968959134574,-16.8292587962898,
-114.673529411765));
#157559=CARTESIAN_POINT('Ctrl Pts',(4.96022910773078,-17.4333970061901,
-116.167647058824));
#157560=CARTESIAN_POINT('Ctrl Pts',(3.31631129755346,-17.7406985030951,
-117.661764705882));
#157561=CARTESIAN_POINT('Ctrl Pts',(1.67239348737615,-18.048,-119.155882352941));
#157562=CARTESIAN_POINT('Ctrl Pts',(0.,-18.048,-120.65));
#157563=CARTESIAN_POINT('Ctrl Pts',(-1.67239348737615,-18.048,-122.144117647059));
#157564=CARTESIAN_POINT('Ctrl Pts',(-3.31631129755346,-17.7406985030951,
-123.638235294118));
#157565=CARTESIAN_POINT('Ctrl Pts',(-4.96022910773077,-17.4333970061901,
-125.132352941177));
#157566=CARTESIAN_POINT('Ctrl Pts',(-6.51968959134574,-16.8292587962898,
-126.626470588235));
#157567=CARTESIAN_POINT('Ctrl Pts',(-8.07915007496071,-16.2251205863895,
-128.120588235294));
#157568=CARTESIAN_POINT('Ctrl Pts',(-9.50104767561052,-15.3447188656481,
-129.614705882353));
#157569=CARTESIAN_POINT('Ctrl Pts',(-10.9229452762603,-14.4643171449067,
-131.108823529412));
#157570=CARTESIAN_POINT('Ctrl Pts',(-12.1588589765331,-13.3376329379985,
-132.602941176471));
#157571=CARTESIAN_POINT('Ctrl Pts',(-13.3947726768058,-12.2109487310903,
-134.097058823529));
#157572=CARTESIAN_POINT('Ctrl Pts',(-14.4026149179538,-10.8763499173728,
-135.591176470588));
#157573=CARTESIAN_POINT('Ctrl Pts',(-15.4104571591017,-9.54175110365538,
-137.085294117647));
#157574=CARTESIAN_POINT('Ctrl Pts',(-16.1559070823762,-8.04468584505497,
-138.579411764706));
#157575=CARTESIAN_POINT('Ctrl Pts',(-16.9013570056506,-6.54762058645456,
-140.073529411765));
#157576=CARTESIAN_POINT('Ctrl Pts',(-17.3590292079831,-4.93906964482095,
-141.567647058823));
#157577=CARTESIAN_POINT('Ctrl Pts',(-17.8167014103155,-3.33051870318735,
-143.061764705882));
#157578=CARTESIAN_POINT('Ctrl Pts',(-17.9710104137728,-1.66525935159368,
-144.555882352941));
#157579=CARTESIAN_POINT('Ctrl Pts',(-18.1253194172301,-1.10985572039171E-15,
-146.05));
#157580=CARTESIAN_POINT('Ctrl Pts',(-17.9710104137728,1.66525935159367,
-147.544117647059));
#157581=CARTESIAN_POINT('Ctrl Pts',(-17.8167014103155,3.33051870318735,
-149.038235294118));
#157582=CARTESIAN_POINT('Ctrl Pts',(-17.3590292079831,4.93906964482096,
-150.532352941176));
#157583=CARTESIAN_POINT('Ctrl Pts',(-16.9013570056506,6.54762058645456,
-152.026470588235));
#157584=CARTESIAN_POINT('Ctrl Pts',(-16.1559070823762,8.04468584505497,
-153.520588235294));
#157585=CARTESIAN_POINT('Ctrl Pts',(-15.4104571591017,9.54175110365538,
-155.014705882353));
#157586=CARTESIAN_POINT('Ctrl Pts',(-14.4026149179538,10.8763499173728,
-156.508823529412));
#157587=CARTESIAN_POINT('Ctrl Pts',(-13.3947726768058,12.2109487310903,
-158.002941176471));
#157588=CARTESIAN_POINT('Ctrl Pts',(-12.1588589765331,13.3376329379985,
-159.497058823529));
#157589=CARTESIAN_POINT('Ctrl Pts',(-10.9229452762603,14.4643171449067,
-160.991176470588));
#157590=CARTESIAN_POINT('Ctrl Pts',(-9.50104767561052,15.3447188656481,
-162.485294117647));
#157591=CARTESIAN_POINT('Ctrl Pts',(-8.07915007496071,16.2251205863895,
-163.979411764706));
#157592=CARTESIAN_POINT('Ctrl Pts',(-6.51968959134574,16.8292587962898,
-165.473529411765));
#157593=CARTESIAN_POINT('Ctrl Pts',(-4.96022910773078,17.4333970061901,
-166.967647058824));
#157594=CARTESIAN_POINT('Ctrl Pts',(-3.31631129755346,17.7406985030951,
-168.461764705882));
#157595=CARTESIAN_POINT('Ctrl Pts',(-1.67239348737615,18.048,-169.955882352941));
#157596=CARTESIAN_POINT('Ctrl Pts',(-2.21024254310115E-15,18.048,-171.45));
#157597=CARTESIAN_POINT('Ctrl Pts',(1.67239348737616,18.048,-172.944117647059));
#157598=CARTESIAN_POINT('Ctrl Pts',(3.31631129755346,17.7406985030951,-174.438235294118));
#157599=CARTESIAN_POINT('Ctrl Pts',(4.96022910773077,17.4333970061901,-175.932352941176));
#157600=CARTESIAN_POINT('Ctrl Pts',(6.51968959134575,16.8292587962898,-177.426470588235));
#157601=CARTESIAN_POINT('Ctrl Pts',(8.07915007496071,16.2251205863895,-178.920588235294));
#157602=CARTESIAN_POINT('Ctrl Pts',(9.50104767561053,15.3447188656481,-180.414705882353));
#157603=CARTESIAN_POINT('Ctrl Pts',(10.9229452762603,14.4643171449067,-181.908823529412));
#157604=CARTESIAN_POINT('Ctrl Pts',(12.1588589765331,13.3376329379985,-183.402941176471));
#157605=CARTESIAN_POINT('Ctrl Pts',(13.3947726768058,12.2109487310903,-184.897058823529));
#157606=CARTESIAN_POINT('Ctrl Pts',(14.4026149179538,10.8763499173728,-186.391176470588));
#157607=CARTESIAN_POINT('Ctrl Pts',(15.4104571591017,9.54175110365538,-187.885294117647));
#157608=CARTESIAN_POINT('Ctrl Pts',(16.1559070823762,8.04468584505496,-189.379411764706));
#157609=CARTESIAN_POINT('Ctrl Pts',(16.9013570056506,6.54762058645456,-190.873529411765));
#157610=CARTESIAN_POINT('Ctrl Pts',(17.3590292079831,4.93906964482096,-192.367647058824));
#157611=CARTESIAN_POINT('Ctrl Pts',(17.8167014103155,3.33051870318735,-193.861764705882));
#157612=CARTESIAN_POINT('Ctrl Pts',(17.9710104137728,1.66525935159367,-195.355882352941));
#157613=CARTESIAN_POINT('Ctrl Pts',(18.1253194172301,3.32956716117513E-15,
-196.85));
#157614=CARTESIAN_POINT('Ctrl Pts',(17.9710104137728,-1.66525935159367,
-198.344117647059));
#157615=CARTESIAN_POINT('Ctrl Pts',(17.8167014103155,-3.33051870318736,
-199.838235294118));
#157616=CARTESIAN_POINT('Ctrl Pts',(17.3590292079831,-4.93906964482095,
-201.332352941176));
#157617=CARTESIAN_POINT('Ctrl Pts',(16.9013570056506,-6.54762058645456,
-202.826470588235));
#157618=CARTESIAN_POINT('Ctrl Pts',(16.1559070823762,-8.04468584505497,
-204.320588235294));
#157619=CARTESIAN_POINT('Ctrl Pts',(15.4104571591017,-9.54175110365538,
-205.814705882353));
#157620=CARTESIAN_POINT('Ctrl Pts',(14.4026149179538,-10.8763499173728,
-207.308823529412));
#157621=CARTESIAN_POINT('Ctrl Pts',(13.3947726768058,-12.2109487310903,
-208.80294117647));
#157622=CARTESIAN_POINT('Ctrl Pts',(12.1588589765331,-13.3376329379985,
-210.297058823529));
#157623=CARTESIAN_POINT('Ctrl Pts',(10.9229452762603,-14.4643171449067,
-211.791176470588));
#157624=CARTESIAN_POINT('Ctrl Pts',(9.50104767561053,-15.3447188656481,
-213.285294117647));
#157625=CARTESIAN_POINT('Ctrl Pts',(8.07915007496071,-16.2251205863895,
-214.779411764706));
#157626=CARTESIAN_POINT('Ctrl Pts',(6.51968959134574,-16.8292587962898,
-216.273529411765));
#157627=CARTESIAN_POINT('Ctrl Pts',(4.96022910773078,-17.4333970061901,
-217.767647058823));
#157628=CARTESIAN_POINT('Ctrl Pts',(3.31631129755346,-17.7406985030951,
-219.261764705882));
#157629=CARTESIAN_POINT('Ctrl Pts',(1.67239348737615,-18.048,-220.755882352941));
#157630=CARTESIAN_POINT('Ctrl Pts',(0.,-18.048,-222.25));
#157631=CARTESIAN_POINT('Ctrl Pts',(-1.67239348737615,-18.048,-223.744117647059));
#157632=CARTESIAN_POINT('Ctrl Pts',(-3.31631129755346,-17.7406985030951,
-225.238235294118));
#157633=CARTESIAN_POINT('Ctrl Pts',(-4.96022910773077,-17.4333970061901,
-226.732352941176));
#157634=CARTESIAN_POINT('Ctrl Pts',(-6.51968959134574,-16.8292587962898,
-228.226470588235));
#157635=CARTESIAN_POINT('Ctrl Pts',(-8.07915007496071,-16.2251205863895,
-229.720588235294));
#157636=CARTESIAN_POINT('Ctrl Pts',(-9.50104767561052,-15.3447188656481,
-231.214705882353));
#157637=CARTESIAN_POINT('Ctrl Pts',(-10.9229452762603,-14.4643171449067,
-232.708823529412));
#157638=CARTESIAN_POINT('Ctrl Pts',(-12.1588589765331,-13.3376329379985,
-234.202941176471));
#157639=CARTESIAN_POINT('Ctrl Pts',(-13.3947726768058,-12.2109487310903,
-235.697058823529));
#157640=CARTESIAN_POINT('Ctrl Pts',(-14.4026149179538,-10.8763499173728,
-237.191176470588));
#157641=CARTESIAN_POINT('Ctrl Pts',(-15.4104571591017,-9.54175110365538,
-238.685294117647));
#157642=CARTESIAN_POINT('Ctrl Pts',(-16.1559070823762,-8.04468584505497,
-240.179411764706));
#157643=CARTESIAN_POINT('Ctrl Pts',(-16.9013570056506,-6.54762058645456,
-241.673529411765));
#157644=CARTESIAN_POINT('Ctrl Pts',(-17.3590292079831,-4.93906964482095,
-243.167647058824));
#157645=CARTESIAN_POINT('Ctrl Pts',(-17.8167014103155,-3.33051870318735,
-244.661764705882));
#157646=CARTESIAN_POINT('Ctrl Pts',(-17.9710104137728,-1.66525935159368,
-246.155882352941));
#157647=CARTESIAN_POINT('Ctrl Pts',(-18.1253194172301,-1.10985572039171E-15,
-247.65));
#157648=CARTESIAN_POINT('Ctrl Pts',(-17.9710104137728,1.66525935159367,
-249.144117647059));
#157649=CARTESIAN_POINT('Ctrl Pts',(-17.8167014103155,3.33051870318735,
-250.638235294118));
#157650=CARTESIAN_POINT('Ctrl Pts',(-17.3590292079831,4.93906964482096,
-252.132352941177));
#157651=CARTESIAN_POINT('Ctrl Pts',(-16.9013570056506,6.54762058645456,
-253.626470588235));
#157652=CARTESIAN_POINT('Ctrl Pts',(-16.1559070823762,8.04468584505497,
-255.120588235294));
#157653=CARTESIAN_POINT('Ctrl Pts',(-15.4104571591017,9.54175110365538,
-256.614705882353));
#157654=CARTESIAN_POINT('Ctrl Pts',(-14.4026149179538,10.8763499173728,
-258.108823529412));
#157655=CARTESIAN_POINT('Ctrl Pts',(-13.3947726768058,12.2109487310903,
-259.602941176471));
#157656=CARTESIAN_POINT('Ctrl Pts',(-12.1588589765331,13.3376329379985,
-261.097058823529));
#157657=CARTESIAN_POINT('Ctrl Pts',(-10.9229452762603,14.4643171449067,
-262.591176470588));
#157658=CARTESIAN_POINT('Ctrl Pts',(-9.50104767561052,15.3447188656481,
-264.085294117647));
#157659=CARTESIAN_POINT('Ctrl Pts',(-8.07915007496071,16.2251205863895,
-265.579411764706));
#157660=CARTESIAN_POINT('Ctrl Pts',(-6.51968959134574,16.8292587962898,
-267.073529411765));
#157661=CARTESIAN_POINT('Ctrl Pts',(-4.96022910773078,17.4333970061901,
-268.567647058823));
#157662=CARTESIAN_POINT('Ctrl Pts',(-3.31631129755346,17.7406985030951,
-270.061764705882));
#157663=CARTESIAN_POINT('Ctrl Pts',(-1.67239348737615,18.048,-271.555882352941));
#157664=CARTESIAN_POINT('Ctrl Pts',(-2.21024254310115E-15,18.048,-273.05));
#157665=CARTESIAN_POINT('Ctrl Pts',(1.67239348737616,18.048,-274.544117647059));
#157666=CARTESIAN_POINT('Ctrl Pts',(3.31631129755346,17.7406985030951,-276.038235294118));
#157667=CARTESIAN_POINT('Ctrl Pts',(4.96022910773077,17.4333970061901,-277.532352941176));
#157668=CARTESIAN_POINT('Ctrl Pts',(6.51968959134575,16.8292587962898,-279.026470588235));
#157669=CARTESIAN_POINT('Ctrl Pts',(8.07915007496071,16.2251205863895,-280.520588235294));
#157670=CARTESIAN_POINT('Ctrl Pts',(9.50104767561053,15.3447188656481,-282.014705882353));
#157671=CARTESIAN_POINT('Ctrl Pts',(10.9229452762603,14.4643171449067,-283.508823529412));
#157672=CARTESIAN_POINT('Ctrl Pts',(12.1588589765331,13.3376329379985,-285.002941176471));
#157673=CARTESIAN_POINT('Ctrl Pts',(13.3947726768058,12.2109487310903,-286.497058823529));
#157674=CARTESIAN_POINT('Ctrl Pts',(14.4026149179538,10.8763499173728,-287.991176470588));
#157675=CARTESIAN_POINT('Ctrl Pts',(15.4104571591017,9.54175110365538,-289.485294117647));
#157676=CARTESIAN_POINT('Ctrl Pts',(16.1559070823762,8.04468584505496,-290.979411764706));
#157677=CARTESIAN_POINT('Ctrl Pts',(16.9013570056506,6.54762058645456,-292.473529411765));
#157678=CARTESIAN_POINT('Ctrl Pts',(17.3590292079831,4.93906964482096,-293.967647058824));
#157679=CARTESIAN_POINT('Ctrl Pts',(17.8167014103155,3.33051870318735,-295.461764705882));
#157680=CARTESIAN_POINT('Ctrl Pts',(17.9710104137728,1.66525935159367,-296.955882352941));
#157681=CARTESIAN_POINT('Ctrl Pts',(18.1253194172301,3.32956716117513E-15,
-298.45));
#157682=CARTESIAN_POINT('Ctrl Pts',(17.9710104137728,-1.66525935159367,
-299.944117647059));
#157683=CARTESIAN_POINT('Ctrl Pts',(17.8167014103155,-3.33051870318736,
-301.438235294118));
#157684=CARTESIAN_POINT('Ctrl Pts',(17.3590292079831,-4.93906964482095,
-302.932352941177));
#157685=CARTESIAN_POINT('Ctrl Pts',(16.9013570056506,-6.54762058645456,
-304.426470588235));
#157686=CARTESIAN_POINT('Ctrl Pts',(16.1559070823762,-8.04468584505497,
-305.920588235294));
#157687=CARTESIAN_POINT('Ctrl Pts',(15.4104571591017,-9.54175110365538,
-307.414705882353));
#157688=CARTESIAN_POINT('Ctrl Pts',(14.4026149179538,-10.8763499173728,
-308.908823529412));
#157689=CARTESIAN_POINT('Ctrl Pts',(13.3947726768058,-12.2109487310903,
-310.402941176471));
#157690=CARTESIAN_POINT('Ctrl Pts',(12.1588589765331,-13.3376329379985,
-311.897058823529));
#157691=CARTESIAN_POINT('Ctrl Pts',(10.9229452762603,-14.4643171449067,
-313.391176470588));
#157692=CARTESIAN_POINT('Ctrl Pts',(9.50104767561053,-15.3447188656481,
-314.885294117647));
#157693=CARTESIAN_POINT('Ctrl Pts',(8.07915007496071,-16.2251205863895,
-316.379411764706));
#157694=CARTESIAN_POINT('Ctrl Pts',(6.51968959134574,-16.8292587962898,
-317.873529411765));
#157695=CARTESIAN_POINT('Ctrl Pts',(4.96022910773078,-17.4333970061901,
-319.367647058824));
#157696=CARTESIAN_POINT('Ctrl Pts',(3.31631129755346,-17.7406985030951,
-320.861764705882));
#157697=CARTESIAN_POINT('Ctrl Pts',(1.67239348737615,-18.048,-322.355882352941));
#157698=CARTESIAN_POINT('Ctrl Pts',(0.,-18.048,-323.85));
#157699=CARTESIAN_POINT('Ctrl Pts',(-1.67239348737615,-18.048,-325.344117647059));
#157700=CARTESIAN_POINT('Ctrl Pts',(-3.31631129755346,-17.7406985030951,
-326.838235294118));
#157701=CARTESIAN_POINT('Ctrl Pts',(-4.96022910773077,-17.4333970061901,
-328.332352941176));
#157702=CARTESIAN_POINT('Ctrl Pts',(-6.51968959134574,-16.8292587962898,
-329.826470588235));
#157703=CARTESIAN_POINT('Ctrl Pts',(-8.07915007496071,-16.2251205863895,
-331.320588235294));
#157704=CARTESIAN_POINT('Ctrl Pts',(-9.50104767561052,-15.3447188656481,
-332.814705882353));
#157705=CARTESIAN_POINT('Ctrl Pts',(-10.9229452762603,-14.4643171449067,
-334.308823529412));
#157706=CARTESIAN_POINT('Ctrl Pts',(-12.1588589765331,-13.3376329379985,
-335.80294117647));
#157707=CARTESIAN_POINT('Ctrl Pts',(-13.3947726768058,-12.2109487310903,
-337.297058823529));
#157708=CARTESIAN_POINT('Ctrl Pts',(-14.4026149179538,-10.8763499173728,
-338.791176470588));
#157709=CARTESIAN_POINT('Ctrl Pts',(-15.4104571591017,-9.54175110365538,
-340.285294117647));
#157710=CARTESIAN_POINT('Ctrl Pts',(-16.1559070823762,-8.04468584505497,
-341.779411764706));
#157711=CARTESIAN_POINT('Ctrl Pts',(-16.9013570056506,-6.54762058645456,
-343.273529411765));
#157712=CARTESIAN_POINT('Ctrl Pts',(-17.3590292079831,-4.93906964482095,
-344.767647058823));
#157713=CARTESIAN_POINT('Ctrl Pts',(-17.8167014103155,-3.33051870318735,
-346.261764705882));
#157714=CARTESIAN_POINT('Ctrl Pts',(-17.9710104137728,-1.66525935159368,
-347.755882352941));
#157715=CARTESIAN_POINT('Ctrl Pts',(-18.1253194172301,-1.10985572039171E-15,
-349.25));
#157716=CARTESIAN_POINT('Ctrl Pts',(-17.9710104137728,1.66525935159367,
-350.744117647059));
#157717=CARTESIAN_POINT('Ctrl Pts',(-17.8167014103155,3.33051870318735,
-352.238235294118));
#157718=CARTESIAN_POINT('Ctrl Pts',(-17.3590292079831,4.93906964482096,
-353.732352941176));
#157719=CARTESIAN_POINT('Ctrl Pts',(-16.9013570056506,6.54762058645456,
-355.226470588235));
#157720=CARTESIAN_POINT('Ctrl Pts',(-16.1559070823762,8.04468584505497,
-356.720588235294));
#157721=CARTESIAN_POINT('Ctrl Pts',(-15.4104571591017,9.54175110365538,
-358.214705882353));
#157722=CARTESIAN_POINT('Ctrl Pts',(-14.4026149179538,10.8763499173728,
-359.708823529412));
#157723=CARTESIAN_POINT('Ctrl Pts',(-13.3947726768058,12.2109487310903,
-361.202941176471));
#157724=CARTESIAN_POINT('Ctrl Pts',(-12.1588589765331,13.3376329379985,
-362.697058823529));
#157725=CARTESIAN_POINT('Ctrl Pts',(-10.9229452762603,14.4643171449067,
-364.191176470588));
#157726=CARTESIAN_POINT('Ctrl Pts',(-9.50104767561052,15.3447188656481,
-365.685294117647));
#157727=CARTESIAN_POINT('Ctrl Pts',(-8.07915007496071,16.2251205863895,
-367.179411764706));
#157728=CARTESIAN_POINT('Ctrl Pts',(-6.51968959134574,16.8292587962898,
-368.673529411765));
#157729=CARTESIAN_POINT('Ctrl Pts',(-4.96022910773078,17.4333970061901,
-370.167647058824));
#157730=CARTESIAN_POINT('Ctrl Pts',(-3.31631129755346,17.7406985030951,
-371.661764705882));
#157731=CARTESIAN_POINT('Ctrl Pts',(-1.67239348737615,18.048,-373.155882352941));
#157732=CARTESIAN_POINT('Ctrl Pts',(-2.21024254310115E-15,18.048,-374.65));
#157733=CARTESIAN_POINT('Ctrl Pts',(1.67239348737616,18.048,-376.144117647059));
#157734=CARTESIAN_POINT('Ctrl Pts',(3.31631129755346,17.7406985030951,-377.638235294118));
#157735=CARTESIAN_POINT('Ctrl Pts',(4.96022910773077,17.4333970061901,-379.132352941177));
#157736=CARTESIAN_POINT('Ctrl Pts',(6.51968959134575,16.8292587962898,-380.626470588235));
#157737=CARTESIAN_POINT('Ctrl Pts',(8.07915007496071,16.2251205863895,-382.120588235294));
#157738=CARTESIAN_POINT('Ctrl Pts',(9.50104767561053,15.3447188656481,-383.614705882353));
#157739=CARTESIAN_POINT('Ctrl Pts',(10.9229452762603,14.4643171449067,-385.108823529412));
#157740=CARTESIAN_POINT('Ctrl Pts',(12.1588589765331,13.3376329379985,-386.602941176471));
#157741=CARTESIAN_POINT('Ctrl Pts',(13.3947726768058,12.2109487310903,-388.097058823529));
#157742=CARTESIAN_POINT('Ctrl Pts',(14.4026149179538,10.8763499173728,-389.591176470588));
#157743=CARTESIAN_POINT('Ctrl Pts',(15.4104571591017,9.54175110365538,-391.085294117647));
#157744=CARTESIAN_POINT('Ctrl Pts',(16.1559070823762,8.04468584505496,-392.579411764706));
#157745=CARTESIAN_POINT('Ctrl Pts',(16.9013570056506,6.54762058645456,-394.073529411765));
#157746=CARTESIAN_POINT('Ctrl Pts',(17.3590292079831,4.93906964482096,-395.567647058823));
#157747=CARTESIAN_POINT('Ctrl Pts',(17.8167014103155,3.33051870318735,-397.061764705882));
#157748=CARTESIAN_POINT('Ctrl Pts',(17.9710104137728,1.66525935159367,-398.555882352941));
#157749=CARTESIAN_POINT('Ctrl Pts',(18.1253194172301,3.32956716117513E-15,
-400.05));
#157750=CARTESIAN_POINT('Ctrl Pts',(17.9710104137728,-1.66525935159367,
-401.544117647059));
#157751=CARTESIAN_POINT('Ctrl Pts',(17.8167014103155,-3.33051870318736,
-403.038235294118));
#157752=CARTESIAN_POINT('Ctrl Pts',(17.3590292079831,-4.93906964482095,
-404.532352941176));
#157753=CARTESIAN_POINT('Ctrl Pts',(16.9013570056506,-6.54762058645456,
-406.026470588235));
#157754=CARTESIAN_POINT('Ctrl Pts',(16.1559070823762,-8.04468584505497,
-407.520588235294));
#157755=CARTESIAN_POINT('Ctrl Pts',(15.4104571591017,-9.54175110365538,
-409.014705882353));
#157756=CARTESIAN_POINT('Ctrl Pts',(14.4026149179538,-10.8763499173728,
-410.508823529412));
#157757=CARTESIAN_POINT('Ctrl Pts',(13.3947726768058,-12.2109487310903,
-412.002941176471));
#157758=CARTESIAN_POINT('Ctrl Pts',(12.1588589765331,-13.3376329379985,
-413.497058823529));
#157759=CARTESIAN_POINT('Ctrl Pts',(10.9229452762603,-14.4643171449067,
-414.991176470588));
#157760=CARTESIAN_POINT('Ctrl Pts',(9.50104767561053,-15.3447188656481,
-416.485294117647));
#157761=CARTESIAN_POINT('Ctrl Pts',(8.07915007496071,-16.2251205863895,
-417.979411764706));
#157762=CARTESIAN_POINT('Ctrl Pts',(6.51968959134574,-16.8292587962898,
-419.473529411765));
#157763=CARTESIAN_POINT('Ctrl Pts',(4.96022910773078,-17.4333970061901,
-420.967647058824));
#157764=CARTESIAN_POINT('Ctrl Pts',(3.31631129755346,-17.7406985030951,
-422.461764705882));
#157765=CARTESIAN_POINT('Ctrl Pts',(1.67239348737615,-18.048,-423.955882352941));
#157766=CARTESIAN_POINT('Ctrl Pts',(0.,-18.048,-425.45));
#157767=CARTESIAN_POINT('Ctrl Pts',(-1.67239348737615,-18.048,-426.944117647059));
#157768=CARTESIAN_POINT('Ctrl Pts',(-3.31631129755346,-17.7406985030951,
-428.438235294118));
#157769=CARTESIAN_POINT('Ctrl Pts',(-4.96022910773077,-17.4333970061901,
-429.932352941177));
#157770=CARTESIAN_POINT('Ctrl Pts',(-6.51968959134574,-16.8292587962898,
-431.426470588235));
#157771=CARTESIAN_POINT('Ctrl Pts',(-8.07915007496071,-16.2251205863895,
-432.920588235294));
#157772=CARTESIAN_POINT('Ctrl Pts',(-9.50104767561052,-15.3447188656481,
-434.414705882353));
#157773=CARTESIAN_POINT('Ctrl Pts',(-10.9229452762603,-14.4643171449067,
-435.908823529412));
#157774=CARTESIAN_POINT('Ctrl Pts',(-12.1588589765331,-13.3376329379985,
-437.402941176471));
#157775=CARTESIAN_POINT('Ctrl Pts',(-13.3947726768058,-12.2109487310903,
-438.89705882353));
#157776=CARTESIAN_POINT('Ctrl Pts',(-14.4026149179538,-10.8763499173728,
-440.391176470588));
#157777=CARTESIAN_POINT('Ctrl Pts',(-15.4104571591017,-9.54175110365538,
-441.885294117647));
#157778=CARTESIAN_POINT('Ctrl Pts',(-16.1559070823762,-8.04468584505497,
-443.379411764706));
#157779=CARTESIAN_POINT('Ctrl Pts',(-16.9013570056506,-6.54762058645456,
-444.873529411765));
#157780=CARTESIAN_POINT('Ctrl Pts',(-17.3590292079831,-4.93906964482095,
-446.367647058824));
#157781=CARTESIAN_POINT('Ctrl Pts',(-17.8167014103155,-3.33051870318735,
-447.861764705882));
#157782=CARTESIAN_POINT('Ctrl Pts',(-17.9710104137728,-1.66525935159368,
-449.355882352941));
#157783=CARTESIAN_POINT('Ctrl Pts',(-18.1253194172301,-1.10985572039171E-15,
-450.85));
#157784=CARTESIAN_POINT('Ctrl Pts',(-17.9710104137728,1.66525935159367,
-452.344117647059));
#157785=CARTESIAN_POINT('Ctrl Pts',(-17.8167014103155,3.33051870318735,
-453.838235294118));
#157786=CARTESIAN_POINT('Ctrl Pts',(-17.3590292079831,4.93906964482096,
-455.332352941176));
#157787=CARTESIAN_POINT('Ctrl Pts',(-16.9013570056506,6.54762058645456,
-456.826470588235));
#157788=CARTESIAN_POINT('Ctrl Pts',(-16.1559070823762,8.04468584505497,
-458.320588235294));
#157789=CARTESIAN_POINT('Ctrl Pts',(-15.4104571591017,9.54175110365538,
-459.814705882353));
#157790=CARTESIAN_POINT('Ctrl Pts',(-14.4026149179538,10.8763499173728,
-461.308823529412));
#157791=CARTESIAN_POINT('Ctrl Pts',(-13.3947726768058,12.2109487310903,
-462.802941176471));
#157792=CARTESIAN_POINT('Ctrl Pts',(-12.1588589765331,13.3376329379985,
-464.297058823529));
#157793=CARTESIAN_POINT('Ctrl Pts',(-10.9229452762603,14.4643171449067,
-465.791176470588));
#157794=CARTESIAN_POINT('Ctrl Pts',(-9.50104767561052,15.3447188656481,
-467.285294117647));
#157795=CARTESIAN_POINT('Ctrl Pts',(-8.07915007496071,16.2251205863895,
-468.779411764706));
#157796=CARTESIAN_POINT('Ctrl Pts',(-6.51968959134574,16.8292587962898,
-470.273529411765));
#157797=CARTESIAN_POINT('Ctrl Pts',(-4.96022910773078,17.4333970061901,
-471.767647058824));
#157798=CARTESIAN_POINT('Ctrl Pts',(-3.31631129755346,17.7406985030951,
-473.261764705882));
#157799=CARTESIAN_POINT('Ctrl Pts',(-1.67239348737615,18.048,-474.755882352941));
#157800=CARTESIAN_POINT('Ctrl Pts',(-2.21024254310115E-15,18.048,-476.25));
#157801=CARTESIAN_POINT('Ctrl Pts',(1.67239348737616,18.048,-477.744117647059));
#157802=CARTESIAN_POINT('Ctrl Pts',(3.31631129755346,17.7406985030951,-479.238235294118));
#157803=CARTESIAN_POINT('Ctrl Pts',(4.96022910773077,17.4333970061901,-480.732352941176));
#157804=CARTESIAN_POINT('Ctrl Pts',(6.51968959134575,16.8292587962898,-482.226470588235));
#157805=CARTESIAN_POINT('Ctrl Pts',(8.07915007496071,16.2251205863895,-483.720588235294));
#157806=CARTESIAN_POINT('Ctrl Pts',(9.50104767561053,15.3447188656481,-485.214705882353));
#157807=CARTESIAN_POINT('Ctrl Pts',(10.9229452762603,14.4643171449067,-486.708823529412));
#157808=CARTESIAN_POINT('Ctrl Pts',(12.1588589765331,13.3376329379985,-488.202941176471));
#157809=CARTESIAN_POINT('Ctrl Pts',(13.3947726768058,12.2109487310903,-489.697058823529));
#157810=CARTESIAN_POINT('Ctrl Pts',(14.4026149179538,10.8763499173728,-491.191176470588));
#157811=CARTESIAN_POINT('Ctrl Pts',(15.4104571591017,9.54175110365538,-492.685294117647));
#157812=CARTESIAN_POINT('Ctrl Pts',(16.1559070823762,8.04468584505496,-494.179411764706));
#157813=CARTESIAN_POINT('Ctrl Pts',(16.9013570056506,6.54762058645456,-495.673529411765));
#157814=CARTESIAN_POINT('Ctrl Pts',(17.3590292079831,4.93906964482096,-497.167647058824));
#157815=CARTESIAN_POINT('Ctrl Pts',(17.8167014103155,3.33051870318735,-498.661764705882));
#157816=CARTESIAN_POINT('Ctrl Pts',(17.9710104137728,1.66525935159367,-500.155882352941));
#157817=CARTESIAN_POINT('Ctrl Pts',(18.1253194172301,3.32956716117513E-15,
-501.65));
#157818=CARTESIAN_POINT('Ctrl Pts',(17.9710104137728,-1.66525935159367,
-503.144117647059));
#157819=CARTESIAN_POINT('Ctrl Pts',(17.8167014103155,-3.33051870318736,
-504.638235294118));
#157820=CARTESIAN_POINT('Ctrl Pts',(17.3590292079831,-4.93906964482095,
-506.132352941176));
#157821=CARTESIAN_POINT('Ctrl Pts',(16.9013570056506,-6.54762058645456,
-507.626470588235));
#157822=CARTESIAN_POINT('Ctrl Pts',(16.1559070823762,-8.04468584505497,
-509.120588235294));
#157823=CARTESIAN_POINT('Ctrl Pts',(15.4104571591017,-9.54175110365538,
-510.614705882353));
#157824=CARTESIAN_POINT('Ctrl Pts',(14.4026149179538,-10.8763499173728,
-512.108823529412));
#157825=CARTESIAN_POINT('Ctrl Pts',(13.3947726768058,-12.2109487310903,
-513.602941176471));
#157826=CARTESIAN_POINT('Ctrl Pts',(12.1588589765331,-13.3376329379985,
-515.09705882353));
#157827=CARTESIAN_POINT('Ctrl Pts',(10.9229452762603,-14.4643171449067,
-516.591176470588));
#157828=CARTESIAN_POINT('Ctrl Pts',(9.50104767561053,-15.3447188656481,
-518.085294117647));
#157829=CARTESIAN_POINT('Ctrl Pts',(8.07915007496071,-16.2251205863895,
-519.579411764706));
#157830=CARTESIAN_POINT('Ctrl Pts',(6.51968959134574,-16.8292587962898,
-521.073529411765));
#157831=CARTESIAN_POINT('Ctrl Pts',(4.96022910773078,-17.4333970061901,
-522.567647058823));
#157832=CARTESIAN_POINT('Ctrl Pts',(3.31631129755346,-17.7406985030951,
-524.061764705882));
#157833=CARTESIAN_POINT('Ctrl Pts',(1.67239348737615,-18.048,-525.555882352941));
#157834=CARTESIAN_POINT('Ctrl Pts',(0.,-18.048,-527.05));
#157835=CARTESIAN_POINT('Ctrl Pts',(-1.67239348737615,-18.048,-528.544117647059));
#157836=CARTESIAN_POINT('Ctrl Pts',(-3.31631129755346,-17.7406985030951,
-530.038235294118));
#157837=CARTESIAN_POINT('Ctrl Pts',(-4.96022910773077,-17.4333970061901,
-531.532352941177));
#157838=CARTESIAN_POINT('Ctrl Pts',(-6.51968959134574,-16.8292587962898,
-533.026470588235));
#157839=CARTESIAN_POINT('Ctrl Pts',(-8.07915007496071,-16.2251205863895,
-534.520588235294));
#157840=CARTESIAN_POINT('Ctrl Pts',(-9.50104767561052,-15.3447188656481,
-536.014705882353));
#157841=CARTESIAN_POINT('Ctrl Pts',(-10.9229452762603,-14.4643171449067,
-537.508823529412));
#157842=CARTESIAN_POINT('Ctrl Pts',(-12.1588589765331,-13.3376329379985,
-539.00294117647));
#157843=CARTESIAN_POINT('Ctrl Pts',(-13.3947726768058,-12.2109487310903,
-540.49705882353));
#157844=CARTESIAN_POINT('Ctrl Pts',(-14.4026149179538,-10.8763499173728,
-541.991176470588));
#157845=CARTESIAN_POINT('Ctrl Pts',(-15.4104571591017,-9.54175110365538,
-543.485294117647));
#157846=CARTESIAN_POINT('Ctrl Pts',(-16.1559070823762,-8.04468584505497,
-544.979411764706));
#157847=CARTESIAN_POINT('Ctrl Pts',(-16.9013570056506,-6.54762058645456,
-546.473529411765));
#157848=CARTESIAN_POINT('Ctrl Pts',(-17.3590292079831,-4.93906964482095,
-547.967647058823));
#157849=CARTESIAN_POINT('Ctrl Pts',(-17.8167014103155,-3.33051870318735,
-549.461764705882));
#157850=CARTESIAN_POINT('Ctrl Pts',(-17.9710104137728,-1.66525935159368,
-550.955882352941));
#157851=CARTESIAN_POINT('Ctrl Pts',(-18.1253194172301,-1.10985572039171E-15,
-552.45));
#157852=CARTESIAN_POINT('Ctrl Pts',(-17.9710104137728,1.66525935159367,
-553.944117647059));
#157853=CARTESIAN_POINT('Ctrl Pts',(-17.8167014103155,3.33051870318735,
-555.438235294118));
#157854=CARTESIAN_POINT('Ctrl Pts',(-17.3590292079831,4.93906964482096,
-556.932352941177));
#157855=CARTESIAN_POINT('Ctrl Pts',(-16.9013570056506,6.54762058645456,
-558.426470588235));
#157856=CARTESIAN_POINT('Ctrl Pts',(-16.1559070823762,8.04468584505497,
-559.920588235294));
#157857=CARTESIAN_POINT('Ctrl Pts',(-15.4104571591017,9.54175110365538,
-561.414705882353));
#157858=CARTESIAN_POINT('Ctrl Pts',(-14.4026149179538,10.8763499173728,
-562.908823529412));
#157859=CARTESIAN_POINT('Ctrl Pts',(-13.3947726768058,12.2109487310903,
-564.402941176471));
#157860=CARTESIAN_POINT('Ctrl Pts',(-12.1588589765331,13.3376329379985,
-565.897058823529));
#157861=CARTESIAN_POINT('Ctrl Pts',(-10.9229452762603,14.4643171449067,
-567.391176470588));
#157862=CARTESIAN_POINT('Ctrl Pts',(-9.50104767561052,15.3447188656481,
-568.885294117647));
#157863=CARTESIAN_POINT('Ctrl Pts',(-8.07915007496071,16.2251205863895,
-570.379411764706));
#157864=CARTESIAN_POINT('Ctrl Pts',(-6.51968959134574,16.8292587962898,
-571.873529411765));
#157865=CARTESIAN_POINT('Ctrl Pts',(-4.96022910773078,17.4333970061901,
-573.367647058824));
#157866=CARTESIAN_POINT('Ctrl Pts',(-3.31631129755346,17.7406985030951,
-574.861764705882));
#157867=CARTESIAN_POINT('Ctrl Pts',(-1.67239348737615,18.048,-576.355882352941));
#157868=CARTESIAN_POINT('Ctrl Pts',(-2.21024254310115E-15,18.048,-577.85));
#157869=CARTESIAN_POINT('Ctrl Pts',(1.67239348737616,18.048,-579.344117647059));
#157870=CARTESIAN_POINT('Ctrl Pts',(3.31631129755346,17.7406985030951,-580.838235294117));
#157871=CARTESIAN_POINT('Ctrl Pts',(4.96022910773077,17.4333970061901,-582.332352941176));
#157872=CARTESIAN_POINT('Ctrl Pts',(6.51968959134575,16.8292587962898,-583.826470588235));
#157873=CARTESIAN_POINT('Ctrl Pts',(8.07915007496071,16.2251205863895,-585.320588235294));
#157874=CARTESIAN_POINT('Ctrl Pts',(9.50104767561053,15.3447188656481,-586.814705882353));
#157875=CARTESIAN_POINT('Ctrl Pts',(10.9229452762603,14.4643171449067,-588.308823529412));
#157876=CARTESIAN_POINT('Ctrl Pts',(12.1588589765331,13.3376329379985,-589.802941176471));
#157877=CARTESIAN_POINT('Ctrl Pts',(13.3947726768058,12.2109487310903,-591.297058823529));
#157878=CARTESIAN_POINT('Ctrl Pts',(14.4026149179538,10.8763499173728,-592.791176470588));
#157879=CARTESIAN_POINT('Ctrl Pts',(15.4104571591017,9.54175110365538,-594.285294117647));
#157880=CARTESIAN_POINT('Ctrl Pts',(16.1559070823762,8.04468584505496,-595.779411764706));
#157881=CARTESIAN_POINT('Ctrl Pts',(16.9013570056506,6.54762058645456,-597.273529411765));
#157882=CARTESIAN_POINT('Ctrl Pts',(17.3590292079831,4.93906964482096,-598.767647058824));
#157883=CARTESIAN_POINT('Ctrl Pts',(17.8167014103155,3.33051870318735,-600.261764705882));
#157884=CARTESIAN_POINT('Ctrl Pts',(17.9710104137728,1.66525935159367,-601.755882352941));
#157885=CARTESIAN_POINT('Ctrl Pts',(18.1253194172301,3.32956716117513E-15,
-603.25));
#157886=CARTESIAN_POINT('Ctrl Pts',(17.9710104137728,-1.66525935159367,
-604.744117647059));
#157887=CARTESIAN_POINT('Ctrl Pts',(17.8167014103155,-3.33051870318736,
-606.238235294118));
#157888=CARTESIAN_POINT('Ctrl Pts',(17.3590292079831,-4.93906964482095,
-607.732352941176));
#157889=CARTESIAN_POINT('Ctrl Pts',(16.9013570056506,-6.54762058645456,
-609.226470588235));
#157890=CARTESIAN_POINT('Ctrl Pts',(16.1559070823762,-8.04468584505497,
-610.720588235294));
#157891=CARTESIAN_POINT('Ctrl Pts',(15.4104571591017,-9.54175110365538,
-612.214705882353));
#157892=CARTESIAN_POINT('Ctrl Pts',(14.4026149179538,-10.8763499173728,
-613.708823529412));
#157893=CARTESIAN_POINT('Ctrl Pts',(13.3947726768058,-12.2109487310903,
-615.202941176471));
#157894=CARTESIAN_POINT('Ctrl Pts',(12.1588589765331,-13.3376329379985,
-616.697058823529));
#157895=CARTESIAN_POINT('Ctrl Pts',(10.9229452762603,-14.4643171449067,
-618.191176470588));
#157896=CARTESIAN_POINT('Ctrl Pts',(9.50104767561053,-15.3447188656481,
-619.685294117647));
#157897=CARTESIAN_POINT('Ctrl Pts',(8.07915007496071,-16.2251205863895,
-621.179411764706));
#157898=CARTESIAN_POINT('Ctrl Pts',(6.51968959134574,-16.8292587962898,
-622.673529411764));
#157899=CARTESIAN_POINT('Ctrl Pts',(4.96022910773078,-17.4333970061901,
-624.167647058823));
#157900=CARTESIAN_POINT('Ctrl Pts',(3.31631129755346,-17.7406985030951,
-625.661764705882));
#157901=CARTESIAN_POINT('Ctrl Pts',(1.67239348737615,-18.048,-627.155882352941));
#157902=CARTESIAN_POINT('Ctrl Pts',(0.,-18.048,-628.65));
#157903=CARTESIAN_POINT('Ctrl Pts',(-1.67239348737615,-18.048,-630.144117647059));
#157904=CARTESIAN_POINT('Ctrl Pts',(-3.31631129755346,-17.7406985030951,
-631.638235294118));
#157905=CARTESIAN_POINT('Ctrl Pts',(-4.96022910773077,-17.4333970061901,
-633.132352941176));
#157906=CARTESIAN_POINT('Ctrl Pts',(-6.51968959134574,-16.8292587962898,
-634.626470588235));
#157907=CARTESIAN_POINT('Ctrl Pts',(-8.07915007496071,-16.2251205863895,
-636.120588235294));
#157908=CARTESIAN_POINT('Ctrl Pts',(-9.50104767561052,-15.3447188656481,
-637.614705882353));
#157909=CARTESIAN_POINT('Ctrl Pts',(-10.9229452762603,-14.4643171449067,
-639.108823529412));
#157910=CARTESIAN_POINT('Ctrl Pts',(-12.1588589765331,-13.3376329379985,
-640.60294117647));
#157911=CARTESIAN_POINT('Ctrl Pts',(-13.3947726768058,-12.2109487310903,
-642.097058823529));
#157912=CARTESIAN_POINT('Ctrl Pts',(-14.4026149179538,-10.8763499173728,
-643.591176470588));
#157913=CARTESIAN_POINT('Ctrl Pts',(-15.4104571591017,-9.54175110365538,
-645.085294117647));
#157914=CARTESIAN_POINT('Ctrl Pts',(-16.1559070823762,-8.04468584505497,
-646.579411764706));
#157915=CARTESIAN_POINT('Ctrl Pts',(-16.9013570056506,-6.54762058645456,
-648.073529411765));
#157916=CARTESIAN_POINT('Ctrl Pts',(-17.3590292079831,-4.93906964482095,
-649.567647058824));
#157917=CARTESIAN_POINT('Ctrl Pts',(-17.8167014103155,-3.33051870318735,
-651.061764705883));
#157918=CARTESIAN_POINT('Ctrl Pts',(-17.9710104137728,-1.66525935159368,
-652.555882352941));
#157919=CARTESIAN_POINT('Ctrl Pts',(-18.1253194172301,-1.10985572039171E-15,
-654.05));
#157920=CARTESIAN_POINT('Ctrl Pts',(-17.9710104137728,1.66525935159367,
-655.544117647059));
#157921=CARTESIAN_POINT('Ctrl Pts',(-17.8167014103155,3.33051870318735,
-657.038235294117));
#157922=CARTESIAN_POINT('Ctrl Pts',(-17.3590292079831,4.93906964482096,
-658.532352941177));
#157923=CARTESIAN_POINT('Ctrl Pts',(-16.9013570056506,6.54762058645456,
-660.026470588235));
#157924=CARTESIAN_POINT('Ctrl Pts',(-16.1559070823762,8.04468584505497,
-661.520588235294));
#157925=CARTESIAN_POINT('Ctrl Pts',(-15.4104571591017,9.54175110365538,
-663.014705882353));
#157926=CARTESIAN_POINT('Ctrl Pts',(-14.4026149179538,10.8763499173728,
-664.508823529412));
#157927=CARTESIAN_POINT('Ctrl Pts',(-13.3947726768058,12.2109487310903,
-666.002941176471));
#157928=CARTESIAN_POINT('Ctrl Pts',(-12.1588589765331,13.3376329379985,
-667.497058823529));
#157929=CARTESIAN_POINT('Ctrl Pts',(-10.9229452762603,14.4643171449067,
-668.991176470588));
#157930=CARTESIAN_POINT('Ctrl Pts',(-9.50104767561052,15.3447188656481,
-670.485294117647));
#157931=CARTESIAN_POINT('Ctrl Pts',(-8.07915007496071,16.2251205863895,
-671.979411764706));
#157932=CARTESIAN_POINT('Ctrl Pts',(-6.51968959134574,16.8292587962898,
-673.473529411765));
#157933=CARTESIAN_POINT('Ctrl Pts',(-4.96022910773078,17.4333970061901,
-674.967647058824));
#157934=CARTESIAN_POINT('Ctrl Pts',(-3.31631129755346,17.7406985030951,
-676.461764705882));
#157935=CARTESIAN_POINT('Ctrl Pts',(-1.67239348737615,18.048,-677.955882352941));
#157936=CARTESIAN_POINT('Ctrl Pts',(-2.21024254310115E-15,18.048,-679.45));
#157937=CARTESIAN_POINT('Ctrl Pts',(1.67239348737616,18.048,-680.944117647059));
#157938=CARTESIAN_POINT('Ctrl Pts',(3.31631129755346,17.7406985030951,-682.438235294117));
#157939=CARTESIAN_POINT('Ctrl Pts',(4.96022910773077,17.4333970061901,-683.932352941176));
#157940=CARTESIAN_POINT('Ctrl Pts',(6.51968959134575,16.8292587962898,-685.426470588235));
#157941=CARTESIAN_POINT('Ctrl Pts',(8.07915007496071,16.2251205863895,-686.920588235294));
#157942=CARTESIAN_POINT('Ctrl Pts',(9.50104767561053,15.3447188656481,-688.414705882353));
#157943=CARTESIAN_POINT('Ctrl Pts',(10.9229452762603,14.4643171449067,-689.908823529412));
#157944=CARTESIAN_POINT('Ctrl Pts',(12.1588589765331,13.3376329379985,-691.402941176471));
#157945=CARTESIAN_POINT('Ctrl Pts',(13.3947726768058,12.2109487310903,-692.89705882353));
#157946=CARTESIAN_POINT('Ctrl Pts',(14.4026149179538,10.8763499173728,-694.391176470588));
#157947=CARTESIAN_POINT('Ctrl Pts',(15.4104571591017,9.54175110365538,-695.885294117647));
#157948=CARTESIAN_POINT('Ctrl Pts',(16.1559070823762,8.04468584505496,-697.379411764706));
#157949=CARTESIAN_POINT('Ctrl Pts',(16.9013570056506,6.54762058645456,-698.873529411764));
#157950=CARTESIAN_POINT('Ctrl Pts',(17.3590292079831,4.93906964482096,-700.367647058823));
#157951=CARTESIAN_POINT('Ctrl Pts',(17.8167014103155,3.33051870318735,-701.861764705882));
#157952=CARTESIAN_POINT('Ctrl Pts',(17.9710104137728,1.66525935159367,-703.355882352941));
#157953=CARTESIAN_POINT('Ctrl Pts',(18.1253194172301,3.32956716117513E-15,
-704.85));
#157954=CARTESIAN_POINT('Ctrl Pts',(17.9710104137728,-1.66525935159367,
-706.344117647059));
#157955=CARTESIAN_POINT('Ctrl Pts',(17.8167014103155,-3.33051870318736,
-707.838235294118));
#157956=CARTESIAN_POINT('Ctrl Pts',(17.3590292079831,-4.93906964482095,
-709.332352941177));
#157957=CARTESIAN_POINT('Ctrl Pts',(16.9013570056506,-6.54762058645456,
-710.826470588236));
#157958=CARTESIAN_POINT('Ctrl Pts',(16.1559070823762,-8.04468584505497,
-712.320588235294));
#157959=CARTESIAN_POINT('Ctrl Pts',(15.4104571591017,-9.54175110365538,
-713.814705882353));
#157960=CARTESIAN_POINT('Ctrl Pts',(14.4026149179538,-10.8763499173728,
-715.308823529412));
#157961=CARTESIAN_POINT('Ctrl Pts',(13.3947726768058,-12.2109487310903,
-716.802941176471));
#157962=CARTESIAN_POINT('Ctrl Pts',(12.1588589765331,-13.3376329379985,
-718.297058823529));
#157963=CARTESIAN_POINT('Ctrl Pts',(10.9229452762603,-14.4643171449067,
-719.791176470588));
#157964=CARTESIAN_POINT('Ctrl Pts',(9.50104767561053,-15.3447188656481,
-721.285294117647));
#157965=CARTESIAN_POINT('Ctrl Pts',(8.07915007496071,-16.2251205863895,
-722.779411764706));
#157966=CARTESIAN_POINT('Ctrl Pts',(6.51968959134574,-16.8292587962898,
-724.273529411765));
#157967=CARTESIAN_POINT('Ctrl Pts',(4.96022910773078,-17.4333970061901,
-725.767647058824));
#157968=CARTESIAN_POINT('Ctrl Pts',(3.31631129755346,-17.7406985030951,
-727.261764705882));
#157969=CARTESIAN_POINT('Ctrl Pts',(1.67239348737615,-18.048,-728.755882352941));
#157970=CARTESIAN_POINT('Ctrl Pts',(0.,-18.048,-730.25));
#157971=CARTESIAN_POINT('Ctrl Pts',(-1.67239348737615,-18.048,-731.744117647059));
#157972=CARTESIAN_POINT('Ctrl Pts',(-3.31631129755346,-17.7406985030951,
-733.238235294118));
#157973=CARTESIAN_POINT('Ctrl Pts',(-4.96022910773077,-17.4333970061901,
-734.732352941177));
#157974=CARTESIAN_POINT('Ctrl Pts',(-6.51968959134574,-16.8292587962898,
-736.226470588235));
#157975=CARTESIAN_POINT('Ctrl Pts',(-8.07915007496071,-16.2251205863895,
-737.720588235294));
#157976=CARTESIAN_POINT('Ctrl Pts',(-9.50104767561052,-15.3447188656481,
-739.214705882353));
#157977=CARTESIAN_POINT('Ctrl Pts',(-10.9229452762603,-14.4643171449067,
-740.708823529412));
#157978=CARTESIAN_POINT('Ctrl Pts',(-12.1588589765331,-13.3376329379985,
-742.20294117647));
#157979=CARTESIAN_POINT('Ctrl Pts',(-13.3947726768058,-12.2109487310903,
-743.697058823529));
#157980=CARTESIAN_POINT('Ctrl Pts',(-14.4026149179538,-10.8763499173728,
-745.191176470588));
#157981=CARTESIAN_POINT('Ctrl Pts',(-15.4104571591017,-9.54175110365538,
-746.685294117647));
#157982=CARTESIAN_POINT('Ctrl Pts',(-16.1559070823762,-8.04468584505497,
-748.179411764706));
#157983=CARTESIAN_POINT('Ctrl Pts',(-16.9013570056506,-6.54762058645456,
-749.673529411765));
#157984=CARTESIAN_POINT('Ctrl Pts',(-17.3590292079831,-4.93906964482095,
-751.167647058824));
#157985=CARTESIAN_POINT('Ctrl Pts',(-17.8167014103155,-3.33051870318735,
-752.661764705882));
#157986=CARTESIAN_POINT('Ctrl Pts',(-17.9710104137728,-1.66525935159368,
-754.155882352941));
#157987=CARTESIAN_POINT('Ctrl Pts',(-18.1253194172301,-1.10985572039171E-15,
-755.65));
#157988=CARTESIAN_POINT('Ctrl Pts',(-17.9710104137728,1.66525935159367,
-757.144117647059));
#157989=CARTESIAN_POINT('Ctrl Pts',(-17.8167014103155,3.33051870318735,
-758.638235294118));
#157990=CARTESIAN_POINT('Ctrl Pts',(-17.3590292079831,4.93906964482096,
-760.132352941176));
#157991=CARTESIAN_POINT('Ctrl Pts',(-16.9013570056506,6.54762058645456,
-761.626470588235));
#157992=CARTESIAN_POINT('Ctrl Pts',(-16.1559070823762,8.04468584505497,
-763.120588235294));
#157993=CARTESIAN_POINT('Ctrl Pts',(-15.4104571591017,9.54175110365538,
-764.614705882353));
#157994=CARTESIAN_POINT('Ctrl Pts',(-14.4026149179538,10.8763499173728,
-766.108823529412));
#157995=CARTESIAN_POINT('Ctrl Pts',(-13.3947726768058,12.2109487310903,
-767.602941176471));
#157996=CARTESIAN_POINT('Ctrl Pts',(-12.1588589765331,13.3376329379985,
-769.09705882353));
#157997=CARTESIAN_POINT('Ctrl Pts',(-10.9229452762603,14.4643171449067,
-770.591176470589));
#157998=CARTESIAN_POINT('Ctrl Pts',(-9.50104767561052,15.3447188656481,
-772.085294117647));
#157999=CARTESIAN_POINT('Ctrl Pts',(-8.07915007496071,16.2251205863895,
-773.579411764706));
#158000=CARTESIAN_POINT('Ctrl Pts',(-6.51968959134574,16.8292587962898,
-775.073529411765));
#158001=CARTESIAN_POINT('Ctrl Pts',(-4.96022910773078,17.4333970061901,
-776.567647058824));
#158002=CARTESIAN_POINT('Ctrl Pts',(-3.31631129755346,17.7406985030951,
-778.061764705882));
#158003=CARTESIAN_POINT('Ctrl Pts',(-1.67239348737615,18.048,-779.555882352941));
#158004=CARTESIAN_POINT('Ctrl Pts',(-2.21024254310115E-15,18.048,-781.05));
#158005=CARTESIAN_POINT('Ctrl Pts',(1.67239348737616,18.048,-782.544117647059));
#158006=CARTESIAN_POINT('Ctrl Pts',(3.31631129755346,17.7406985030951,-784.038235294118));
#158007=CARTESIAN_POINT('Ctrl Pts',(4.96022910773077,17.4333970061901,-785.532352941177));
#158008=CARTESIAN_POINT('Ctrl Pts',(6.51968959134575,16.8292587962898,-787.026470588235));
#158009=CARTESIAN_POINT('Ctrl Pts',(8.07915007496071,16.2251205863895,-788.520588235294));
#158010=CARTESIAN_POINT('Ctrl Pts',(9.50104767561053,15.3447188656481,-790.014705882353));
#158011=CARTESIAN_POINT('Ctrl Pts',(10.9229452762603,14.4643171449067,-791.508823529412));
#158012=CARTESIAN_POINT('Ctrl Pts',(12.1588589765331,13.3376329379985,-793.002941176471));
#158013=CARTESIAN_POINT('Ctrl Pts',(13.3947726768058,12.2109487310903,-794.497058823529));
#158014=CARTESIAN_POINT('Ctrl Pts',(14.4026149179538,10.8763499173728,-795.991176470588));
#158015=CARTESIAN_POINT('Ctrl Pts',(15.4104571591017,9.54175110365538,-797.485294117647));
#158016=CARTESIAN_POINT('Ctrl Pts',(16.1559070823762,8.04468584505496,-798.979411764706));
#158017=CARTESIAN_POINT('Ctrl Pts',(16.9013570056506,6.54762058645456,-800.473529411765));
#158018=CARTESIAN_POINT('Ctrl Pts',(17.3590292079831,4.93906964482096,-801.967647058823));
#158019=CARTESIAN_POINT('Ctrl Pts',(17.8167014103155,3.33051870318735,-803.461764705882));
#158020=CARTESIAN_POINT('Ctrl Pts',(17.9710104137728,1.66525935159367,-804.955882352941));
#158021=CARTESIAN_POINT('Ctrl Pts',(18.1253194172301,3.32956716117513E-15,
-806.45));
#158022=CARTESIAN_POINT('Ctrl Pts',(17.9710104137728,-1.66525935159367,
-807.944117647059));
#158023=CARTESIAN_POINT('Ctrl Pts',(17.8167014103155,-3.33051870318736,
-809.438235294118));
#158024=CARTESIAN_POINT('Ctrl Pts',(17.3590292079831,-4.93906964482095,
-810.932352941177));
#158025=CARTESIAN_POINT('Ctrl Pts',(16.9013570056506,-6.54762058645456,
-812.426470588235));
#158026=CARTESIAN_POINT('Ctrl Pts',(16.1559070823762,-8.04468584505497,
-813.920588235294));
#158027=CARTESIAN_POINT('Ctrl Pts',(15.4104571591017,-9.54175110365538,
-815.414705882353));
#158028=CARTESIAN_POINT('Ctrl Pts',(14.4026149179538,-10.8763499173728,
-816.908823529412));
#158029=CARTESIAN_POINT('Ctrl Pts',(13.3947726768058,-12.2109487310903,
-818.40294117647));
#158030=CARTESIAN_POINT('Ctrl Pts',(12.1588589765331,-13.3376329379985,
-819.897058823529));
#158031=CARTESIAN_POINT('Ctrl Pts',(10.9229452762603,-14.4643171449067,
-821.391176470588));
#158032=CARTESIAN_POINT('Ctrl Pts',(9.50104767561053,-15.3447188656481,
-822.885294117647));
#158033=CARTESIAN_POINT('Ctrl Pts',(8.07915007496071,-16.2251205863895,
-824.379411764706));
#158034=CARTESIAN_POINT('Ctrl Pts',(6.51968959134574,-16.8292587962898,
-825.873529411765));
#158035=CARTESIAN_POINT('Ctrl Pts',(4.96022910773078,-17.4333970061901,
-827.367647058824));
#158036=CARTESIAN_POINT('Ctrl Pts',(3.31631129755346,-17.7406985030951,
-828.861764705882));
#158037=CARTESIAN_POINT('Ctrl Pts',(1.67239348737615,-18.048,-830.355882352941));
#158038=CARTESIAN_POINT('Ctrl Pts',(0.,-18.048,-831.85));
#158039=CARTESIAN_POINT('Ctrl Pts',(-1.67239348737615,-18.048,-833.344117647059));
#158040=CARTESIAN_POINT('Ctrl Pts',(-3.31631129755346,-17.7406985030951,
-834.838235294118));
#158041=CARTESIAN_POINT('Ctrl Pts',(-4.96022910773077,-17.4333970061901,
-836.332352941177));
#158042=CARTESIAN_POINT('Ctrl Pts',(-6.51968959134574,-16.8292587962898,
-837.826470588235));
#158043=CARTESIAN_POINT('Ctrl Pts',(-8.07915007496071,-16.2251205863895,
-839.320588235294));
#158044=CARTESIAN_POINT('Ctrl Pts',(-9.50104767561052,-15.3447188656481,
-840.814705882353));
#158045=CARTESIAN_POINT('Ctrl Pts',(-10.9229452762603,-14.4643171449067,
-842.308823529412));
#158046=CARTESIAN_POINT('Ctrl Pts',(-12.1588589765331,-13.3376329379985,
-843.802941176471));
#158047=CARTESIAN_POINT('Ctrl Pts',(-13.3947726768058,-12.2109487310903,
-845.29705882353));
#158048=CARTESIAN_POINT('Ctrl Pts',(-14.4026149179538,-10.8763499173728,
-846.791176470588));
#158049=CARTESIAN_POINT('Ctrl Pts',(-15.4104571591017,-9.54175110365538,
-848.285294117647));
#158050=CARTESIAN_POINT('Ctrl Pts',(-16.1559070823762,-8.04468584505497,
-849.779411764706));
#158051=CARTESIAN_POINT('Ctrl Pts',(-16.9013570056506,-6.54762058645456,
-851.273529411765));
#158052=CARTESIAN_POINT('Ctrl Pts',(-17.3590292079831,-4.93906964482095,
-852.767647058824));
#158053=CARTESIAN_POINT('Ctrl Pts',(-17.8167014103155,-3.33051870318735,
-854.261764705882));
#158054=CARTESIAN_POINT('Ctrl Pts',(-17.9710104137728,-1.66525935159368,
-855.755882352941));
#158055=CARTESIAN_POINT('Ctrl Pts',(-18.1253194172301,-1.10985572039171E-15,
-857.25));
#158056=CARTESIAN_POINT('Ctrl Pts',(-17.9710104137728,1.66525935159367,
-858.744117647059));
#158057=CARTESIAN_POINT('Ctrl Pts',(-17.8167014103155,3.33051870318735,
-860.238235294118));
#158058=CARTESIAN_POINT('Ctrl Pts',(-17.3590292079831,4.93906964482096,
-861.732352941176));
#158059=CARTESIAN_POINT('Ctrl Pts',(-16.9013570056506,6.54762058645456,
-863.226470588235));
#158060=CARTESIAN_POINT('Ctrl Pts',(-16.1559070823762,8.04468584505497,
-864.720588235294));
#158061=CARTESIAN_POINT('Ctrl Pts',(-15.4104571591017,9.54175110365538,
-866.214705882353));
#158062=CARTESIAN_POINT('Ctrl Pts',(-14.4026149179538,10.8763499173728,
-867.708823529412));
#158063=CARTESIAN_POINT('Ctrl Pts',(-13.3947726768058,12.2109487310903,
-869.202941176471));
#158064=CARTESIAN_POINT('Ctrl Pts',(-12.1588589765331,13.3376329379985,
-870.697058823529));
#158065=CARTESIAN_POINT('Ctrl Pts',(-10.9229452762603,14.4643171449067,
-872.191176470589));
#158066=CARTESIAN_POINT('Ctrl Pts',(-9.50104767561052,15.3447188656481,
-873.685294117647));
#158067=CARTESIAN_POINT('Ctrl Pts',(-8.07915007496071,16.2251205863895,
-875.179411764706));
#158068=CARTESIAN_POINT('Ctrl Pts',(-6.51968959134574,16.8292587962898,
-876.673529411764));
#158069=CARTESIAN_POINT('Ctrl Pts',(-4.96022910773078,17.4333970061901,
-878.167647058823));
#158070=CARTESIAN_POINT('Ctrl Pts',(-3.31631129755346,17.7406985030951,
-879.661764705882));
#158071=CARTESIAN_POINT('Ctrl Pts',(-1.67239348737615,18.048,-881.155882352941));
#158072=CARTESIAN_POINT('Ctrl Pts',(-2.21024254310115E-15,18.048,-882.65));
#158073=CARTESIAN_POINT('Ctrl Pts',(1.67239348737616,18.048,-884.144117647059));
#158074=CARTESIAN_POINT('Ctrl Pts',(3.31631129755346,17.7406985030951,-885.638235294118));
#158075=CARTESIAN_POINT('Ctrl Pts',(4.96022910773077,17.4333970061901,-887.132352941177));
#158076=CARTESIAN_POINT('Ctrl Pts',(6.51968959134575,16.8292587962898,-888.626470588235));
#158077=CARTESIAN_POINT('Ctrl Pts',(8.07915007496071,16.2251205863895,-890.120588235294));
#158078=CARTESIAN_POINT('Ctrl Pts',(9.50104767561053,15.3447188656481,-891.614705882353));
#158079=CARTESIAN_POINT('Ctrl Pts',(10.9229452762603,14.4643171449067,-893.108823529412));
#158080=CARTESIAN_POINT('Ctrl Pts',(12.1588589765331,13.3376329379985,-894.60294117647));
#158081=CARTESIAN_POINT('Ctrl Pts',(13.3947726768058,12.2109487310903,-896.09705882353));
#158082=CARTESIAN_POINT('Ctrl Pts',(14.4026149179538,10.8763499173728,-897.591176470588));
#158083=CARTESIAN_POINT('Ctrl Pts',(15.4104571591017,9.54175110365538,-899.085294117647));
#158084=CARTESIAN_POINT('Ctrl Pts',(16.1559070823762,8.04468584505496,-900.579411764706));
#158085=CARTESIAN_POINT('Ctrl Pts',(16.9013570056506,6.54762058645456,-902.073529411765));
#158086=CARTESIAN_POINT('Ctrl Pts',(17.3590292079831,4.93906964482096,-903.567647058824));
#158087=CARTESIAN_POINT('Ctrl Pts',(17.8167014103155,3.33051870318735,-905.061764705883));
#158088=CARTESIAN_POINT('Ctrl Pts',(17.9710104137728,1.66525935159367,-906.555882352941));
#158089=CARTESIAN_POINT('Ctrl Pts',(18.1253194172301,3.32956716117513E-15,
-908.05));
#158090=CARTESIAN_POINT('Ctrl Pts',(17.9710104137728,-1.66525935159367,
-909.544117647059));
#158091=CARTESIAN_POINT('Ctrl Pts',(17.8167014103155,-3.33051870318736,
-911.038235294118));
#158092=CARTESIAN_POINT('Ctrl Pts',(17.3590292079831,-4.93906964482095,
-912.532352941176));
#158093=CARTESIAN_POINT('Ctrl Pts',(16.9013570056506,-6.54762058645456,
-914.026470588235));
#158094=CARTESIAN_POINT('Ctrl Pts',(16.1559070823762,-8.04468584505497,
-915.520588235294));
#158095=CARTESIAN_POINT('Ctrl Pts',(15.4104571591017,-9.54175110365538,
-917.014705882353));
#158096=CARTESIAN_POINT('Ctrl Pts',(14.4026149179538,-10.8763499173728,
-918.508823529412));
#158097=CARTESIAN_POINT('Ctrl Pts',(13.3947726768058,-12.2109487310903,
-920.002941176471));
#158098=CARTESIAN_POINT('Ctrl Pts',(12.1588589765331,-13.3376329379985,
-921.497058823529));
#158099=CARTESIAN_POINT('Ctrl Pts',(10.9229452762603,-14.4643171449067,
-922.991176470588));
#158100=CARTESIAN_POINT('Ctrl Pts',(9.50104767561053,-15.3447188656481,
-924.485294117647));
#158101=CARTESIAN_POINT('Ctrl Pts',(8.07915007496071,-16.2251205863895,
-925.979411764706));
#158102=CARTESIAN_POINT('Ctrl Pts',(6.51968959134574,-16.8292587962898,
-927.473529411765));
#158103=CARTESIAN_POINT('Ctrl Pts',(4.96022910773078,-17.4333970061901,
-928.967647058823));
#158104=CARTESIAN_POINT('Ctrl Pts',(3.31631129755346,-17.7406985030951,
-930.461764705883));
#158105=CARTESIAN_POINT('Ctrl Pts',(1.67239348737615,-18.048,-931.955882352941));
#158106=CARTESIAN_POINT('Ctrl Pts',(0.,-18.048,-933.45));
#158107=CARTESIAN_POINT('Ctrl Pts',(-1.67239348737615,-18.048,-934.944117647059));
#158108=CARTESIAN_POINT('Ctrl Pts',(-3.31631129755346,-17.7406985030951,
-936.438235294117));
#158109=CARTESIAN_POINT('Ctrl Pts',(-4.96022910773077,-17.4333970061901,
-937.932352941177));
#158110=CARTESIAN_POINT('Ctrl Pts',(-6.51968959134574,-16.8292587962898,
-939.426470588235));
#158111=CARTESIAN_POINT('Ctrl Pts',(-8.07915007496071,-16.2251205863895,
-940.920588235294));
#158112=CARTESIAN_POINT('Ctrl Pts',(-9.50104767561052,-15.3447188656481,
-942.414705882353));
#158113=CARTESIAN_POINT('Ctrl Pts',(-10.9229452762603,-14.4643171449067,
-943.908823529412));
#158114=CARTESIAN_POINT('Ctrl Pts',(-12.1588589765331,-13.3376329379985,
-945.402941176471));
#158115=CARTESIAN_POINT('Ctrl Pts',(-13.3947726768058,-12.2109487310903,
-946.89705882353));
#158116=CARTESIAN_POINT('Ctrl Pts',(-14.4026149179538,-10.8763499173728,
-948.391176470588));
#158117=CARTESIAN_POINT('Ctrl Pts',(-15.4104571591017,-9.54175110365538,
-949.885294117647));
#158118=CARTESIAN_POINT('Ctrl Pts',(-16.1559070823762,-8.04468584505497,
-951.379411764706));
#158119=CARTESIAN_POINT('Ctrl Pts',(-16.9013570056506,-6.54762058645456,
-952.873529411765));
#158120=CARTESIAN_POINT('Ctrl Pts',(-17.3590292079831,-4.93906964482095,
-954.367647058824));
#158121=CARTESIAN_POINT('Ctrl Pts',(-17.8167014103155,-3.33051870318735,
-955.861764705882));
#158122=CARTESIAN_POINT('Ctrl Pts',(-17.9710104137728,-1.66525935159368,
-957.355882352941));
#158123=CARTESIAN_POINT('Ctrl Pts',(-18.1253194172301,-1.10985572039171E-15,
-958.85));
#158124=CARTESIAN_POINT('Ctrl Pts',(-17.9710104137728,1.66525935159367,
-960.344117647059));
#158125=CARTESIAN_POINT('Ctrl Pts',(-17.8167014103155,3.33051870318735,
-961.838235294118));
#158126=CARTESIAN_POINT('Ctrl Pts',(-17.3590292079831,4.93906964482096,
-963.332352941177));
#158127=CARTESIAN_POINT('Ctrl Pts',(-16.9013570056506,6.54762058645456,
-964.826470588235));
#158128=CARTESIAN_POINT('Ctrl Pts',(-16.1559070823762,8.04468584505497,
-966.320588235294));
#158129=CARTESIAN_POINT('Ctrl Pts',(-15.4104571591017,9.54175110365538,
-967.814705882353));
#158130=CARTESIAN_POINT('Ctrl Pts',(-14.4026149179538,10.8763499173728,
-969.308823529412));
#158131=CARTESIAN_POINT('Ctrl Pts',(-13.3947726768058,12.2109487310903,
-970.80294117647));
#158132=CARTESIAN_POINT('Ctrl Pts',(-12.1588589765331,13.3376329379985,
-972.297058823529));
#158133=CARTESIAN_POINT('Ctrl Pts',(-10.9229452762603,14.4643171449067,
-973.791176470588));
#158134=CARTESIAN_POINT('Ctrl Pts',(-9.50104767561052,15.3447188656481,
-975.285294117647));
#158135=CARTESIAN_POINT('Ctrl Pts',(-8.07915007496071,16.2251205863895,
-976.779411764706));
#158136=CARTESIAN_POINT('Ctrl Pts',(-6.51968959134574,16.8292587962898,
-978.273529411765));
#158137=CARTESIAN_POINT('Ctrl Pts',(-4.96022910773078,17.4333970061901,
-979.767647058824));
#158138=CARTESIAN_POINT('Ctrl Pts',(-3.31631129755346,17.7406985030951,
-981.261764705882));
#158139=CARTESIAN_POINT('Ctrl Pts',(-1.67239348737615,18.048,-982.755882352941));
#158140=CARTESIAN_POINT('Ctrl Pts',(-2.21024254310115E-15,18.048,-984.25));
#158141=CARTESIAN_POINT('Ctrl Pts',(1.67239348737616,18.048,-985.744117647059));
#158142=CARTESIAN_POINT('Ctrl Pts',(3.31631129755346,17.7406985030951,-987.238235294118));
#158143=CARTESIAN_POINT('Ctrl Pts',(4.96022910773077,17.4333970061901,-988.732352941177));
#158144=CARTESIAN_POINT('Ctrl Pts',(6.51968959134575,16.8292587962898,-990.226470588235));
#158145=CARTESIAN_POINT('Ctrl Pts',(8.07915007496071,16.2251205863895,-991.720588235294));
#158146=CARTESIAN_POINT('Ctrl Pts',(9.50104767561053,15.3447188656481,-993.214705882353));
#158147=CARTESIAN_POINT('Ctrl Pts',(10.9229452762603,14.4643171449067,-994.708823529412));
#158148=CARTESIAN_POINT('Ctrl Pts',(12.1588589765331,13.3376329379985,-996.202941176471));
#158149=CARTESIAN_POINT('Ctrl Pts',(13.3947726768058,12.2109487310903,-997.697058823529));
#158150=CARTESIAN_POINT('Ctrl Pts',(14.4026149179538,10.8763499173728,-999.191176470588));
#158151=CARTESIAN_POINT('Ctrl Pts',(15.4104571591017,9.54175110365538,-1000.68529411765));
#158152=CARTESIAN_POINT('Ctrl Pts',(16.1559070823762,8.04468584505496,-1002.17941176471));
#158153=CARTESIAN_POINT('Ctrl Pts',(16.9013570056506,6.54762058645456,-1003.67352941176));
#158154=CARTESIAN_POINT('Ctrl Pts',(17.3590292079831,4.93906964482096,-1005.16764705882));
#158155=CARTESIAN_POINT('Ctrl Pts',(17.8167014103155,3.33051870318735,-1006.66176470588));
#158156=CARTESIAN_POINT('Ctrl Pts',(17.9710104137728,1.66525935159367,-1008.15588235294));
#158157=CARTESIAN_POINT('Ctrl Pts',(18.1253194172301,3.32956716117513E-15,
-1009.65));
#158158=CARTESIAN_POINT('Ctrl Pts',(17.9710104137728,-1.66525935159367,
-1011.14411764706));
#158159=CARTESIAN_POINT('Ctrl Pts',(17.8167014103155,-3.33051870318736,
-1012.63823529412));
#158160=CARTESIAN_POINT('Ctrl Pts',(17.3590292079831,-4.93906964482095,
-1014.13235294118));
#158161=CARTESIAN_POINT('Ctrl Pts',(16.9013570056506,-6.54762058645456,
-1015.62647058824));
#158162=CARTESIAN_POINT('Ctrl Pts',(16.1559070823762,-8.04468584505497,
-1017.12058823529));
#158163=CARTESIAN_POINT('Ctrl Pts',(15.4104571591017,-9.54175110365538,
-1018.61470588235));
#158164=CARTESIAN_POINT('Ctrl Pts',(14.4026149179538,-10.8763499173728,
-1020.10882352941));
#158165=CARTESIAN_POINT('Ctrl Pts',(13.3947726768058,-12.2109487310903,
-1021.60294117647));
#158166=CARTESIAN_POINT('Ctrl Pts',(12.1588589765331,-13.3376329379985,
-1023.09705882353));
#158167=CARTESIAN_POINT('Ctrl Pts',(10.9229452762603,-14.4643171449067,
-1024.59117647059));
#158168=CARTESIAN_POINT('Ctrl Pts',(9.50104767561053,-15.3447188656481,
-1026.08529411765));
#158169=CARTESIAN_POINT('Ctrl Pts',(8.07915007496071,-16.2251205863895,
-1027.57941176471));
#158170=CARTESIAN_POINT('Ctrl Pts',(6.51968959134574,-16.8292587962898,
-1029.07352941176));
#158171=CARTESIAN_POINT('Ctrl Pts',(4.96022910773078,-17.4333970061901,
-1030.56764705882));
#158172=CARTESIAN_POINT('Ctrl Pts',(3.31631129755346,-17.7406985030951,
-1032.06176470588));
#158173=CARTESIAN_POINT('Ctrl Pts',(1.67239348737615,-18.048,-1033.55588235294));
#158174=CARTESIAN_POINT('Ctrl Pts',(0.,-18.048,-1035.05));
#158175=CARTESIAN_POINT('Ctrl Pts',(-1.67239348737615,-18.048,-1036.54411764706));
#158176=CARTESIAN_POINT('Ctrl Pts',(-3.31631129755346,-17.7406985030951,
-1038.03823529412));
#158177=CARTESIAN_POINT('Ctrl Pts',(-4.96022910773077,-17.4333970061901,
-1039.53235294118));
#158178=CARTESIAN_POINT('Ctrl Pts',(-6.51968959134574,-16.8292587962898,
-1041.02647058824));
#158179=CARTESIAN_POINT('Ctrl Pts',(-8.07915007496071,-16.2251205863895,
-1042.52058823529));
#158180=CARTESIAN_POINT('Ctrl Pts',(-9.50104767561052,-15.3447188656481,
-1044.01470588235));
#158181=CARTESIAN_POINT('Ctrl Pts',(-10.9229452762603,-14.4643171449067,
-1045.50882352941));
#158182=CARTESIAN_POINT('Ctrl Pts',(-12.1588589765331,-13.3376329379985,
-1047.00294117647));
#158183=CARTESIAN_POINT('Ctrl Pts',(-13.3947726768058,-12.2109487310903,
-1048.49705882353));
#158184=CARTESIAN_POINT('Ctrl Pts',(-14.4026149179538,-10.8763499173728,
-1049.99117647059));
#158185=CARTESIAN_POINT('Ctrl Pts',(-15.4104571591017,-9.54175110365538,
-1051.48529411765));
#158186=CARTESIAN_POINT('Ctrl Pts',(-16.1559070823762,-8.04468584505497,
-1052.97941176471));
#158187=CARTESIAN_POINT('Ctrl Pts',(-16.9013570056506,-6.54762058645456,
-1054.47352941176));
#158188=CARTESIAN_POINT('Ctrl Pts',(-17.3590292079831,-4.93906964482095,
-1055.96764705882));
#158189=CARTESIAN_POINT('Ctrl Pts',(-17.8167014103155,-3.33051870318735,
-1057.46176470588));
#158190=CARTESIAN_POINT('Ctrl Pts',(-17.9710104137728,-1.66525935159368,
-1058.95588235294));
#158191=CARTESIAN_POINT('Ctrl Pts',(-18.1253194172301,-1.10985572039171E-15,
-1060.45));
#158192=CARTESIAN_POINT('Ctrl Pts',(-17.9710104137728,1.66525935159367,
-1061.94411764706));
#158193=CARTESIAN_POINT('Ctrl Pts',(-17.8167014103155,3.33051870318735,
-1063.43823529412));
#158194=CARTESIAN_POINT('Ctrl Pts',(-17.3590292079831,4.93906964482096,
-1064.93235294118));
#158195=CARTESIAN_POINT('Ctrl Pts',(-16.9013570056506,6.54762058645456,
-1066.42647058824));
#158196=CARTESIAN_POINT('Ctrl Pts',(-16.1559070823762,8.04468584505497,
-1067.92058823529));
#158197=CARTESIAN_POINT('Ctrl Pts',(-15.4104571591017,9.54175110365538,
-1069.41470588235));
#158198=CARTESIAN_POINT('Ctrl Pts',(-14.4026149179538,10.8763499173728,
-1070.90882352941));
#158199=CARTESIAN_POINT('Ctrl Pts',(-13.3947726768058,12.2109487310903,
-1072.40294117647));
#158200=CARTESIAN_POINT('Ctrl Pts',(-12.1588589765331,13.3376329379985,
-1073.89705882353));
#158201=CARTESIAN_POINT('Ctrl Pts',(-10.9229452762603,14.4643171449067,
-1075.39117647059));
#158202=CARTESIAN_POINT('Ctrl Pts',(-9.50104767561052,15.3447188656481,
-1076.88529411765));
#158203=CARTESIAN_POINT('Ctrl Pts',(-8.07915007496071,16.2251205863895,
-1078.37941176471));
#158204=CARTESIAN_POINT('Ctrl Pts',(-6.51968959134574,16.8292587962898,
-1079.87352941176));
#158205=CARTESIAN_POINT('Ctrl Pts',(-4.96022910773078,17.4333970061901,
-1081.36764705882));
#158206=CARTESIAN_POINT('Ctrl Pts',(-3.31631129755346,17.7406985030951,
-1082.86176470588));
#158207=CARTESIAN_POINT('Ctrl Pts',(-1.67239348737615,18.048,-1084.35588235294));
#158208=CARTESIAN_POINT('Ctrl Pts',(-2.21024254310115E-15,18.048,-1085.85));
#158209=CARTESIAN_POINT('Ctrl Pts',(1.67239348737616,18.048,-1087.34411764706));
#158210=CARTESIAN_POINT('Ctrl Pts',(3.31631129755346,17.7406985030951,-1088.83823529412));
#158211=CARTESIAN_POINT('Ctrl Pts',(4.96022910773077,17.4333970061901,-1090.33235294118));
#158212=CARTESIAN_POINT('Ctrl Pts',(6.51968959134575,16.8292587962898,-1091.82647058824));
#158213=CARTESIAN_POINT('Ctrl Pts',(8.07915007496071,16.2251205863895,-1093.32058823529));
#158214=CARTESIAN_POINT('Ctrl Pts',(9.50104767561053,15.3447188656481,-1094.81470588235));
#158215=CARTESIAN_POINT('Ctrl Pts',(10.9229452762603,14.4643171449067,-1096.30882352941));
#158216=CARTESIAN_POINT('Ctrl Pts',(12.1588589765331,13.3376329379985,-1097.80294117647));
#158217=CARTESIAN_POINT('Ctrl Pts',(13.3947726768058,12.2109487310903,-1099.29705882353));
#158218=CARTESIAN_POINT('Ctrl Pts',(14.4026149179538,10.8763499173728,-1100.79117647059));
#158219=CARTESIAN_POINT('Ctrl Pts',(15.4104571591017,9.54175110365538,-1102.28529411765));
#158220=CARTESIAN_POINT('Ctrl Pts',(16.1559070823762,8.04468584505496,-1103.77941176471));
#158221=CARTESIAN_POINT('Ctrl Pts',(16.9013570056506,6.54762058645456,-1105.27352941176));
#158222=CARTESIAN_POINT('Ctrl Pts',(17.3590292079831,4.93906964482096,-1106.76764705882));
#158223=CARTESIAN_POINT('Ctrl Pts',(17.8167014103155,3.33051870318735,-1108.26176470588));
#158224=CARTESIAN_POINT('Ctrl Pts',(17.9710104137728,1.66525935159367,-1109.75588235294));
#158225=CARTESIAN_POINT('Ctrl Pts',(18.1253194172301,3.32956716117513E-15,
-1111.25));
#158226=CARTESIAN_POINT('Ctrl Pts',(17.9710104137728,-1.66525935159367,
-1112.74411764706));
#158227=CARTESIAN_POINT('Ctrl Pts',(17.8167014103155,-3.33051870318736,
-1114.23823529412));
#158228=CARTESIAN_POINT('Ctrl Pts',(17.3590292079831,-4.93906964482095,
-1115.73235294118));
#158229=CARTESIAN_POINT('Ctrl Pts',(16.9013570056506,-6.54762058645456,
-1117.22647058824));
#158230=CARTESIAN_POINT('Ctrl Pts',(16.1559070823762,-8.04468584505497,
-1118.72058823529));
#158231=CARTESIAN_POINT('Ctrl Pts',(15.4104571591017,-9.54175110365538,
-1120.21470588235));
#158232=CARTESIAN_POINT('Ctrl Pts',(14.4026149179538,-10.8763499173728,
-1121.70882352941));
#158233=CARTESIAN_POINT('Ctrl Pts',(13.3947726768058,-12.2109487310903,
-1123.20294117647));
#158234=CARTESIAN_POINT('Ctrl Pts',(12.1588589765331,-13.3376329379985,
-1124.69705882353));
#158235=CARTESIAN_POINT('Ctrl Pts',(10.9229452762603,-14.4643171449067,
-1126.19117647059));
#158236=CARTESIAN_POINT('Ctrl Pts',(9.50104767561053,-15.3447188656481,
-1127.68529411765));
#158237=CARTESIAN_POINT('Ctrl Pts',(8.07915007496071,-16.2251205863895,
-1129.17941176471));
#158238=CARTESIAN_POINT('Ctrl Pts',(6.51968959134574,-16.8292587962898,
-1130.67352941176));
#158239=CARTESIAN_POINT('Ctrl Pts',(4.96022910773078,-17.4333970061901,
-1132.16764705882));
#158240=CARTESIAN_POINT('Ctrl Pts',(3.31631129755346,-17.7406985030951,
-1133.66176470588));
#158241=CARTESIAN_POINT('Ctrl Pts',(1.67239348737615,-18.048,-1135.15588235294));
#158242=CARTESIAN_POINT('Ctrl Pts',(0.,-18.048,-1136.65));
#158243=CARTESIAN_POINT('Ctrl Pts',(-1.67239348737615,-18.048,-1138.14411764706));
#158244=CARTESIAN_POINT('Ctrl Pts',(-3.31631129755346,-17.7406985030951,
-1139.63823529412));
#158245=CARTESIAN_POINT('Ctrl Pts',(-4.96022910773077,-17.4333970061901,
-1141.13235294118));
#158246=CARTESIAN_POINT('Ctrl Pts',(-6.51968959134574,-16.8292587962898,
-1142.62647058824));
#158247=CARTESIAN_POINT('Ctrl Pts',(-8.07915007496071,-16.2251205863895,
-1144.12058823529));
#158248=CARTESIAN_POINT('Ctrl Pts',(-9.50104767561052,-15.3447188656481,
-1145.61470588235));
#158249=CARTESIAN_POINT('Ctrl Pts',(-10.9229452762603,-14.4643171449067,
-1147.10882352941));
#158250=CARTESIAN_POINT('Ctrl Pts',(-12.1588589765331,-13.3376329379985,
-1148.60294117647));
#158251=CARTESIAN_POINT('Ctrl Pts',(-13.3947726768058,-12.2109487310903,
-1150.09705882353));
#158252=CARTESIAN_POINT('Ctrl Pts',(-14.4026149179538,-10.8763499173728,
-1151.59117647059));
#158253=CARTESIAN_POINT('Ctrl Pts',(-15.4104571591017,-9.54175110365538,
-1153.08529411765));
#158254=CARTESIAN_POINT('Ctrl Pts',(-16.1559070823762,-8.04468584505497,
-1154.57941176471));
#158255=CARTESIAN_POINT('Ctrl Pts',(-16.9013570056506,-6.54762058645456,
-1156.07352941176));
#158256=CARTESIAN_POINT('Ctrl Pts',(-17.3590292079831,-4.93906964482095,
-1157.56764705882));
#158257=CARTESIAN_POINT('Ctrl Pts',(-17.8167014103155,-3.33051870318735,
-1159.06176470588));
#158258=CARTESIAN_POINT('Ctrl Pts',(-17.9710104137728,-1.66525935159368,
-1160.55588235294));
#158259=CARTESIAN_POINT('Ctrl Pts',(-18.1253194172301,-1.10985572039171E-15,
-1162.05));
#158260=CARTESIAN_POINT('Ctrl Pts',(-17.9710104137728,1.66525935159367,
-1163.54411764706));
#158261=CARTESIAN_POINT('Ctrl Pts',(-17.8167014103155,3.33051870318735,
-1165.03823529412));
#158262=CARTESIAN_POINT('Ctrl Pts',(-17.3590292079831,4.93906964482096,
-1166.53235294118));
#158263=CARTESIAN_POINT('Ctrl Pts',(-16.9013570056506,6.54762058645456,
-1168.02647058824));
#158264=CARTESIAN_POINT('Ctrl Pts',(-16.1559070823762,8.04468584505497,
-1169.52058823529));
#158265=CARTESIAN_POINT('Ctrl Pts',(-15.4104571591017,9.54175110365538,
-1171.01470588235));
#158266=CARTESIAN_POINT('Ctrl Pts',(-14.4026149179538,10.8763499173728,
-1172.50882352941));
#158267=CARTESIAN_POINT('Ctrl Pts',(-13.3947726768058,12.2109487310903,
-1174.00294117647));
#158268=CARTESIAN_POINT('Ctrl Pts',(-12.1588589765331,13.3376329379985,
-1175.49705882353));
#158269=CARTESIAN_POINT('Ctrl Pts',(-10.9229452762603,14.4643171449067,
-1176.99117647059));
#158270=CARTESIAN_POINT('Ctrl Pts',(-9.50104767561052,15.3447188656481,
-1178.48529411765));
#158271=CARTESIAN_POINT('Ctrl Pts',(-8.07915007496071,16.2251205863895,
-1179.97941176471));
#158272=CARTESIAN_POINT('Ctrl Pts',(-6.51968959134574,16.8292587962898,
-1181.47352941176));
#158273=CARTESIAN_POINT('Ctrl Pts',(-4.96022910773078,17.4333970061901,
-1182.96764705882));
#158274=CARTESIAN_POINT('Ctrl Pts',(-3.31631129755346,17.7406985030951,
-1184.46176470588));
#158275=CARTESIAN_POINT('Ctrl Pts',(-1.67239348737615,18.048,-1185.95588235294));
#158276=CARTESIAN_POINT('Ctrl Pts',(-2.21024254310115E-15,18.048,-1187.45));
#158277=CARTESIAN_POINT('Ctrl Pts',(1.67239348737616,18.048,-1188.94411764706));
#158278=CARTESIAN_POINT('Ctrl Pts',(3.31631129755346,17.7406985030951,-1190.43823529412));
#158279=CARTESIAN_POINT('Ctrl Pts',(4.96022910773077,17.4333970061901,-1191.93235294118));
#158280=CARTESIAN_POINT('Ctrl Pts',(6.51968959134575,16.8292587962898,-1193.42647058824));
#158281=CARTESIAN_POINT('Ctrl Pts',(8.07915007496071,16.2251205863895,-1194.92058823529));
#158282=CARTESIAN_POINT('Ctrl Pts',(9.50104767561053,15.3447188656481,-1196.41470588235));
#158283=CARTESIAN_POINT('Ctrl Pts',(10.9229452762603,14.4643171449067,-1197.90882352941));
#158284=CARTESIAN_POINT('Ctrl Pts',(12.1588589765331,13.3376329379985,-1199.40294117647));
#158285=CARTESIAN_POINT('Ctrl Pts',(13.3947726768058,12.2109487310903,-1200.89705882353));
#158286=CARTESIAN_POINT('Ctrl Pts',(14.4026149179538,10.8763499173728,-1202.39117647059));
#158287=CARTESIAN_POINT('Ctrl Pts',(15.4104571591017,9.54175110365538,-1203.88529411765));
#158288=CARTESIAN_POINT('Ctrl Pts',(16.1559070823762,8.04468584505496,-1205.37941176471));
#158289=CARTESIAN_POINT('Ctrl Pts',(16.9013570056506,6.54762058645456,-1206.87352941176));
#158290=CARTESIAN_POINT('Ctrl Pts',(17.3590292079831,4.93906964482096,-1208.36764705882));
#158291=CARTESIAN_POINT('Ctrl Pts',(17.8167014103155,3.33051870318735,-1209.86176470588));
#158292=CARTESIAN_POINT('Ctrl Pts',(17.9710104137728,1.66525935159367,-1211.35588235294));
#158293=CARTESIAN_POINT('Ctrl Pts',(18.1253194172301,3.32956716117513E-15,
-1212.85));
#158294=CARTESIAN_POINT('Ctrl Pts',(17.9710104137728,-1.66525935159367,
-1214.34411764706));
#158295=CARTESIAN_POINT('Ctrl Pts',(17.8167014103155,-3.33051870318736,
-1215.83823529412));
#158296=CARTESIAN_POINT('Ctrl Pts',(17.3590292079831,-4.93906964482095,
-1217.33235294118));
#158297=CARTESIAN_POINT('Ctrl Pts',(16.9013570056506,-6.54762058645456,
-1218.82647058824));
#158298=CARTESIAN_POINT('Ctrl Pts',(16.1559070823762,-8.04468584505497,
-1220.32058823529));
#158299=CARTESIAN_POINT('Ctrl Pts',(15.4104571591017,-9.54175110365538,
-1221.81470588235));
#158300=CARTESIAN_POINT('Ctrl Pts',(14.4026149179538,-10.8763499173728,
-1223.30882352941));
#158301=CARTESIAN_POINT('Ctrl Pts',(13.3947726768058,-12.2109487310903,
-1224.80294117647));
#158302=CARTESIAN_POINT('Ctrl Pts',(12.1588589765331,-13.3376329379985,
-1226.29705882353));
#158303=CARTESIAN_POINT('Ctrl Pts',(10.9229452762603,-14.4643171449067,
-1227.79117647059));
#158304=CARTESIAN_POINT('Ctrl Pts',(9.50104767561053,-15.3447188656481,
-1229.28529411765));
#158305=CARTESIAN_POINT('Ctrl Pts',(8.07915007496071,-16.2251205863895,
-1230.77941176471));
#158306=CARTESIAN_POINT('Ctrl Pts',(6.51968959134574,-16.8292587962898,
-1232.27352941176));
#158307=CARTESIAN_POINT('Ctrl Pts',(4.96022910773078,-17.4333970061901,
-1233.76764705882));
#158308=CARTESIAN_POINT('Ctrl Pts',(3.31631129755346,-17.7406985030951,
-1235.26176470588));
#158309=CARTESIAN_POINT('Ctrl Pts',(1.67239348737615,-18.048,-1236.75588235294));
#158310=CARTESIAN_POINT('Ctrl Pts',(0.,-18.048,-1238.25));
#158311=CARTESIAN_POINT('Ctrl Pts',(-1.67239348737615,-18.048,-1239.74411764706));
#158312=CARTESIAN_POINT('Ctrl Pts',(-3.31631129755346,-17.7406985030951,
-1241.23823529412));
#158313=CARTESIAN_POINT('Ctrl Pts',(-4.96022910773077,-17.4333970061901,
-1242.73235294118));
#158314=CARTESIAN_POINT('Ctrl Pts',(-6.51968959134574,-16.8292587962898,
-1244.22647058824));
#158315=CARTESIAN_POINT('Ctrl Pts',(-8.07915007496071,-16.2251205863895,
-1245.72058823529));
#158316=CARTESIAN_POINT('Ctrl Pts',(-9.50104767561052,-15.3447188656481,
-1247.21470588235));
#158317=CARTESIAN_POINT('Ctrl Pts',(-10.9229452762603,-14.4643171449067,
-1248.70882352941));
#158318=CARTESIAN_POINT('Ctrl Pts',(-12.1588589765331,-13.3376329379985,
-1250.20294117647));
#158319=CARTESIAN_POINT('Ctrl Pts',(-13.3947726768058,-12.2109487310903,
-1251.69705882353));
#158320=CARTESIAN_POINT('Ctrl Pts',(-14.4026149179538,-10.8763499173728,
-1253.19117647059));
#158321=CARTESIAN_POINT('Ctrl Pts',(-15.4104571591017,-9.54175110365538,
-1254.68529411765));
#158322=CARTESIAN_POINT('Ctrl Pts',(-16.1559070823762,-8.04468584505497,
-1256.17941176471));
#158323=CARTESIAN_POINT('Ctrl Pts',(-16.9013570056506,-6.54762058645456,
-1257.67352941176));
#158324=CARTESIAN_POINT('Ctrl Pts',(-17.3590292079831,-4.93906964482095,
-1259.16764705882));
#158325=CARTESIAN_POINT('Ctrl Pts',(-17.8167014103155,-3.33051870318735,
-1260.66176470588));
#158326=CARTESIAN_POINT('Ctrl Pts',(-17.9710104137728,-1.66525935159368,
-1262.15588235294));
#158327=CARTESIAN_POINT('Ctrl Pts',(-18.1253194172301,-1.10985572039171E-15,
-1263.65));
#158328=CARTESIAN_POINT('Ctrl Pts',(-17.9710104137728,1.66525935159367,
-1265.14411764706));
#158329=CARTESIAN_POINT('Ctrl Pts',(-17.8167014103155,3.33051870318735,
-1266.63823529412));
#158330=CARTESIAN_POINT('Ctrl Pts',(-17.3590292079831,4.93906964482096,
-1268.13235294118));
#158331=CARTESIAN_POINT('Ctrl Pts',(-16.9013570056506,6.54762058645456,
-1269.62647058824));
#158332=CARTESIAN_POINT('Ctrl Pts',(-16.1559070823762,8.04468584505497,
-1271.12058823529));
#158333=CARTESIAN_POINT('Ctrl Pts',(-15.4104571591017,9.54175110365538,
-1272.61470588235));
#158334=CARTESIAN_POINT('Ctrl Pts',(-14.4026149179538,10.8763499173728,
-1274.10882352941));
#158335=CARTESIAN_POINT('Ctrl Pts',(-13.3947726768058,12.2109487310903,
-1275.60294117647));
#158336=CARTESIAN_POINT('Ctrl Pts',(-12.1588589765331,13.3376329379985,
-1277.09705882353));
#158337=CARTESIAN_POINT('Ctrl Pts',(-10.9229452762603,14.4643171449067,
-1278.59117647059));
#158338=CARTESIAN_POINT('Ctrl Pts',(-9.50104767561052,15.3447188656481,
-1280.08529411765));
#158339=CARTESIAN_POINT('Ctrl Pts',(-8.07915007496071,16.2251205863895,
-1281.57941176471));
#158340=CARTESIAN_POINT('Ctrl Pts',(-6.51968959134574,16.8292587962898,
-1283.07352941176));
#158341=CARTESIAN_POINT('Ctrl Pts',(-4.96022910773078,17.4333970061901,
-1284.56764705882));
#158342=CARTESIAN_POINT('Ctrl Pts',(-3.31631129755346,17.7406985030951,
-1286.06176470588));
#158343=CARTESIAN_POINT('Ctrl Pts',(-1.67239348737615,18.048,-1287.55588235294));
#158344=CARTESIAN_POINT('Ctrl Pts',(-2.21024254310115E-15,18.048,-1289.05));
#158345=CARTESIAN_POINT('Ctrl Pts',(1.67239348737616,18.048,-1290.54411764706));
#158346=CARTESIAN_POINT('Ctrl Pts',(3.31631129755346,17.7406985030951,-1292.03823529412));
#158347=CARTESIAN_POINT('Ctrl Pts',(4.96022910773077,17.4333970061901,-1293.53235294118));
#158348=CARTESIAN_POINT('Ctrl Pts',(6.51968959134575,16.8292587962898,-1295.02647058824));
#158349=CARTESIAN_POINT('Ctrl Pts',(8.07915007496071,16.2251205863895,-1296.52058823529));
#158350=CARTESIAN_POINT('Ctrl Pts',(9.50104767561053,15.3447188656481,-1298.01470588235));
#158351=CARTESIAN_POINT('Ctrl Pts',(10.9229452762603,14.4643171449067,-1299.50882352941));
#158352=CARTESIAN_POINT('Ctrl Pts',(12.1588589765331,13.3376329379985,-1301.00294117647));
#158353=CARTESIAN_POINT('Ctrl Pts',(13.3947726768058,12.2109487310903,-1302.49705882353));
#158354=CARTESIAN_POINT('Ctrl Pts',(14.4026149179538,10.8763499173728,-1303.99117647059));
#158355=CARTESIAN_POINT('Ctrl Pts',(15.4104571591017,9.54175110365538,-1305.48529411765));
#158356=CARTESIAN_POINT('Ctrl Pts',(16.1559070823762,8.04468584505496,-1306.97941176471));
#158357=CARTESIAN_POINT('Ctrl Pts',(16.9013570056506,6.54762058645456,-1308.47352941176));
#158358=CARTESIAN_POINT('Ctrl Pts',(17.3590292079831,4.93906964482096,-1309.96764705882));
#158359=CARTESIAN_POINT('Ctrl Pts',(17.8167014103155,3.33051870318735,-1311.46176470588));
#158360=CARTESIAN_POINT('Ctrl Pts',(17.9710104137728,1.66525935159367,-1312.95588235294));
#158361=CARTESIAN_POINT('Ctrl Pts',(18.1253194172301,3.32956716117513E-15,
-1314.45));
#158362=CARTESIAN_POINT('Ctrl Pts',(17.9710104137728,-1.66525935159367,
-1315.94411764706));
#158363=CARTESIAN_POINT('Ctrl Pts',(17.8167014103155,-3.33051870318736,
-1317.43823529412));
#158364=CARTESIAN_POINT('Ctrl Pts',(17.3590292079831,-4.93906964482095,
-1318.93235294118));
#158365=CARTESIAN_POINT('Ctrl Pts',(16.9013570056506,-6.54762058645456,
-1320.42647058824));
#158366=CARTESIAN_POINT('Ctrl Pts',(16.1559070823762,-8.04468584505497,
-1321.92058823529));
#158367=CARTESIAN_POINT('Ctrl Pts',(15.4104571591017,-9.54175110365538,
-1323.41470588235));
#158368=CARTESIAN_POINT('Ctrl Pts',(14.4026149179538,-10.8763499173728,
-1324.90882352941));
#158369=CARTESIAN_POINT('Ctrl Pts',(13.3947726768058,-12.2109487310903,
-1326.40294117647));
#158370=CARTESIAN_POINT('Ctrl Pts',(12.1588589765331,-13.3376329379985,
-1327.89705882353));
#158371=CARTESIAN_POINT('Ctrl Pts',(10.9229452762603,-14.4643171449067,
-1329.39117647059));
#158372=CARTESIAN_POINT('Ctrl Pts',(9.50104767561053,-15.3447188656481,
-1330.88529411765));
#158373=CARTESIAN_POINT('Ctrl Pts',(8.07915007496071,-16.2251205863895,
-1332.37941176471));
#158374=CARTESIAN_POINT('Ctrl Pts',(6.51968959134574,-16.8292587962898,
-1333.87352941176));
#158375=CARTESIAN_POINT('Ctrl Pts',(4.96022910773078,-17.4333970061901,
-1335.36764705882));
#158376=CARTESIAN_POINT('Ctrl Pts',(3.31631129755346,-17.7406985030951,
-1336.86176470588));
#158377=CARTESIAN_POINT('Ctrl Pts',(1.67239348737615,-18.048,-1338.35588235294));
#158378=CARTESIAN_POINT('Ctrl Pts',(0.,-18.048,-1339.85));
#158379=CARTESIAN_POINT('Ctrl Pts',(-1.67239348737615,-18.048,-1341.34411764706));
#158380=CARTESIAN_POINT('Ctrl Pts',(-3.31631129755346,-17.7406985030951,
-1342.83823529412));
#158381=CARTESIAN_POINT('Ctrl Pts',(-4.96022910773077,-17.4333970061901,
-1344.33235294118));
#158382=CARTESIAN_POINT('Ctrl Pts',(-6.51968959134574,-16.8292587962898,
-1345.82647058824));
#158383=CARTESIAN_POINT('Ctrl Pts',(-8.07915007496071,-16.2251205863895,
-1347.32058823529));
#158384=CARTESIAN_POINT('Ctrl Pts',(-9.50104767561052,-15.3447188656481,
-1348.81470588235));
#158385=CARTESIAN_POINT('Ctrl Pts',(-10.9229452762603,-14.4643171449067,
-1350.30882352941));
#158386=CARTESIAN_POINT('Ctrl Pts',(-12.1588589765331,-13.3376329379985,
-1351.80294117647));
#158387=CARTESIAN_POINT('Ctrl Pts',(-13.3947726768058,-12.2109487310903,
-1353.29705882353));
#158388=CARTESIAN_POINT('Ctrl Pts',(-14.4026149179538,-10.8763499173728,
-1354.79117647059));
#158389=CARTESIAN_POINT('Ctrl Pts',(-15.4104571591017,-9.54175110365538,
-1356.28529411765));
#158390=CARTESIAN_POINT('Ctrl Pts',(-16.1559070823762,-8.04468584505497,
-1357.77941176471));
#158391=CARTESIAN_POINT('Ctrl Pts',(-16.9013570056506,-6.54762058645456,
-1359.27352941176));
#158392=CARTESIAN_POINT('Ctrl Pts',(-17.3590292079831,-4.93906964482095,
-1360.76764705882));
#158393=CARTESIAN_POINT('Ctrl Pts',(-17.8167014103155,-3.33051870318735,
-1362.26176470588));
#158394=CARTESIAN_POINT('Ctrl Pts',(-17.9710104137728,-1.66525935159368,
-1363.75588235294));
#158395=CARTESIAN_POINT('Ctrl Pts',(-18.1253194172301,-1.10985572039171E-15,
-1365.25));
#158396=CARTESIAN_POINT('Ctrl Pts',(-17.9710104137728,1.66525935159367,
-1366.74411764706));
#158397=CARTESIAN_POINT('Ctrl Pts',(-17.8167014103155,3.33051870318735,
-1368.23823529412));
#158398=CARTESIAN_POINT('Ctrl Pts',(-17.3590292079831,4.93906964482096,
-1369.73235294118));
#158399=CARTESIAN_POINT('Ctrl Pts',(-16.9013570056506,6.54762058645456,
-1371.22647058824));
#158400=CARTESIAN_POINT('Ctrl Pts',(-16.1559070823762,8.04468584505497,
-1372.72058823529));
#158401=CARTESIAN_POINT('Ctrl Pts',(-15.4104571591017,9.54175110365538,
-1374.21470588235));
#158402=CARTESIAN_POINT('Ctrl Pts',(-14.4026149179538,10.8763499173728,
-1375.70882352941));
#158403=CARTESIAN_POINT('Ctrl Pts',(-13.3947726768058,12.2109487310903,
-1377.20294117647));
#158404=CARTESIAN_POINT('Ctrl Pts',(-12.1588589765331,13.3376329379985,
-1378.69705882353));
#158405=CARTESIAN_POINT('Ctrl Pts',(-10.9229452762603,14.4643171449067,
-1380.19117647059));
#158406=CARTESIAN_POINT('Ctrl Pts',(-9.50104767561052,15.3447188656481,
-1381.68529411765));
#158407=CARTESIAN_POINT('Ctrl Pts',(-8.07915007496071,16.2251205863895,
-1383.17941176471));
#158408=CARTESIAN_POINT('Ctrl Pts',(-6.51968959134574,16.8292587962898,
-1384.67352941176));
#158409=CARTESIAN_POINT('Ctrl Pts',(-4.96022910773078,17.4333970061901,
-1386.16764705882));
#158410=CARTESIAN_POINT('Ctrl Pts',(-3.31631129755346,17.7406985030951,
-1387.66176470588));
#158411=CARTESIAN_POINT('Ctrl Pts',(-1.67239348737615,18.048,-1389.15588235294));
#158412=CARTESIAN_POINT('Ctrl Pts',(-2.21024254310115E-15,18.048,-1390.65));
#158413=CARTESIAN_POINT('Ctrl Pts',(1.67239348737616,18.048,-1392.14411764706));
#158414=CARTESIAN_POINT('Ctrl Pts',(3.31631129755346,17.7406985030951,-1393.63823529412));
#158415=CARTESIAN_POINT('Ctrl Pts',(4.96022910773077,17.4333970061901,-1395.13235294118));
#158416=CARTESIAN_POINT('Ctrl Pts',(6.51968959134575,16.8292587962898,-1396.62647058824));
#158417=CARTESIAN_POINT('Ctrl Pts',(8.07915007496071,16.2251205863895,-1398.12058823529));
#158418=CARTESIAN_POINT('Ctrl Pts',(9.50104767561053,15.3447188656481,-1399.61470588235));
#158419=CARTESIAN_POINT('Ctrl Pts',(10.9229452762603,14.4643171449067,-1401.10882352941));
#158420=CARTESIAN_POINT('Ctrl Pts',(12.1588589765331,13.3376329379985,-1402.60294117647));
#158421=CARTESIAN_POINT('Ctrl Pts',(13.3947726768058,12.2109487310903,-1404.09705882353));
#158422=CARTESIAN_POINT('Ctrl Pts',(14.4026149179538,10.8763499173728,-1405.59117647059));
#158423=CARTESIAN_POINT('Ctrl Pts',(15.4104571591017,9.54175110365538,-1407.08529411765));
#158424=CARTESIAN_POINT('Ctrl Pts',(16.1559070823762,8.04468584505496,-1408.57941176471));
#158425=CARTESIAN_POINT('Ctrl Pts',(16.9013570056506,6.54762058645456,-1410.07352941176));
#158426=CARTESIAN_POINT('Ctrl Pts',(17.3590292079831,4.93906964482096,-1411.56764705882));
#158427=CARTESIAN_POINT('Ctrl Pts',(17.8167014103155,3.33051870318735,-1413.06176470588));
#158428=CARTESIAN_POINT('Ctrl Pts',(17.9710104137728,1.66525935159367,-1414.55588235294));
#158429=CARTESIAN_POINT('Ctrl Pts',(18.1253194172301,3.32956716117513E-15,
-1416.05));
#158430=CARTESIAN_POINT('Ctrl Pts',(17.9710104137728,-1.66525935159367,
-1417.54411764706));
#158431=CARTESIAN_POINT('Ctrl Pts',(17.8167014103155,-3.33051870318736,
-1419.03823529412));
#158432=CARTESIAN_POINT('Ctrl Pts',(17.3590292079831,-4.93906964482095,
-1420.53235294118));
#158433=CARTESIAN_POINT('Ctrl Pts',(16.9013570056506,-6.54762058645456,
-1422.02647058824));
#158434=CARTESIAN_POINT('Ctrl Pts',(16.1559070823762,-8.04468584505497,
-1423.52058823529));
#158435=CARTESIAN_POINT('Ctrl Pts',(15.4104571591017,-9.54175110365538,
-1425.01470588235));
#158436=CARTESIAN_POINT('Ctrl Pts',(14.4026149179538,-10.8763499173728,
-1426.50882352941));
#158437=CARTESIAN_POINT('Ctrl Pts',(13.3947726768058,-12.2109487310903,
-1428.00294117647));
#158438=CARTESIAN_POINT('Ctrl Pts',(12.1588589765331,-13.3376329379985,
-1429.49705882353));
#158439=CARTESIAN_POINT('Ctrl Pts',(10.9229452762603,-14.4643171449067,
-1430.99117647059));
#158440=CARTESIAN_POINT('Ctrl Pts',(9.50104767561053,-15.3447188656481,
-1432.48529411765));
#158441=CARTESIAN_POINT('Ctrl Pts',(8.07915007496071,-16.2251205863895,
-1433.97941176471));
#158442=CARTESIAN_POINT('Ctrl Pts',(6.51968959134574,-16.8292587962898,
-1435.47352941176));
#158443=CARTESIAN_POINT('Ctrl Pts',(4.96022910773078,-17.4333970061901,
-1436.96764705882));
#158444=CARTESIAN_POINT('Ctrl Pts',(3.31631129755346,-17.7406985030951,
-1438.46176470588));
#158445=CARTESIAN_POINT('Ctrl Pts',(1.67239348737615,-18.048,-1439.95588235294));
#158446=CARTESIAN_POINT('Ctrl Pts',(0.,-18.048,-1441.45));
#158447=CARTESIAN_POINT('Ctrl Pts',(-1.67239348737615,-18.048,-1442.94411764706));
#158448=CARTESIAN_POINT('Ctrl Pts',(-3.31631129755346,-17.7406985030951,
-1444.43823529412));
#158449=CARTESIAN_POINT('Ctrl Pts',(-4.96022910773077,-17.4333970061901,
-1445.93235294118));
#158450=CARTESIAN_POINT('Ctrl Pts',(-6.51968959134574,-16.8292587962898,
-1447.42647058824));
#158451=CARTESIAN_POINT('Ctrl Pts',(-8.07915007496071,-16.2251205863895,
-1448.92058823529));
#158452=CARTESIAN_POINT('Ctrl Pts',(-9.50104767561052,-15.3447188656481,
-1450.41470588235));
#158453=CARTESIAN_POINT('Ctrl Pts',(-10.9229452762603,-14.4643171449067,
-1451.90882352941));
#158454=CARTESIAN_POINT('Ctrl Pts',(-12.1588589765331,-13.3376329379985,
-1453.40294117647));
#158455=CARTESIAN_POINT('Ctrl Pts',(-13.3947726768058,-12.2109487310903,
-1454.89705882353));
#158456=CARTESIAN_POINT('Ctrl Pts',(-14.4026149179538,-10.8763499173728,
-1456.39117647059));
#158457=CARTESIAN_POINT('Ctrl Pts',(-15.4104571591017,-9.54175110365538,
-1457.88529411765));
#158458=CARTESIAN_POINT('Ctrl Pts',(-16.1559070823762,-8.04468584505497,
-1459.37941176471));
#158459=CARTESIAN_POINT('Ctrl Pts',(-16.9013570056506,-6.54762058645456,
-1460.87352941176));
#158460=CARTESIAN_POINT('Ctrl Pts',(-17.3590292079831,-4.93906964482095,
-1462.36764705882));
#158461=CARTESIAN_POINT('Ctrl Pts',(-17.8167014103155,-3.33051870318735,
-1463.86176470588));
#158462=CARTESIAN_POINT('Ctrl Pts',(-17.9710104137728,-1.66525935159368,
-1465.35588235294));
#158463=CARTESIAN_POINT('Ctrl Pts',(-18.1253194172301,-1.10985572039171E-15,
-1466.85));
#158464=CARTESIAN_POINT('Ctrl Pts',(-17.9710104137728,1.66525935159367,
-1468.34411764706));
#158465=CARTESIAN_POINT('Ctrl Pts',(-17.8167014103155,3.33051870318735,
-1469.83823529412));
#158466=CARTESIAN_POINT('Ctrl Pts',(-17.3590292079831,4.93906964482096,
-1471.33235294118));
#158467=CARTESIAN_POINT('Ctrl Pts',(-16.9013570056506,6.54762058645456,
-1472.82647058824));
#158468=CARTESIAN_POINT('Ctrl Pts',(-16.1559070823762,8.04468584505497,
-1474.32058823529));
#158469=CARTESIAN_POINT('Ctrl Pts',(-15.4104571591017,9.54175110365538,
-1475.81470588235));
#158470=CARTESIAN_POINT('Ctrl Pts',(-14.4026149179538,10.8763499173728,
-1477.30882352941));
#158471=CARTESIAN_POINT('Ctrl Pts',(-13.3947726768058,12.2109487310903,
-1478.80294117647));
#158472=CARTESIAN_POINT('Ctrl Pts',(-12.1588589765331,13.3376329379985,
-1480.29705882353));
#158473=CARTESIAN_POINT('Ctrl Pts',(-10.9229452762603,14.4643171449067,
-1481.79117647059));
#158474=CARTESIAN_POINT('Ctrl Pts',(-9.50104767561052,15.3447188656481,
-1483.28529411765));
#158475=CARTESIAN_POINT('Ctrl Pts',(-8.07915007496071,16.2251205863895,
-1484.77941176471));
#158476=CARTESIAN_POINT('Ctrl Pts',(-6.51968959134574,16.8292587962898,
-1486.27352941176));
#158477=CARTESIAN_POINT('Ctrl Pts',(-4.96022910773078,17.4333970061901,
-1487.76764705882));
#158478=CARTESIAN_POINT('Ctrl Pts',(-3.31631129755346,17.7406985030951,
-1489.26176470588));
#158479=CARTESIAN_POINT('Ctrl Pts',(-1.67239348737615,18.048,-1490.75588235294));
#158480=CARTESIAN_POINT('Ctrl Pts',(-2.21024254310115E-15,18.048,-1492.25));
#158481=CARTESIAN_POINT('Ctrl Pts',(1.67239348737616,18.048,-1493.74411764706));
#158482=CARTESIAN_POINT('Ctrl Pts',(3.31631129755346,17.7406985030951,-1495.23823529412));
#158483=CARTESIAN_POINT('Ctrl Pts',(4.96022910773077,17.4333970061901,-1496.73235294118));
#158484=CARTESIAN_POINT('Ctrl Pts',(6.51968959134575,16.8292587962898,-1498.22647058824));
#158485=CARTESIAN_POINT('Ctrl Pts',(7.54125551215708,16.4335020501724,-1499.20523195215));
#158486=CARTESIAN_POINT('Ctrl Pts',(8.50745084181327,15.9170846631577,-1500.18777724595));
#158487=CARTESIAN_POINT('Ctrl Pts',(23.3054395224043,8.00777438919566,-1515.23617759469));
#158488=CARTESIAN_POINT('Ctrl Pts',(38.1034282029954,0.0984641152335814,
-1530.28457794343));
#158489=CARTESIAN_POINT('',(-0.167825465190317,-18.0472196920532,692.));
#158490=CARTESIAN_POINT('',(-0.167825465190317,-18.0472196920532,692.));
#158491=CARTESIAN_POINT('Ctrl Pts',(-2.21024254310115E-15,18.048,742.95));
#158492=CARTESIAN_POINT('Ctrl Pts',(1.67239348737616,18.048,741.455882352941));
#158493=CARTESIAN_POINT('Ctrl Pts',(3.31631129755346,17.7406985030951,739.961764705882));
#158494=CARTESIAN_POINT('Ctrl Pts',(4.96022910773077,17.4333970061901,738.467647058824));
#158495=CARTESIAN_POINT('Ctrl Pts',(6.51968959134575,16.8292587962898,736.973529411765));
#158496=CARTESIAN_POINT('Ctrl Pts',(8.07915007496071,16.2251205863895,735.479411764706));
#158497=CARTESIAN_POINT('Ctrl Pts',(9.50104767561053,15.3447188656481,733.985294117647));
#158498=CARTESIAN_POINT('Ctrl Pts',(10.9229452762603,14.4643171449067,732.491176470588));
#158499=CARTESIAN_POINT('Ctrl Pts',(12.1588589765331,13.3376329379985,730.99705882353));
#158500=CARTESIAN_POINT('Ctrl Pts',(13.3947726768058,12.2109487310903,729.502941176471));
#158501=CARTESIAN_POINT('Ctrl Pts',(14.4026149179538,10.8763499173728,728.008823529412));
#158502=CARTESIAN_POINT('Ctrl Pts',(15.4104571591017,9.54175110365539,726.514705882353));
#158503=CARTESIAN_POINT('Ctrl Pts',(16.1559070823762,8.04468584505496,725.020588235294));
#158504=CARTESIAN_POINT('Ctrl Pts',(16.9013570056506,6.54762058645456,723.526470588235));
#158505=CARTESIAN_POINT('Ctrl Pts',(17.3590292079831,4.93906964482096,722.032352941177));
#158506=CARTESIAN_POINT('Ctrl Pts',(17.8167014103155,3.33051870318735,720.538235294118));
#158507=CARTESIAN_POINT('Ctrl Pts',(17.9710104137728,1.66525935159367,719.044117647059));
#158508=CARTESIAN_POINT('Ctrl Pts',(18.1253194172301,3.32956716117513E-15,
717.55));
#158509=CARTESIAN_POINT('Ctrl Pts',(17.9710104137728,-1.66525935159367,
716.055882352941));
#158510=CARTESIAN_POINT('Ctrl Pts',(17.8167014103155,-3.33051870318736,
714.561764705883));
#158511=CARTESIAN_POINT('Ctrl Pts',(17.3590292079831,-4.93906964482095,
713.067647058824));
#158512=CARTESIAN_POINT('Ctrl Pts',(16.9013570056506,-6.54762058645456,
711.573529411765));
#158513=CARTESIAN_POINT('Ctrl Pts',(16.1559070823762,-8.04468584505497,
710.079411764706));
#158514=CARTESIAN_POINT('Ctrl Pts',(15.4104571591017,-9.54175110365538,
708.585294117647));
#158515=CARTESIAN_POINT('Ctrl Pts',(14.4026149179538,-10.8763499173728,
707.091176470588));
#158516=CARTESIAN_POINT('Ctrl Pts',(13.3947726768058,-12.2109487310903,
705.597058823529));
#158517=CARTESIAN_POINT('Ctrl Pts',(12.1588589765331,-13.3376329379985,
704.102941176471));
#158518=CARTESIAN_POINT('Ctrl Pts',(10.9229452762603,-14.4643171449067,
702.608823529412));
#158519=CARTESIAN_POINT('Ctrl Pts',(9.50104767561053,-15.3447188656481,
701.114705882353));
#158520=CARTESIAN_POINT('Ctrl Pts',(8.07915007496071,-16.2251205863895,
699.620588235294));
#158521=CARTESIAN_POINT('Ctrl Pts',(6.51968959134574,-16.8292587962898,
698.126470588235));
#158522=CARTESIAN_POINT('Ctrl Pts',(4.96022910773078,-17.4333970061901,
696.632352941177));
#158523=CARTESIAN_POINT('Ctrl Pts',(3.31631129755346,-17.7406985030951,
695.138235294118));
#158524=CARTESIAN_POINT('Ctrl Pts',(1.67239348737615,-18.048,693.644117647059));
#158525=CARTESIAN_POINT('Ctrl Pts',(0.,-18.048,692.15));
#158526=CARTESIAN_POINT('Ctrl Pts',(-0.0839145466253093,-18.048,692.075030678543));
#158527=CARTESIAN_POINT('Ctrl Pts',(-0.167825465190317,-18.0472196920532,
692.));
#158528=CARTESIAN_POINT('',(0.,-15.0000000000001,1504.95));
#158529=CARTESIAN_POINT('Ctrl Pts',(0.,-18.048,1500.1875));
#158530=CARTESIAN_POINT('Ctrl Pts',(-1.67239348737615,-18.048,1498.69338235294));
#158531=CARTESIAN_POINT('Ctrl Pts',(-3.31631129755346,-17.7406985030951,
1497.19926470588));
#158532=CARTESIAN_POINT('Ctrl Pts',(-4.96022910773077,-17.4333970061901,
1495.70514705882));
#158533=CARTESIAN_POINT('Ctrl Pts',(-6.51968959134574,-16.8292587962898,
1494.21102941176));
#158534=CARTESIAN_POINT('Ctrl Pts',(-8.07915007496071,-16.2251205863895,
1492.71691176471));
#158535=CARTESIAN_POINT('Ctrl Pts',(-9.50104767561052,-15.3447188656481,
1491.22279411765));
#158536=CARTESIAN_POINT('Ctrl Pts',(-10.9229452762603,-14.4643171449067,
1489.72867647059));
#158537=CARTESIAN_POINT('Ctrl Pts',(-12.1588589765331,-13.3376329379985,
1488.23455882353));
#158538=CARTESIAN_POINT('Ctrl Pts',(-13.3947726768058,-12.2109487310903,
1486.74044117647));
#158539=CARTESIAN_POINT('Ctrl Pts',(-14.4026149179538,-10.8763499173728,
1485.24632352941));
#158540=CARTESIAN_POINT('Ctrl Pts',(-15.4104571591017,-9.54175110365538,
1483.75220588235));
#158541=CARTESIAN_POINT('Ctrl Pts',(-16.1559070823762,-8.04468584505497,
1482.25808823529));
#158542=CARTESIAN_POINT('Ctrl Pts',(-16.9013570056506,-6.54762058645456,
1480.76397058824));
#158543=CARTESIAN_POINT('Ctrl Pts',(-17.3590292079831,-4.93906964482095,
1479.26985294118));
#158544=CARTESIAN_POINT('Ctrl Pts',(-17.8167014103155,-3.33051870318735,
1477.77573529412));
#158545=CARTESIAN_POINT('Ctrl Pts',(-17.9710104137728,-1.66525935159368,
1476.28161764706));
#158546=CARTESIAN_POINT('Ctrl Pts',(-18.1253194172301,-1.10985572039171E-15,
1474.7875));
#158547=CARTESIAN_POINT('Ctrl Pts',(-17.9710104137728,1.66525935159367,
1473.29338235294));
#158548=CARTESIAN_POINT('Ctrl Pts',(-17.8167014103155,3.33051870318735,
1471.79926470588));
#158549=CARTESIAN_POINT('Ctrl Pts',(-17.3590292079831,4.93906964482096,
1470.30514705882));
#158550=CARTESIAN_POINT('Ctrl Pts',(-16.9013570056506,6.54762058645456,
1468.81102941177));
#158551=CARTESIAN_POINT('Ctrl Pts',(-16.1559070823762,8.04468584505497,
1467.31691176471));
#158552=CARTESIAN_POINT('Ctrl Pts',(-15.4104571591017,9.54175110365538,
1465.82279411765));
#158553=CARTESIAN_POINT('Ctrl Pts',(-14.4026149179538,10.8763499173728,
1464.32867647059));
#158554=CARTESIAN_POINT('Ctrl Pts',(-13.3947726768058,12.2109487310903,
1462.83455882353));
#158555=CARTESIAN_POINT('Ctrl Pts',(-12.1588589765331,13.3376329379985,
1461.34044117647));
#158556=CARTESIAN_POINT('Ctrl Pts',(-10.9229452762603,14.4643171449067,
1459.84632352941));
#158557=CARTESIAN_POINT('Ctrl Pts',(-9.50104767561052,15.3447188656481,
1458.35220588235));
#158558=CARTESIAN_POINT('Ctrl Pts',(-8.07915007496071,16.2251205863895,
1456.85808823529));
#158559=CARTESIAN_POINT('Ctrl Pts',(-6.51968959134574,16.8292587962898,
1455.36397058824));
#158560=CARTESIAN_POINT('Ctrl Pts',(-4.96022910773078,17.4333970061901,
1453.86985294118));
#158561=CARTESIAN_POINT('Ctrl Pts',(-3.31631129755346,17.7406985030951,
1452.37573529412));
#158562=CARTESIAN_POINT('Ctrl Pts',(-1.67239348737615,18.048,1450.88161764706));
#158563=CARTESIAN_POINT('Ctrl Pts',(-2.21024254310115E-15,18.048,1449.3875));
#158564=CARTESIAN_POINT('Ctrl Pts',(1.67239348737616,18.048,1447.89338235294));
#158565=CARTESIAN_POINT('Ctrl Pts',(3.31631129755346,17.7406985030951,1446.39926470588));
#158566=CARTESIAN_POINT('Ctrl Pts',(4.96022910773077,17.4333970061901,1444.90514705882));
#158567=CARTESIAN_POINT('Ctrl Pts',(6.51968959134575,16.8292587962898,1443.41102941176));
#158568=CARTESIAN_POINT('Ctrl Pts',(8.07915007496071,16.2251205863895,1441.91691176471));
#158569=CARTESIAN_POINT('Ctrl Pts',(9.50104767561053,15.3447188656481,1440.42279411765));
#158570=CARTESIAN_POINT('Ctrl Pts',(10.9229452762603,14.4643171449067,1438.92867647059));
#158571=CARTESIAN_POINT('Ctrl Pts',(12.1588589765331,13.3376329379985,1437.43455882353));
#158572=CARTESIAN_POINT('Ctrl Pts',(13.3947726768058,12.2109487310903,1435.94044117647));
#158573=CARTESIAN_POINT('Ctrl Pts',(14.4026149179538,10.8763499173728,1434.44632352941));
#158574=CARTESIAN_POINT('Ctrl Pts',(15.4104571591017,9.54175110365538,1432.95220588235));
#158575=CARTESIAN_POINT('Ctrl Pts',(16.1559070823762,8.04468584505496,1431.45808823529));
#158576=CARTESIAN_POINT('Ctrl Pts',(16.9013570056506,6.54762058645456,1429.96397058824));
#158577=CARTESIAN_POINT('Ctrl Pts',(17.3590292079831,4.93906964482096,1428.46985294118));
#158578=CARTESIAN_POINT('Ctrl Pts',(17.8167014103155,3.33051870318735,1426.97573529412));
#158579=CARTESIAN_POINT('Ctrl Pts',(17.9710104137728,1.66525935159367,1425.48161764706));
#158580=CARTESIAN_POINT('Ctrl Pts',(18.1253194172301,3.32956716117513E-15,
1423.9875));
#158581=CARTESIAN_POINT('Ctrl Pts',(17.9710104137728,-1.66525935159367,
1422.49338235294));
#158582=CARTESIAN_POINT('Ctrl Pts',(17.8167014103155,-3.33051870318736,
1420.99926470588));
#158583=CARTESIAN_POINT('Ctrl Pts',(17.3590292079831,-4.93906964482095,
1419.50514705882));
#158584=CARTESIAN_POINT('Ctrl Pts',(16.9013570056506,-6.54762058645456,
1418.01102941176));
#158585=CARTESIAN_POINT('Ctrl Pts',(16.1559070823762,-8.04468584505497,
1416.51691176471));
#158586=CARTESIAN_POINT('Ctrl Pts',(15.4104571591017,-9.54175110365538,
1415.02279411765));
#158587=CARTESIAN_POINT('Ctrl Pts',(14.4026149179538,-10.8763499173728,
1413.52867647059));
#158588=CARTESIAN_POINT('Ctrl Pts',(13.3947726768058,-12.2109487310903,
1412.03455882353));
#158589=CARTESIAN_POINT('Ctrl Pts',(12.1588589765331,-13.3376329379985,
1410.54044117647));
#158590=CARTESIAN_POINT('Ctrl Pts',(10.9229452762603,-14.4643171449067,
1409.04632352941));
#158591=CARTESIAN_POINT('Ctrl Pts',(9.50104767561053,-15.3447188656481,
1407.55220588235));
#158592=CARTESIAN_POINT('Ctrl Pts',(8.07915007496071,-16.2251205863895,
1406.05808823529));
#158593=CARTESIAN_POINT('Ctrl Pts',(6.51968959134574,-16.8292587962898,
1404.56397058824));
#158594=CARTESIAN_POINT('Ctrl Pts',(4.96022910773078,-17.4333970061901,
1403.06985294118));
#158595=CARTESIAN_POINT('Ctrl Pts',(3.31631129755346,-17.7406985030951,
1401.57573529412));
#158596=CARTESIAN_POINT('Ctrl Pts',(1.67239348737615,-18.048,1400.08161764706));
#158597=CARTESIAN_POINT('Ctrl Pts',(0.,-18.048,1398.5875));
#158598=CARTESIAN_POINT('Ctrl Pts',(-1.67239348737615,-18.048,1397.09338235294));
#158599=CARTESIAN_POINT('Ctrl Pts',(-3.31631129755346,-17.7406985030951,
1395.59926470588));
#158600=CARTESIAN_POINT('Ctrl Pts',(-4.96022910773077,-17.4333970061901,
1394.10514705882));
#158601=CARTESIAN_POINT('Ctrl Pts',(-6.51968959134574,-16.8292587962898,
1392.61102941176));
#158602=CARTESIAN_POINT('Ctrl Pts',(-8.07915007496071,-16.2251205863895,
1391.11691176471));
#158603=CARTESIAN_POINT('Ctrl Pts',(-9.50104767561052,-15.3447188656481,
1389.62279411765));
#158604=CARTESIAN_POINT('Ctrl Pts',(-10.9229452762603,-14.4643171449067,
1388.12867647059));
#158605=CARTESIAN_POINT('Ctrl Pts',(-12.1588589765331,-13.3376329379985,
1386.63455882353));
#158606=CARTESIAN_POINT('Ctrl Pts',(-13.3947726768058,-12.2109487310903,
1385.14044117647));
#158607=CARTESIAN_POINT('Ctrl Pts',(-14.4026149179538,-10.8763499173728,
1383.64632352941));
#158608=CARTESIAN_POINT('Ctrl Pts',(-15.4104571591017,-9.54175110365538,
1382.15220588235));
#158609=CARTESIAN_POINT('Ctrl Pts',(-16.1559070823762,-8.04468584505497,
1380.65808823529));
#158610=CARTESIAN_POINT('Ctrl Pts',(-16.9013570056506,-6.54762058645456,
1379.16397058824));
#158611=CARTESIAN_POINT('Ctrl Pts',(-17.3590292079831,-4.93906964482095,
1377.66985294118));
#158612=CARTESIAN_POINT('Ctrl Pts',(-17.8167014103155,-3.33051870318735,
1376.17573529412));
#158613=CARTESIAN_POINT('Ctrl Pts',(-17.9710104137728,-1.66525935159368,
1374.68161764706));
#158614=CARTESIAN_POINT('Ctrl Pts',(-18.1253194172301,-1.10985572039171E-15,
1373.1875));
#158615=CARTESIAN_POINT('Ctrl Pts',(-17.9710104137728,1.66525935159367,
1371.69338235294));
#158616=CARTESIAN_POINT('Ctrl Pts',(-17.8167014103155,3.33051870318735,
1370.19926470588));
#158617=CARTESIAN_POINT('Ctrl Pts',(-17.3590292079831,4.93906964482096,
1368.70514705882));
#158618=CARTESIAN_POINT('Ctrl Pts',(-16.9013570056506,6.54762058645456,
1367.21102941176));
#158619=CARTESIAN_POINT('Ctrl Pts',(-16.1559070823762,8.04468584505497,
1365.71691176471));
#158620=CARTESIAN_POINT('Ctrl Pts',(-15.4104571591017,9.54175110365538,
1364.22279411765));
#158621=CARTESIAN_POINT('Ctrl Pts',(-14.4026149179538,10.8763499173728,
1362.72867647059));
#158622=CARTESIAN_POINT('Ctrl Pts',(-13.3947726768058,12.2109487310903,
1361.23455882353));
#158623=CARTESIAN_POINT('Ctrl Pts',(-12.1588589765331,13.3376329379985,
1359.74044117647));
#158624=CARTESIAN_POINT('Ctrl Pts',(-10.9229452762603,14.4643171449067,
1358.24632352941));
#158625=CARTESIAN_POINT('Ctrl Pts',(-9.50104767561052,15.3447188656481,
1356.75220588235));
#158626=CARTESIAN_POINT('Ctrl Pts',(-8.07915007496071,16.2251205863895,
1355.25808823529));
#158627=CARTESIAN_POINT('Ctrl Pts',(-6.51968959134574,16.8292587962898,
1353.76397058824));
#158628=CARTESIAN_POINT('Ctrl Pts',(-4.96022910773078,17.4333970061901,
1352.26985294118));
#158629=CARTESIAN_POINT('Ctrl Pts',(-3.31631129755346,17.7406985030951,
1350.77573529412));
#158630=CARTESIAN_POINT('Ctrl Pts',(-1.67239348737615,18.048,1349.28161764706));
#158631=CARTESIAN_POINT('Ctrl Pts',(-2.21024254310115E-15,18.048,1347.7875));
#158632=CARTESIAN_POINT('Ctrl Pts',(1.67239348737616,18.048,1346.29338235294));
#158633=CARTESIAN_POINT('Ctrl Pts',(3.31631129755346,17.7406985030951,1344.79926470588));
#158634=CARTESIAN_POINT('Ctrl Pts',(4.96022910773077,17.4333970061901,1343.30514705882));
#158635=CARTESIAN_POINT('Ctrl Pts',(6.51968959134575,16.8292587962898,1341.81102941176));
#158636=CARTESIAN_POINT('Ctrl Pts',(8.07915007496071,16.2251205863895,1340.31691176471));
#158637=CARTESIAN_POINT('Ctrl Pts',(9.50104767561053,15.3447188656481,1338.82279411765));
#158638=CARTESIAN_POINT('Ctrl Pts',(10.9229452762603,14.4643171449067,1337.32867647059));
#158639=CARTESIAN_POINT('Ctrl Pts',(12.1588589765331,13.3376329379985,1335.83455882353));
#158640=CARTESIAN_POINT('Ctrl Pts',(13.3947726768058,12.2109487310903,1334.34044117647));
#158641=CARTESIAN_POINT('Ctrl Pts',(14.4026149179538,10.8763499173728,1332.84632352941));
#158642=CARTESIAN_POINT('Ctrl Pts',(15.4104571591017,9.54175110365538,1331.35220588235));
#158643=CARTESIAN_POINT('Ctrl Pts',(16.1559070823762,8.04468584505496,1329.85808823529));
#158644=CARTESIAN_POINT('Ctrl Pts',(16.9013570056506,6.54762058645456,1328.36397058824));
#158645=CARTESIAN_POINT('Ctrl Pts',(17.3590292079831,4.93906964482096,1326.86985294118));
#158646=CARTESIAN_POINT('Ctrl Pts',(17.8167014103155,3.33051870318735,1325.37573529412));
#158647=CARTESIAN_POINT('Ctrl Pts',(17.9710104137728,1.66525935159367,1323.88161764706));
#158648=CARTESIAN_POINT('Ctrl Pts',(18.1253194172301,3.32956716117513E-15,
1322.3875));
#158649=CARTESIAN_POINT('Ctrl Pts',(17.9710104137728,-1.66525935159367,
1320.89338235294));
#158650=CARTESIAN_POINT('Ctrl Pts',(17.8167014103155,-3.33051870318736,
1319.39926470588));
#158651=CARTESIAN_POINT('Ctrl Pts',(17.3590292079831,-4.93906964482095,
1317.90514705882));
#158652=CARTESIAN_POINT('Ctrl Pts',(16.9013570056506,-6.54762058645456,
1316.41102941176));
#158653=CARTESIAN_POINT('Ctrl Pts',(16.1559070823762,-8.04468584505497,
1314.91691176471));
#158654=CARTESIAN_POINT('Ctrl Pts',(15.4104571591017,-9.54175110365538,
1313.42279411765));
#158655=CARTESIAN_POINT('Ctrl Pts',(14.4026149179538,-10.8763499173728,
1311.92867647059));
#158656=CARTESIAN_POINT('Ctrl Pts',(13.3947726768058,-12.2109487310903,
1310.43455882353));
#158657=CARTESIAN_POINT('Ctrl Pts',(12.1588589765331,-13.3376329379985,
1308.94044117647));
#158658=CARTESIAN_POINT('Ctrl Pts',(10.9229452762603,-14.4643171449067,
1307.44632352941));
#158659=CARTESIAN_POINT('Ctrl Pts',(9.50104767561053,-15.3447188656481,
1305.95220588235));
#158660=CARTESIAN_POINT('Ctrl Pts',(8.07915007496071,-16.2251205863895,
1304.45808823529));
#158661=CARTESIAN_POINT('Ctrl Pts',(6.51968959134574,-16.8292587962898,
1302.96397058824));
#158662=CARTESIAN_POINT('Ctrl Pts',(4.96022910773078,-17.4333970061901,
1301.46985294118));
#158663=CARTESIAN_POINT('Ctrl Pts',(3.31631129755346,-17.7406985030951,
1299.97573529412));
#158664=CARTESIAN_POINT('Ctrl Pts',(1.67239348737615,-18.048,1298.48161764706));
#158665=CARTESIAN_POINT('Ctrl Pts',(0.,-18.048,1296.9875));
#158666=CARTESIAN_POINT('Ctrl Pts',(-1.67239348737615,-18.048,1295.49338235294));
#158667=CARTESIAN_POINT('Ctrl Pts',(-3.31631129755346,-17.7406985030951,
1293.99926470588));
#158668=CARTESIAN_POINT('Ctrl Pts',(-4.96022910773077,-17.4333970061901,
1292.50514705882));
#158669=CARTESIAN_POINT('Ctrl Pts',(-6.51968959134574,-16.8292587962898,
1291.01102941176));
#158670=CARTESIAN_POINT('Ctrl Pts',(-8.07915007496071,-16.2251205863895,
1289.51691176471));
#158671=CARTESIAN_POINT('Ctrl Pts',(-9.50104767561052,-15.3447188656481,
1288.02279411765));
#158672=CARTESIAN_POINT('Ctrl Pts',(-10.9229452762603,-14.4643171449067,
1286.52867647059));
#158673=CARTESIAN_POINT('Ctrl Pts',(-12.1588589765331,-13.3376329379985,
1285.03455882353));
#158674=CARTESIAN_POINT('Ctrl Pts',(-13.3947726768058,-12.2109487310903,
1283.54044117647));
#158675=CARTESIAN_POINT('Ctrl Pts',(-14.4026149179538,-10.8763499173728,
1282.04632352941));
#158676=CARTESIAN_POINT('Ctrl Pts',(-15.4104571591017,-9.54175110365538,
1280.55220588235));
#158677=CARTESIAN_POINT('Ctrl Pts',(-16.1559070823762,-8.04468584505497,
1279.05808823529));
#158678=CARTESIAN_POINT('Ctrl Pts',(-16.9013570056506,-6.54762058645456,
1277.56397058824));
#158679=CARTESIAN_POINT('Ctrl Pts',(-17.3590292079831,-4.93906964482095,
1276.06985294118));
#158680=CARTESIAN_POINT('Ctrl Pts',(-17.8167014103155,-3.33051870318735,
1274.57573529412));
#158681=CARTESIAN_POINT('Ctrl Pts',(-17.9710104137728,-1.66525935159368,
1273.08161764706));
#158682=CARTESIAN_POINT('Ctrl Pts',(-18.1253194172301,-1.10985572039171E-15,
1271.5875));
#158683=CARTESIAN_POINT('Ctrl Pts',(-17.9710104137728,1.66525935159367,
1270.09338235294));
#158684=CARTESIAN_POINT('Ctrl Pts',(-17.8167014103155,3.33051870318735,
1268.59926470588));
#158685=CARTESIAN_POINT('Ctrl Pts',(-17.3590292079831,4.93906964482096,
1267.10514705882));
#158686=CARTESIAN_POINT('Ctrl Pts',(-16.9013570056506,6.54762058645456,
1265.61102941176));
#158687=CARTESIAN_POINT('Ctrl Pts',(-16.1559070823762,8.04468584505497,
1264.11691176471));
#158688=CARTESIAN_POINT('Ctrl Pts',(-15.4104571591017,9.54175110365538,
1262.62279411765));
#158689=CARTESIAN_POINT('Ctrl Pts',(-14.4026149179538,10.8763499173728,
1261.12867647059));
#158690=CARTESIAN_POINT('Ctrl Pts',(-13.3947726768058,12.2109487310903,
1259.63455882353));
#158691=CARTESIAN_POINT('Ctrl Pts',(-12.1588589765331,13.3376329379985,
1258.14044117647));
#158692=CARTESIAN_POINT('Ctrl Pts',(-10.9229452762603,14.4643171449067,
1256.64632352941));
#158693=CARTESIAN_POINT('Ctrl Pts',(-9.50104767561052,15.3447188656481,
1255.15220588235));
#158694=CARTESIAN_POINT('Ctrl Pts',(-8.07915007496071,16.2251205863895,
1253.65808823529));
#158695=CARTESIAN_POINT('Ctrl Pts',(-6.51968959134574,16.8292587962898,
1252.16397058824));
#158696=CARTESIAN_POINT('Ctrl Pts',(-4.96022910773078,17.4333970061901,
1250.66985294118));
#158697=CARTESIAN_POINT('Ctrl Pts',(-3.31631129755346,17.7406985030951,
1249.17573529412));
#158698=CARTESIAN_POINT('Ctrl Pts',(-1.67239348737615,18.048,1247.68161764706));
#158699=CARTESIAN_POINT('Ctrl Pts',(-2.21024254310115E-15,18.048,1246.1875));
#158700=CARTESIAN_POINT('Ctrl Pts',(1.67239348737616,18.048,1244.69338235294));
#158701=CARTESIAN_POINT('Ctrl Pts',(3.31631129755346,17.7406985030951,1243.19926470588));
#158702=CARTESIAN_POINT('Ctrl Pts',(4.96022910773077,17.4333970061901,1241.70514705882));
#158703=CARTESIAN_POINT('Ctrl Pts',(6.51968959134575,16.8292587962898,1240.21102941176));
#158704=CARTESIAN_POINT('Ctrl Pts',(8.07915007496071,16.2251205863895,1238.71691176471));
#158705=CARTESIAN_POINT('Ctrl Pts',(9.50104767561053,15.3447188656481,1237.22279411765));
#158706=CARTESIAN_POINT('Ctrl Pts',(10.9229452762603,14.4643171449067,1235.72867647059));
#158707=CARTESIAN_POINT('Ctrl Pts',(12.1588589765331,13.3376329379985,1234.23455882353));
#158708=CARTESIAN_POINT('Ctrl Pts',(13.3947726768058,12.2109487310903,1232.74044117647));
#158709=CARTESIAN_POINT('Ctrl Pts',(14.4026149179538,10.8763499173728,1231.24632352941));
#158710=CARTESIAN_POINT('Ctrl Pts',(15.4104571591017,9.54175110365538,1229.75220588235));
#158711=CARTESIAN_POINT('Ctrl Pts',(16.1559070823762,8.04468584505496,1228.25808823529));
#158712=CARTESIAN_POINT('Ctrl Pts',(16.9013570056506,6.54762058645456,1226.76397058824));
#158713=CARTESIAN_POINT('Ctrl Pts',(17.3590292079831,4.93906964482096,1225.26985294118));
#158714=CARTESIAN_POINT('Ctrl Pts',(17.8167014103155,3.33051870318735,1223.77573529412));
#158715=CARTESIAN_POINT('Ctrl Pts',(17.9710104137728,1.66525935159367,1222.28161764706));
#158716=CARTESIAN_POINT('Ctrl Pts',(18.1253194172301,3.32956716117513E-15,
1220.7875));
#158717=CARTESIAN_POINT('Ctrl Pts',(17.9710104137728,-1.66525935159367,
1219.29338235294));
#158718=CARTESIAN_POINT('Ctrl Pts',(17.8167014103155,-3.33051870318736,
1217.79926470588));
#158719=CARTESIAN_POINT('Ctrl Pts',(17.3590292079831,-4.93906964482095,
1216.30514705882));
#158720=CARTESIAN_POINT('Ctrl Pts',(16.9013570056506,-6.54762058645456,
1214.81102941176));
#158721=CARTESIAN_POINT('Ctrl Pts',(16.1559070823762,-8.04468584505497,
1213.31691176471));
#158722=CARTESIAN_POINT('Ctrl Pts',(15.4104571591017,-9.54175110365538,
1211.82279411765));
#158723=CARTESIAN_POINT('Ctrl Pts',(14.4026149179538,-10.8763499173728,
1210.32867647059));
#158724=CARTESIAN_POINT('Ctrl Pts',(13.3947726768058,-12.2109487310903,
1208.83455882353));
#158725=CARTESIAN_POINT('Ctrl Pts',(12.1588589765331,-13.3376329379985,
1207.34044117647));
#158726=CARTESIAN_POINT('Ctrl Pts',(10.9229452762603,-14.4643171449067,
1205.84632352941));
#158727=CARTESIAN_POINT('Ctrl Pts',(9.50104767561053,-15.3447188656481,
1204.35220588235));
#158728=CARTESIAN_POINT('Ctrl Pts',(8.07915007496071,-16.2251205863895,
1202.85808823529));
#158729=CARTESIAN_POINT('Ctrl Pts',(6.51968959134574,-16.8292587962898,
1201.36397058824));
#158730=CARTESIAN_POINT('Ctrl Pts',(4.96022910773078,-17.4333970061901,
1199.86985294118));
#158731=CARTESIAN_POINT('Ctrl Pts',(3.31631129755346,-17.7406985030951,
1198.37573529412));
#158732=CARTESIAN_POINT('Ctrl Pts',(1.67239348737615,-18.048,1196.88161764706));
#158733=CARTESIAN_POINT('Ctrl Pts',(0.,-18.048,1195.3875));
#158734=CARTESIAN_POINT('Ctrl Pts',(-1.67239348737615,-18.048,1193.89338235294));
#158735=CARTESIAN_POINT('Ctrl Pts',(-3.31631129755346,-17.7406985030951,
1192.39926470588));
#158736=CARTESIAN_POINT('Ctrl Pts',(-4.96022910773077,-17.4333970061901,
1190.90514705882));
#158737=CARTESIAN_POINT('Ctrl Pts',(-6.51968959134574,-16.8292587962898,
1189.41102941176));
#158738=CARTESIAN_POINT('Ctrl Pts',(-8.07915007496071,-16.2251205863895,
1187.91691176471));
#158739=CARTESIAN_POINT('Ctrl Pts',(-9.50104767561052,-15.3447188656481,
1186.42279411765));
#158740=CARTESIAN_POINT('Ctrl Pts',(-10.9229452762603,-14.4643171449067,
1184.92867647059));
#158741=CARTESIAN_POINT('Ctrl Pts',(-12.1588589765331,-13.3376329379985,
1183.43455882353));
#158742=CARTESIAN_POINT('Ctrl Pts',(-13.3947726768058,-12.2109487310903,
1181.94044117647));
#158743=CARTESIAN_POINT('Ctrl Pts',(-14.4026149179538,-10.8763499173728,
1180.44632352941));
#158744=CARTESIAN_POINT('Ctrl Pts',(-15.4104571591017,-9.54175110365538,
1178.95220588235));
#158745=CARTESIAN_POINT('Ctrl Pts',(-16.1559070823762,-8.04468584505497,
1177.45808823529));
#158746=CARTESIAN_POINT('Ctrl Pts',(-16.9013570056506,-6.54762058645456,
1175.96397058824));
#158747=CARTESIAN_POINT('Ctrl Pts',(-17.3590292079831,-4.93906964482095,
1174.46985294118));
#158748=CARTESIAN_POINT('Ctrl Pts',(-17.8167014103155,-3.33051870318735,
1172.97573529412));
#158749=CARTESIAN_POINT('Ctrl Pts',(-17.9710104137728,-1.66525935159368,
1171.48161764706));
#158750=CARTESIAN_POINT('Ctrl Pts',(-18.1253194172301,-1.10985572039171E-15,
1169.9875));
#158751=CARTESIAN_POINT('Ctrl Pts',(-17.9710104137728,1.66525935159367,
1168.49338235294));
#158752=CARTESIAN_POINT('Ctrl Pts',(-17.8167014103155,3.33051870318735,
1166.99926470588));
#158753=CARTESIAN_POINT('Ctrl Pts',(-17.3590292079831,4.93906964482096,
1165.50514705882));
#158754=CARTESIAN_POINT('Ctrl Pts',(-16.9013570056506,6.54762058645456,
1164.01102941176));
#158755=CARTESIAN_POINT('Ctrl Pts',(-16.1559070823762,8.04468584505497,
1162.51691176471));
#158756=CARTESIAN_POINT('Ctrl Pts',(-15.4104571591017,9.54175110365538,
1161.02279411765));
#158757=CARTESIAN_POINT('Ctrl Pts',(-14.4026149179538,10.8763499173728,
1159.52867647059));
#158758=CARTESIAN_POINT('Ctrl Pts',(-13.3947726768058,12.2109487310903,
1158.03455882353));
#158759=CARTESIAN_POINT('Ctrl Pts',(-12.1588589765331,13.3376329379985,
1156.54044117647));
#158760=CARTESIAN_POINT('Ctrl Pts',(-10.9229452762603,14.4643171449067,
1155.04632352941));
#158761=CARTESIAN_POINT('Ctrl Pts',(-9.50104767561052,15.3447188656481,
1153.55220588235));
#158762=CARTESIAN_POINT('Ctrl Pts',(-8.07915007496071,16.2251205863895,
1152.05808823529));
#158763=CARTESIAN_POINT('Ctrl Pts',(-6.51968959134574,16.8292587962898,
1150.56397058824));
#158764=CARTESIAN_POINT('Ctrl Pts',(-4.96022910773078,17.4333970061901,
1149.06985294118));
#158765=CARTESIAN_POINT('Ctrl Pts',(-3.31631129755346,17.7406985030951,
1147.57573529412));
#158766=CARTESIAN_POINT('Ctrl Pts',(-1.67239348737615,18.048,1146.08161764706));
#158767=CARTESIAN_POINT('Ctrl Pts',(-2.21024254310115E-15,18.048,1144.5875));
#158768=CARTESIAN_POINT('Ctrl Pts',(1.67239348737616,18.048,1143.09338235294));
#158769=CARTESIAN_POINT('Ctrl Pts',(3.31631129755346,17.7406985030951,1141.59926470588));
#158770=CARTESIAN_POINT('Ctrl Pts',(4.96022910773077,17.4333970061901,1140.10514705882));
#158771=CARTESIAN_POINT('Ctrl Pts',(6.51968959134575,16.8292587962898,1138.61102941176));
#158772=CARTESIAN_POINT('Ctrl Pts',(8.07915007496071,16.2251205863895,1137.11691176471));
#158773=CARTESIAN_POINT('Ctrl Pts',(9.50104767561053,15.3447188656481,1135.62279411765));
#158774=CARTESIAN_POINT('Ctrl Pts',(10.9229452762603,14.4643171449067,1134.12867647059));
#158775=CARTESIAN_POINT('Ctrl Pts',(12.1588589765331,13.3376329379985,1132.63455882353));
#158776=CARTESIAN_POINT('Ctrl Pts',(13.3947726768058,12.2109487310903,1131.14044117647));
#158777=CARTESIAN_POINT('Ctrl Pts',(14.4026149179538,10.8763499173728,1129.64632352941));
#158778=CARTESIAN_POINT('Ctrl Pts',(15.4104571591017,9.54175110365538,1128.15220588235));
#158779=CARTESIAN_POINT('Ctrl Pts',(16.1559070823762,8.04468584505496,1126.65808823529));
#158780=CARTESIAN_POINT('Ctrl Pts',(16.9013570056506,6.54762058645456,1125.16397058824));
#158781=CARTESIAN_POINT('Ctrl Pts',(17.3590292079831,4.93906964482096,1123.66985294118));
#158782=CARTESIAN_POINT('Ctrl Pts',(17.8167014103155,3.33051870318735,1122.17573529412));
#158783=CARTESIAN_POINT('Ctrl Pts',(17.9710104137728,1.66525935159367,1120.68161764706));
#158784=CARTESIAN_POINT('Ctrl Pts',(18.1253194172301,3.32956716117513E-15,
1119.1875));
#158785=CARTESIAN_POINT('Ctrl Pts',(17.9710104137728,-1.66525935159367,
1117.69338235294));
#158786=CARTESIAN_POINT('Ctrl Pts',(17.8167014103155,-3.33051870318736,
1116.19926470588));
#158787=CARTESIAN_POINT('Ctrl Pts',(17.3590292079831,-4.93906964482095,
1114.70514705882));
#158788=CARTESIAN_POINT('Ctrl Pts',(16.9013570056506,-6.54762058645456,
1113.21102941176));
#158789=CARTESIAN_POINT('Ctrl Pts',(16.1559070823762,-8.04468584505497,
1111.71691176471));
#158790=CARTESIAN_POINT('Ctrl Pts',(15.4104571591017,-9.54175110365538,
1110.22279411765));
#158791=CARTESIAN_POINT('Ctrl Pts',(14.4026149179538,-10.8763499173728,
1108.72867647059));
#158792=CARTESIAN_POINT('Ctrl Pts',(13.3947726768058,-12.2109487310903,
1107.23455882353));
#158793=CARTESIAN_POINT('Ctrl Pts',(12.1588589765331,-13.3376329379985,
1105.74044117647));
#158794=CARTESIAN_POINT('Ctrl Pts',(10.9229452762603,-14.4643171449067,
1104.24632352941));
#158795=CARTESIAN_POINT('Ctrl Pts',(9.50104767561053,-15.3447188656481,
1102.75220588235));
#158796=CARTESIAN_POINT('Ctrl Pts',(8.07915007496071,-16.2251205863895,
1101.25808823529));
#158797=CARTESIAN_POINT('Ctrl Pts',(6.51968959134574,-16.8292587962898,
1099.76397058824));
#158798=CARTESIAN_POINT('Ctrl Pts',(4.96022910773078,-17.4333970061901,
1098.26985294118));
#158799=CARTESIAN_POINT('Ctrl Pts',(3.31631129755346,-17.7406985030951,
1096.77573529412));
#158800=CARTESIAN_POINT('Ctrl Pts',(1.67239348737615,-18.048,1095.28161764706));
#158801=CARTESIAN_POINT('Ctrl Pts',(0.,-18.048,1093.7875));
#158802=CARTESIAN_POINT('Ctrl Pts',(-1.67239348737615,-18.048,1092.29338235294));
#158803=CARTESIAN_POINT('Ctrl Pts',(-3.31631129755346,-17.7406985030951,
1090.79926470588));
#158804=CARTESIAN_POINT('Ctrl Pts',(-4.96022910773077,-17.4333970061901,
1089.30514705882));
#158805=CARTESIAN_POINT('Ctrl Pts',(-6.51968959134574,-16.8292587962898,
1087.81102941176));
#158806=CARTESIAN_POINT('Ctrl Pts',(-8.07915007496071,-16.2251205863895,
1086.31691176471));
#158807=CARTESIAN_POINT('Ctrl Pts',(-9.50104767561052,-15.3447188656481,
1084.82279411765));
#158808=CARTESIAN_POINT('Ctrl Pts',(-10.9229452762603,-14.4643171449067,
1083.32867647059));
#158809=CARTESIAN_POINT('Ctrl Pts',(-12.1588589765331,-13.3376329379985,
1081.83455882353));
#158810=CARTESIAN_POINT('Ctrl Pts',(-13.3947726768058,-12.2109487310903,
1080.34044117647));
#158811=CARTESIAN_POINT('Ctrl Pts',(-14.4026149179538,-10.8763499173728,
1078.84632352941));
#158812=CARTESIAN_POINT('Ctrl Pts',(-15.4104571591017,-9.54175110365538,
1077.35220588235));
#158813=CARTESIAN_POINT('Ctrl Pts',(-16.1559070823762,-8.04468584505497,
1075.85808823529));
#158814=CARTESIAN_POINT('Ctrl Pts',(-16.9013570056506,-6.54762058645456,
1074.36397058824));
#158815=CARTESIAN_POINT('Ctrl Pts',(-17.3590292079831,-4.93906964482095,
1072.86985294118));
#158816=CARTESIAN_POINT('Ctrl Pts',(-17.8167014103155,-3.33051870318735,
1071.37573529412));
#158817=CARTESIAN_POINT('Ctrl Pts',(-17.9710104137728,-1.66525935159368,
1069.88161764706));
#158818=CARTESIAN_POINT('Ctrl Pts',(-18.1253194172301,-1.10985572039171E-15,
1068.3875));
#158819=CARTESIAN_POINT('Ctrl Pts',(-17.9710104137728,1.66525935159367,
1066.89338235294));
#158820=CARTESIAN_POINT('Ctrl Pts',(-17.8167014103155,3.33051870318735,
1065.39926470588));
#158821=CARTESIAN_POINT('Ctrl Pts',(-17.3590292079831,4.93906964482096,
1063.90514705882));
#158822=CARTESIAN_POINT('Ctrl Pts',(-16.9013570056506,6.54762058645456,
1062.41102941176));
#158823=CARTESIAN_POINT('Ctrl Pts',(-16.1559070823762,8.04468584505497,
1060.91691176471));
#158824=CARTESIAN_POINT('Ctrl Pts',(-15.4104571591017,9.54175110365538,
1059.42279411765));
#158825=CARTESIAN_POINT('Ctrl Pts',(-14.4026149179538,10.8763499173728,
1057.92867647059));
#158826=CARTESIAN_POINT('Ctrl Pts',(-13.3947726768058,12.2109487310903,
1056.43455882353));
#158827=CARTESIAN_POINT('Ctrl Pts',(-12.1588589765331,13.3376329379985,
1054.94044117647));
#158828=CARTESIAN_POINT('Ctrl Pts',(-10.9229452762603,14.4643171449067,
1053.44632352941));
#158829=CARTESIAN_POINT('Ctrl Pts',(-9.50104767561052,15.3447188656481,
1051.95220588235));
#158830=CARTESIAN_POINT('Ctrl Pts',(-8.07915007496071,16.2251205863895,
1050.45808823529));
#158831=CARTESIAN_POINT('Ctrl Pts',(-6.51968959134574,16.8292587962898,
1048.96397058824));
#158832=CARTESIAN_POINT('Ctrl Pts',(-4.96022910773078,17.4333970061901,
1047.46985294118));
#158833=CARTESIAN_POINT('Ctrl Pts',(-3.31631129755346,17.7406985030951,
1045.97573529412));
#158834=CARTESIAN_POINT('Ctrl Pts',(-1.67239348737615,18.048,1044.48161764706));
#158835=CARTESIAN_POINT('Ctrl Pts',(-2.21024254310115E-15,18.048,1042.9875));
#158836=CARTESIAN_POINT('Ctrl Pts',(1.67239348737616,18.048,1041.49338235294));
#158837=CARTESIAN_POINT('Ctrl Pts',(3.31631129755346,17.7406985030951,1039.99926470588));
#158838=CARTESIAN_POINT('Ctrl Pts',(4.96022910773077,17.4333970061901,1038.50514705882));
#158839=CARTESIAN_POINT('Ctrl Pts',(6.51968959134575,16.8292587962898,1037.01102941176));
#158840=CARTESIAN_POINT('Ctrl Pts',(8.07915007496071,16.2251205863895,1035.51691176471));
#158841=CARTESIAN_POINT('Ctrl Pts',(9.50104767561053,15.3447188656481,1034.02279411765));
#158842=CARTESIAN_POINT('Ctrl Pts',(10.9229452762603,14.4643171449067,1032.52867647059));
#158843=CARTESIAN_POINT('Ctrl Pts',(12.1588589765331,13.3376329379985,1031.03455882353));
#158844=CARTESIAN_POINT('Ctrl Pts',(13.3947726768058,12.2109487310903,1029.54044117647));
#158845=CARTESIAN_POINT('Ctrl Pts',(14.4026149179538,10.8763499173728,1028.04632352941));
#158846=CARTESIAN_POINT('Ctrl Pts',(15.4104571591017,9.54175110365538,1026.55220588235));
#158847=CARTESIAN_POINT('Ctrl Pts',(16.1559070823762,8.04468584505496,1025.05808823529));
#158848=CARTESIAN_POINT('Ctrl Pts',(16.9013570056506,6.54762058645456,1023.56397058824));
#158849=CARTESIAN_POINT('Ctrl Pts',(17.3590292079831,4.93906964482096,1022.06985294118));
#158850=CARTESIAN_POINT('Ctrl Pts',(17.8167014103155,3.33051870318735,1020.57573529412));
#158851=CARTESIAN_POINT('Ctrl Pts',(17.9710104137728,1.66525935159367,1019.08161764706));
#158852=CARTESIAN_POINT('Ctrl Pts',(18.1253194172301,3.32956716117513E-15,
1017.5875));
#158853=CARTESIAN_POINT('Ctrl Pts',(17.9710104137728,-1.66525935159367,
1016.09338235294));
#158854=CARTESIAN_POINT('Ctrl Pts',(17.8167014103155,-3.33051870318736,
1014.59926470588));
#158855=CARTESIAN_POINT('Ctrl Pts',(17.3590292079831,-4.93906964482095,
1013.10514705882));
#158856=CARTESIAN_POINT('Ctrl Pts',(16.9013570056506,-6.54762058645456,
1011.61102941176));
#158857=CARTESIAN_POINT('Ctrl Pts',(16.1559070823762,-8.04468584505497,
1010.11691176471));
#158858=CARTESIAN_POINT('Ctrl Pts',(15.4104571591017,-9.54175110365538,
1008.62279411765));
#158859=CARTESIAN_POINT('Ctrl Pts',(14.4026149179538,-10.8763499173728,
1007.12867647059));
#158860=CARTESIAN_POINT('Ctrl Pts',(13.3947726768058,-12.2109487310903,
1005.63455882353));
#158861=CARTESIAN_POINT('Ctrl Pts',(12.1588589765331,-13.3376329379985,
1004.14044117647));
#158862=CARTESIAN_POINT('Ctrl Pts',(10.9229452762603,-14.4643171449067,
1002.64632352941));
#158863=CARTESIAN_POINT('Ctrl Pts',(9.50104767561053,-15.3447188656481,
1001.15220588235));
#158864=CARTESIAN_POINT('Ctrl Pts',(8.07915007496071,-16.2251205863895,
999.658088235294));
#158865=CARTESIAN_POINT('Ctrl Pts',(6.51968959134574,-16.8292587962898,
998.163970588235));
#158866=CARTESIAN_POINT('Ctrl Pts',(4.96022910773078,-17.4333970061901,
996.669852941177));
#158867=CARTESIAN_POINT('Ctrl Pts',(3.31631129755346,-17.7406985030951,
995.175735294118));
#158868=CARTESIAN_POINT('Ctrl Pts',(1.67239348737615,-18.048,993.681617647059));
#158869=CARTESIAN_POINT('Ctrl Pts',(0.,-18.048,992.1875));
#158870=CARTESIAN_POINT('Ctrl Pts',(-1.67239348737615,-18.048,990.693382352941));
#158871=CARTESIAN_POINT('Ctrl Pts',(-3.31631129755346,-17.7406985030951,
989.199264705882));
#158872=CARTESIAN_POINT('Ctrl Pts',(-4.96022910773077,-17.4333970061901,
987.705147058824));
#158873=CARTESIAN_POINT('Ctrl Pts',(-6.51968959134574,-16.8292587962898,
986.211029411765));
#158874=CARTESIAN_POINT('Ctrl Pts',(-8.07915007496071,-16.2251205863895,
984.716911764706));
#158875=CARTESIAN_POINT('Ctrl Pts',(-9.50104767561052,-15.3447188656481,
983.222794117647));
#158876=CARTESIAN_POINT('Ctrl Pts',(-10.9229452762603,-14.4643171449067,
981.728676470589));
#158877=CARTESIAN_POINT('Ctrl Pts',(-12.1588589765331,-13.3376329379985,
980.234558823529));
#158878=CARTESIAN_POINT('Ctrl Pts',(-13.3947726768058,-12.2109487310903,
978.740441176471));
#158879=CARTESIAN_POINT('Ctrl Pts',(-14.4026149179538,-10.8763499173728,
977.246323529412));
#158880=CARTESIAN_POINT('Ctrl Pts',(-15.4104571591017,-9.54175110365538,
975.752205882353));
#158881=CARTESIAN_POINT('Ctrl Pts',(-16.1559070823762,-8.04468584505497,
974.258088235294));
#158882=CARTESIAN_POINT('Ctrl Pts',(-16.9013570056506,-6.54762058645456,
972.763970588235));
#158883=CARTESIAN_POINT('Ctrl Pts',(-17.3590292079831,-4.93906964482095,
971.269852941177));
#158884=CARTESIAN_POINT('Ctrl Pts',(-17.8167014103155,-3.33051870318735,
969.775735294118));
#158885=CARTESIAN_POINT('Ctrl Pts',(-17.9710104137728,-1.66525935159368,
968.281617647059));
#158886=CARTESIAN_POINT('Ctrl Pts',(-18.1253194172301,-1.10985572039171E-15,
966.7875));
#158887=CARTESIAN_POINT('Ctrl Pts',(-17.9710104137728,1.66525935159367,
965.293382352941));
#158888=CARTESIAN_POINT('Ctrl Pts',(-17.8167014103155,3.33051870318735,
963.799264705882));
#158889=CARTESIAN_POINT('Ctrl Pts',(-17.3590292079831,4.93906964482096,
962.305147058824));
#158890=CARTESIAN_POINT('Ctrl Pts',(-16.9013570056506,6.54762058645456,
960.811029411765));
#158891=CARTESIAN_POINT('Ctrl Pts',(-16.1559070823762,8.04468584505497,
959.316911764706));
#158892=CARTESIAN_POINT('Ctrl Pts',(-15.4104571591017,9.54175110365538,
957.822794117647));
#158893=CARTESIAN_POINT('Ctrl Pts',(-14.4026149179538,10.8763499173728,
956.328676470588));
#158894=CARTESIAN_POINT('Ctrl Pts',(-13.3947726768058,12.2109487310903,
954.834558823529));
#158895=CARTESIAN_POINT('Ctrl Pts',(-12.1588589765331,13.3376329379985,
953.340441176471));
#158896=CARTESIAN_POINT('Ctrl Pts',(-10.9229452762603,14.4643171449067,
951.846323529412));
#158897=CARTESIAN_POINT('Ctrl Pts',(-9.50104767561052,15.3447188656481,
950.352205882353));
#158898=CARTESIAN_POINT('Ctrl Pts',(-8.07915007496071,16.2251205863895,
948.858088235294));
#158899=CARTESIAN_POINT('Ctrl Pts',(-6.51968959134574,16.8292587962898,
947.363970588235));
#158900=CARTESIAN_POINT('Ctrl Pts',(-4.96022910773078,17.4333970061901,
945.869852941177));
#158901=CARTESIAN_POINT('Ctrl Pts',(-3.31631129755346,17.7406985030951,
944.375735294118));
#158902=CARTESIAN_POINT('Ctrl Pts',(-1.67239348737615,18.048,942.881617647059));
#158903=CARTESIAN_POINT('Ctrl Pts',(-2.21024254310115E-15,18.048,941.3875));
#158904=CARTESIAN_POINT('Ctrl Pts',(1.67239348737616,18.048,939.893382352941));
#158905=CARTESIAN_POINT('Ctrl Pts',(3.31631129755346,17.7406985030951,938.399264705882));
#158906=CARTESIAN_POINT('Ctrl Pts',(4.96022910773077,17.4333970061901,936.905147058824));
#158907=CARTESIAN_POINT('Ctrl Pts',(6.51968959134575,16.8292587962898,935.411029411765));
#158908=CARTESIAN_POINT('Ctrl Pts',(8.07915007496071,16.2251205863895,933.916911764706));
#158909=CARTESIAN_POINT('Ctrl Pts',(9.50104767561053,15.3447188656481,932.422794117647));
#158910=CARTESIAN_POINT('Ctrl Pts',(10.9229452762603,14.4643171449067,930.928676470588));
#158911=CARTESIAN_POINT('Ctrl Pts',(12.1588589765331,13.3376329379985,929.43455882353));
#158912=CARTESIAN_POINT('Ctrl Pts',(13.3947726768058,12.2109487310903,927.94044117647));
#158913=CARTESIAN_POINT('Ctrl Pts',(14.4026149179538,10.8763499173728,926.446323529412));
#158914=CARTESIAN_POINT('Ctrl Pts',(15.4104571591017,9.54175110365538,924.952205882353));
#158915=CARTESIAN_POINT('Ctrl Pts',(16.1559070823762,8.04468584505496,923.458088235294));
#158916=CARTESIAN_POINT('Ctrl Pts',(16.9013570056506,6.54762058645456,921.963970588235));
#158917=CARTESIAN_POINT('Ctrl Pts',(17.3590292079831,4.93906964482096,920.469852941176));
#158918=CARTESIAN_POINT('Ctrl Pts',(17.8167014103155,3.33051870318735,918.975735294118));
#158919=CARTESIAN_POINT('Ctrl Pts',(17.9710104137728,1.66525935159367,917.481617647059));
#158920=CARTESIAN_POINT('Ctrl Pts',(18.1253194172301,3.32956716117513E-15,
915.9875));
#158921=CARTESIAN_POINT('Ctrl Pts',(17.9710104137728,-1.66525935159367,
914.493382352941));
#158922=CARTESIAN_POINT('Ctrl Pts',(17.8167014103155,-3.33051870318736,
912.999264705882));
#158923=CARTESIAN_POINT('Ctrl Pts',(17.3590292079831,-4.93906964482095,
911.505147058824));
#158924=CARTESIAN_POINT('Ctrl Pts',(16.9013570056506,-6.54762058645456,
910.011029411765));
#158925=CARTESIAN_POINT('Ctrl Pts',(16.1559070823762,-8.04468584505497,
908.516911764706));
#158926=CARTESIAN_POINT('Ctrl Pts',(15.4104571591017,-9.54175110365538,
907.022794117647));
#158927=CARTESIAN_POINT('Ctrl Pts',(14.4026149179538,-10.8763499173728,
905.528676470588));
#158928=CARTESIAN_POINT('Ctrl Pts',(13.3947726768058,-12.2109487310903,
904.034558823529));
#158929=CARTESIAN_POINT('Ctrl Pts',(12.1588589765331,-13.3376329379985,
902.540441176471));
#158930=CARTESIAN_POINT('Ctrl Pts',(10.9229452762603,-14.4643171449067,
901.046323529412));
#158931=CARTESIAN_POINT('Ctrl Pts',(9.50104767561053,-15.3447188656481,
899.552205882353));
#158932=CARTESIAN_POINT('Ctrl Pts',(8.07915007496071,-16.2251205863895,
898.058088235294));
#158933=CARTESIAN_POINT('Ctrl Pts',(6.51968959134574,-16.8292587962898,
896.563970588235));
#158934=CARTESIAN_POINT('Ctrl Pts',(4.96022910773078,-17.4333970061901,
895.069852941177));
#158935=CARTESIAN_POINT('Ctrl Pts',(3.31631129755346,-17.7406985030951,
893.575735294118));
#158936=CARTESIAN_POINT('Ctrl Pts',(1.67239348737615,-18.048,892.081617647059));
#158937=CARTESIAN_POINT('Ctrl Pts',(0.,-18.048,890.5875));
#158938=CARTESIAN_POINT('Ctrl Pts',(-1.67239348737615,-18.048,889.093382352941));
#158939=CARTESIAN_POINT('Ctrl Pts',(-3.31631129755346,-17.7406985030951,
887.599264705882));
#158940=CARTESIAN_POINT('Ctrl Pts',(-4.96022910773077,-17.4333970061901,
886.105147058824));
#158941=CARTESIAN_POINT('Ctrl Pts',(-6.51968959134574,-16.8292587962898,
884.611029411765));
#158942=CARTESIAN_POINT('Ctrl Pts',(-8.07915007496071,-16.2251205863895,
883.116911764706));
#158943=CARTESIAN_POINT('Ctrl Pts',(-9.50104767561052,-15.3447188656481,
881.622794117647));
#158944=CARTESIAN_POINT('Ctrl Pts',(-10.9229452762603,-14.4643171449067,
880.128676470588));
#158945=CARTESIAN_POINT('Ctrl Pts',(-12.1588589765331,-13.3376329379985,
878.634558823529));
#158946=CARTESIAN_POINT('Ctrl Pts',(-13.3947726768058,-12.2109487310903,
877.140441176471));
#158947=CARTESIAN_POINT('Ctrl Pts',(-14.4026149179538,-10.8763499173728,
875.646323529412));
#158948=CARTESIAN_POINT('Ctrl Pts',(-15.4104571591017,-9.54175110365538,
874.152205882353));
#158949=CARTESIAN_POINT('Ctrl Pts',(-16.1559070823762,-8.04468584505497,
872.658088235294));
#158950=CARTESIAN_POINT('Ctrl Pts',(-16.9013570056506,-6.54762058645456,
871.163970588236));
#158951=CARTESIAN_POINT('Ctrl Pts',(-17.3590292079831,-4.93906964482095,
869.669852941176));
#158952=CARTESIAN_POINT('Ctrl Pts',(-17.8167014103155,-3.33051870318735,
868.175735294118));
#158953=CARTESIAN_POINT('Ctrl Pts',(-17.9710104137728,-1.66525935159368,
866.681617647059));
#158954=CARTESIAN_POINT('Ctrl Pts',(-18.1253194172301,-1.10985572039171E-15,
865.1875));
#158955=CARTESIAN_POINT('Ctrl Pts',(-17.9710104137728,1.66525935159367,
863.693382352941));
#158956=CARTESIAN_POINT('Ctrl Pts',(-17.8167014103155,3.33051870318735,
862.199264705883));
#158957=CARTESIAN_POINT('Ctrl Pts',(-17.3590292079831,4.93906964482096,
860.705147058824));
#158958=CARTESIAN_POINT('Ctrl Pts',(-16.9013570056506,6.54762058645456,
859.211029411765));
#158959=CARTESIAN_POINT('Ctrl Pts',(-16.1559070823762,8.04468584505497,
857.716911764706));
#158960=CARTESIAN_POINT('Ctrl Pts',(-15.4104571591017,9.54175110365538,
856.222794117647));
#158961=CARTESIAN_POINT('Ctrl Pts',(-14.4026149179538,10.8763499173728,
854.728676470588));
#158962=CARTESIAN_POINT('Ctrl Pts',(-13.3947726768058,12.2109487310903,
853.234558823529));
#158963=CARTESIAN_POINT('Ctrl Pts',(-12.1588589765331,13.3376329379985,
851.740441176471));
#158964=CARTESIAN_POINT('Ctrl Pts',(-10.9229452762603,14.4643171449067,
850.246323529412));
#158965=CARTESIAN_POINT('Ctrl Pts',(-9.50104767561052,15.3447188656481,
848.752205882353));
#158966=CARTESIAN_POINT('Ctrl Pts',(-8.07915007496071,16.2251205863895,
847.258088235294));
#158967=CARTESIAN_POINT('Ctrl Pts',(-6.51968959134574,16.8292587962898,
845.763970588235));
#158968=CARTESIAN_POINT('Ctrl Pts',(-4.96022910773078,17.4333970061901,
844.269852941177));
#158969=CARTESIAN_POINT('Ctrl Pts',(-3.31631129755346,17.7406985030951,
842.775735294118));
#158970=CARTESIAN_POINT('Ctrl Pts',(-1.67239348737615,18.048,841.281617647059));
#158971=CARTESIAN_POINT('Ctrl Pts',(-2.21024254310115E-15,18.048,839.7875));
#158972=CARTESIAN_POINT('Ctrl Pts',(1.67239348737616,18.048,838.293382352941));
#158973=CARTESIAN_POINT('Ctrl Pts',(3.31631129755346,17.7406985030951,836.799264705882));
#158974=CARTESIAN_POINT('Ctrl Pts',(4.96022910773077,17.4333970061901,835.305147058824));
#158975=CARTESIAN_POINT('Ctrl Pts',(6.51968959134575,16.8292587962898,833.811029411765));
#158976=CARTESIAN_POINT('Ctrl Pts',(8.07915007496071,16.2251205863895,832.316911764706));
#158977=CARTESIAN_POINT('Ctrl Pts',(9.50104767561053,15.3447188656481,830.822794117647));
#158978=CARTESIAN_POINT('Ctrl Pts',(10.9229452762603,14.4643171449067,829.328676470588));
#158979=CARTESIAN_POINT('Ctrl Pts',(12.1588589765331,13.3376329379985,827.834558823529));
#158980=CARTESIAN_POINT('Ctrl Pts',(13.3947726768058,12.2109487310903,826.340441176471));
#158981=CARTESIAN_POINT('Ctrl Pts',(14.4026149179538,10.8763499173728,824.846323529412));
#158982=CARTESIAN_POINT('Ctrl Pts',(15.4104571591017,9.54175110365538,823.352205882353));
#158983=CARTESIAN_POINT('Ctrl Pts',(16.1559070823762,8.04468584505496,821.858088235294));
#158984=CARTESIAN_POINT('Ctrl Pts',(16.9013570056506,6.54762058645456,820.363970588236));
#158985=CARTESIAN_POINT('Ctrl Pts',(17.3590292079831,4.93906964482096,818.869852941177));
#158986=CARTESIAN_POINT('Ctrl Pts',(17.8167014103155,3.33051870318735,817.375735294118));
#158987=CARTESIAN_POINT('Ctrl Pts',(17.9710104137728,1.66525935159367,815.881617647059));
#158988=CARTESIAN_POINT('Ctrl Pts',(18.1253194172301,3.32956716117513E-15,
814.3875));
#158989=CARTESIAN_POINT('Ctrl Pts',(17.9710104137728,-1.66525935159367,
812.893382352941));
#158990=CARTESIAN_POINT('Ctrl Pts',(17.8167014103155,-3.33051870318736,
811.399264705883));
#158991=CARTESIAN_POINT('Ctrl Pts',(17.3590292079831,-4.93906964482095,
809.905147058824));
#158992=CARTESIAN_POINT('Ctrl Pts',(16.9013570056506,-6.54762058645456,
808.411029411765));
#158993=CARTESIAN_POINT('Ctrl Pts',(16.1559070823762,-8.04468584505497,
806.916911764706));
#158994=CARTESIAN_POINT('Ctrl Pts',(15.4104571591017,-9.54175110365538,
805.422794117647));
#158995=CARTESIAN_POINT('Ctrl Pts',(14.4026149179538,-10.8763499173728,
803.928676470588));
#158996=CARTESIAN_POINT('Ctrl Pts',(13.3947726768058,-12.2109487310903,
802.434558823529));
#158997=CARTESIAN_POINT('Ctrl Pts',(12.1588589765331,-13.3376329379985,
800.940441176471));
#158998=CARTESIAN_POINT('Ctrl Pts',(10.9229452762603,-14.4643171449067,
799.446323529412));
#158999=CARTESIAN_POINT('Ctrl Pts',(9.50104767561053,-15.3447188656481,
797.952205882353));
#159000=CARTESIAN_POINT('Ctrl Pts',(8.07915007496071,-16.2251205863895,
796.458088235294));
#159001=CARTESIAN_POINT('Ctrl Pts',(6.51968959134574,-16.8292587962898,
794.963970588235));
#159002=CARTESIAN_POINT('Ctrl Pts',(4.96022910773078,-17.4333970061901,
793.469852941176));
#159003=CARTESIAN_POINT('Ctrl Pts',(3.31631129755346,-17.7406985030951,
791.975735294118));
#159004=CARTESIAN_POINT('Ctrl Pts',(1.67239348737615,-18.048,790.481617647059));
#159005=CARTESIAN_POINT('Ctrl Pts',(0.,-18.048,788.9875));
#159006=CARTESIAN_POINT('Ctrl Pts',(-1.67239348737615,-18.048,787.493382352941));
#159007=CARTESIAN_POINT('Ctrl Pts',(-3.31631129755346,-17.7406985030951,
785.999264705882));
#159008=CARTESIAN_POINT('Ctrl Pts',(-4.96022910773077,-17.4333970061901,
784.505147058824));
#159009=CARTESIAN_POINT('Ctrl Pts',(-6.51968959134574,-16.8292587962898,
783.011029411765));
#159010=CARTESIAN_POINT('Ctrl Pts',(-8.07915007496071,-16.2251205863895,
781.516911764706));
#159011=CARTESIAN_POINT('Ctrl Pts',(-9.50104767561052,-15.3447188656481,
780.022794117647));
#159012=CARTESIAN_POINT('Ctrl Pts',(-10.9229452762603,-14.4643171449067,
778.528676470588));
#159013=CARTESIAN_POINT('Ctrl Pts',(-12.1588589765331,-13.3376329379985,
777.03455882353));
#159014=CARTESIAN_POINT('Ctrl Pts',(-13.3947726768058,-12.2109487310903,
775.540441176471));
#159015=CARTESIAN_POINT('Ctrl Pts',(-14.4026149179538,-10.8763499173728,
774.046323529412));
#159016=CARTESIAN_POINT('Ctrl Pts',(-15.4104571591017,-9.54175110365538,
772.552205882353));
#159017=CARTESIAN_POINT('Ctrl Pts',(-16.1559070823762,-8.04468584505497,
771.058088235294));
#159018=CARTESIAN_POINT('Ctrl Pts',(-16.9013570056506,-6.54762058645456,
769.563970588235));
#159019=CARTESIAN_POINT('Ctrl Pts',(-17.3590292079831,-4.93906964482095,
768.069852941177));
#159020=CARTESIAN_POINT('Ctrl Pts',(-17.8167014103155,-3.33051870318735,
766.575735294118));
#159021=CARTESIAN_POINT('Ctrl Pts',(-17.9710104137728,-1.66525935159368,
765.081617647059));
#159022=CARTESIAN_POINT('Ctrl Pts',(-18.1253194172301,-1.10985572039171E-15,
763.5875));
#159023=CARTESIAN_POINT('Ctrl Pts',(-17.9710104137728,1.66525935159367,
762.093382352941));
#159024=CARTESIAN_POINT('Ctrl Pts',(-17.8167014103155,3.33051870318735,
760.599264705883));
#159025=CARTESIAN_POINT('Ctrl Pts',(-17.3590292079831,4.93906964482096,
759.105147058824));
#159026=CARTESIAN_POINT('Ctrl Pts',(-16.9013570056506,6.54762058645456,
757.611029411765));
#159027=CARTESIAN_POINT('Ctrl Pts',(-16.1559070823762,8.04468584505497,
756.116911764706));
#159028=CARTESIAN_POINT('Ctrl Pts',(-15.4104571591017,9.54175110365538,
754.622794117647));
#159029=CARTESIAN_POINT('Ctrl Pts',(-14.4026149179538,10.8763499173728,
753.128676470588));
#159030=CARTESIAN_POINT('Ctrl Pts',(-13.3947726768058,12.2109487310903,
751.634558823529));
#159031=CARTESIAN_POINT('Ctrl Pts',(-12.1588589765331,13.3376329379985,
750.140441176471));
#159032=CARTESIAN_POINT('Ctrl Pts',(-10.9229452762603,14.4643171449067,
748.646323529412));
#159033=CARTESIAN_POINT('Ctrl Pts',(-9.50104767561052,15.3447188656481,
747.152205882353));
#159034=CARTESIAN_POINT('Ctrl Pts',(-8.07915007496071,16.2251205863895,
745.658088235294));
#159035=CARTESIAN_POINT('Ctrl Pts',(-6.51968959134574,16.8292587962898,
744.163970588235));
#159036=CARTESIAN_POINT('Ctrl Pts',(-4.96022910773078,17.4333970061901,
742.669852941176));
#159037=CARTESIAN_POINT('Ctrl Pts',(-3.31631129755346,17.7406985030951,
741.175735294118));
#159038=CARTESIAN_POINT('Ctrl Pts',(-1.67239348737615,18.048,739.681617647059));
#159039=CARTESIAN_POINT('Ctrl Pts',(-2.21024254310115E-15,18.048,738.1875));
#159040=CARTESIAN_POINT('Ctrl Pts',(1.67239348737616,18.048,736.693382352941));
#159041=CARTESIAN_POINT('Ctrl Pts',(3.31631129755346,17.7406985030951,735.199264705882));
#159042=CARTESIAN_POINT('Ctrl Pts',(4.96022910773077,17.4333970061901,733.705147058824));
#159043=CARTESIAN_POINT('Ctrl Pts',(6.51968959134575,16.8292587962898,732.211029411765));
#159044=CARTESIAN_POINT('Ctrl Pts',(8.07915007496071,16.2251205863895,730.716911764706));
#159045=CARTESIAN_POINT('Ctrl Pts',(9.50104767561053,15.3447188656481,729.222794117647));
#159046=CARTESIAN_POINT('Ctrl Pts',(10.9229452762603,14.4643171449067,727.728676470588));
#159047=CARTESIAN_POINT('Ctrl Pts',(12.1588589765331,13.3376329379985,726.234558823529));
#159048=CARTESIAN_POINT('Ctrl Pts',(13.3947726768058,12.2109487310903,724.740441176471));
#159049=CARTESIAN_POINT('Ctrl Pts',(14.4026149179538,10.8763499173728,723.246323529412));
#159050=CARTESIAN_POINT('Ctrl Pts',(15.4104571591017,9.54175110365538,721.752205882353));
#159051=CARTESIAN_POINT('Ctrl Pts',(16.1559070823762,8.04468584505496,720.258088235294));
#159052=CARTESIAN_POINT('Ctrl Pts',(16.9013570056506,6.54762058645456,718.763970588235));
#159053=CARTESIAN_POINT('Ctrl Pts',(17.3590292079831,4.93906964482096,717.269852941177));
#159054=CARTESIAN_POINT('Ctrl Pts',(17.8167014103155,3.33051870318735,715.775735294118));
#159055=CARTESIAN_POINT('Ctrl Pts',(17.9710104137728,1.66525935159367,714.281617647059));
#159056=CARTESIAN_POINT('Ctrl Pts',(18.1253194172301,3.32956716117513E-15,
712.7875));
#159057=CARTESIAN_POINT('Ctrl Pts',(17.9710104137728,-1.66525935159367,
711.293382352941));
#159058=CARTESIAN_POINT('Ctrl Pts',(17.8167014103155,-3.33051870318736,
709.799264705883));
#159059=CARTESIAN_POINT('Ctrl Pts',(17.3590292079831,-4.93906964482095,
708.305147058824));
#159060=CARTESIAN_POINT('Ctrl Pts',(16.9013570056506,-6.54762058645456,
706.811029411765));
#159061=CARTESIAN_POINT('Ctrl Pts',(16.1559070823762,-8.04468584505497,
705.316911764706));
#159062=CARTESIAN_POINT('Ctrl Pts',(15.4104571591017,-9.54175110365538,
703.822794117647));
#159063=CARTESIAN_POINT('Ctrl Pts',(14.4026149179538,-10.8763499173728,
702.328676470588));
#159064=CARTESIAN_POINT('Ctrl Pts',(13.3947726768058,-12.2109487310903,
700.83455882353));
#159065=CARTESIAN_POINT('Ctrl Pts',(12.1588589765331,-13.3376329379985,
699.340441176471));
#159066=CARTESIAN_POINT('Ctrl Pts',(10.9229452762603,-14.4643171449067,
697.846323529412));
#159067=CARTESIAN_POINT('Ctrl Pts',(9.50104767561053,-15.3447188656481,
696.352205882353));
#159068=CARTESIAN_POINT('Ctrl Pts',(8.07915007496071,-16.2251205863895,
694.858088235294));
#159069=CARTESIAN_POINT('Ctrl Pts',(6.51968959134574,-16.8292587962898,
693.363970588235));
#159070=CARTESIAN_POINT('Ctrl Pts',(4.96022910773078,-17.4333970061901,
691.869852941177));
#159071=CARTESIAN_POINT('Ctrl Pts',(3.31631129755346,-17.7406985030951,
690.375735294118));
#159072=CARTESIAN_POINT('Ctrl Pts',(1.67239348737615,-18.048,688.881617647059));
#159073=CARTESIAN_POINT('Ctrl Pts',(0.,-18.048,687.3875));
#159074=CARTESIAN_POINT('Ctrl Pts',(-1.67239348737615,-18.048,685.893382352941));
#159075=CARTESIAN_POINT('Ctrl Pts',(-3.31631129755346,-17.7406985030951,
684.399264705883));
#159076=CARTESIAN_POINT('Ctrl Pts',(-4.96022910773077,-17.4333970061901,
682.905147058824));
#159077=CARTESIAN_POINT('Ctrl Pts',(-6.51968959134574,-16.8292587962898,
681.411029411765));
#159078=CARTESIAN_POINT('Ctrl Pts',(-8.07915007496071,-16.2251205863895,
679.916911764706));
#159079=CARTESIAN_POINT('Ctrl Pts',(-9.50104767561052,-15.3447188656481,
678.422794117647));
#159080=CARTESIAN_POINT('Ctrl Pts',(-10.9229452762603,-14.4643171449067,
676.928676470588));
#159081=CARTESIAN_POINT('Ctrl Pts',(-12.1588589765331,-13.3376329379985,
675.434558823529));
#159082=CARTESIAN_POINT('Ctrl Pts',(-13.3947726768058,-12.2109487310903,
673.940441176471));
#159083=CARTESIAN_POINT('Ctrl Pts',(-14.4026149179538,-10.8763499173728,
672.446323529412));
#159084=CARTESIAN_POINT('Ctrl Pts',(-15.4104571591017,-9.54175110365538,
670.952205882353));
#159085=CARTESIAN_POINT('Ctrl Pts',(-16.1559070823762,-8.04468584505497,
669.458088235294));
#159086=CARTESIAN_POINT('Ctrl Pts',(-16.9013570056506,-6.54762058645456,
667.963970588235));
#159087=CARTESIAN_POINT('Ctrl Pts',(-17.3590292079831,-4.93906964482095,
666.469852941176));
#159088=CARTESIAN_POINT('Ctrl Pts',(-17.8167014103155,-3.33051870318735,
664.975735294118));
#159089=CARTESIAN_POINT('Ctrl Pts',(-17.9710104137728,-1.66525935159368,
663.481617647059));
#159090=CARTESIAN_POINT('Ctrl Pts',(-18.1253194172301,-1.10985572039171E-15,
661.9875));
#159091=CARTESIAN_POINT('Ctrl Pts',(-17.9710104137728,1.66525935159367,
660.493382352941));
#159092=CARTESIAN_POINT('Ctrl Pts',(-17.8167014103155,3.33051870318735,
658.999264705882));
#159093=CARTESIAN_POINT('Ctrl Pts',(-17.3590292079831,4.93906964482096,
657.505147058824));
#159094=CARTESIAN_POINT('Ctrl Pts',(-16.9013570056506,6.54762058645456,
656.011029411765));
#159095=CARTESIAN_POINT('Ctrl Pts',(-16.1559070823762,8.04468584505497,
654.516911764706));
#159096=CARTESIAN_POINT('Ctrl Pts',(-15.4104571591017,9.54175110365538,
653.022794117647));
#159097=CARTESIAN_POINT('Ctrl Pts',(-14.4026149179538,10.8763499173728,
651.528676470588));
#159098=CARTESIAN_POINT('Ctrl Pts',(-13.3947726768058,12.2109487310903,
650.03455882353));
#159099=CARTESIAN_POINT('Ctrl Pts',(-12.1588589765331,13.3376329379985,
648.540441176471));
#159100=CARTESIAN_POINT('Ctrl Pts',(-10.9229452762603,14.4643171449067,
647.046323529412));
#159101=CARTESIAN_POINT('Ctrl Pts',(-9.50104767561052,15.3447188656481,
645.552205882353));
#159102=CARTESIAN_POINT('Ctrl Pts',(-8.07915007496071,16.2251205863895,
644.058088235294));
#159103=CARTESIAN_POINT('Ctrl Pts',(-6.51968959134574,16.8292587962898,
642.563970588235));
#159104=CARTESIAN_POINT('Ctrl Pts',(-4.96022910773078,17.4333970061901,
641.069852941176));
#159105=CARTESIAN_POINT('Ctrl Pts',(-3.31631129755346,17.7406985030951,
639.575735294118));
#159106=CARTESIAN_POINT('Ctrl Pts',(-1.67239348737615,18.048,638.081617647059));
#159107=CARTESIAN_POINT('Ctrl Pts',(-2.21024254310115E-15,18.048,636.5875));
#159108=CARTESIAN_POINT('Ctrl Pts',(1.67239348737616,18.048,635.093382352941));
#159109=CARTESIAN_POINT('Ctrl Pts',(3.31631129755346,17.7406985030951,633.599264705882));
#159110=CARTESIAN_POINT('Ctrl Pts',(4.96022910773077,17.4333970061901,632.105147058824));
#159111=CARTESIAN_POINT('Ctrl Pts',(6.51968959134575,16.8292587962898,630.611029411765));
#159112=CARTESIAN_POINT('Ctrl Pts',(8.07915007496071,16.2251205863895,629.116911764706));
#159113=CARTESIAN_POINT('Ctrl Pts',(9.50104767561053,15.3447188656481,627.622794117647));
#159114=CARTESIAN_POINT('Ctrl Pts',(10.9229452762603,14.4643171449067,626.128676470588));
#159115=CARTESIAN_POINT('Ctrl Pts',(12.1588589765331,13.3376329379985,624.634558823529));
#159116=CARTESIAN_POINT('Ctrl Pts',(13.3947726768058,12.2109487310903,623.140441176471));
#159117=CARTESIAN_POINT('Ctrl Pts',(14.4026149179538,10.8763499173728,621.646323529412));
#159118=CARTESIAN_POINT('Ctrl Pts',(15.4104571591017,9.54175110365538,620.152205882353));
#159119=CARTESIAN_POINT('Ctrl Pts',(16.1559070823762,8.04468584505496,618.658088235294));
#159120=CARTESIAN_POINT('Ctrl Pts',(16.9013570056506,6.54762058645456,617.163970588235));
#159121=CARTESIAN_POINT('Ctrl Pts',(17.3590292079831,4.93906964482096,615.669852941176));
#159122=CARTESIAN_POINT('Ctrl Pts',(17.8167014103155,3.33051870318735,614.175735294118));
#159123=CARTESIAN_POINT('Ctrl Pts',(17.9710104137728,1.66525935159367,612.681617647059));
#159124=CARTESIAN_POINT('Ctrl Pts',(18.1253194172301,3.32956716117513E-15,
611.1875));
#159125=CARTESIAN_POINT('Ctrl Pts',(17.9710104137728,-1.66525935159367,
609.693382352941));
#159126=CARTESIAN_POINT('Ctrl Pts',(17.8167014103155,-3.33051870318736,
608.199264705882));
#159127=CARTESIAN_POINT('Ctrl Pts',(17.3590292079831,-4.93906964482095,
606.705147058824));
#159128=CARTESIAN_POINT('Ctrl Pts',(16.9013570056506,-6.54762058645456,
605.211029411765));
#159129=CARTESIAN_POINT('Ctrl Pts',(16.1559070823762,-8.04468584505497,
603.716911764706));
#159130=CARTESIAN_POINT('Ctrl Pts',(15.4104571591017,-9.54175110365538,
602.222794117647));
#159131=CARTESIAN_POINT('Ctrl Pts',(14.4026149179538,-10.8763499173728,
600.728676470588));
#159132=CARTESIAN_POINT('Ctrl Pts',(13.3947726768058,-12.2109487310903,
599.23455882353));
#159133=CARTESIAN_POINT('Ctrl Pts',(12.1588589765331,-13.3376329379985,
597.740441176471));
#159134=CARTESIAN_POINT('Ctrl Pts',(10.9229452762603,-14.4643171449067,
596.246323529412));
#159135=CARTESIAN_POINT('Ctrl Pts',(9.50104767561053,-15.3447188656481,
594.752205882353));
#159136=CARTESIAN_POINT('Ctrl Pts',(8.07915007496071,-16.2251205863895,
593.258088235294));
#159137=CARTESIAN_POINT('Ctrl Pts',(6.51968959134574,-16.8292587962898,
591.763970588235));
#159138=CARTESIAN_POINT('Ctrl Pts',(4.96022910773078,-17.4333970061901,
590.269852941177));
#159139=CARTESIAN_POINT('Ctrl Pts',(3.31631129755346,-17.7406985030951,
588.775735294118));
#159140=CARTESIAN_POINT('Ctrl Pts',(1.67239348737615,-18.048,587.281617647059));
#159141=CARTESIAN_POINT('Ctrl Pts',(0.,-18.048,585.7875));
#159142=CARTESIAN_POINT('Ctrl Pts',(-1.67239348737615,-18.048,584.293382352941));
#159143=CARTESIAN_POINT('Ctrl Pts',(-3.31631129755346,-17.7406985030951,
582.799264705882));
#159144=CARTESIAN_POINT('Ctrl Pts',(-4.96022910773077,-17.4333970061901,
581.305147058824));
#159145=CARTESIAN_POINT('Ctrl Pts',(-6.51968959134574,-16.8292587962898,
579.811029411765));
#159146=CARTESIAN_POINT('Ctrl Pts',(-8.07915007496071,-16.2251205863895,
578.316911764706));
#159147=CARTESIAN_POINT('Ctrl Pts',(-9.50104767561052,-15.3447188656481,
576.822794117647));
#159148=CARTESIAN_POINT('Ctrl Pts',(-10.9229452762603,-14.4643171449067,
575.328676470588));
#159149=CARTESIAN_POINT('Ctrl Pts',(-12.1588589765331,-13.3376329379985,
573.834558823529));
#159150=CARTESIAN_POINT('Ctrl Pts',(-13.3947726768058,-12.2109487310903,
572.340441176471));
#159151=CARTESIAN_POINT('Ctrl Pts',(-14.4026149179538,-10.8763499173728,
570.846323529412));
#159152=CARTESIAN_POINT('Ctrl Pts',(-15.4104571591017,-9.54175110365538,
569.352205882353));
#159153=CARTESIAN_POINT('Ctrl Pts',(-16.1559070823762,-8.04468584505497,
567.858088235294));
#159154=CARTESIAN_POINT('Ctrl Pts',(-16.9013570056506,-6.54762058645456,
566.363970588235));
#159155=CARTESIAN_POINT('Ctrl Pts',(-17.3590292079831,-4.93906964482095,
564.869852941177));
#159156=CARTESIAN_POINT('Ctrl Pts',(-17.8167014103155,-3.33051870318735,
563.375735294118));
#159157=CARTESIAN_POINT('Ctrl Pts',(-17.9710104137728,-1.66525935159368,
561.881617647059));
#159158=CARTESIAN_POINT('Ctrl Pts',(-18.1253194172301,-1.10985572039171E-15,
560.3875));
#159159=CARTESIAN_POINT('Ctrl Pts',(-17.9710104137728,1.66525935159367,
558.893382352941));
#159160=CARTESIAN_POINT('Ctrl Pts',(-17.8167014103155,3.33051870318735,
557.399264705882));
#159161=CARTESIAN_POINT('Ctrl Pts',(-17.3590292079831,4.93906964482096,
555.905147058824));
#159162=CARTESIAN_POINT('Ctrl Pts',(-16.9013570056506,6.54762058645456,
554.411029411765));
#159163=CARTESIAN_POINT('Ctrl Pts',(-16.1559070823762,8.04468584505497,
552.916911764706));
#159164=CARTESIAN_POINT('Ctrl Pts',(-15.4104571591017,9.54175110365538,
551.422794117647));
#159165=CARTESIAN_POINT('Ctrl Pts',(-14.4026149179538,10.8763499173728,
549.928676470588));
#159166=CARTESIAN_POINT('Ctrl Pts',(-13.3947726768058,12.2109487310903,
548.43455882353));
#159167=CARTESIAN_POINT('Ctrl Pts',(-12.1588589765331,13.3376329379985,
546.940441176471));
#159168=CARTESIAN_POINT('Ctrl Pts',(-10.9229452762603,14.4643171449067,
545.446323529412));
#159169=CARTESIAN_POINT('Ctrl Pts',(-9.50104767561052,15.3447188656481,
543.952205882353));
#159170=CARTESIAN_POINT('Ctrl Pts',(-8.07915007496071,16.2251205863895,
542.458088235294));
#159171=CARTESIAN_POINT('Ctrl Pts',(-6.51968959134574,16.8292587962898,
540.963970588235));
#159172=CARTESIAN_POINT('Ctrl Pts',(-4.96022910773078,17.4333970061901,
539.469852941177));
#159173=CARTESIAN_POINT('Ctrl Pts',(-3.31631129755346,17.7406985030951,
537.975735294118));
#159174=CARTESIAN_POINT('Ctrl Pts',(-1.67239348737615,18.048,536.481617647059));
#159175=CARTESIAN_POINT('Ctrl Pts',(-2.21024254310115E-15,18.048,534.9875));
#159176=CARTESIAN_POINT('Ctrl Pts',(1.67239348737616,18.048,533.493382352941));
#159177=CARTESIAN_POINT('Ctrl Pts',(3.31631129755346,17.7406985030951,531.999264705882));
#159178=CARTESIAN_POINT('Ctrl Pts',(4.96022910773077,17.4333970061901,530.505147058824));
#159179=CARTESIAN_POINT('Ctrl Pts',(6.51968959134575,16.8292587962898,529.011029411765));
#159180=CARTESIAN_POINT('Ctrl Pts',(8.07915007496071,16.2251205863895,527.516911764706));
#159181=CARTESIAN_POINT('Ctrl Pts',(9.50104767561053,15.3447188656481,526.022794117647));
#159182=CARTESIAN_POINT('Ctrl Pts',(10.9229452762603,14.4643171449067,524.528676470588));
#159183=CARTESIAN_POINT('Ctrl Pts',(12.1588589765331,13.3376329379985,523.03455882353));
#159184=CARTESIAN_POINT('Ctrl Pts',(13.3947726768058,12.2109487310903,521.540441176471));
#159185=CARTESIAN_POINT('Ctrl Pts',(14.4026149179538,10.8763499173728,520.046323529412));
#159186=CARTESIAN_POINT('Ctrl Pts',(15.4104571591017,9.54175110365538,518.552205882353));
#159187=CARTESIAN_POINT('Ctrl Pts',(16.1559070823762,8.04468584505496,517.058088235294));
#159188=CARTESIAN_POINT('Ctrl Pts',(16.9013570056506,6.54762058645456,515.563970588235));
#159189=CARTESIAN_POINT('Ctrl Pts',(17.3590292079831,4.93906964482096,514.069852941176));
#159190=CARTESIAN_POINT('Ctrl Pts',(17.8167014103155,3.33051870318735,512.575735294118));
#159191=CARTESIAN_POINT('Ctrl Pts',(17.9710104137728,1.66525935159367,511.081617647059));
#159192=CARTESIAN_POINT('Ctrl Pts',(18.1253194172301,3.32956716117513E-15,
509.5875));
#159193=CARTESIAN_POINT('Ctrl Pts',(17.9710104137728,-1.66525935159367,
508.093382352941));
#159194=CARTESIAN_POINT('Ctrl Pts',(17.8167014103155,-3.33051870318736,
506.599264705882));
#159195=CARTESIAN_POINT('Ctrl Pts',(17.3590292079831,-4.93906964482095,
505.105147058824));
#159196=CARTESIAN_POINT('Ctrl Pts',(16.9013570056506,-6.54762058645456,
503.611029411765));
#159197=CARTESIAN_POINT('Ctrl Pts',(16.1559070823762,-8.04468584505497,
502.116911764706));
#159198=CARTESIAN_POINT('Ctrl Pts',(15.4104571591017,-9.54175110365538,
500.622794117647));
#159199=CARTESIAN_POINT('Ctrl Pts',(14.4026149179538,-10.8763499173728,
499.128676470588));
#159200=CARTESIAN_POINT('Ctrl Pts',(13.3947726768058,-12.2109487310903,
497.63455882353));
#159201=CARTESIAN_POINT('Ctrl Pts',(12.1588589765331,-13.3376329379985,
496.140441176471));
#159202=CARTESIAN_POINT('Ctrl Pts',(10.9229452762603,-14.4643171449067,
494.646323529412));
#159203=CARTESIAN_POINT('Ctrl Pts',(9.50104767561053,-15.3447188656481,
493.152205882353));
#159204=CARTESIAN_POINT('Ctrl Pts',(8.07915007496071,-16.2251205863895,
491.658088235294));
#159205=CARTESIAN_POINT('Ctrl Pts',(6.51968959134574,-16.8292587962898,
490.163970588235));
#159206=CARTESIAN_POINT('Ctrl Pts',(4.96022910773078,-17.4333970061901,
488.669852941177));
#159207=CARTESIAN_POINT('Ctrl Pts',(3.31631129755346,-17.7406985030951,
487.175735294118));
#159208=CARTESIAN_POINT('Ctrl Pts',(1.67239348737615,-18.048,485.681617647059));
#159209=CARTESIAN_POINT('Ctrl Pts',(0.,-18.048,484.1875));
#159210=CARTESIAN_POINT('Ctrl Pts',(-1.67239348737615,-18.048,482.693382352941));
#159211=CARTESIAN_POINT('Ctrl Pts',(-3.31631129755346,-17.7406985030951,
481.199264705882));
#159212=CARTESIAN_POINT('Ctrl Pts',(-4.96022910773077,-17.4333970061901,
479.705147058824));
#159213=CARTESIAN_POINT('Ctrl Pts',(-6.51968959134574,-16.8292587962898,
478.211029411765));
#159214=CARTESIAN_POINT('Ctrl Pts',(-8.07915007496071,-16.2251205863895,
476.716911764706));
#159215=CARTESIAN_POINT('Ctrl Pts',(-9.50104767561052,-15.3447188656481,
475.222794117647));
#159216=CARTESIAN_POINT('Ctrl Pts',(-10.9229452762603,-14.4643171449067,
473.728676470588));
#159217=CARTESIAN_POINT('Ctrl Pts',(-12.1588589765331,-13.3376329379985,
472.234558823529));
#159218=CARTESIAN_POINT('Ctrl Pts',(-13.3947726768058,-12.2109487310903,
470.740441176471));
#159219=CARTESIAN_POINT('Ctrl Pts',(-14.4026149179538,-10.8763499173728,
469.246323529412));
#159220=CARTESIAN_POINT('Ctrl Pts',(-15.4104571591017,-9.54175110365538,
467.752205882353));
#159221=CARTESIAN_POINT('Ctrl Pts',(-16.1559070823762,-8.04468584505497,
466.258088235294));
#159222=CARTESIAN_POINT('Ctrl Pts',(-16.9013570056506,-6.54762058645456,
464.763970588236));
#159223=CARTESIAN_POINT('Ctrl Pts',(-17.3590292079831,-4.93906964482095,
463.269852941177));
#159224=CARTESIAN_POINT('Ctrl Pts',(-17.8167014103155,-3.33051870318735,
461.775735294118));
#159225=CARTESIAN_POINT('Ctrl Pts',(-17.9710104137728,-1.66525935159368,
460.281617647059));
#159226=CARTESIAN_POINT('Ctrl Pts',(-18.1253194172301,-1.10985572039171E-15,
458.7875));
#159227=CARTESIAN_POINT('Ctrl Pts',(-17.9710104137728,1.66525935159367,
457.293382352941));
#159228=CARTESIAN_POINT('Ctrl Pts',(-17.8167014103155,3.33051870318735,
455.799264705882));
#159229=CARTESIAN_POINT('Ctrl Pts',(-17.3590292079831,4.93906964482096,
454.305147058824));
#159230=CARTESIAN_POINT('Ctrl Pts',(-16.9013570056506,6.54762058645456,
452.811029411765));
#159231=CARTESIAN_POINT('Ctrl Pts',(-16.1559070823762,8.04468584505497,
451.316911764706));
#159232=CARTESIAN_POINT('Ctrl Pts',(-15.4104571591017,9.54175110365538,
449.822794117647));
#159233=CARTESIAN_POINT('Ctrl Pts',(-14.4026149179538,10.8763499173728,
448.328676470588));
#159234=CARTESIAN_POINT('Ctrl Pts',(-13.3947726768058,12.2109487310903,
446.83455882353));
#159235=CARTESIAN_POINT('Ctrl Pts',(-12.1588589765331,13.3376329379985,
445.340441176471));
#159236=CARTESIAN_POINT('Ctrl Pts',(-10.9229452762603,14.4643171449067,
443.846323529412));
#159237=CARTESIAN_POINT('Ctrl Pts',(-9.50104767561052,15.3447188656481,
442.352205882353));
#159238=CARTESIAN_POINT('Ctrl Pts',(-8.07915007496071,16.2251205863895,
440.858088235294));
#159239=CARTESIAN_POINT('Ctrl Pts',(-6.51968959134574,16.8292587962898,
439.363970588235));
#159240=CARTESIAN_POINT('Ctrl Pts',(-4.96022910773078,17.4333970061901,
437.869852941176));
#159241=CARTESIAN_POINT('Ctrl Pts',(-3.31631129755346,17.7406985030951,
436.375735294118));
#159242=CARTESIAN_POINT('Ctrl Pts',(-1.67239348737615,18.048,434.881617647059));
#159243=CARTESIAN_POINT('Ctrl Pts',(-2.21024254310115E-15,18.048,433.3875));
#159244=CARTESIAN_POINT('Ctrl Pts',(1.67239348737616,18.048,431.893382352941));
#159245=CARTESIAN_POINT('Ctrl Pts',(3.31631129755346,17.7406985030951,430.399264705882));
#159246=CARTESIAN_POINT('Ctrl Pts',(4.96022910773077,17.4333970061901,428.905147058824));
#159247=CARTESIAN_POINT('Ctrl Pts',(6.51968959134575,16.8292587962898,427.411029411765));
#159248=CARTESIAN_POINT('Ctrl Pts',(8.07915007496071,16.2251205863895,425.916911764706));
#159249=CARTESIAN_POINT('Ctrl Pts',(9.50104767561053,15.3447188656481,424.422794117647));
#159250=CARTESIAN_POINT('Ctrl Pts',(10.9229452762603,14.4643171449067,422.928676470588));
#159251=CARTESIAN_POINT('Ctrl Pts',(12.1588589765331,13.3376329379985,421.43455882353));
#159252=CARTESIAN_POINT('Ctrl Pts',(13.3947726768058,12.2109487310903,419.940441176471));
#159253=CARTESIAN_POINT('Ctrl Pts',(14.4026149179538,10.8763499173728,418.446323529412));
#159254=CARTESIAN_POINT('Ctrl Pts',(15.4104571591017,9.54175110365538,416.952205882353));
#159255=CARTESIAN_POINT('Ctrl Pts',(16.1559070823762,8.04468584505496,415.458088235294));
#159256=CARTESIAN_POINT('Ctrl Pts',(16.9013570056506,6.54762058645456,413.963970588235));
#159257=CARTESIAN_POINT('Ctrl Pts',(17.3590292079831,4.93906964482096,412.469852941177));
#159258=CARTESIAN_POINT('Ctrl Pts',(17.8167014103155,3.33051870318735,410.975735294118));
#159259=CARTESIAN_POINT('Ctrl Pts',(17.9710104137728,1.66525935159367,409.481617647059));
#159260=CARTESIAN_POINT('Ctrl Pts',(18.1253194172301,3.32956716117513E-15,
407.9875));
#159261=CARTESIAN_POINT('Ctrl Pts',(17.9710104137728,-1.66525935159367,
406.493382352941));
#159262=CARTESIAN_POINT('Ctrl Pts',(17.8167014103155,-3.33051870318736,
404.999264705882));
#159263=CARTESIAN_POINT('Ctrl Pts',(17.3590292079831,-4.93906964482095,
403.505147058824));
#159264=CARTESIAN_POINT('Ctrl Pts',(16.9013570056506,-6.54762058645456,
402.011029411765));
#159265=CARTESIAN_POINT('Ctrl Pts',(16.1559070823762,-8.04468584505497,
400.516911764706));
#159266=CARTESIAN_POINT('Ctrl Pts',(15.4104571591017,-9.54175110365538,
399.022794117647));
#159267=CARTESIAN_POINT('Ctrl Pts',(14.4026149179538,-10.8763499173728,
397.528676470588));
#159268=CARTESIAN_POINT('Ctrl Pts',(13.3947726768058,-12.2109487310903,
396.034558823529));
#159269=CARTESIAN_POINT('Ctrl Pts',(12.1588589765331,-13.3376329379985,
394.540441176471));
#159270=CARTESIAN_POINT('Ctrl Pts',(10.9229452762603,-14.4643171449067,
393.046323529412));
#159271=CARTESIAN_POINT('Ctrl Pts',(9.50104767561053,-15.3447188656481,
391.552205882353));
#159272=CARTESIAN_POINT('Ctrl Pts',(8.07915007496071,-16.2251205863895,
390.058088235294));
#159273=CARTESIAN_POINT('Ctrl Pts',(6.51968959134574,-16.8292587962898,
388.563970588235));
#159274=CARTESIAN_POINT('Ctrl Pts',(4.96022910773078,-17.4333970061901,
387.069852941177));
#159275=CARTESIAN_POINT('Ctrl Pts',(3.31631129755346,-17.7406985030951,
385.575735294118));
#159276=CARTESIAN_POINT('Ctrl Pts',(1.67239348737615,-18.048,384.081617647059));
#159277=CARTESIAN_POINT('Ctrl Pts',(0.,-18.048,382.5875));
#159278=CARTESIAN_POINT('Ctrl Pts',(-1.67239348737615,-18.048,381.093382352941));
#159279=CARTESIAN_POINT('Ctrl Pts',(-3.31631129755346,-17.7406985030951,
379.599264705882));
#159280=CARTESIAN_POINT('Ctrl Pts',(-4.96022910773077,-17.4333970061901,
378.105147058823));
#159281=CARTESIAN_POINT('Ctrl Pts',(-6.51968959134574,-16.8292587962898,
376.611029411765));
#159282=CARTESIAN_POINT('Ctrl Pts',(-8.07915007496071,-16.2251205863895,
375.116911764706));
#159283=CARTESIAN_POINT('Ctrl Pts',(-9.50104767561052,-15.3447188656481,
373.622794117647));
#159284=CARTESIAN_POINT('Ctrl Pts',(-10.9229452762603,-14.4643171449067,
372.128676470588));
#159285=CARTESIAN_POINT('Ctrl Pts',(-12.1588589765331,-13.3376329379985,
370.634558823529));
#159286=CARTESIAN_POINT('Ctrl Pts',(-13.3947726768058,-12.2109487310903,
369.140441176471));
#159287=CARTESIAN_POINT('Ctrl Pts',(-14.4026149179538,-10.8763499173728,
367.646323529412));
#159288=CARTESIAN_POINT('Ctrl Pts',(-15.4104571591017,-9.54175110365538,
366.152205882353));
#159289=CARTESIAN_POINT('Ctrl Pts',(-16.1559070823762,-8.04468584505497,
364.658088235294));
#159290=CARTESIAN_POINT('Ctrl Pts',(-16.9013570056506,-6.54762058645456,
363.163970588235));
#159291=CARTESIAN_POINT('Ctrl Pts',(-17.3590292079831,-4.93906964482095,
361.669852941177));
#159292=CARTESIAN_POINT('Ctrl Pts',(-17.8167014103155,-3.33051870318735,
360.175735294118));
#159293=CARTESIAN_POINT('Ctrl Pts',(-17.9710104137728,-1.66525935159368,
358.681617647059));
#159294=CARTESIAN_POINT('Ctrl Pts',(-18.1253194172301,-1.10985572039171E-15,
357.1875));
#159295=CARTESIAN_POINT('Ctrl Pts',(-17.9710104137728,1.66525935159367,
355.693382352941));
#159296=CARTESIAN_POINT('Ctrl Pts',(-17.8167014103155,3.33051870318735,
354.199264705883));
#159297=CARTESIAN_POINT('Ctrl Pts',(-17.3590292079831,4.93906964482096,
352.705147058824));
#159298=CARTESIAN_POINT('Ctrl Pts',(-16.9013570056506,6.54762058645456,
351.211029411765));
#159299=CARTESIAN_POINT('Ctrl Pts',(-16.1559070823762,8.04468584505497,
349.716911764706));
#159300=CARTESIAN_POINT('Ctrl Pts',(-15.4104571591017,9.54175110365538,
348.222794117647));
#159301=CARTESIAN_POINT('Ctrl Pts',(-14.4026149179538,10.8763499173728,
346.728676470588));
#159302=CARTESIAN_POINT('Ctrl Pts',(-13.3947726768058,12.2109487310903,
345.234558823529));
#159303=CARTESIAN_POINT('Ctrl Pts',(-12.1588589765331,13.3376329379985,
343.740441176471));
#159304=CARTESIAN_POINT('Ctrl Pts',(-10.9229452762603,14.4643171449067,
342.246323529412));
#159305=CARTESIAN_POINT('Ctrl Pts',(-9.50104767561052,15.3447188656481,
340.752205882353));
#159306=CARTESIAN_POINT('Ctrl Pts',(-8.07915007496071,16.2251205863895,
339.258088235294));
#159307=CARTESIAN_POINT('Ctrl Pts',(-6.51968959134574,16.8292587962898,
337.763970588235));
#159308=CARTESIAN_POINT('Ctrl Pts',(-4.96022910773078,17.4333970061901,
336.269852941177));
#159309=CARTESIAN_POINT('Ctrl Pts',(-3.31631129755346,17.7406985030951,
334.775735294118));
#159310=CARTESIAN_POINT('Ctrl Pts',(-1.67239348737615,18.048,333.281617647059));
#159311=CARTESIAN_POINT('Ctrl Pts',(-2.21024254310115E-15,18.048,331.7875));
#159312=CARTESIAN_POINT('Ctrl Pts',(1.67239348737616,18.048,330.293382352941));
#159313=CARTESIAN_POINT('Ctrl Pts',(3.31631129755346,17.7406985030951,328.799264705882));
#159314=CARTESIAN_POINT('Ctrl Pts',(4.96022910773077,17.4333970061901,327.305147058824));
#159315=CARTESIAN_POINT('Ctrl Pts',(6.51968959134575,16.8292587962898,325.811029411765));
#159316=CARTESIAN_POINT('Ctrl Pts',(8.07915007496071,16.2251205863895,324.316911764706));
#159317=CARTESIAN_POINT('Ctrl Pts',(9.50104767561053,15.3447188656481,322.822794117647));
#159318=CARTESIAN_POINT('Ctrl Pts',(10.9229452762603,14.4643171449067,321.328676470588));
#159319=CARTESIAN_POINT('Ctrl Pts',(12.1588589765331,13.3376329379985,319.834558823529));
#159320=CARTESIAN_POINT('Ctrl Pts',(13.3947726768058,12.2109487310903,318.340441176471));
#159321=CARTESIAN_POINT('Ctrl Pts',(14.4026149179538,10.8763499173728,316.846323529412));
#159322=CARTESIAN_POINT('Ctrl Pts',(15.4104571591017,9.54175110365538,315.352205882353));
#159323=CARTESIAN_POINT('Ctrl Pts',(16.1559070823762,8.04468584505496,313.858088235294));
#159324=CARTESIAN_POINT('Ctrl Pts',(16.9013570056506,6.54762058645456,312.363970588235));
#159325=CARTESIAN_POINT('Ctrl Pts',(17.3590292079831,4.93906964482096,310.869852941176));
#159326=CARTESIAN_POINT('Ctrl Pts',(17.8167014103155,3.33051870318735,309.375735294118));
#159327=CARTESIAN_POINT('Ctrl Pts',(17.9710104137728,1.66525935159367,307.881617647059));
#159328=CARTESIAN_POINT('Ctrl Pts',(18.1253194172301,3.32956716117513E-15,
306.3875));
#159329=CARTESIAN_POINT('Ctrl Pts',(17.9710104137728,-1.66525935159367,
304.893382352941));
#159330=CARTESIAN_POINT('Ctrl Pts',(17.8167014103155,-3.33051870318736,
303.399264705882));
#159331=CARTESIAN_POINT('Ctrl Pts',(17.3590292079831,-4.93906964482095,
301.905147058824));
#159332=CARTESIAN_POINT('Ctrl Pts',(16.9013570056506,-6.54762058645456,
300.411029411765));
#159333=CARTESIAN_POINT('Ctrl Pts',(16.1559070823762,-8.04468584505497,
298.916911764706));
#159334=CARTESIAN_POINT('Ctrl Pts',(15.4104571591017,-9.54175110365538,
297.422794117647));
#159335=CARTESIAN_POINT('Ctrl Pts',(14.4026149179538,-10.8763499173728,
295.928676470588));
#159336=CARTESIAN_POINT('Ctrl Pts',(13.3947726768058,-12.2109487310903,
294.43455882353));
#159337=CARTESIAN_POINT('Ctrl Pts',(12.1588589765331,-13.3376329379985,
292.940441176471));
#159338=CARTESIAN_POINT('Ctrl Pts',(10.9229452762603,-14.4643171449067,
291.446323529412));
#159339=CARTESIAN_POINT('Ctrl Pts',(9.50104767561053,-15.3447188656481,
289.952205882353));
#159340=CARTESIAN_POINT('Ctrl Pts',(8.07915007496071,-16.2251205863895,
288.458088235294));
#159341=CARTESIAN_POINT('Ctrl Pts',(6.51968959134574,-16.8292587962898,
286.963970588235));
#159342=CARTESIAN_POINT('Ctrl Pts',(4.96022910773078,-17.4333970061901,
285.469852941177));
#159343=CARTESIAN_POINT('Ctrl Pts',(3.31631129755346,-17.7406985030951,
283.975735294118));
#159344=CARTESIAN_POINT('Ctrl Pts',(1.67239348737615,-18.048,282.481617647059));
#159345=CARTESIAN_POINT('Ctrl Pts',(0.,-18.048,280.9875));
#159346=CARTESIAN_POINT('Ctrl Pts',(-1.67239348737615,-18.048,279.493382352941));
#159347=CARTESIAN_POINT('Ctrl Pts',(-3.31631129755346,-17.7406985030951,
277.999264705882));
#159348=CARTESIAN_POINT('Ctrl Pts',(-4.96022910773077,-17.4333970061901,
276.505147058824));
#159349=CARTESIAN_POINT('Ctrl Pts',(-6.51968959134574,-16.8292587962898,
275.011029411765));
#159350=CARTESIAN_POINT('Ctrl Pts',(-8.07915007496071,-16.2251205863895,
273.516911764706));
#159351=CARTESIAN_POINT('Ctrl Pts',(-9.50104767561052,-15.3447188656481,
272.022794117647));
#159352=CARTESIAN_POINT('Ctrl Pts',(-10.9229452762603,-14.4643171449067,
270.528676470588));
#159353=CARTESIAN_POINT('Ctrl Pts',(-12.1588589765331,-13.3376329379985,
269.034558823529));
#159354=CARTESIAN_POINT('Ctrl Pts',(-13.3947726768058,-12.2109487310903,
267.540441176471));
#159355=CARTESIAN_POINT('Ctrl Pts',(-14.4026149179538,-10.8763499173728,
266.046323529412));
#159356=CARTESIAN_POINT('Ctrl Pts',(-15.4104571591017,-9.54175110365538,
264.552205882353));
#159357=CARTESIAN_POINT('Ctrl Pts',(-16.1559070823762,-8.04468584505497,
263.058088235294));
#159358=CARTESIAN_POINT('Ctrl Pts',(-16.9013570056506,-6.54762058645456,
261.563970588235));
#159359=CARTESIAN_POINT('Ctrl Pts',(-17.3590292079831,-4.93906964482095,
260.069852941176));
#159360=CARTESIAN_POINT('Ctrl Pts',(-17.8167014103155,-3.33051870318735,
258.575735294118));
#159361=CARTESIAN_POINT('Ctrl Pts',(-17.9710104137728,-1.66525935159368,
257.081617647059));
#159362=CARTESIAN_POINT('Ctrl Pts',(-18.1253194172301,-1.10985572039171E-15,
255.5875));
#159363=CARTESIAN_POINT('Ctrl Pts',(-17.9710104137728,1.66525935159367,
254.093382352941));
#159364=CARTESIAN_POINT('Ctrl Pts',(-17.8167014103155,3.33051870318735,
252.599264705882));
#159365=CARTESIAN_POINT('Ctrl Pts',(-17.3590292079831,4.93906964482096,
251.105147058823));
#159366=CARTESIAN_POINT('Ctrl Pts',(-16.9013570056506,6.54762058645456,
249.611029411765));
#159367=CARTESIAN_POINT('Ctrl Pts',(-16.1559070823762,8.04468584505497,
248.116911764706));
#159368=CARTESIAN_POINT('Ctrl Pts',(-15.4104571591017,9.54175110365538,
246.622794117647));
#159369=CARTESIAN_POINT('Ctrl Pts',(-14.4026149179538,10.8763499173728,
245.128676470588));
#159370=CARTESIAN_POINT('Ctrl Pts',(-13.3947726768058,12.2109487310903,
243.634558823529));
#159371=CARTESIAN_POINT('Ctrl Pts',(-12.1588589765331,13.3376329379985,
242.140441176471));
#159372=CARTESIAN_POINT('Ctrl Pts',(-10.9229452762603,14.4643171449067,
240.646323529412));
#159373=CARTESIAN_POINT('Ctrl Pts',(-9.50104767561052,15.3447188656481,
239.152205882353));
#159374=CARTESIAN_POINT('Ctrl Pts',(-8.07915007496071,16.2251205863895,
237.658088235294));
#159375=CARTESIAN_POINT('Ctrl Pts',(-6.51968959134574,16.8292587962898,
236.163970588235));
#159376=CARTESIAN_POINT('Ctrl Pts',(-4.96022910773078,17.4333970061901,
234.669852941177));
#159377=CARTESIAN_POINT('Ctrl Pts',(-3.31631129755346,17.7406985030951,
233.175735294118));
#159378=CARTESIAN_POINT('Ctrl Pts',(-1.67239348737615,18.048,231.681617647059));
#159379=CARTESIAN_POINT('Ctrl Pts',(-2.21024254310115E-15,18.048,230.1875));
#159380=CARTESIAN_POINT('Ctrl Pts',(1.67239348737616,18.048,228.693382352941));
#159381=CARTESIAN_POINT('Ctrl Pts',(3.31631129755346,17.7406985030951,227.199264705882));
#159382=CARTESIAN_POINT('Ctrl Pts',(4.96022910773077,17.4333970061901,225.705147058824));
#159383=CARTESIAN_POINT('Ctrl Pts',(6.51968959134575,16.8292587962898,224.211029411765));
#159384=CARTESIAN_POINT('Ctrl Pts',(8.07915007496071,16.2251205863895,222.716911764706));
#159385=CARTESIAN_POINT('Ctrl Pts',(9.50104767561053,15.3447188656481,221.222794117647));
#159386=CARTESIAN_POINT('Ctrl Pts',(10.9229452762603,14.4643171449067,219.728676470588));
#159387=CARTESIAN_POINT('Ctrl Pts',(12.1588589765331,13.3376329379985,218.234558823529));
#159388=CARTESIAN_POINT('Ctrl Pts',(13.3947726768058,12.2109487310903,216.740441176471));
#159389=CARTESIAN_POINT('Ctrl Pts',(14.4026149179538,10.8763499173728,215.246323529412));
#159390=CARTESIAN_POINT('Ctrl Pts',(15.4104571591017,9.54175110365538,213.752205882353));
#159391=CARTESIAN_POINT('Ctrl Pts',(16.1559070823762,8.04468584505496,212.258088235294));
#159392=CARTESIAN_POINT('Ctrl Pts',(16.9013570056506,6.54762058645456,210.763970588235));
#159393=CARTESIAN_POINT('Ctrl Pts',(17.3590292079831,4.93906964482096,209.269852941177));
#159394=CARTESIAN_POINT('Ctrl Pts',(17.8167014103155,3.33051870318735,207.775735294118));
#159395=CARTESIAN_POINT('Ctrl Pts',(17.9710104137728,1.66525935159367,206.281617647059));
#159396=CARTESIAN_POINT('Ctrl Pts',(18.1253194172301,3.32956716117513E-15,
204.7875));
#159397=CARTESIAN_POINT('Ctrl Pts',(17.9710104137728,-1.66525935159367,
203.293382352941));
#159398=CARTESIAN_POINT('Ctrl Pts',(17.8167014103155,-3.33051870318736,
201.799264705882));
#159399=CARTESIAN_POINT('Ctrl Pts',(17.3590292079831,-4.93906964482095,
200.305147058824));
#159400=CARTESIAN_POINT('Ctrl Pts',(16.9013570056506,-6.54762058645456,
198.811029411765));
#159401=CARTESIAN_POINT('Ctrl Pts',(16.1559070823762,-8.04468584505497,
197.316911764706));
#159402=CARTESIAN_POINT('Ctrl Pts',(15.4104571591017,-9.54175110365538,
195.822794117647));
#159403=CARTESIAN_POINT('Ctrl Pts',(14.4026149179538,-10.8763499173728,
194.328676470588));
#159404=CARTESIAN_POINT('Ctrl Pts',(13.3947726768058,-12.2109487310903,
192.834558823529));
#159405=CARTESIAN_POINT('Ctrl Pts',(12.1588589765331,-13.3376329379985,
191.340441176471));
#159406=CARTESIAN_POINT('Ctrl Pts',(10.9229452762603,-14.4643171449067,
189.846323529412));
#159407=CARTESIAN_POINT('Ctrl Pts',(9.50104767561053,-15.3447188656481,
188.352205882353));
#159408=CARTESIAN_POINT('Ctrl Pts',(8.07915007496071,-16.2251205863895,
186.858088235294));
#159409=CARTESIAN_POINT('Ctrl Pts',(6.51968959134574,-16.8292587962898,
185.363970588235));
#159410=CARTESIAN_POINT('Ctrl Pts',(4.96022910773078,-17.4333970061901,
183.869852941176));
#159411=CARTESIAN_POINT('Ctrl Pts',(3.31631129755346,-17.7406985030951,
182.375735294118));
#159412=CARTESIAN_POINT('Ctrl Pts',(1.67239348737615,-18.048,180.881617647059));
#159413=CARTESIAN_POINT('Ctrl Pts',(0.,-18.048,179.3875));
#159414=CARTESIAN_POINT('Ctrl Pts',(-1.67239348737615,-18.048,177.893382352941));
#159415=CARTESIAN_POINT('Ctrl Pts',(-3.31631129755346,-17.7406985030951,
176.399264705882));
#159416=CARTESIAN_POINT('Ctrl Pts',(-4.96022910773077,-17.4333970061901,
174.905147058824));
#159417=CARTESIAN_POINT('Ctrl Pts',(-6.51968959134574,-16.8292587962898,
173.411029411765));
#159418=CARTESIAN_POINT('Ctrl Pts',(-8.07915007496071,-16.2251205863895,
171.916911764706));
#159419=CARTESIAN_POINT('Ctrl Pts',(-9.50104767561052,-15.3447188656481,
170.422794117647));
#159420=CARTESIAN_POINT('Ctrl Pts',(-10.9229452762603,-14.4643171449067,
168.928676470588));
#159421=CARTESIAN_POINT('Ctrl Pts',(-12.1588589765331,-13.3376329379985,
167.43455882353));
#159422=CARTESIAN_POINT('Ctrl Pts',(-13.3947726768058,-12.2109487310903,
165.940441176471));
#159423=CARTESIAN_POINT('Ctrl Pts',(-14.4026149179538,-10.8763499173728,
164.446323529412));
#159424=CARTESIAN_POINT('Ctrl Pts',(-15.4104571591017,-9.54175110365538,
162.952205882353));
#159425=CARTESIAN_POINT('Ctrl Pts',(-16.1559070823762,-8.04468584505497,
161.458088235294));
#159426=CARTESIAN_POINT('Ctrl Pts',(-16.9013570056506,-6.54762058645456,
159.963970588235));
#159427=CARTESIAN_POINT('Ctrl Pts',(-17.3590292079831,-4.93906964482095,
158.469852941177));
#159428=CARTESIAN_POINT('Ctrl Pts',(-17.8167014103155,-3.33051870318735,
156.975735294118));
#159429=CARTESIAN_POINT('Ctrl Pts',(-17.9710104137728,-1.66525935159368,
155.481617647059));
#159430=CARTESIAN_POINT('Ctrl Pts',(-18.1253194172301,-1.10985572039171E-15,
153.9875));
#159431=CARTESIAN_POINT('Ctrl Pts',(-17.9710104137728,1.66525935159367,
152.493382352941));
#159432=CARTESIAN_POINT('Ctrl Pts',(-17.8167014103155,3.33051870318735,
150.999264705882));
#159433=CARTESIAN_POINT('Ctrl Pts',(-17.3590292079831,4.93906964482096,
149.505147058824));
#159434=CARTESIAN_POINT('Ctrl Pts',(-16.9013570056506,6.54762058645456,
148.011029411765));
#159435=CARTESIAN_POINT('Ctrl Pts',(-16.1559070823762,8.04468584505497,
146.516911764706));
#159436=CARTESIAN_POINT('Ctrl Pts',(-15.4104571591017,9.54175110365538,
145.022794117647));
#159437=CARTESIAN_POINT('Ctrl Pts',(-14.4026149179538,10.8763499173728,
143.528676470588));
#159438=CARTESIAN_POINT('Ctrl Pts',(-13.3947726768058,12.2109487310903,
142.034558823529));
#159439=CARTESIAN_POINT('Ctrl Pts',(-12.1588589765331,13.3376329379985,
140.540441176471));
#159440=CARTESIAN_POINT('Ctrl Pts',(-10.9229452762603,14.4643171449067,
139.046323529412));
#159441=CARTESIAN_POINT('Ctrl Pts',(-9.50104767561052,15.3447188656481,
137.552205882353));
#159442=CARTESIAN_POINT('Ctrl Pts',(-8.07915007496071,16.2251205863895,
136.058088235294));
#159443=CARTESIAN_POINT('Ctrl Pts',(-6.51968959134574,16.8292587962898,
134.563970588235));
#159444=CARTESIAN_POINT('Ctrl Pts',(-4.96022910773078,17.4333970061901,
133.069852941176));
#159445=CARTESIAN_POINT('Ctrl Pts',(-3.31631129755346,17.7406985030951,
131.575735294118));
#159446=CARTESIAN_POINT('Ctrl Pts',(-1.67239348737615,18.048,130.081617647059));
#159447=CARTESIAN_POINT('Ctrl Pts',(-2.21024254310115E-15,18.048,128.5875));
#159448=CARTESIAN_POINT('Ctrl Pts',(1.67239348737616,18.048,127.093382352941));
#159449=CARTESIAN_POINT('Ctrl Pts',(3.31631129755346,17.7406985030951,125.599264705882));
#159450=CARTESIAN_POINT('Ctrl Pts',(4.96022910773077,17.4333970061901,124.105147058824));
#159451=CARTESIAN_POINT('Ctrl Pts',(6.51968959134575,16.8292587962898,122.611029411765));
#159452=CARTESIAN_POINT('Ctrl Pts',(8.07915007496071,16.2251205863895,121.116911764706));
#159453=CARTESIAN_POINT('Ctrl Pts',(9.50104767561053,15.3447188656481,119.622794117647));
#159454=CARTESIAN_POINT('Ctrl Pts',(10.9229452762603,14.4643171449067,118.128676470588));
#159455=CARTESIAN_POINT('Ctrl Pts',(12.1588589765331,13.3376329379985,116.634558823529));
#159456=CARTESIAN_POINT('Ctrl Pts',(13.3947726768058,12.2109487310903,115.140441176471));
#159457=CARTESIAN_POINT('Ctrl Pts',(14.4026149179538,10.8763499173728,113.646323529412));
#159458=CARTESIAN_POINT('Ctrl Pts',(15.4104571591017,9.54175110365538,112.152205882353));
#159459=CARTESIAN_POINT('Ctrl Pts',(16.1559070823762,8.04468584505496,110.658088235294));
#159460=CARTESIAN_POINT('Ctrl Pts',(16.9013570056506,6.54762058645456,109.163970588235));
#159461=CARTESIAN_POINT('Ctrl Pts',(17.3590292079831,4.93906964482096,107.669852941177));
#159462=CARTESIAN_POINT('Ctrl Pts',(17.8167014103155,3.33051870318735,106.175735294118));
#159463=CARTESIAN_POINT('Ctrl Pts',(17.9710104137728,1.66525935159367,104.681617647059));
#159464=CARTESIAN_POINT('Ctrl Pts',(18.1253194172301,3.32956716117513E-15,
103.1875));
#159465=CARTESIAN_POINT('Ctrl Pts',(17.9710104137728,-1.66525935159367,
101.693382352941));
#159466=CARTESIAN_POINT('Ctrl Pts',(17.8167014103155,-3.33051870318736,
100.199264705882));
#159467=CARTESIAN_POINT('Ctrl Pts',(17.3590292079831,-4.93906964482095,
98.7051470588236));
#159468=CARTESIAN_POINT('Ctrl Pts',(16.9013570056506,-6.54762058645456,
97.2110294117647));
#159469=CARTESIAN_POINT('Ctrl Pts',(16.1559070823762,-8.04468584505497,
95.7169117647059));
#159470=CARTESIAN_POINT('Ctrl Pts',(15.4104571591017,-9.54175110365538,
94.222794117647));
#159471=CARTESIAN_POINT('Ctrl Pts',(14.4026149179538,-10.8763499173728,
92.7286764705884));
#159472=CARTESIAN_POINT('Ctrl Pts',(13.3947726768058,-12.2109487310903,
91.2345588235295));
#159473=CARTESIAN_POINT('Ctrl Pts',(12.1588589765331,-13.3376329379985,
89.7404411764706));
#159474=CARTESIAN_POINT('Ctrl Pts',(10.9229452762603,-14.4643171449067,
88.2463235294117));
#159475=CARTESIAN_POINT('Ctrl Pts',(9.50104767561053,-15.3447188656481,
86.7522058823529));
#159476=CARTESIAN_POINT('Ctrl Pts',(8.07915007496071,-16.2251205863895,
85.2580882352942));
#159477=CARTESIAN_POINT('Ctrl Pts',(6.51968959134574,-16.8292587962898,
83.7639705882354));
#159478=CARTESIAN_POINT('Ctrl Pts',(4.96022910773078,-17.4333970061901,
82.2698529411765));
#159479=CARTESIAN_POINT('Ctrl Pts',(3.31631129755346,-17.7406985030951,
80.7757352941176));
#159480=CARTESIAN_POINT('Ctrl Pts',(1.67239348737615,-18.048,79.2816176470588));
#159481=CARTESIAN_POINT('Ctrl Pts',(0.,-18.048,77.7875000000001));
#159482=CARTESIAN_POINT('Ctrl Pts',(-1.67239348737615,-18.048,76.2933823529413));
#159483=CARTESIAN_POINT('Ctrl Pts',(-3.31631129755346,-17.7406985030951,
74.7992647058824));
#159484=CARTESIAN_POINT('Ctrl Pts',(-4.96022910773077,-17.4333970061901,
73.3051470588235));
#159485=CARTESIAN_POINT('Ctrl Pts',(-6.51968959134574,-16.8292587962898,
71.8110294117647));
#159486=CARTESIAN_POINT('Ctrl Pts',(-8.07915007496071,-16.2251205863895,
70.316911764706));
#159487=CARTESIAN_POINT('Ctrl Pts',(-9.50104767561052,-15.3447188656481,
68.8227941176471));
#159488=CARTESIAN_POINT('Ctrl Pts',(-10.9229452762603,-14.4643171449067,
67.3286764705883));
#159489=CARTESIAN_POINT('Ctrl Pts',(-12.1588589765331,-13.3376329379985,
65.8345588235294));
#159490=CARTESIAN_POINT('Ctrl Pts',(-13.3947726768058,-12.2109487310903,
64.3404411764705));
#159491=CARTESIAN_POINT('Ctrl Pts',(-14.4026149179538,-10.8763499173728,
62.8463235294119));
#159492=CARTESIAN_POINT('Ctrl Pts',(-15.4104571591017,-9.54175110365538,
61.352205882353));
#159493=CARTESIAN_POINT('Ctrl Pts',(-16.1559070823762,-8.04468584505497,
59.8580882352941));
#159494=CARTESIAN_POINT('Ctrl Pts',(-16.9013570056506,-6.54762058645456,
58.3639705882353));
#159495=CARTESIAN_POINT('Ctrl Pts',(-17.3590292079831,-4.93906964482095,
56.8698529411764));
#159496=CARTESIAN_POINT('Ctrl Pts',(-17.8167014103155,-3.33051870318735,
55.3757352941178));
#159497=CARTESIAN_POINT('Ctrl Pts',(-17.9710104137728,-1.66525935159368,
53.8816176470589));
#159498=CARTESIAN_POINT('Ctrl Pts',(-18.1253194172301,-1.10985572039171E-15,
52.3875));
#159499=CARTESIAN_POINT('Ctrl Pts',(-17.9710104137728,1.66525935159367,
50.8933823529412));
#159500=CARTESIAN_POINT('Ctrl Pts',(-17.8167014103155,3.33051870318735,
49.3992647058823));
#159501=CARTESIAN_POINT('Ctrl Pts',(-17.3590292079831,4.93906964482096,
47.9051470588237));
#159502=CARTESIAN_POINT('Ctrl Pts',(-16.9013570056506,6.54762058645456,
46.4110294117648));
#159503=CARTESIAN_POINT('Ctrl Pts',(-16.1559070823762,8.04468584505497,
44.9169117647059));
#159504=CARTESIAN_POINT('Ctrl Pts',(-15.4104571591017,9.54175110365538,
43.422794117647));
#159505=CARTESIAN_POINT('Ctrl Pts',(-14.4026149179538,10.8763499173728,
41.9286764705882));
#159506=CARTESIAN_POINT('Ctrl Pts',(-13.3947726768058,12.2109487310903,
40.4345588235295));
#159507=CARTESIAN_POINT('Ctrl Pts',(-12.1588589765331,13.3376329379985,
38.9404411764707));
#159508=CARTESIAN_POINT('Ctrl Pts',(-10.9229452762603,14.4643171449067,
37.4463235294118));
#159509=CARTESIAN_POINT('Ctrl Pts',(-9.50104767561052,15.3447188656481,
35.9522058823529));
#159510=CARTESIAN_POINT('Ctrl Pts',(-8.07915007496071,16.2251205863895,
34.4580882352941));
#159511=CARTESIAN_POINT('Ctrl Pts',(-6.51968959134574,16.8292587962898,
32.9639705882354));
#159512=CARTESIAN_POINT('Ctrl Pts',(-4.96022910773078,17.4333970061901,
31.4698529411765));
#159513=CARTESIAN_POINT('Ctrl Pts',(-3.31631129755346,17.7406985030951,
29.9757352941177));
#159514=CARTESIAN_POINT('Ctrl Pts',(-1.67239348737615,18.048,28.4816176470588));
#159515=CARTESIAN_POINT('Ctrl Pts',(-2.21024254310115E-15,18.048,26.9874999999999));
#159516=CARTESIAN_POINT('Ctrl Pts',(1.67239348737616,18.048,25.4933823529413));
#159517=CARTESIAN_POINT('Ctrl Pts',(3.31631129755346,17.7406985030951,23.9992647058824));
#159518=CARTESIAN_POINT('Ctrl Pts',(4.96022910773077,17.4333970061901,22.5051470588236));
#159519=CARTESIAN_POINT('Ctrl Pts',(6.51968959134575,16.8292587962898,21.0110294117647));
#159520=CARTESIAN_POINT('Ctrl Pts',(8.07915007496071,16.2251205863895,19.5169117647058));
#159521=CARTESIAN_POINT('Ctrl Pts',(9.50104767561053,15.3447188656481,18.0227941176472));
#159522=CARTESIAN_POINT('Ctrl Pts',(10.9229452762603,14.4643171449067,16.5286764705883));
#159523=CARTESIAN_POINT('Ctrl Pts',(12.1588589765331,13.3376329379985,15.0345588235294));
#159524=CARTESIAN_POINT('Ctrl Pts',(13.3947726768058,12.2109487310903,13.5404411764706));
#159525=CARTESIAN_POINT('Ctrl Pts',(14.4026149179538,10.8763499173728,12.0463235294117));
#159526=CARTESIAN_POINT('Ctrl Pts',(15.4104571591017,9.54175110365538,10.5522058823531));
#159527=CARTESIAN_POINT('Ctrl Pts',(16.1559070823762,8.04468584505496,9.05808823529419));
#159528=CARTESIAN_POINT('Ctrl Pts',(16.9013570056506,6.54762058645456,7.56397058823533));
#159529=CARTESIAN_POINT('Ctrl Pts',(17.3590292079831,4.93906964482096,6.06985294117646));
#159530=CARTESIAN_POINT('Ctrl Pts',(17.8167014103155,3.33051870318735,4.57573529411759));
#159531=CARTESIAN_POINT('Ctrl Pts',(17.9710104137728,1.66525935159367,3.08161764705894));
#159532=CARTESIAN_POINT('Ctrl Pts',(18.1253194172301,3.32956716117513E-15,
1.58750000000007));
#159533=CARTESIAN_POINT('Ctrl Pts',(17.9710104137728,-1.66525935159367,
0.093382352941207));
#159534=CARTESIAN_POINT('Ctrl Pts',(17.8167014103155,-3.33051870318736,
-1.40073529411766));
#159535=CARTESIAN_POINT('Ctrl Pts',(17.3590292079831,-4.93906964482095,
-2.89485294117653));
#159536=CARTESIAN_POINT('Ctrl Pts',(16.9013570056506,-6.54762058645456,
-4.38897058823517));
#159537=CARTESIAN_POINT('Ctrl Pts',(16.1559070823762,-8.04468584505497,
-5.88308823529404));
#159538=CARTESIAN_POINT('Ctrl Pts',(15.4104571591017,-9.54175110365538,
-7.37720588235291));
#159539=CARTESIAN_POINT('Ctrl Pts',(14.4026149179538,-10.8763499173728,
-8.87132352941178));
#159540=CARTESIAN_POINT('Ctrl Pts',(13.3947726768058,-12.2109487310903,
-10.3654411764706));
#159541=CARTESIAN_POINT('Ctrl Pts',(12.1588589765331,-13.3376329379985,
-11.8595588235293));
#159542=CARTESIAN_POINT('Ctrl Pts',(10.9229452762603,-14.4643171449067,
-13.3536764705882));
#159543=CARTESIAN_POINT('Ctrl Pts',(9.50104767561053,-15.3447188656481,
-14.847794117647));
#159544=CARTESIAN_POINT('Ctrl Pts',(8.07915007496071,-16.2251205863895,
-16.3419117647059));
#159545=CARTESIAN_POINT('Ctrl Pts',(6.51968959134574,-16.8292587962898,
-17.8360294117648));
#159546=CARTESIAN_POINT('Ctrl Pts',(4.96022910773078,-17.4333970061901,
-19.3301470588234));
#159547=CARTESIAN_POINT('Ctrl Pts',(3.31631129755346,-17.7406985030951,
-20.8242647058823));
#159548=CARTESIAN_POINT('Ctrl Pts',(1.67239348737615,-18.048,-22.3183823529411));
#159549=CARTESIAN_POINT('Ctrl Pts',(0.,-18.048,-23.8125));
#159550=CARTESIAN_POINT('Ctrl Pts',(-1.67239348737615,-18.048,-25.3066176470589));
#159551=CARTESIAN_POINT('Ctrl Pts',(-3.31631129755346,-17.7406985030951,
-26.8007352941175));
#159552=CARTESIAN_POINT('Ctrl Pts',(-4.96022910773077,-17.4333970061901,
-28.2948529411764));
#159553=CARTESIAN_POINT('Ctrl Pts',(-6.51968959134574,-16.8292587962898,
-29.7889705882353));
#159554=CARTESIAN_POINT('Ctrl Pts',(-8.07915007496071,-16.2251205863895,
-31.2830882352941));
#159555=CARTESIAN_POINT('Ctrl Pts',(-9.50104767561052,-15.3447188656481,
-32.777205882353));
#159556=CARTESIAN_POINT('Ctrl Pts',(-10.9229452762603,-14.4643171449067,
-34.2713235294116));
#159557=CARTESIAN_POINT('Ctrl Pts',(-12.1588589765331,-13.3376329379985,
-35.7654411764705));
#159558=CARTESIAN_POINT('Ctrl Pts',(-13.3947726768058,-12.2109487310903,
-37.2595588235294));
#159559=CARTESIAN_POINT('Ctrl Pts',(-14.4026149179538,-10.8763499173728,
-38.7536764705882));
#159560=CARTESIAN_POINT('Ctrl Pts',(-15.4104571591017,-9.54175110365538,
-40.2477941176471));
#159561=CARTESIAN_POINT('Ctrl Pts',(-16.1559070823762,-8.04468584505497,
-41.7419117647058));
#159562=CARTESIAN_POINT('Ctrl Pts',(-16.9013570056506,-6.54762058645456,
-43.2360294117646));
#159563=CARTESIAN_POINT('Ctrl Pts',(-17.3590292079831,-4.93906964482095,
-44.7301470588235));
#159564=CARTESIAN_POINT('Ctrl Pts',(-17.8167014103155,-3.33051870318735,
-46.2242647058824));
#159565=CARTESIAN_POINT('Ctrl Pts',(-17.9710104137728,-1.66525935159368,
-47.7183823529412));
#159566=CARTESIAN_POINT('Ctrl Pts',(-18.1253194172301,-1.10985572039171E-15,
-49.2124999999999));
#159567=CARTESIAN_POINT('Ctrl Pts',(-17.9710104137728,1.66525935159367,
-50.7066176470587));
#159568=CARTESIAN_POINT('Ctrl Pts',(-17.8167014103155,3.33051870318735,
-52.2007352941176));
#159569=CARTESIAN_POINT('Ctrl Pts',(-17.3590292079831,4.93906964482096,
-53.6948529411765));
#159570=CARTESIAN_POINT('Ctrl Pts',(-16.9013570056506,6.54762058645456,
-55.1889705882354));
#159571=CARTESIAN_POINT('Ctrl Pts',(-16.1559070823762,8.04468584505497,
-56.683088235294));
#159572=CARTESIAN_POINT('Ctrl Pts',(-15.4104571591017,9.54175110365538,
-58.1772058823529));
#159573=CARTESIAN_POINT('Ctrl Pts',(-14.4026149179538,10.8763499173728,
-59.6713235294117));
#159574=CARTESIAN_POINT('Ctrl Pts',(-13.3947726768058,12.2109487310903,
-61.1654411764706));
#159575=CARTESIAN_POINT('Ctrl Pts',(-12.1588589765331,13.3376329379985,
-62.6595588235295));
#159576=CARTESIAN_POINT('Ctrl Pts',(-10.9229452762603,14.4643171449067,
-64.1536764705881));
#159577=CARTESIAN_POINT('Ctrl Pts',(-9.50104767561052,15.3447188656481,
-65.647794117647));
#159578=CARTESIAN_POINT('Ctrl Pts',(-8.07915007496071,16.2251205863895,
-67.1419117647059));
#159579=CARTESIAN_POINT('Ctrl Pts',(-6.51968959134574,16.8292587962898,
-68.6360294117647));
#159580=CARTESIAN_POINT('Ctrl Pts',(-4.96022910773078,17.4333970061901,
-70.1301470588236));
#159581=CARTESIAN_POINT('Ctrl Pts',(-3.31631129755346,17.7406985030951,
-71.6242647058822));
#159582=CARTESIAN_POINT('Ctrl Pts',(-1.67239348737615,18.048,-73.1183823529411));
#159583=CARTESIAN_POINT('Ctrl Pts',(-2.21024254310115E-15,18.048,-74.6125));
#159584=CARTESIAN_POINT('Ctrl Pts',(1.67239348737616,18.048,-76.1066176470589));
#159585=CARTESIAN_POINT('Ctrl Pts',(3.31631129755346,17.7406985030951,-77.6007352941177));
#159586=CARTESIAN_POINT('Ctrl Pts',(4.96022910773077,17.4333970061901,-79.0948529411764));
#159587=CARTESIAN_POINT('Ctrl Pts',(6.51968959134575,16.8292587962898,-80.5889705882352));
#159588=CARTESIAN_POINT('Ctrl Pts',(8.07915007496071,16.2251205863895,-82.0830882352941));
#159589=CARTESIAN_POINT('Ctrl Pts',(9.50104767561053,15.3447188656481,-83.577205882353));
#159590=CARTESIAN_POINT('Ctrl Pts',(10.9229452762603,14.4643171449067,-85.0713235294118));
#159591=CARTESIAN_POINT('Ctrl Pts',(12.1588589765331,13.3376329379985,-86.5654411764705));
#159592=CARTESIAN_POINT('Ctrl Pts',(13.3947726768058,12.2109487310903,-88.0595588235294));
#159593=CARTESIAN_POINT('Ctrl Pts',(14.4026149179538,10.8763499173728,-89.5536764705882));
#159594=CARTESIAN_POINT('Ctrl Pts',(15.4104571591017,9.54175110365538,-91.0477941176471));
#159595=CARTESIAN_POINT('Ctrl Pts',(16.1559070823762,8.04468584505496,-92.541911764706));
#159596=CARTESIAN_POINT('Ctrl Pts',(16.9013570056506,6.54762058645456,-94.0360294117646));
#159597=CARTESIAN_POINT('Ctrl Pts',(17.3590292079831,4.93906964482096,-95.5301470588235));
#159598=CARTESIAN_POINT('Ctrl Pts',(17.8167014103155,3.33051870318735,-97.0242647058824));
#159599=CARTESIAN_POINT('Ctrl Pts',(17.9710104137728,1.66525935159367,-98.5183823529412));
#159600=CARTESIAN_POINT('Ctrl Pts',(18.1253194172301,3.32956716117513E-15,
-100.0125));
#159601=CARTESIAN_POINT('Ctrl Pts',(17.9710104137728,-1.66525935159367,
-101.506617647059));
#159602=CARTESIAN_POINT('Ctrl Pts',(17.8167014103155,-3.33051870318736,
-103.000735294118));
#159603=CARTESIAN_POINT('Ctrl Pts',(17.3590292079831,-4.93906964482095,
-104.494852941176));
#159604=CARTESIAN_POINT('Ctrl Pts',(16.9013570056506,-6.54762058645456,
-105.988970588235));
#159605=CARTESIAN_POINT('Ctrl Pts',(16.1559070823762,-8.04468584505497,
-107.483088235294));
#159606=CARTESIAN_POINT('Ctrl Pts',(15.4104571591017,-9.54175110365538,
-108.977205882353));
#159607=CARTESIAN_POINT('Ctrl Pts',(14.4026149179538,-10.8763499173728,
-110.471323529412));
#159608=CARTESIAN_POINT('Ctrl Pts',(13.3947726768058,-12.2109487310903,
-111.965441176471));
#159609=CARTESIAN_POINT('Ctrl Pts',(12.1588589765331,-13.3376329379985,
-113.459558823529));
#159610=CARTESIAN_POINT('Ctrl Pts',(10.9229452762603,-14.4643171449067,
-114.953676470588));
#159611=CARTESIAN_POINT('Ctrl Pts',(9.50104767561053,-15.3447188656481,
-116.447794117647));
#159612=CARTESIAN_POINT('Ctrl Pts',(8.07915007496071,-16.2251205863895,
-117.941911764706));
#159613=CARTESIAN_POINT('Ctrl Pts',(6.51968959134574,-16.8292587962898,
-119.436029411765));
#159614=CARTESIAN_POINT('Ctrl Pts',(4.96022910773078,-17.4333970061901,
-120.930147058824));
#159615=CARTESIAN_POINT('Ctrl Pts',(3.31631129755346,-17.7406985030951,
-122.424264705882));
#159616=CARTESIAN_POINT('Ctrl Pts',(1.67239348737615,-18.048,-123.918382352941));
#159617=CARTESIAN_POINT('Ctrl Pts',(0.,-18.048,-125.4125));
#159618=CARTESIAN_POINT('Ctrl Pts',(-1.67239348737615,-18.048,-126.906617647059));
#159619=CARTESIAN_POINT('Ctrl Pts',(-3.31631129755346,-17.7406985030951,
-128.400735294118));
#159620=CARTESIAN_POINT('Ctrl Pts',(-4.96022910773077,-17.4333970061901,
-129.894852941177));
#159621=CARTESIAN_POINT('Ctrl Pts',(-6.51968959134574,-16.8292587962898,
-131.388970588235));
#159622=CARTESIAN_POINT('Ctrl Pts',(-8.07915007496071,-16.2251205863895,
-132.883088235294));
#159623=CARTESIAN_POINT('Ctrl Pts',(-9.50104767561052,-15.3447188656481,
-134.377205882353));
#159624=CARTESIAN_POINT('Ctrl Pts',(-10.9229452762603,-14.4643171449067,
-135.871323529412));
#159625=CARTESIAN_POINT('Ctrl Pts',(-12.1588589765331,-13.3376329379985,
-137.365441176471));
#159626=CARTESIAN_POINT('Ctrl Pts',(-13.3947726768058,-12.2109487310903,
-138.859558823529));
#159627=CARTESIAN_POINT('Ctrl Pts',(-14.4026149179538,-10.8763499173728,
-140.353676470588));
#159628=CARTESIAN_POINT('Ctrl Pts',(-15.4104571591017,-9.54175110365538,
-141.847794117647));
#159629=CARTESIAN_POINT('Ctrl Pts',(-16.1559070823762,-8.04468584505497,
-143.341911764706));
#159630=CARTESIAN_POINT('Ctrl Pts',(-16.9013570056506,-6.54762058645456,
-144.836029411765));
#159631=CARTESIAN_POINT('Ctrl Pts',(-17.3590292079831,-4.93906964482095,
-146.330147058823));
#159632=CARTESIAN_POINT('Ctrl Pts',(-17.8167014103155,-3.33051870318735,
-147.824264705882));
#159633=CARTESIAN_POINT('Ctrl Pts',(-17.9710104137728,-1.66525935159368,
-149.318382352941));
#159634=CARTESIAN_POINT('Ctrl Pts',(-18.1253194172301,-1.10985572039171E-15,
-150.8125));
#159635=CARTESIAN_POINT('Ctrl Pts',(-17.9710104137728,1.66525935159367,
-152.306617647059));
#159636=CARTESIAN_POINT('Ctrl Pts',(-17.8167014103155,3.33051870318735,
-153.800735294118));
#159637=CARTESIAN_POINT('Ctrl Pts',(-17.3590292079831,4.93906964482096,
-155.294852941176));
#159638=CARTESIAN_POINT('Ctrl Pts',(-16.9013570056506,6.54762058645456,
-156.788970588235));
#159639=CARTESIAN_POINT('Ctrl Pts',(-16.1559070823762,8.04468584505497,
-158.283088235294));
#159640=CARTESIAN_POINT('Ctrl Pts',(-15.4104571591017,9.54175110365538,
-159.777205882353));
#159641=CARTESIAN_POINT('Ctrl Pts',(-14.4026149179538,10.8763499173728,
-161.271323529412));
#159642=CARTESIAN_POINT('Ctrl Pts',(-13.3947726768058,12.2109487310903,
-162.765441176471));
#159643=CARTESIAN_POINT('Ctrl Pts',(-12.1588589765331,13.3376329379985,
-164.259558823529));
#159644=CARTESIAN_POINT('Ctrl Pts',(-10.9229452762603,14.4643171449067,
-165.753676470588));
#159645=CARTESIAN_POINT('Ctrl Pts',(-9.50104767561052,15.3447188656481,
-167.247794117647));
#159646=CARTESIAN_POINT('Ctrl Pts',(-8.07915007496071,16.2251205863895,
-168.741911764706));
#159647=CARTESIAN_POINT('Ctrl Pts',(-6.51968959134574,16.8292587962898,
-170.236029411765));
#159648=CARTESIAN_POINT('Ctrl Pts',(-4.96022910773078,17.4333970061901,
-171.730147058823));
#159649=CARTESIAN_POINT('Ctrl Pts',(-3.31631129755346,17.7406985030951,
-173.224264705882));
#159650=CARTESIAN_POINT('Ctrl Pts',(-1.67239348737615,18.048,-174.718382352941));
#159651=CARTESIAN_POINT('Ctrl Pts',(-2.21024254310115E-15,18.048,-176.2125));
#159652=CARTESIAN_POINT('Ctrl Pts',(1.67239348737616,18.048,-177.706617647059));
#159653=CARTESIAN_POINT('Ctrl Pts',(3.31631129755346,17.7406985030951,-179.200735294118));
#159654=CARTESIAN_POINT('Ctrl Pts',(4.96022910773077,17.4333970061901,-180.694852941176));
#159655=CARTESIAN_POINT('Ctrl Pts',(6.51968959134575,16.8292587962898,-182.188970588235));
#159656=CARTESIAN_POINT('Ctrl Pts',(8.07915007496071,16.2251205863895,-183.683088235294));
#159657=CARTESIAN_POINT('Ctrl Pts',(9.50104767561053,15.3447188656481,-185.177205882353));
#159658=CARTESIAN_POINT('Ctrl Pts',(10.9229452762603,14.4643171449067,-186.671323529412));
#159659=CARTESIAN_POINT('Ctrl Pts',(12.1588589765331,13.3376329379985,-188.165441176471));
#159660=CARTESIAN_POINT('Ctrl Pts',(13.3947726768058,12.2109487310903,-189.659558823529));
#159661=CARTESIAN_POINT('Ctrl Pts',(14.4026149179538,10.8763499173728,-191.153676470588));
#159662=CARTESIAN_POINT('Ctrl Pts',(15.4104571591017,9.54175110365538,-192.647794117647));
#159663=CARTESIAN_POINT('Ctrl Pts',(16.1559070823762,8.04468584505496,-194.141911764706));
#159664=CARTESIAN_POINT('Ctrl Pts',(16.9013570056506,6.54762058645456,-195.636029411765));
#159665=CARTESIAN_POINT('Ctrl Pts',(17.3590292079831,4.93906964482096,-197.130147058824));
#159666=CARTESIAN_POINT('Ctrl Pts',(17.8167014103155,3.33051870318735,-198.624264705882));
#159667=CARTESIAN_POINT('Ctrl Pts',(17.9710104137728,1.66525935159367,-200.118382352941));
#159668=CARTESIAN_POINT('Ctrl Pts',(18.1253194172301,3.32956716117513E-15,
-201.6125));
#159669=CARTESIAN_POINT('Ctrl Pts',(17.9710104137728,-1.66525935159367,
-203.106617647059));
#159670=CARTESIAN_POINT('Ctrl Pts',(17.8167014103155,-3.33051870318736,
-204.600735294118));
#159671=CARTESIAN_POINT('Ctrl Pts',(17.3590292079831,-4.93906964482095,
-206.094852941176));
#159672=CARTESIAN_POINT('Ctrl Pts',(16.9013570056506,-6.54762058645456,
-207.588970588235));
#159673=CARTESIAN_POINT('Ctrl Pts',(16.1559070823762,-8.04468584505497,
-209.083088235294));
#159674=CARTESIAN_POINT('Ctrl Pts',(15.4104571591017,-9.54175110365538,
-210.577205882353));
#159675=CARTESIAN_POINT('Ctrl Pts',(14.4026149179538,-10.8763499173728,
-212.071323529412));
#159676=CARTESIAN_POINT('Ctrl Pts',(13.3947726768058,-12.2109487310903,
-213.56544117647));
#159677=CARTESIAN_POINT('Ctrl Pts',(12.1588589765331,-13.3376329379985,
-215.059558823529));
#159678=CARTESIAN_POINT('Ctrl Pts',(10.9229452762603,-14.4643171449067,
-216.553676470588));
#159679=CARTESIAN_POINT('Ctrl Pts',(9.50104767561053,-15.3447188656481,
-218.047794117647));
#159680=CARTESIAN_POINT('Ctrl Pts',(8.07915007496071,-16.2251205863895,
-219.541911764706));
#159681=CARTESIAN_POINT('Ctrl Pts',(6.51968959134574,-16.8292587962898,
-221.036029411765));
#159682=CARTESIAN_POINT('Ctrl Pts',(4.96022910773078,-17.4333970061901,
-222.530147058823));
#159683=CARTESIAN_POINT('Ctrl Pts',(3.31631129755346,-17.7406985030951,
-224.024264705882));
#159684=CARTESIAN_POINT('Ctrl Pts',(1.67239348737615,-18.048,-225.518382352941));
#159685=CARTESIAN_POINT('Ctrl Pts',(0.,-18.048,-227.0125));
#159686=CARTESIAN_POINT('Ctrl Pts',(-1.67239348737615,-18.048,-228.506617647059));
#159687=CARTESIAN_POINT('Ctrl Pts',(-3.31631129755346,-17.7406985030951,
-230.000735294118));
#159688=CARTESIAN_POINT('Ctrl Pts',(-4.96022910773077,-17.4333970061901,
-231.494852941176));
#159689=CARTESIAN_POINT('Ctrl Pts',(-6.51968959134574,-16.8292587962898,
-232.988970588235));
#159690=CARTESIAN_POINT('Ctrl Pts',(-8.07915007496071,-16.2251205863895,
-234.483088235294));
#159691=CARTESIAN_POINT('Ctrl Pts',(-9.50104767561052,-15.3447188656481,
-235.977205882353));
#159692=CARTESIAN_POINT('Ctrl Pts',(-10.9229452762603,-14.4643171449067,
-237.471323529412));
#159693=CARTESIAN_POINT('Ctrl Pts',(-12.1588589765331,-13.3376329379985,
-238.965441176471));
#159694=CARTESIAN_POINT('Ctrl Pts',(-13.3947726768058,-12.2109487310903,
-240.459558823529));
#159695=CARTESIAN_POINT('Ctrl Pts',(-14.4026149179538,-10.8763499173728,
-241.953676470588));
#159696=CARTESIAN_POINT('Ctrl Pts',(-15.4104571591017,-9.54175110365538,
-243.447794117647));
#159697=CARTESIAN_POINT('Ctrl Pts',(-16.1559070823762,-8.04468584505497,
-244.941911764706));
#159698=CARTESIAN_POINT('Ctrl Pts',(-16.9013570056506,-6.54762058645456,
-246.436029411765));
#159699=CARTESIAN_POINT('Ctrl Pts',(-17.3590292079831,-4.93906964482095,
-247.930147058824));
#159700=CARTESIAN_POINT('Ctrl Pts',(-17.8167014103155,-3.33051870318735,
-249.424264705882));
#159701=CARTESIAN_POINT('Ctrl Pts',(-17.9710104137728,-1.66525935159368,
-250.918382352941));
#159702=CARTESIAN_POINT('Ctrl Pts',(-18.1253194172301,-1.10985572039171E-15,
-252.4125));
#159703=CARTESIAN_POINT('Ctrl Pts',(-17.9710104137728,1.66525935159367,
-253.906617647059));
#159704=CARTESIAN_POINT('Ctrl Pts',(-17.8167014103155,3.33051870318735,
-255.400735294118));
#159705=CARTESIAN_POINT('Ctrl Pts',(-17.3590292079831,4.93906964482096,
-256.894852941177));
#159706=CARTESIAN_POINT('Ctrl Pts',(-16.9013570056506,6.54762058645456,
-258.388970588235));
#159707=CARTESIAN_POINT('Ctrl Pts',(-16.1559070823762,8.04468584505497,
-259.883088235294));
#159708=CARTESIAN_POINT('Ctrl Pts',(-15.4104571591017,9.54175110365538,
-261.377205882353));
#159709=CARTESIAN_POINT('Ctrl Pts',(-14.4026149179538,10.8763499173728,
-262.871323529412));
#159710=CARTESIAN_POINT('Ctrl Pts',(-13.3947726768058,12.2109487310903,
-264.365441176471));
#159711=CARTESIAN_POINT('Ctrl Pts',(-12.1588589765331,13.3376329379985,
-265.859558823529));
#159712=CARTESIAN_POINT('Ctrl Pts',(-10.9229452762603,14.4643171449067,
-267.353676470588));
#159713=CARTESIAN_POINT('Ctrl Pts',(-9.50104767561052,15.3447188656481,
-268.847794117647));
#159714=CARTESIAN_POINT('Ctrl Pts',(-8.07915007496071,16.2251205863895,
-270.341911764706));
#159715=CARTESIAN_POINT('Ctrl Pts',(-6.51968959134574,16.8292587962898,
-271.836029411765));
#159716=CARTESIAN_POINT('Ctrl Pts',(-4.96022910773078,17.4333970061901,
-273.330147058823));
#159717=CARTESIAN_POINT('Ctrl Pts',(-3.31631129755346,17.7406985030951,
-274.824264705882));
#159718=CARTESIAN_POINT('Ctrl Pts',(-1.67239348737615,18.048,-276.318382352941));
#159719=CARTESIAN_POINT('Ctrl Pts',(-2.21024254310115E-15,18.048,-277.8125));
#159720=CARTESIAN_POINT('Ctrl Pts',(1.67239348737616,18.048,-279.306617647059));
#159721=CARTESIAN_POINT('Ctrl Pts',(3.31631129755346,17.7406985030951,-280.800735294118));
#159722=CARTESIAN_POINT('Ctrl Pts',(4.96022910773077,17.4333970061901,-282.294852941176));
#159723=CARTESIAN_POINT('Ctrl Pts',(6.51968959134575,16.8292587962898,-283.788970588235));
#159724=CARTESIAN_POINT('Ctrl Pts',(8.07915007496071,16.2251205863895,-285.283088235294));
#159725=CARTESIAN_POINT('Ctrl Pts',(9.50104767561053,15.3447188656481,-286.777205882353));
#159726=CARTESIAN_POINT('Ctrl Pts',(10.9229452762603,14.4643171449067,-288.271323529412));
#159727=CARTESIAN_POINT('Ctrl Pts',(12.1588589765331,13.3376329379985,-289.765441176471));
#159728=CARTESIAN_POINT('Ctrl Pts',(13.3947726768058,12.2109487310903,-291.259558823529));
#159729=CARTESIAN_POINT('Ctrl Pts',(14.4026149179538,10.8763499173728,-292.753676470588));
#159730=CARTESIAN_POINT('Ctrl Pts',(15.4104571591017,9.54175110365538,-294.247794117647));
#159731=CARTESIAN_POINT('Ctrl Pts',(16.1559070823762,8.04468584505496,-295.741911764706));
#159732=CARTESIAN_POINT('Ctrl Pts',(16.9013570056506,6.54762058645456,-297.236029411765));
#159733=CARTESIAN_POINT('Ctrl Pts',(17.3590292079831,4.93906964482096,-298.730147058823));
#159734=CARTESIAN_POINT('Ctrl Pts',(17.8167014103155,3.33051870318735,-300.224264705882));
#159735=CARTESIAN_POINT('Ctrl Pts',(17.9710104137728,1.66525935159367,-301.718382352941));
#159736=CARTESIAN_POINT('Ctrl Pts',(18.1253194172301,3.32956716117513E-15,
-303.2125));
#159737=CARTESIAN_POINT('Ctrl Pts',(17.9710104137728,-1.66525935159367,
-304.706617647059));
#159738=CARTESIAN_POINT('Ctrl Pts',(17.8167014103155,-3.33051870318736,
-306.200735294118));
#159739=CARTESIAN_POINT('Ctrl Pts',(17.3590292079831,-4.93906964482095,
-307.694852941176));
#159740=CARTESIAN_POINT('Ctrl Pts',(16.9013570056506,-6.54762058645456,
-309.188970588235));
#159741=CARTESIAN_POINT('Ctrl Pts',(16.1559070823762,-8.04468584505497,
-310.683088235294));
#159742=CARTESIAN_POINT('Ctrl Pts',(15.4104571591017,-9.54175110365538,
-312.177205882353));
#159743=CARTESIAN_POINT('Ctrl Pts',(14.4026149179538,-10.8763499173728,
-313.671323529412));
#159744=CARTESIAN_POINT('Ctrl Pts',(13.3947726768058,-12.2109487310903,
-315.165441176471));
#159745=CARTESIAN_POINT('Ctrl Pts',(12.1588589765331,-13.3376329379985,
-316.659558823529));
#159746=CARTESIAN_POINT('Ctrl Pts',(10.9229452762603,-14.4643171449067,
-318.153676470588));
#159747=CARTESIAN_POINT('Ctrl Pts',(9.50104767561053,-15.3447188656481,
-319.647794117647));
#159748=CARTESIAN_POINT('Ctrl Pts',(8.07915007496071,-16.2251205863895,
-321.141911764706));
#159749=CARTESIAN_POINT('Ctrl Pts',(6.51968959134574,-16.8292587962898,
-322.636029411765));
#159750=CARTESIAN_POINT('Ctrl Pts',(4.96022910773078,-17.4333970061901,
-324.130147058824));
#159751=CARTESIAN_POINT('Ctrl Pts',(3.31631129755346,-17.7406985030951,
-325.624264705882));
#159752=CARTESIAN_POINT('Ctrl Pts',(1.67239348737615,-18.048,-327.118382352941));
#159753=CARTESIAN_POINT('Ctrl Pts',(0.,-18.048,-328.6125));
#159754=CARTESIAN_POINT('Ctrl Pts',(-1.67239348737615,-18.048,-330.106617647059));
#159755=CARTESIAN_POINT('Ctrl Pts',(-3.31631129755346,-17.7406985030951,
-331.600735294118));
#159756=CARTESIAN_POINT('Ctrl Pts',(-4.96022910773077,-17.4333970061901,
-333.094852941176));
#159757=CARTESIAN_POINT('Ctrl Pts',(-6.51968959134574,-16.8292587962898,
-334.588970588235));
#159758=CARTESIAN_POINT('Ctrl Pts',(-8.07915007496071,-16.2251205863895,
-336.083088235294));
#159759=CARTESIAN_POINT('Ctrl Pts',(-9.50104767561052,-15.3447188656481,
-337.577205882353));
#159760=CARTESIAN_POINT('Ctrl Pts',(-10.9229452762603,-14.4643171449067,
-339.071323529412));
#159761=CARTESIAN_POINT('Ctrl Pts',(-12.1588589765331,-13.3376329379985,
-340.56544117647));
#159762=CARTESIAN_POINT('Ctrl Pts',(-13.3947726768058,-12.2109487310903,
-342.059558823529));
#159763=CARTESIAN_POINT('Ctrl Pts',(-14.4026149179538,-10.8763499173728,
-343.553676470588));
#159764=CARTESIAN_POINT('Ctrl Pts',(-15.4104571591017,-9.54175110365538,
-345.047794117647));
#159765=CARTESIAN_POINT('Ctrl Pts',(-16.1559070823762,-8.04468584505497,
-346.541911764706));
#159766=CARTESIAN_POINT('Ctrl Pts',(-16.9013570056506,-6.54762058645456,
-348.036029411765));
#159767=CARTESIAN_POINT('Ctrl Pts',(-17.3590292079831,-4.93906964482095,
-349.530147058823));
#159768=CARTESIAN_POINT('Ctrl Pts',(-17.8167014103155,-3.33051870318735,
-351.024264705883));
#159769=CARTESIAN_POINT('Ctrl Pts',(-17.9710104137728,-1.66525935159368,
-352.518382352941));
#159770=CARTESIAN_POINT('Ctrl Pts',(-18.1253194172301,-1.10985572039171E-15,
-354.0125));
#159771=CARTESIAN_POINT('Ctrl Pts',(-17.9710104137728,1.66525935159367,
-355.506617647059));
#159772=CARTESIAN_POINT('Ctrl Pts',(-17.8167014103155,3.33051870318735,
-357.000735294118));
#159773=CARTESIAN_POINT('Ctrl Pts',(-17.3590292079831,4.93906964482096,
-358.494852941176));
#159774=CARTESIAN_POINT('Ctrl Pts',(-16.9013570056506,6.54762058645456,
-359.988970588235));
#159775=CARTESIAN_POINT('Ctrl Pts',(-16.1559070823762,8.04468584505497,
-361.483088235294));
#159776=CARTESIAN_POINT('Ctrl Pts',(-15.4104571591017,9.54175110365538,
-362.977205882353));
#159777=CARTESIAN_POINT('Ctrl Pts',(-14.4026149179538,10.8763499173728,
-364.471323529412));
#159778=CARTESIAN_POINT('Ctrl Pts',(-13.3947726768058,12.2109487310903,
-365.965441176471));
#159779=CARTESIAN_POINT('Ctrl Pts',(-12.1588589765331,13.3376329379985,
-367.459558823529));
#159780=CARTESIAN_POINT('Ctrl Pts',(-10.9229452762603,14.4643171449067,
-368.953676470588));
#159781=CARTESIAN_POINT('Ctrl Pts',(-9.50104767561052,15.3447188656481,
-370.447794117647));
#159782=CARTESIAN_POINT('Ctrl Pts',(-8.07915007496071,16.2251205863895,
-371.941911764706));
#159783=CARTESIAN_POINT('Ctrl Pts',(-6.51968959134574,16.8292587962898,
-373.436029411765));
#159784=CARTESIAN_POINT('Ctrl Pts',(-4.96022910773078,17.4333970061901,
-374.930147058824));
#159785=CARTESIAN_POINT('Ctrl Pts',(-3.31631129755346,17.7406985030951,
-376.424264705882));
#159786=CARTESIAN_POINT('Ctrl Pts',(-1.67239348737615,18.048,-377.918382352941));
#159787=CARTESIAN_POINT('Ctrl Pts',(-2.21024254310115E-15,18.048,-379.4125));
#159788=CARTESIAN_POINT('Ctrl Pts',(1.67239348737616,18.048,-380.906617647059));
#159789=CARTESIAN_POINT('Ctrl Pts',(3.31631129755346,17.7406985030951,-382.400735294118));
#159790=CARTESIAN_POINT('Ctrl Pts',(4.96022910773077,17.4333970061901,-383.894852941177));
#159791=CARTESIAN_POINT('Ctrl Pts',(6.51968959134575,16.8292587962898,-385.388970588235));
#159792=CARTESIAN_POINT('Ctrl Pts',(8.07915007496071,16.2251205863895,-386.883088235294));
#159793=CARTESIAN_POINT('Ctrl Pts',(9.50104767561053,15.3447188656481,-388.377205882353));
#159794=CARTESIAN_POINT('Ctrl Pts',(10.9229452762603,14.4643171449067,-389.871323529412));
#159795=CARTESIAN_POINT('Ctrl Pts',(12.1588589765331,13.3376329379985,-391.365441176471));
#159796=CARTESIAN_POINT('Ctrl Pts',(13.3947726768058,12.2109487310903,-392.859558823529));
#159797=CARTESIAN_POINT('Ctrl Pts',(14.4026149179538,10.8763499173728,-394.353676470588));
#159798=CARTESIAN_POINT('Ctrl Pts',(15.4104571591017,9.54175110365538,-395.847794117647));
#159799=CARTESIAN_POINT('Ctrl Pts',(16.1559070823762,8.04468584505496,-397.341911764706));
#159800=CARTESIAN_POINT('Ctrl Pts',(16.9013570056506,6.54762058645456,-398.836029411765));
#159801=CARTESIAN_POINT('Ctrl Pts',(17.3590292079831,4.93906964482096,-400.330147058823));
#159802=CARTESIAN_POINT('Ctrl Pts',(17.8167014103155,3.33051870318735,-401.824264705882));
#159803=CARTESIAN_POINT('Ctrl Pts',(17.9710104137728,1.66525935159367,-403.318382352941));
#159804=CARTESIAN_POINT('Ctrl Pts',(18.1253194172301,3.32956716117513E-15,
-404.8125));
#159805=CARTESIAN_POINT('Ctrl Pts',(17.9710104137728,-1.66525935159367,
-406.306617647059));
#159806=CARTESIAN_POINT('Ctrl Pts',(17.8167014103155,-3.33051870318736,
-407.800735294118));
#159807=CARTESIAN_POINT('Ctrl Pts',(17.3590292079831,-4.93906964482095,
-409.294852941176));
#159808=CARTESIAN_POINT('Ctrl Pts',(16.9013570056506,-6.54762058645456,
-410.788970588235));
#159809=CARTESIAN_POINT('Ctrl Pts',(16.1559070823762,-8.04468584505497,
-412.283088235294));
#159810=CARTESIAN_POINT('Ctrl Pts',(15.4104571591017,-9.54175110365538,
-413.777205882353));
#159811=CARTESIAN_POINT('Ctrl Pts',(14.4026149179538,-10.8763499173728,
-415.271323529412));
#159812=CARTESIAN_POINT('Ctrl Pts',(13.3947726768058,-12.2109487310903,
-416.765441176471));
#159813=CARTESIAN_POINT('Ctrl Pts',(12.1588589765331,-13.3376329379985,
-418.259558823529));
#159814=CARTESIAN_POINT('Ctrl Pts',(10.9229452762603,-14.4643171449067,
-419.753676470588));
#159815=CARTESIAN_POINT('Ctrl Pts',(9.50104767561053,-15.3447188656481,
-421.247794117647));
#159816=CARTESIAN_POINT('Ctrl Pts',(8.07915007496071,-16.2251205863895,
-422.741911764706));
#159817=CARTESIAN_POINT('Ctrl Pts',(6.51968959134574,-16.8292587962898,
-424.236029411765));
#159818=CARTESIAN_POINT('Ctrl Pts',(4.96022910773078,-17.4333970061901,
-425.730147058824));
#159819=CARTESIAN_POINT('Ctrl Pts',(3.31631129755346,-17.7406985030951,
-427.224264705882));
#159820=CARTESIAN_POINT('Ctrl Pts',(1.67239348737615,-18.048,-428.718382352941));
#159821=CARTESIAN_POINT('Ctrl Pts',(0.,-18.048,-430.2125));
#159822=CARTESIAN_POINT('Ctrl Pts',(-1.67239348737615,-18.048,-431.706617647059));
#159823=CARTESIAN_POINT('Ctrl Pts',(-3.31631129755346,-17.7406985030951,
-433.200735294118));
#159824=CARTESIAN_POINT('Ctrl Pts',(-4.96022910773077,-17.4333970061901,
-434.694852941176));
#159825=CARTESIAN_POINT('Ctrl Pts',(-6.51968959134574,-16.8292587962898,
-436.188970588235));
#159826=CARTESIAN_POINT('Ctrl Pts',(-8.07915007496071,-16.2251205863895,
-437.683088235294));
#159827=CARTESIAN_POINT('Ctrl Pts',(-9.50104767561052,-15.3447188656481,
-439.177205882353));
#159828=CARTESIAN_POINT('Ctrl Pts',(-10.9229452762603,-14.4643171449067,
-440.671323529412));
#159829=CARTESIAN_POINT('Ctrl Pts',(-12.1588589765331,-13.3376329379985,
-442.165441176471));
#159830=CARTESIAN_POINT('Ctrl Pts',(-13.3947726768058,-12.2109487310903,
-443.65955882353));
#159831=CARTESIAN_POINT('Ctrl Pts',(-14.4026149179538,-10.8763499173728,
-445.153676470588));
#159832=CARTESIAN_POINT('Ctrl Pts',(-15.4104571591017,-9.54175110365538,
-446.647794117647));
#159833=CARTESIAN_POINT('Ctrl Pts',(-16.1559070823762,-8.04468584505497,
-448.141911764706));
#159834=CARTESIAN_POINT('Ctrl Pts',(-16.9013570056506,-6.54762058645456,
-449.636029411765));
#159835=CARTESIAN_POINT('Ctrl Pts',(-17.3590292079831,-4.93906964482095,
-451.130147058824));
#159836=CARTESIAN_POINT('Ctrl Pts',(-17.8167014103155,-3.33051870318735,
-452.624264705882));
#159837=CARTESIAN_POINT('Ctrl Pts',(-17.9710104137728,-1.66525935159368,
-454.118382352941));
#159838=CARTESIAN_POINT('Ctrl Pts',(-18.1253194172301,-1.10985572039171E-15,
-455.6125));
#159839=CARTESIAN_POINT('Ctrl Pts',(-17.9710104137728,1.66525935159367,
-457.106617647059));
#159840=CARTESIAN_POINT('Ctrl Pts',(-17.8167014103155,3.33051870318735,
-458.600735294118));
#159841=CARTESIAN_POINT('Ctrl Pts',(-17.3590292079831,4.93906964482096,
-460.094852941176));
#159842=CARTESIAN_POINT('Ctrl Pts',(-16.9013570056506,6.54762058645456,
-461.588970588235));
#159843=CARTESIAN_POINT('Ctrl Pts',(-16.1559070823762,8.04468584505497,
-463.083088235294));
#159844=CARTESIAN_POINT('Ctrl Pts',(-15.4104571591017,9.54175110365538,
-464.577205882353));
#159845=CARTESIAN_POINT('Ctrl Pts',(-14.4026149179538,10.8763499173728,
-466.071323529412));
#159846=CARTESIAN_POINT('Ctrl Pts',(-13.3947726768058,12.2109487310903,
-467.565441176471));
#159847=CARTESIAN_POINT('Ctrl Pts',(-12.1588589765331,13.3376329379985,
-469.059558823529));
#159848=CARTESIAN_POINT('Ctrl Pts',(-10.9229452762603,14.4643171449067,
-470.553676470588));
#159849=CARTESIAN_POINT('Ctrl Pts',(-9.50104767561052,15.3447188656481,
-472.047794117647));
#159850=CARTESIAN_POINT('Ctrl Pts',(-8.07915007496071,16.2251205863895,
-473.541911764706));
#159851=CARTESIAN_POINT('Ctrl Pts',(-6.51968959134574,16.8292587962898,
-475.036029411765));
#159852=CARTESIAN_POINT('Ctrl Pts',(-4.96022910773078,17.4333970061901,
-476.530147058824));
#159853=CARTESIAN_POINT('Ctrl Pts',(-3.31631129755346,17.7406985030951,
-478.024264705882));
#159854=CARTESIAN_POINT('Ctrl Pts',(-1.67239348737615,18.048,-479.518382352941));
#159855=CARTESIAN_POINT('Ctrl Pts',(-2.21024254310115E-15,18.048,-481.0125));
#159856=CARTESIAN_POINT('Ctrl Pts',(1.67239348737616,18.048,-482.506617647059));
#159857=CARTESIAN_POINT('Ctrl Pts',(3.31631129755346,17.7406985030951,-484.000735294118));
#159858=CARTESIAN_POINT('Ctrl Pts',(4.96022910773077,17.4333970061901,-485.494852941177));
#159859=CARTESIAN_POINT('Ctrl Pts',(6.51968959134575,16.8292587962898,-486.988970588235));
#159860=CARTESIAN_POINT('Ctrl Pts',(8.07915007496071,16.2251205863895,-488.483088235294));
#159861=CARTESIAN_POINT('Ctrl Pts',(9.50104767561053,15.3447188656481,-489.977205882353));
#159862=CARTESIAN_POINT('Ctrl Pts',(10.9229452762603,14.4643171449067,-491.471323529412));
#159863=CARTESIAN_POINT('Ctrl Pts',(12.1588589765331,13.3376329379985,-492.965441176471));
#159864=CARTESIAN_POINT('Ctrl Pts',(13.3947726768058,12.2109487310903,-494.45955882353));
#159865=CARTESIAN_POINT('Ctrl Pts',(14.4026149179538,10.8763499173728,-495.953676470588));
#159866=CARTESIAN_POINT('Ctrl Pts',(15.4104571591017,9.54175110365538,-497.447794117647));
#159867=CARTESIAN_POINT('Ctrl Pts',(16.1559070823762,8.04468584505496,-498.941911764706));
#159868=CARTESIAN_POINT('Ctrl Pts',(16.9013570056506,6.54762058645456,-500.436029411765));
#159869=CARTESIAN_POINT('Ctrl Pts',(17.3590292079831,4.93906964482096,-501.930147058824));
#159870=CARTESIAN_POINT('Ctrl Pts',(17.8167014103155,3.33051870318735,-503.424264705883));
#159871=CARTESIAN_POINT('Ctrl Pts',(17.9710104137728,1.66525935159367,-504.918382352941));
#159872=CARTESIAN_POINT('Ctrl Pts',(18.1253194172301,3.32956716117513E-15,
-506.4125));
#159873=CARTESIAN_POINT('Ctrl Pts',(17.9710104137728,-1.66525935159367,
-507.906617647059));
#159874=CARTESIAN_POINT('Ctrl Pts',(17.8167014103155,-3.33051870318736,
-509.400735294117));
#159875=CARTESIAN_POINT('Ctrl Pts',(17.3590292079831,-4.93906964482095,
-510.894852941176));
#159876=CARTESIAN_POINT('Ctrl Pts',(16.9013570056506,-6.54762058645456,
-512.388970588235));
#159877=CARTESIAN_POINT('Ctrl Pts',(16.1559070823762,-8.04468584505497,
-513.883088235294));
#159878=CARTESIAN_POINT('Ctrl Pts',(15.4104571591017,-9.54175110365538,
-515.377205882353));
#159879=CARTESIAN_POINT('Ctrl Pts',(14.4026149179538,-10.8763499173728,
-516.871323529412));
#159880=CARTESIAN_POINT('Ctrl Pts',(13.3947726768058,-12.2109487310903,
-518.365441176471));
#159881=CARTESIAN_POINT('Ctrl Pts',(12.1588589765331,-13.3376329379985,
-519.85955882353));
#159882=CARTESIAN_POINT('Ctrl Pts',(10.9229452762603,-14.4643171449067,
-521.353676470588));
#159883=CARTESIAN_POINT('Ctrl Pts',(9.50104767561053,-15.3447188656481,
-522.847794117647));
#159884=CARTESIAN_POINT('Ctrl Pts',(8.07915007496071,-16.2251205863895,
-524.341911764706));
#159885=CARTESIAN_POINT('Ctrl Pts',(6.51968959134574,-16.8292587962898,
-525.836029411765));
#159886=CARTESIAN_POINT('Ctrl Pts',(4.96022910773078,-17.4333970061901,
-527.330147058823));
#159887=CARTESIAN_POINT('Ctrl Pts',(3.31631129755346,-17.7406985030951,
-528.824264705882));
#159888=CARTESIAN_POINT('Ctrl Pts',(1.67239348737615,-18.048,-530.318382352941));
#159889=CARTESIAN_POINT('Ctrl Pts',(0.,-18.048,-531.8125));
#159890=CARTESIAN_POINT('Ctrl Pts',(-1.67239348737615,-18.048,-533.306617647059));
#159891=CARTESIAN_POINT('Ctrl Pts',(-3.31631129755346,-17.7406985030951,
-534.800735294118));
#159892=CARTESIAN_POINT('Ctrl Pts',(-4.96022910773077,-17.4333970061901,
-536.294852941177));
#159893=CARTESIAN_POINT('Ctrl Pts',(-6.51968959134574,-16.8292587962898,
-537.788970588235));
#159894=CARTESIAN_POINT('Ctrl Pts',(-8.07915007496071,-16.2251205863895,
-539.283088235294));
#159895=CARTESIAN_POINT('Ctrl Pts',(-9.50104767561052,-15.3447188656481,
-540.777205882353));
#159896=CARTESIAN_POINT('Ctrl Pts',(-10.9229452762603,-14.4643171449067,
-542.271323529412));
#159897=CARTESIAN_POINT('Ctrl Pts',(-12.1588589765331,-13.3376329379985,
-543.765441176471));
#159898=CARTESIAN_POINT('Ctrl Pts',(-13.3947726768058,-12.2109487310903,
-545.259558823529));
#159899=CARTESIAN_POINT('Ctrl Pts',(-14.4026149179538,-10.8763499173728,
-546.753676470588));
#159900=CARTESIAN_POINT('Ctrl Pts',(-15.4104571591017,-9.54175110365538,
-548.247794117647));
#159901=CARTESIAN_POINT('Ctrl Pts',(-16.1559070823762,-8.04468584505497,
-549.741911764706));
#159902=CARTESIAN_POINT('Ctrl Pts',(-16.9013570056506,-6.54762058645456,
-551.236029411765));
#159903=CARTESIAN_POINT('Ctrl Pts',(-17.3590292079831,-4.93906964482095,
-552.730147058823));
#159904=CARTESIAN_POINT('Ctrl Pts',(-17.8167014103155,-3.33051870318735,
-554.224264705882));
#159905=CARTESIAN_POINT('Ctrl Pts',(-17.9710104137728,-1.66525935159368,
-555.718382352941));
#159906=CARTESIAN_POINT('Ctrl Pts',(-18.1253194172301,-1.10985572039171E-15,
-557.2125));
#159907=CARTESIAN_POINT('Ctrl Pts',(-17.9710104137728,1.66525935159367,
-558.706617647059));
#159908=CARTESIAN_POINT('Ctrl Pts',(-17.8167014103155,3.33051870318735,
-560.200735294118));
#159909=CARTESIAN_POINT('Ctrl Pts',(-17.3590292079831,4.93906964482096,
-561.694852941176));
#159910=CARTESIAN_POINT('Ctrl Pts',(-16.9013570056506,6.54762058645456,
-563.188970588235));
#159911=CARTESIAN_POINT('Ctrl Pts',(-16.1559070823762,8.04468584505497,
-564.683088235294));
#159912=CARTESIAN_POINT('Ctrl Pts',(-15.4104571591017,9.54175110365538,
-566.177205882353));
#159913=CARTESIAN_POINT('Ctrl Pts',(-14.4026149179538,10.8763499173728,
-567.671323529412));
#159914=CARTESIAN_POINT('Ctrl Pts',(-13.3947726768058,12.2109487310903,
-569.16544117647));
#159915=CARTESIAN_POINT('Ctrl Pts',(-12.1588589765331,13.3376329379985,
-570.659558823529));
#159916=CARTESIAN_POINT('Ctrl Pts',(-10.9229452762603,14.4643171449067,
-572.153676470588));
#159917=CARTESIAN_POINT('Ctrl Pts',(-9.50104767561052,15.3447188656481,
-573.647794117647));
#159918=CARTESIAN_POINT('Ctrl Pts',(-8.07915007496071,16.2251205863895,
-575.141911764706));
#159919=CARTESIAN_POINT('Ctrl Pts',(-6.51968959134574,16.8292587962898,
-576.636029411765));
#159920=CARTESIAN_POINT('Ctrl Pts',(-4.96022910773078,17.4333970061901,
-578.130147058824));
#159921=CARTESIAN_POINT('Ctrl Pts',(-3.31631129755346,17.7406985030951,
-579.624264705882));
#159922=CARTESIAN_POINT('Ctrl Pts',(-1.67239348737615,18.048,-581.118382352941));
#159923=CARTESIAN_POINT('Ctrl Pts',(-2.21024254310115E-15,18.048,-582.6125));
#159924=CARTESIAN_POINT('Ctrl Pts',(1.67239348737616,18.048,-584.106617647059));
#159925=CARTESIAN_POINT('Ctrl Pts',(3.31631129755346,17.7406985030951,-585.600735294117));
#159926=CARTESIAN_POINT('Ctrl Pts',(4.96022910773077,17.4333970061901,-587.094852941176));
#159927=CARTESIAN_POINT('Ctrl Pts',(6.51968959134575,16.8292587962898,-588.588970588235));
#159928=CARTESIAN_POINT('Ctrl Pts',(8.07915007496071,16.2251205863895,-590.083088235294));
#159929=CARTESIAN_POINT('Ctrl Pts',(9.50104767561053,15.3447188656481,-591.577205882353));
#159930=CARTESIAN_POINT('Ctrl Pts',(10.9229452762603,14.4643171449067,-593.071323529412));
#159931=CARTESIAN_POINT('Ctrl Pts',(12.1588589765331,13.3376329379985,-594.565441176471));
#159932=CARTESIAN_POINT('Ctrl Pts',(13.3947726768058,12.2109487310903,-596.05955882353));
#159933=CARTESIAN_POINT('Ctrl Pts',(14.4026149179538,10.8763499173728,-597.553676470588));
#159934=CARTESIAN_POINT('Ctrl Pts',(15.4104571591017,9.54175110365538,-599.047794117647));
#159935=CARTESIAN_POINT('Ctrl Pts',(16.1559070823762,8.04468584505496,-600.541911764706));
#159936=CARTESIAN_POINT('Ctrl Pts',(16.9013570056506,6.54762058645456,-602.036029411765));
#159937=CARTESIAN_POINT('Ctrl Pts',(17.3590292079831,4.93906964482096,-603.530147058823));
#159938=CARTESIAN_POINT('Ctrl Pts',(17.8167014103155,3.33051870318735,-605.024264705882));
#159939=CARTESIAN_POINT('Ctrl Pts',(17.9710104137728,1.66525935159367,-606.518382352941));
#159940=CARTESIAN_POINT('Ctrl Pts',(18.1253194172301,3.32956716117513E-15,
-608.0125));
#159941=CARTESIAN_POINT('Ctrl Pts',(17.9710104137728,-1.66525935159367,
-609.506617647059));
#159942=CARTESIAN_POINT('Ctrl Pts',(17.8167014103155,-3.33051870318736,
-611.000735294118));
#159943=CARTESIAN_POINT('Ctrl Pts',(17.3590292079831,-4.93906964482095,
-612.494852941176));
#159944=CARTESIAN_POINT('Ctrl Pts',(16.9013570056506,-6.54762058645456,
-613.988970588235));
#159945=CARTESIAN_POINT('Ctrl Pts',(16.1559070823762,-8.04468584505497,
-615.483088235294));
#159946=CARTESIAN_POINT('Ctrl Pts',(15.4104571591017,-9.54175110365538,
-616.977205882353));
#159947=CARTESIAN_POINT('Ctrl Pts',(14.4026149179538,-10.8763499173728,
-618.471323529412));
#159948=CARTESIAN_POINT('Ctrl Pts',(13.3947726768058,-12.2109487310903,
-619.96544117647));
#159949=CARTESIAN_POINT('Ctrl Pts',(12.1588589765331,-13.3376329379985,
-621.459558823529));
#159950=CARTESIAN_POINT('Ctrl Pts',(10.9229452762603,-14.4643171449067,
-622.953676470588));
#159951=CARTESIAN_POINT('Ctrl Pts',(9.50104767561053,-15.3447188656481,
-624.447794117647));
#159952=CARTESIAN_POINT('Ctrl Pts',(8.07915007496071,-16.2251205863895,
-625.941911764706));
#159953=CARTESIAN_POINT('Ctrl Pts',(6.51968959134574,-16.8292587962898,
-627.436029411764));
#159954=CARTESIAN_POINT('Ctrl Pts',(4.96022910773078,-17.4333970061901,
-628.930147058823));
#159955=CARTESIAN_POINT('Ctrl Pts',(3.31631129755346,-17.7406985030951,
-630.424264705882));
#159956=CARTESIAN_POINT('Ctrl Pts',(1.67239348737615,-18.048,-631.918382352941));
#159957=CARTESIAN_POINT('Ctrl Pts',(0.,-18.048,-633.4125));
#159958=CARTESIAN_POINT('Ctrl Pts',(-1.67239348737615,-18.048,-634.906617647059));
#159959=CARTESIAN_POINT('Ctrl Pts',(-3.31631129755346,-17.7406985030951,
-636.400735294118));
#159960=CARTESIAN_POINT('Ctrl Pts',(-4.96022910773077,-17.4333970061901,
-637.894852941177));
#159961=CARTESIAN_POINT('Ctrl Pts',(-6.51968959134574,-16.8292587962898,
-639.388970588235));
#159962=CARTESIAN_POINT('Ctrl Pts',(-8.07915007496071,-16.2251205863895,
-640.883088235294));
#159963=CARTESIAN_POINT('Ctrl Pts',(-9.50104767561052,-15.3447188656481,
-642.377205882353));
#159964=CARTESIAN_POINT('Ctrl Pts',(-10.9229452762603,-14.4643171449067,
-643.871323529412));
#159965=CARTESIAN_POINT('Ctrl Pts',(-12.1588589765331,-13.3376329379985,
-645.36544117647));
#159966=CARTESIAN_POINT('Ctrl Pts',(-13.3947726768058,-12.2109487310903,
-646.859558823529));
#159967=CARTESIAN_POINT('Ctrl Pts',(-14.4026149179538,-10.8763499173728,
-648.353676470588));
#159968=CARTESIAN_POINT('Ctrl Pts',(-15.4104571591017,-9.54175110365538,
-649.847794117647));
#159969=CARTESIAN_POINT('Ctrl Pts',(-16.1559070823762,-8.04468584505497,
-651.341911764706));
#159970=CARTESIAN_POINT('Ctrl Pts',(-16.9013570056506,-6.54762058645456,
-652.836029411765));
#159971=CARTESIAN_POINT('Ctrl Pts',(-17.3590292079831,-4.93906964482095,
-654.330147058824));
#159972=CARTESIAN_POINT('Ctrl Pts',(-17.8167014103155,-3.33051870318735,
-655.824264705882));
#159973=CARTESIAN_POINT('Ctrl Pts',(-17.9710104137728,-1.66525935159368,
-657.318382352941));
#159974=CARTESIAN_POINT('Ctrl Pts',(-18.1253194172301,-1.10985572039171E-15,
-658.8125));
#159975=CARTESIAN_POINT('Ctrl Pts',(-17.9710104137728,1.66525935159367,
-660.306617647059));
#159976=CARTESIAN_POINT('Ctrl Pts',(-17.8167014103155,3.33051870318735,
-661.800735294117));
#159977=CARTESIAN_POINT('Ctrl Pts',(-17.3590292079831,4.93906964482096,
-663.294852941176));
#159978=CARTESIAN_POINT('Ctrl Pts',(-16.9013570056506,6.54762058645456,
-664.788970588236));
#159979=CARTESIAN_POINT('Ctrl Pts',(-16.1559070823762,8.04468584505497,
-666.283088235294));
#159980=CARTESIAN_POINT('Ctrl Pts',(-15.4104571591017,9.54175110365538,
-667.777205882353));
#159981=CARTESIAN_POINT('Ctrl Pts',(-14.4026149179538,10.8763499173728,
-669.271323529412));
#159982=CARTESIAN_POINT('Ctrl Pts',(-13.3947726768058,12.2109487310903,
-670.765441176471));
#159983=CARTESIAN_POINT('Ctrl Pts',(-12.1588589765331,13.3376329379985,
-672.259558823529));
#159984=CARTESIAN_POINT('Ctrl Pts',(-10.9229452762603,14.4643171449067,
-673.753676470588));
#159985=CARTESIAN_POINT('Ctrl Pts',(-9.50104767561052,15.3447188656481,
-675.247794117647));
#159986=CARTESIAN_POINT('Ctrl Pts',(-8.07915007496071,16.2251205863895,
-676.741911764706));
#159987=CARTESIAN_POINT('Ctrl Pts',(-6.51968959134574,16.8292587962898,
-678.236029411765));
#159988=CARTESIAN_POINT('Ctrl Pts',(-4.96022910773078,17.4333970061901,
-679.730147058824));
#159989=CARTESIAN_POINT('Ctrl Pts',(-3.31631129755346,17.7406985030951,
-681.224264705883));
#159990=CARTESIAN_POINT('Ctrl Pts',(-1.67239348737615,18.048,-682.718382352941));
#159991=CARTESIAN_POINT('Ctrl Pts',(-2.21024254310115E-15,18.048,-684.2125));
#159992=CARTESIAN_POINT('Ctrl Pts',(1.67239348737616,18.048,-685.706617647059));
#159993=CARTESIAN_POINT('Ctrl Pts',(3.31631129755346,17.7406985030951,-687.200735294118));
#159994=CARTESIAN_POINT('Ctrl Pts',(4.96022910773077,17.4333970061901,-688.694852941176));
#159995=CARTESIAN_POINT('Ctrl Pts',(6.51968959134575,16.8292587962898,-690.188970588235));
#159996=CARTESIAN_POINT('Ctrl Pts',(8.07915007496071,16.2251205863895,-691.683088235294));
#159997=CARTESIAN_POINT('Ctrl Pts',(9.50104767561053,15.3447188656481,-693.177205882353));
#159998=CARTESIAN_POINT('Ctrl Pts',(10.9229452762603,14.4643171449067,-694.671323529412));
#159999=CARTESIAN_POINT('Ctrl Pts',(12.1588589765331,13.3376329379985,-696.165441176471));
#160000=CARTESIAN_POINT('Ctrl Pts',(13.3947726768058,12.2109487310903,-697.659558823529));
#160001=CARTESIAN_POINT('Ctrl Pts',(14.4026149179538,10.8763499173728,-699.153676470588));
#160002=CARTESIAN_POINT('Ctrl Pts',(15.4104571591017,9.54175110365538,-700.647794117647));
#160003=CARTESIAN_POINT('Ctrl Pts',(16.1559070823762,8.04468584505496,-702.141911764706));
#160004=CARTESIAN_POINT('Ctrl Pts',(16.9013570056506,6.54762058645456,-703.636029411765));
#160005=CARTESIAN_POINT('Ctrl Pts',(17.3590292079831,4.93906964482096,-705.130147058823));
#160006=CARTESIAN_POINT('Ctrl Pts',(17.8167014103155,3.33051870318735,-706.624264705882));
#160007=CARTESIAN_POINT('Ctrl Pts',(17.9710104137728,1.66525935159367,-708.118382352941));
#160008=CARTESIAN_POINT('Ctrl Pts',(18.1253194172301,3.32956716117513E-15,
-709.6125));
#160009=CARTESIAN_POINT('Ctrl Pts',(17.9710104137728,-1.66525935159367,
-711.106617647059));
#160010=CARTESIAN_POINT('Ctrl Pts',(17.8167014103155,-3.33051870318736,
-712.600735294118));
#160011=CARTESIAN_POINT('Ctrl Pts',(17.3590292079831,-4.93906964482095,
-714.094852941177));
#160012=CARTESIAN_POINT('Ctrl Pts',(16.9013570056506,-6.54762058645456,
-715.588970588235));
#160013=CARTESIAN_POINT('Ctrl Pts',(16.1559070823762,-8.04468584505497,
-717.083088235294));
#160014=CARTESIAN_POINT('Ctrl Pts',(15.4104571591017,-9.54175110365538,
-718.577205882353));
#160015=CARTESIAN_POINT('Ctrl Pts',(14.4026149179538,-10.8763499173728,
-720.071323529412));
#160016=CARTESIAN_POINT('Ctrl Pts',(13.3947726768058,-12.2109487310903,
-721.56544117647));
#160017=CARTESIAN_POINT('Ctrl Pts',(12.1588589765331,-13.3376329379985,
-723.059558823529));
#160018=CARTESIAN_POINT('Ctrl Pts',(10.9229452762603,-14.4643171449067,
-724.553676470588));
#160019=CARTESIAN_POINT('Ctrl Pts',(9.50104767561053,-15.3447188656481,
-726.047794117647));
#160020=CARTESIAN_POINT('Ctrl Pts',(8.07915007496071,-16.2251205863895,
-727.541911764706));
#160021=CARTESIAN_POINT('Ctrl Pts',(6.51968959134574,-16.8292587962898,
-729.036029411765));
#160022=CARTESIAN_POINT('Ctrl Pts',(4.96022910773078,-17.4333970061901,
-730.530147058824));
#160023=CARTESIAN_POINT('Ctrl Pts',(3.31631129755346,-17.7406985030951,
-732.024264705882));
#160024=CARTESIAN_POINT('Ctrl Pts',(1.67239348737615,-18.048,-733.518382352941));
#160025=CARTESIAN_POINT('Ctrl Pts',(0.,-18.048,-735.0125));
#160026=CARTESIAN_POINT('Ctrl Pts',(-1.67239348737615,-18.048,-736.506617647059));
#160027=CARTESIAN_POINT('Ctrl Pts',(-3.31631129755346,-17.7406985030951,
-738.000735294118));
#160028=CARTESIAN_POINT('Ctrl Pts',(-4.96022910773077,-17.4333970061901,
-739.494852941177));
#160029=CARTESIAN_POINT('Ctrl Pts',(-6.51968959134574,-16.8292587962898,
-740.988970588235));
#160030=CARTESIAN_POINT('Ctrl Pts',(-8.07915007496071,-16.2251205863895,
-742.483088235294));
#160031=CARTESIAN_POINT('Ctrl Pts',(-9.50104767561052,-15.3447188656481,
-743.977205882353));
#160032=CARTESIAN_POINT('Ctrl Pts',(-10.9229452762603,-14.4643171449067,
-745.471323529412));
#160033=CARTESIAN_POINT('Ctrl Pts',(-12.1588589765331,-13.3376329379985,
-746.96544117647));
#160034=CARTESIAN_POINT('Ctrl Pts',(-13.3947726768058,-12.2109487310903,
-748.459558823529));
#160035=CARTESIAN_POINT('Ctrl Pts',(-14.4026149179538,-10.8763499173728,
-749.953676470588));
#160036=CARTESIAN_POINT('Ctrl Pts',(-15.4104571591017,-9.54175110365538,
-751.447794117647));
#160037=CARTESIAN_POINT('Ctrl Pts',(-16.1559070823762,-8.04468584505497,
-752.941911764706));
#160038=CARTESIAN_POINT('Ctrl Pts',(-16.9013570056506,-6.54762058645456,
-754.436029411765));
#160039=CARTESIAN_POINT('Ctrl Pts',(-17.3590292079831,-4.93906964482095,
-755.930147058824));
#160040=CARTESIAN_POINT('Ctrl Pts',(-17.8167014103155,-3.33051870318735,
-757.424264705882));
#160041=CARTESIAN_POINT('Ctrl Pts',(-17.9710104137728,-1.66525935159368,
-758.918382352941));
#160042=CARTESIAN_POINT('Ctrl Pts',(-18.1253194172301,-1.10985572039171E-15,
-760.4125));
#160043=CARTESIAN_POINT('Ctrl Pts',(-17.9710104137728,1.66525935159367,
-761.906617647059));
#160044=CARTESIAN_POINT('Ctrl Pts',(-17.8167014103155,3.33051870318735,
-763.400735294118));
#160045=CARTESIAN_POINT('Ctrl Pts',(-17.3590292079831,4.93906964482096,
-764.894852941176));
#160046=CARTESIAN_POINT('Ctrl Pts',(-16.9013570056506,6.54762058645456,
-766.388970588235));
#160047=CARTESIAN_POINT('Ctrl Pts',(-16.1559070823762,8.04468584505497,
-767.883088235294));
#160048=CARTESIAN_POINT('Ctrl Pts',(-15.4104571591017,9.54175110365538,
-769.377205882353));
#160049=CARTESIAN_POINT('Ctrl Pts',(-14.4026149179538,10.8763499173728,
-770.871323529412));
#160050=CARTESIAN_POINT('Ctrl Pts',(-13.3947726768058,12.2109487310903,
-772.365441176471));
#160051=CARTESIAN_POINT('Ctrl Pts',(-12.1588589765331,13.3376329379985,
-773.85955882353));
#160052=CARTESIAN_POINT('Ctrl Pts',(-10.9229452762603,14.4643171449067,
-775.353676470589));
#160053=CARTESIAN_POINT('Ctrl Pts',(-9.50104767561052,15.3447188656481,
-776.847794117647));
#160054=CARTESIAN_POINT('Ctrl Pts',(-8.07915007496071,16.2251205863895,
-778.341911764706));
#160055=CARTESIAN_POINT('Ctrl Pts',(-6.51968959134574,16.8292587962898,
-779.836029411765));
#160056=CARTESIAN_POINT('Ctrl Pts',(-4.96022910773078,17.4333970061901,
-781.330147058823));
#160057=CARTESIAN_POINT('Ctrl Pts',(-3.31631129755346,17.7406985030951,
-782.824264705882));
#160058=CARTESIAN_POINT('Ctrl Pts',(-1.67239348737615,18.048,-784.318382352941));
#160059=CARTESIAN_POINT('Ctrl Pts',(-2.21024254310115E-15,18.048,-785.8125));
#160060=CARTESIAN_POINT('Ctrl Pts',(1.67239348737616,18.048,-787.306617647059));
#160061=CARTESIAN_POINT('Ctrl Pts',(3.31631129755346,17.7406985030951,-788.800735294118));
#160062=CARTESIAN_POINT('Ctrl Pts',(4.96022910773077,17.4333970061901,-790.294852941177));
#160063=CARTESIAN_POINT('Ctrl Pts',(6.51968959134575,16.8292587962898,-791.788970588235));
#160064=CARTESIAN_POINT('Ctrl Pts',(8.07915007496071,16.2251205863895,-793.283088235294));
#160065=CARTESIAN_POINT('Ctrl Pts',(9.50104767561053,15.3447188656481,-794.777205882353));
#160066=CARTESIAN_POINT('Ctrl Pts',(10.9229452762603,14.4643171449067,-796.271323529412));
#160067=CARTESIAN_POINT('Ctrl Pts',(12.1588589765331,13.3376329379985,-797.765441176471));
#160068=CARTESIAN_POINT('Ctrl Pts',(13.3947726768058,12.2109487310903,-799.259558823529));
#160069=CARTESIAN_POINT('Ctrl Pts',(14.4026149179538,10.8763499173728,-800.753676470588));
#160070=CARTESIAN_POINT('Ctrl Pts',(15.4104571591017,9.54175110365538,-802.247794117647));
#160071=CARTESIAN_POINT('Ctrl Pts',(16.1559070823762,8.04468584505496,-803.741911764706));
#160072=CARTESIAN_POINT('Ctrl Pts',(16.9013570056506,6.54762058645456,-805.236029411765));
#160073=CARTESIAN_POINT('Ctrl Pts',(17.3590292079831,4.93906964482096,-806.730147058823));
#160074=CARTESIAN_POINT('Ctrl Pts',(17.8167014103155,3.33051870318735,-808.224264705882));
#160075=CARTESIAN_POINT('Ctrl Pts',(17.9710104137728,1.66525935159367,-809.718382352941));
#160076=CARTESIAN_POINT('Ctrl Pts',(18.1253194172301,3.32956716117513E-15,
-811.2125));
#160077=CARTESIAN_POINT('Ctrl Pts',(17.9710104137728,-1.66525935159367,
-812.706617647059));
#160078=CARTESIAN_POINT('Ctrl Pts',(17.8167014103155,-3.33051870318736,
-814.200735294118));
#160079=CARTESIAN_POINT('Ctrl Pts',(17.3590292079831,-4.93906964482095,
-815.694852941177));
#160080=CARTESIAN_POINT('Ctrl Pts',(16.9013570056506,-6.54762058645456,
-817.188970588235));
#160081=CARTESIAN_POINT('Ctrl Pts',(16.1559070823762,-8.04468584505497,
-818.683088235294));
#160082=CARTESIAN_POINT('Ctrl Pts',(15.4104571591017,-9.54175110365538,
-820.177205882353));
#160083=CARTESIAN_POINT('Ctrl Pts',(14.4026149179538,-10.8763499173728,
-821.671323529412));
#160084=CARTESIAN_POINT('Ctrl Pts',(13.3947726768058,-12.2109487310903,
-823.16544117647));
#160085=CARTESIAN_POINT('Ctrl Pts',(12.1588589765331,-13.3376329379985,
-824.659558823529));
#160086=CARTESIAN_POINT('Ctrl Pts',(10.9229452762603,-14.4643171449067,
-826.153676470588));
#160087=CARTESIAN_POINT('Ctrl Pts',(9.50104767561053,-15.3447188656481,
-827.647794117647));
#160088=CARTESIAN_POINT('Ctrl Pts',(8.07915007496071,-16.2251205863895,
-829.141911764706));
#160089=CARTESIAN_POINT('Ctrl Pts',(6.51968959134574,-16.8292587962898,
-830.636029411765));
#160090=CARTESIAN_POINT('Ctrl Pts',(4.96022910773078,-17.4333970061901,
-832.130147058824));
#160091=CARTESIAN_POINT('Ctrl Pts',(3.31631129755346,-17.7406985030951,
-833.624264705883));
#160092=CARTESIAN_POINT('Ctrl Pts',(1.67239348737615,-18.048,-835.118382352941));
#160093=CARTESIAN_POINT('Ctrl Pts',(0.,-18.048,-836.6125));
#160094=CARTESIAN_POINT('Ctrl Pts',(-1.67239348737615,-18.048,-838.106617647059));
#160095=CARTESIAN_POINT('Ctrl Pts',(-3.31631129755346,-17.7406985030951,
-839.600735294118));
#160096=CARTESIAN_POINT('Ctrl Pts',(-4.96022910773077,-17.4333970061901,
-841.094852941176));
#160097=CARTESIAN_POINT('Ctrl Pts',(-6.51968959134574,-16.8292587962898,
-842.588970588235));
#160098=CARTESIAN_POINT('Ctrl Pts',(-8.07915007496071,-16.2251205863895,
-844.083088235294));
#160099=CARTESIAN_POINT('Ctrl Pts',(-9.50104767561052,-15.3447188656481,
-845.577205882353));
#160100=CARTESIAN_POINT('Ctrl Pts',(-10.9229452762603,-14.4643171449067,
-847.071323529412));
#160101=CARTESIAN_POINT('Ctrl Pts',(-12.1588589765331,-13.3376329379985,
-848.565441176471));
#160102=CARTESIAN_POINT('Ctrl Pts',(-13.3947726768058,-12.2109487310903,
-850.05955882353));
#160103=CARTESIAN_POINT('Ctrl Pts',(-14.4026149179538,-10.8763499173728,
-851.553676470588));
#160104=CARTESIAN_POINT('Ctrl Pts',(-15.4104571591017,-9.54175110365538,
-853.047794117647));
#160105=CARTESIAN_POINT('Ctrl Pts',(-16.1559070823762,-8.04468584505497,
-854.541911764706));
#160106=CARTESIAN_POINT('Ctrl Pts',(-16.9013570056506,-6.54762058645456,
-856.036029411765));
#160107=CARTESIAN_POINT('Ctrl Pts',(-17.3590292079831,-4.93906964482095,
-857.530147058824));
#160108=CARTESIAN_POINT('Ctrl Pts',(-17.8167014103155,-3.33051870318735,
-859.024264705882));
#160109=CARTESIAN_POINT('Ctrl Pts',(-17.9710104137728,-1.66525935159368,
-860.518382352941));
#160110=CARTESIAN_POINT('Ctrl Pts',(-18.1253194172301,-1.10985572039171E-15,
-862.0125));
#160111=CARTESIAN_POINT('Ctrl Pts',(-17.9710104137728,1.66525935159367,
-863.506617647059));
#160112=CARTESIAN_POINT('Ctrl Pts',(-17.8167014103155,3.33051870318735,
-865.000735294118));
#160113=CARTESIAN_POINT('Ctrl Pts',(-17.3590292079831,4.93906964482096,
-866.494852941176));
#160114=CARTESIAN_POINT('Ctrl Pts',(-16.9013570056506,6.54762058645456,
-867.988970588235));
#160115=CARTESIAN_POINT('Ctrl Pts',(-16.1559070823762,8.04468584505497,
-869.483088235294));
#160116=CARTESIAN_POINT('Ctrl Pts',(-15.4104571591017,9.54175110365538,
-870.977205882353));
#160117=CARTESIAN_POINT('Ctrl Pts',(-14.4026149179538,10.8763499173728,
-872.471323529412));
#160118=CARTESIAN_POINT('Ctrl Pts',(-13.3947726768058,12.2109487310903,
-873.965441176471));
#160119=CARTESIAN_POINT('Ctrl Pts',(-12.1588589765331,13.3376329379985,
-875.459558823529));
#160120=CARTESIAN_POINT('Ctrl Pts',(-10.9229452762603,14.4643171449067,
-876.953676470588));
#160121=CARTESIAN_POINT('Ctrl Pts',(-9.50104767561052,15.3447188656481,
-878.447794117647));
#160122=CARTESIAN_POINT('Ctrl Pts',(-8.07915007496071,16.2251205863895,
-879.941911764706));
#160123=CARTESIAN_POINT('Ctrl Pts',(-6.51968959134574,16.8292587962898,
-881.436029411765));
#160124=CARTESIAN_POINT('Ctrl Pts',(-4.96022910773078,17.4333970061901,
-882.930147058823));
#160125=CARTESIAN_POINT('Ctrl Pts',(-3.31631129755346,17.7406985030951,
-884.424264705882));
#160126=CARTESIAN_POINT('Ctrl Pts',(-1.67239348737615,18.048,-885.918382352941));
#160127=CARTESIAN_POINT('Ctrl Pts',(-2.21024254310115E-15,18.048,-887.4125));
#160128=CARTESIAN_POINT('Ctrl Pts',(1.67239348737616,18.048,-888.906617647059));
#160129=CARTESIAN_POINT('Ctrl Pts',(3.31631129755346,17.7406985030951,-890.400735294118));
#160130=CARTESIAN_POINT('Ctrl Pts',(4.96022910773077,17.4333970061901,-891.894852941177));
#160131=CARTESIAN_POINT('Ctrl Pts',(6.51968959134575,16.8292587962898,-893.388970588235));
#160132=CARTESIAN_POINT('Ctrl Pts',(8.07915007496071,16.2251205863895,-894.883088235295));
#160133=CARTESIAN_POINT('Ctrl Pts',(9.50104767561053,15.3447188656481,-896.377205882353));
#160134=CARTESIAN_POINT('Ctrl Pts',(10.9229452762603,14.4643171449067,-897.871323529412));
#160135=CARTESIAN_POINT('Ctrl Pts',(12.1588589765331,13.3376329379985,-899.36544117647));
#160136=CARTESIAN_POINT('Ctrl Pts',(13.3947726768058,12.2109487310903,-900.859558823529));
#160137=CARTESIAN_POINT('Ctrl Pts',(14.4026149179538,10.8763499173728,-902.353676470588));
#160138=CARTESIAN_POINT('Ctrl Pts',(15.4104571591017,9.54175110365538,-903.847794117647));
#160139=CARTESIAN_POINT('Ctrl Pts',(16.1559070823762,8.04468584505496,-905.341911764706));
#160140=CARTESIAN_POINT('Ctrl Pts',(16.9013570056506,6.54762058645456,-906.836029411765));
#160141=CARTESIAN_POINT('Ctrl Pts',(17.3590292079831,4.93906964482096,-908.330147058824));
#160142=CARTESIAN_POINT('Ctrl Pts',(17.8167014103155,3.33051870318735,-909.824264705883));
#160143=CARTESIAN_POINT('Ctrl Pts',(17.9710104137728,1.66525935159367,-911.318382352941));
#160144=CARTESIAN_POINT('Ctrl Pts',(18.1253194172301,3.32956716117513E-15,
-912.8125));
#160145=CARTESIAN_POINT('Ctrl Pts',(17.9710104137728,-1.66525935159367,
-914.306617647059));
#160146=CARTESIAN_POINT('Ctrl Pts',(17.8167014103155,-3.33051870318736,
-915.800735294118));
#160147=CARTESIAN_POINT('Ctrl Pts',(17.3590292079831,-4.93906964482095,
-917.294852941176));
#160148=CARTESIAN_POINT('Ctrl Pts',(16.9013570056506,-6.54762058645456,
-918.788970588235));
#160149=CARTESIAN_POINT('Ctrl Pts',(16.1559070823762,-8.04468584505497,
-920.283088235294));
#160150=CARTESIAN_POINT('Ctrl Pts',(15.4104571591017,-9.54175110365538,
-921.777205882353));
#160151=CARTESIAN_POINT('Ctrl Pts',(14.4026149179538,-10.8763499173728,
-923.271323529412));
#160152=CARTESIAN_POINT('Ctrl Pts',(13.3947726768058,-12.2109487310903,
-924.765441176471));
#160153=CARTESIAN_POINT('Ctrl Pts',(12.1588589765331,-13.3376329379985,
-926.259558823529));
#160154=CARTESIAN_POINT('Ctrl Pts',(10.9229452762603,-14.4643171449067,
-927.753676470588));
#160155=CARTESIAN_POINT('Ctrl Pts',(9.50104767561053,-15.3447188656481,
-929.247794117647));
#160156=CARTESIAN_POINT('Ctrl Pts',(8.07915007496071,-16.2251205863895,
-930.741911764706));
#160157=CARTESIAN_POINT('Ctrl Pts',(6.51968959134574,-16.8292587962898,
-932.236029411765));
#160158=CARTESIAN_POINT('Ctrl Pts',(4.96022910773078,-17.4333970061901,
-933.730147058824));
#160159=CARTESIAN_POINT('Ctrl Pts',(3.31631129755346,-17.7406985030951,
-935.224264705882));
#160160=CARTESIAN_POINT('Ctrl Pts',(1.67239348737615,-18.048,-936.718382352941));
#160161=CARTESIAN_POINT('Ctrl Pts',(0.,-18.048,-938.2125));
#160162=CARTESIAN_POINT('Ctrl Pts',(-1.67239348737615,-18.048,-939.706617647059));
#160163=CARTESIAN_POINT('Ctrl Pts',(-3.31631129755346,-17.7406985030951,
-941.200735294117));
#160164=CARTESIAN_POINT('Ctrl Pts',(-4.96022910773077,-17.4333970061901,
-942.694852941176));
#160165=CARTESIAN_POINT('Ctrl Pts',(-6.51968959134574,-16.8292587962898,
-944.188970588235));
#160166=CARTESIAN_POINT('Ctrl Pts',(-8.07915007496071,-16.2251205863895,
-945.683088235294));
#160167=CARTESIAN_POINT('Ctrl Pts',(-9.50104767561052,-15.3447188656481,
-947.177205882353));
#160168=CARTESIAN_POINT('Ctrl Pts',(-10.9229452762603,-14.4643171449067,
-948.671323529412));
#160169=CARTESIAN_POINT('Ctrl Pts',(-12.1588589765331,-13.3376329379985,
-950.165441176471));
#160170=CARTESIAN_POINT('Ctrl Pts',(-13.3947726768058,-12.2109487310903,
-951.65955882353));
#160171=CARTESIAN_POINT('Ctrl Pts',(-14.4026149179538,-10.8763499173728,
-953.153676470588));
#160172=CARTESIAN_POINT('Ctrl Pts',(-15.4104571591017,-9.54175110365538,
-954.647794117647));
#160173=CARTESIAN_POINT('Ctrl Pts',(-16.1559070823762,-8.04468584505497,
-956.141911764706));
#160174=CARTESIAN_POINT('Ctrl Pts',(-16.9013570056506,-6.54762058645456,
-957.636029411764));
#160175=CARTESIAN_POINT('Ctrl Pts',(-17.3590292079831,-4.93906964482095,
-959.130147058823));
#160176=CARTESIAN_POINT('Ctrl Pts',(-17.8167014103155,-3.33051870318735,
-960.624264705882));
#160177=CARTESIAN_POINT('Ctrl Pts',(-17.9710104137728,-1.66525935159368,
-962.118382352941));
#160178=CARTESIAN_POINT('Ctrl Pts',(-18.1253194172301,-1.10985572039171E-15,
-963.6125));
#160179=CARTESIAN_POINT('Ctrl Pts',(-17.9710104137728,1.66525935159367,
-965.106617647059));
#160180=CARTESIAN_POINT('Ctrl Pts',(-17.8167014103155,3.33051870318735,
-966.600735294118));
#160181=CARTESIAN_POINT('Ctrl Pts',(-17.3590292079831,4.93906964482096,
-968.094852941177));
#160182=CARTESIAN_POINT('Ctrl Pts',(-16.9013570056506,6.54762058645456,
-969.588970588235));
#160183=CARTESIAN_POINT('Ctrl Pts',(-16.1559070823762,8.04468584505497,
-971.083088235294));
#160184=CARTESIAN_POINT('Ctrl Pts',(-15.4104571591017,9.54175110365538,
-972.577205882353));
#160185=CARTESIAN_POINT('Ctrl Pts',(-14.4026149179538,10.8763499173728,
-974.071323529412));
#160186=CARTESIAN_POINT('Ctrl Pts',(-13.3947726768058,12.2109487310903,
-975.565441176471));
#160187=CARTESIAN_POINT('Ctrl Pts',(-12.1588589765331,13.3376329379985,
-977.059558823529));
#160188=CARTESIAN_POINT('Ctrl Pts',(-10.9229452762603,14.4643171449067,
-978.553676470588));
#160189=CARTESIAN_POINT('Ctrl Pts',(-9.50104767561052,15.3447188656481,
-980.047794117647));
#160190=CARTESIAN_POINT('Ctrl Pts',(-8.07915007496071,16.2251205863895,
-981.541911764706));
#160191=CARTESIAN_POINT('Ctrl Pts',(-6.51968959134574,16.8292587962898,
-983.036029411765));
#160192=CARTESIAN_POINT('Ctrl Pts',(-4.96022910773078,17.4333970061901,
-984.530147058824));
#160193=CARTESIAN_POINT('Ctrl Pts',(-3.31631129755346,17.7406985030951,
-986.024264705882));
#160194=CARTESIAN_POINT('Ctrl Pts',(-1.67239348737615,18.048,-987.518382352941));
#160195=CARTESIAN_POINT('Ctrl Pts',(-2.21024254310115E-15,18.048,-989.0125));
#160196=CARTESIAN_POINT('Ctrl Pts',(1.67239348737616,18.048,-990.506617647059));
#160197=CARTESIAN_POINT('Ctrl Pts',(3.31631129755346,17.7406985030951,-992.000735294118));
#160198=CARTESIAN_POINT('Ctrl Pts',(4.96022910773077,17.4333970061901,-993.494852941176));
#160199=CARTESIAN_POINT('Ctrl Pts',(6.51968959134575,16.8292587962898,-994.988970588235));
#160200=CARTESIAN_POINT('Ctrl Pts',(8.07915007496071,16.2251205863895,-996.483088235294));
#160201=CARTESIAN_POINT('Ctrl Pts',(9.50104767561053,15.3447188656481,-997.977205882353));
#160202=CARTESIAN_POINT('Ctrl Pts',(10.9229452762603,14.4643171449067,-999.471323529412));
#160203=CARTESIAN_POINT('Ctrl Pts',(12.1588589765331,13.3376329379985,-1000.96544117647));
#160204=CARTESIAN_POINT('Ctrl Pts',(13.3947726768058,12.2109487310903,-1002.45955882353));
#160205=CARTESIAN_POINT('Ctrl Pts',(14.4026149179538,10.8763499173728,-1003.95367647059));
#160206=CARTESIAN_POINT('Ctrl Pts',(15.4104571591017,9.54175110365538,-1005.44779411765));
#160207=CARTESIAN_POINT('Ctrl Pts',(16.1559070823762,8.04468584505496,-1006.94191176471));
#160208=CARTESIAN_POINT('Ctrl Pts',(16.9013570056506,6.54762058645456,-1008.43602941176));
#160209=CARTESIAN_POINT('Ctrl Pts',(17.3590292079831,4.93906964482096,-1009.93014705882));
#160210=CARTESIAN_POINT('Ctrl Pts',(17.8167014103155,3.33051870318735,-1011.42426470588));
#160211=CARTESIAN_POINT('Ctrl Pts',(17.9710104137728,1.66525935159367,-1012.91838235294));
#160212=CARTESIAN_POINT('Ctrl Pts',(18.1253194172301,3.32956716117513E-15,
-1014.4125));
#160213=CARTESIAN_POINT('Ctrl Pts',(17.9710104137728,-1.66525935159367,
-1015.90661764706));
#160214=CARTESIAN_POINT('Ctrl Pts',(17.8167014103155,-3.33051870318736,
-1017.40073529412));
#160215=CARTESIAN_POINT('Ctrl Pts',(17.3590292079831,-4.93906964482095,
-1018.89485294118));
#160216=CARTESIAN_POINT('Ctrl Pts',(16.9013570056506,-6.54762058645456,
-1020.38897058824));
#160217=CARTESIAN_POINT('Ctrl Pts',(16.1559070823762,-8.04468584505497,
-1021.88308823529));
#160218=CARTESIAN_POINT('Ctrl Pts',(15.4104571591017,-9.54175110365538,
-1023.37720588235));
#160219=CARTESIAN_POINT('Ctrl Pts',(14.4026149179538,-10.8763499173728,
-1024.87132352941));
#160220=CARTESIAN_POINT('Ctrl Pts',(13.3947726768058,-12.2109487310903,
-1026.36544117647));
#160221=CARTESIAN_POINT('Ctrl Pts',(12.1588589765331,-13.3376329379985,
-1027.85955882353));
#160222=CARTESIAN_POINT('Ctrl Pts',(10.9229452762603,-14.4643171449067,
-1029.35367647059));
#160223=CARTESIAN_POINT('Ctrl Pts',(9.50104767561053,-15.3447188656481,
-1030.84779411765));
#160224=CARTESIAN_POINT('Ctrl Pts',(8.07915007496071,-16.2251205863895,
-1032.34191176471));
#160225=CARTESIAN_POINT('Ctrl Pts',(6.51968959134574,-16.8292587962898,
-1033.83602941176));
#160226=CARTESIAN_POINT('Ctrl Pts',(4.96022910773078,-17.4333970061901,
-1035.33014705882));
#160227=CARTESIAN_POINT('Ctrl Pts',(3.31631129755346,-17.7406985030951,
-1036.82426470588));
#160228=CARTESIAN_POINT('Ctrl Pts',(1.67239348737615,-18.048,-1038.31838235294));
#160229=CARTESIAN_POINT('Ctrl Pts',(0.,-18.048,-1039.8125));
#160230=CARTESIAN_POINT('Ctrl Pts',(-1.67239348737615,-18.048,-1041.30661764706));
#160231=CARTESIAN_POINT('Ctrl Pts',(-3.31631129755346,-17.7406985030951,
-1042.80073529412));
#160232=CARTESIAN_POINT('Ctrl Pts',(-4.96022910773077,-17.4333970061901,
-1044.29485294118));
#160233=CARTESIAN_POINT('Ctrl Pts',(-6.51968959134574,-16.8292587962898,
-1045.78897058824));
#160234=CARTESIAN_POINT('Ctrl Pts',(-8.07915007496071,-16.2251205863895,
-1047.28308823529));
#160235=CARTESIAN_POINT('Ctrl Pts',(-9.50104767561052,-15.3447188656481,
-1048.77720588235));
#160236=CARTESIAN_POINT('Ctrl Pts',(-10.9229452762603,-14.4643171449067,
-1050.27132352941));
#160237=CARTESIAN_POINT('Ctrl Pts',(-12.1588589765331,-13.3376329379985,
-1051.76544117647));
#160238=CARTESIAN_POINT('Ctrl Pts',(-13.3947726768058,-12.2109487310903,
-1053.25955882353));
#160239=CARTESIAN_POINT('Ctrl Pts',(-14.4026149179538,-10.8763499173728,
-1054.75367647059));
#160240=CARTESIAN_POINT('Ctrl Pts',(-15.4104571591017,-9.54175110365538,
-1056.24779411765));
#160241=CARTESIAN_POINT('Ctrl Pts',(-16.1559070823762,-8.04468584505497,
-1057.74191176471));
#160242=CARTESIAN_POINT('Ctrl Pts',(-16.9013570056506,-6.54762058645456,
-1059.23602941177));
#160243=CARTESIAN_POINT('Ctrl Pts',(-17.3590292079831,-4.93906964482095,
-1060.73014705882));
#160244=CARTESIAN_POINT('Ctrl Pts',(-17.8167014103155,-3.33051870318735,
-1062.22426470588));
#160245=CARTESIAN_POINT('Ctrl Pts',(-17.9710104137728,-1.66525935159368,
-1063.71838235294));
#160246=CARTESIAN_POINT('Ctrl Pts',(-18.1253194172301,-1.10985572039171E-15,
-1065.2125));
#160247=CARTESIAN_POINT('Ctrl Pts',(-17.9710104137728,1.66525935159367,
-1066.70661764706));
#160248=CARTESIAN_POINT('Ctrl Pts',(-17.8167014103155,3.33051870318735,
-1068.20073529412));
#160249=CARTESIAN_POINT('Ctrl Pts',(-17.3590292079831,4.93906964482096,
-1069.69485294118));
#160250=CARTESIAN_POINT('Ctrl Pts',(-16.9013570056506,6.54762058645456,
-1071.18897058824));
#160251=CARTESIAN_POINT('Ctrl Pts',(-16.1559070823762,8.04468584505497,
-1072.68308823529));
#160252=CARTESIAN_POINT('Ctrl Pts',(-15.4104571591017,9.54175110365538,
-1074.17720588235));
#160253=CARTESIAN_POINT('Ctrl Pts',(-14.4026149179538,10.8763499173728,
-1075.67132352941));
#160254=CARTESIAN_POINT('Ctrl Pts',(-13.3947726768058,12.2109487310903,
-1077.16544117647));
#160255=CARTESIAN_POINT('Ctrl Pts',(-12.1588589765331,13.3376329379985,
-1078.65955882353));
#160256=CARTESIAN_POINT('Ctrl Pts',(-10.9229452762603,14.4643171449067,
-1080.15367647059));
#160257=CARTESIAN_POINT('Ctrl Pts',(-9.50104767561052,15.3447188656481,
-1081.64779411765));
#160258=CARTESIAN_POINT('Ctrl Pts',(-8.07915007496071,16.2251205863895,
-1083.14191176471));
#160259=CARTESIAN_POINT('Ctrl Pts',(-6.51968959134574,16.8292587962898,
-1084.63602941176));
#160260=CARTESIAN_POINT('Ctrl Pts',(-4.96022910773078,17.4333970061901,
-1086.13014705882));
#160261=CARTESIAN_POINT('Ctrl Pts',(-3.31631129755346,17.7406985030951,
-1087.62426470588));
#160262=CARTESIAN_POINT('Ctrl Pts',(-1.67239348737615,18.048,-1089.11838235294));
#160263=CARTESIAN_POINT('Ctrl Pts',(-2.21024254310115E-15,18.048,-1090.6125));
#160264=CARTESIAN_POINT('Ctrl Pts',(1.67239348737616,18.048,-1092.10661764706));
#160265=CARTESIAN_POINT('Ctrl Pts',(3.31631129755346,17.7406985030951,-1093.60073529412));
#160266=CARTESIAN_POINT('Ctrl Pts',(4.96022910773077,17.4333970061901,-1095.09485294118));
#160267=CARTESIAN_POINT('Ctrl Pts',(6.51968959134575,16.8292587962898,-1096.58897058824));
#160268=CARTESIAN_POINT('Ctrl Pts',(8.07915007496071,16.2251205863895,-1098.08308823529));
#160269=CARTESIAN_POINT('Ctrl Pts',(9.50104767561053,15.3447188656481,-1099.57720588235));
#160270=CARTESIAN_POINT('Ctrl Pts',(10.9229452762603,14.4643171449067,-1101.07132352941));
#160271=CARTESIAN_POINT('Ctrl Pts',(12.1588589765331,13.3376329379985,-1102.56544117647));
#160272=CARTESIAN_POINT('Ctrl Pts',(13.3947726768058,12.2109487310903,-1104.05955882353));
#160273=CARTESIAN_POINT('Ctrl Pts',(14.4026149179538,10.8763499173728,-1105.55367647059));
#160274=CARTESIAN_POINT('Ctrl Pts',(15.4104571591017,9.54175110365538,-1107.04779411765));
#160275=CARTESIAN_POINT('Ctrl Pts',(16.1559070823762,8.04468584505496,-1108.54191176471));
#160276=CARTESIAN_POINT('Ctrl Pts',(16.9013570056506,6.54762058645456,-1110.03602941176));
#160277=CARTESIAN_POINT('Ctrl Pts',(17.3590292079831,4.93906964482096,-1111.53014705882));
#160278=CARTESIAN_POINT('Ctrl Pts',(17.8167014103155,3.33051870318735,-1113.02426470588));
#160279=CARTESIAN_POINT('Ctrl Pts',(17.9710104137728,1.66525935159367,-1114.51838235294));
#160280=CARTESIAN_POINT('Ctrl Pts',(18.1253194172301,3.32956716117513E-15,
-1116.0125));
#160281=CARTESIAN_POINT('Ctrl Pts',(17.9710104137728,-1.66525935159367,
-1117.50661764706));
#160282=CARTESIAN_POINT('Ctrl Pts',(17.8167014103155,-3.33051870318736,
-1119.00073529412));
#160283=CARTESIAN_POINT('Ctrl Pts',(17.3590292079831,-4.93906964482095,
-1120.49485294118));
#160284=CARTESIAN_POINT('Ctrl Pts',(16.9013570056506,-6.54762058645456,
-1121.98897058824));
#160285=CARTESIAN_POINT('Ctrl Pts',(16.1559070823762,-8.04468584505497,
-1123.48308823529));
#160286=CARTESIAN_POINT('Ctrl Pts',(15.4104571591017,-9.54175110365538,
-1124.97720588235));
#160287=CARTESIAN_POINT('Ctrl Pts',(14.4026149179538,-10.8763499173728,
-1126.47132352941));
#160288=CARTESIAN_POINT('Ctrl Pts',(13.3947726768058,-12.2109487310903,
-1127.96544117647));
#160289=CARTESIAN_POINT('Ctrl Pts',(12.1588589765331,-13.3376329379985,
-1129.45955882353));
#160290=CARTESIAN_POINT('Ctrl Pts',(10.9229452762603,-14.4643171449067,
-1130.95367647059));
#160291=CARTESIAN_POINT('Ctrl Pts',(9.50104767561053,-15.3447188656481,
-1132.44779411765));
#160292=CARTESIAN_POINT('Ctrl Pts',(8.07915007496071,-16.2251205863895,
-1133.94191176471));
#160293=CARTESIAN_POINT('Ctrl Pts',(6.51968959134574,-16.8292587962898,
-1135.43602941176));
#160294=CARTESIAN_POINT('Ctrl Pts',(4.96022910773078,-17.4333970061901,
-1136.93014705882));
#160295=CARTESIAN_POINT('Ctrl Pts',(3.31631129755346,-17.7406985030951,
-1138.42426470588));
#160296=CARTESIAN_POINT('Ctrl Pts',(1.67239348737615,-18.048,-1139.91838235294));
#160297=CARTESIAN_POINT('Ctrl Pts',(0.,-18.048,-1141.4125));
#160298=CARTESIAN_POINT('Ctrl Pts',(-1.67239348737615,-18.048,-1142.90661764706));
#160299=CARTESIAN_POINT('Ctrl Pts',(-3.31631129755346,-17.7406985030951,
-1144.40073529412));
#160300=CARTESIAN_POINT('Ctrl Pts',(-4.96022910773077,-17.4333970061901,
-1145.89485294118));
#160301=CARTESIAN_POINT('Ctrl Pts',(-6.51968959134574,-16.8292587962898,
-1147.38897058824));
#160302=CARTESIAN_POINT('Ctrl Pts',(-8.07915007496071,-16.2251205863895,
-1148.88308823529));
#160303=CARTESIAN_POINT('Ctrl Pts',(-9.50104767561052,-15.3447188656481,
-1150.37720588235));
#160304=CARTESIAN_POINT('Ctrl Pts',(-10.9229452762603,-14.4643171449067,
-1151.87132352941));
#160305=CARTESIAN_POINT('Ctrl Pts',(-12.1588589765331,-13.3376329379985,
-1153.36544117647));
#160306=CARTESIAN_POINT('Ctrl Pts',(-13.3947726768058,-12.2109487310903,
-1154.85955882353));
#160307=CARTESIAN_POINT('Ctrl Pts',(-14.4026149179538,-10.8763499173728,
-1156.35367647059));
#160308=CARTESIAN_POINT('Ctrl Pts',(-15.4104571591017,-9.54175110365538,
-1157.84779411765));
#160309=CARTESIAN_POINT('Ctrl Pts',(-16.1559070823762,-8.04468584505497,
-1159.34191176471));
#160310=CARTESIAN_POINT('Ctrl Pts',(-16.9013570056506,-6.54762058645456,
-1160.83602941176));
#160311=CARTESIAN_POINT('Ctrl Pts',(-17.3590292079831,-4.93906964482095,
-1162.33014705882));
#160312=CARTESIAN_POINT('Ctrl Pts',(-17.8167014103155,-3.33051870318735,
-1163.82426470588));
#160313=CARTESIAN_POINT('Ctrl Pts',(-17.9710104137728,-1.66525935159368,
-1165.31838235294));
#160314=CARTESIAN_POINT('Ctrl Pts',(-18.1253194172301,-1.10985572039171E-15,
-1166.8125));
#160315=CARTESIAN_POINT('Ctrl Pts',(-17.9710104137728,1.66525935159367,
-1168.30661764706));
#160316=CARTESIAN_POINT('Ctrl Pts',(-17.8167014103155,3.33051870318735,
-1169.80073529412));
#160317=CARTESIAN_POINT('Ctrl Pts',(-17.3590292079831,4.93906964482096,
-1171.29485294118));
#160318=CARTESIAN_POINT('Ctrl Pts',(-16.9013570056506,6.54762058645456,
-1172.78897058824));
#160319=CARTESIAN_POINT('Ctrl Pts',(-16.1559070823762,8.04468584505497,
-1174.28308823529));
#160320=CARTESIAN_POINT('Ctrl Pts',(-15.4104571591017,9.54175110365538,
-1175.77720588235));
#160321=CARTESIAN_POINT('Ctrl Pts',(-14.4026149179538,10.8763499173728,
-1177.27132352941));
#160322=CARTESIAN_POINT('Ctrl Pts',(-13.3947726768058,12.2109487310903,
-1178.76544117647));
#160323=CARTESIAN_POINT('Ctrl Pts',(-12.1588589765331,13.3376329379985,
-1180.25955882353));
#160324=CARTESIAN_POINT('Ctrl Pts',(-10.9229452762603,14.4643171449067,
-1181.75367647059));
#160325=CARTESIAN_POINT('Ctrl Pts',(-9.50104767561052,15.3447188656481,
-1183.24779411765));
#160326=CARTESIAN_POINT('Ctrl Pts',(-8.07915007496071,16.2251205863895,
-1184.74191176471));
#160327=CARTESIAN_POINT('Ctrl Pts',(-6.51968959134574,16.8292587962898,
-1186.23602941176));
#160328=CARTESIAN_POINT('Ctrl Pts',(-4.96022910773078,17.4333970061901,
-1187.73014705882));
#160329=CARTESIAN_POINT('Ctrl Pts',(-3.31631129755346,17.7406985030951,
-1189.22426470588));
#160330=CARTESIAN_POINT('Ctrl Pts',(-1.67239348737615,18.048,-1190.71838235294));
#160331=CARTESIAN_POINT('Ctrl Pts',(-2.21024254310115E-15,18.048,-1192.2125));
#160332=CARTESIAN_POINT('Ctrl Pts',(1.67239348737616,18.048,-1193.70661764706));
#160333=CARTESIAN_POINT('Ctrl Pts',(3.31631129755346,17.7406985030951,-1195.20073529412));
#160334=CARTESIAN_POINT('Ctrl Pts',(4.96022910773077,17.4333970061901,-1196.69485294118));
#160335=CARTESIAN_POINT('Ctrl Pts',(6.51968959134575,16.8292587962898,-1198.18897058824));
#160336=CARTESIAN_POINT('Ctrl Pts',(8.07915007496071,16.2251205863895,-1199.68308823529));
#160337=CARTESIAN_POINT('Ctrl Pts',(9.50104767561053,15.3447188656481,-1201.17720588235));
#160338=CARTESIAN_POINT('Ctrl Pts',(10.9229452762603,14.4643171449067,-1202.67132352941));
#160339=CARTESIAN_POINT('Ctrl Pts',(12.1588589765331,13.3376329379985,-1204.16544117647));
#160340=CARTESIAN_POINT('Ctrl Pts',(13.3947726768058,12.2109487310903,-1205.65955882353));
#160341=CARTESIAN_POINT('Ctrl Pts',(14.4026149179538,10.8763499173728,-1207.15367647059));
#160342=CARTESIAN_POINT('Ctrl Pts',(15.4104571591017,9.54175110365538,-1208.64779411765));
#160343=CARTESIAN_POINT('Ctrl Pts',(16.1559070823762,8.04468584505496,-1210.14191176471));
#160344=CARTESIAN_POINT('Ctrl Pts',(16.9013570056506,6.54762058645456,-1211.63602941176));
#160345=CARTESIAN_POINT('Ctrl Pts',(17.3590292079831,4.93906964482096,-1213.13014705882));
#160346=CARTESIAN_POINT('Ctrl Pts',(17.8167014103155,3.33051870318735,-1214.62426470588));
#160347=CARTESIAN_POINT('Ctrl Pts',(17.9710104137728,1.66525935159367,-1216.11838235294));
#160348=CARTESIAN_POINT('Ctrl Pts',(18.1253194172301,3.32956716117513E-15,
-1217.6125));
#160349=CARTESIAN_POINT('Ctrl Pts',(17.9710104137728,-1.66525935159367,
-1219.10661764706));
#160350=CARTESIAN_POINT('Ctrl Pts',(17.8167014103155,-3.33051870318736,
-1220.60073529412));
#160351=CARTESIAN_POINT('Ctrl Pts',(17.3590292079831,-4.93906964482095,
-1222.09485294118));
#160352=CARTESIAN_POINT('Ctrl Pts',(16.9013570056506,-6.54762058645456,
-1223.58897058824));
#160353=CARTESIAN_POINT('Ctrl Pts',(16.1559070823762,-8.04468584505497,
-1225.08308823529));
#160354=CARTESIAN_POINT('Ctrl Pts',(15.4104571591017,-9.54175110365538,
-1226.57720588235));
#160355=CARTESIAN_POINT('Ctrl Pts',(14.4026149179538,-10.8763499173728,
-1228.07132352941));
#160356=CARTESIAN_POINT('Ctrl Pts',(13.3947726768058,-12.2109487310903,
-1229.56544117647));
#160357=CARTESIAN_POINT('Ctrl Pts',(12.1588589765331,-13.3376329379985,
-1231.05955882353));
#160358=CARTESIAN_POINT('Ctrl Pts',(10.9229452762603,-14.4643171449067,
-1232.55367647059));
#160359=CARTESIAN_POINT('Ctrl Pts',(9.50104767561053,-15.3447188656481,
-1234.04779411765));
#160360=CARTESIAN_POINT('Ctrl Pts',(8.07915007496071,-16.2251205863895,
-1235.54191176471));
#160361=CARTESIAN_POINT('Ctrl Pts',(6.51968959134574,-16.8292587962898,
-1237.03602941176));
#160362=CARTESIAN_POINT('Ctrl Pts',(4.96022910773078,-17.4333970061901,
-1238.53014705882));
#160363=CARTESIAN_POINT('Ctrl Pts',(3.31631129755346,-17.7406985030951,
-1240.02426470588));
#160364=CARTESIAN_POINT('Ctrl Pts',(1.67239348737615,-18.048,-1241.51838235294));
#160365=CARTESIAN_POINT('Ctrl Pts',(0.,-18.048,-1243.0125));
#160366=CARTESIAN_POINT('Ctrl Pts',(-1.67239348737615,-18.048,-1244.50661764706));
#160367=CARTESIAN_POINT('Ctrl Pts',(-3.31631129755346,-17.7406985030951,
-1246.00073529412));
#160368=CARTESIAN_POINT('Ctrl Pts',(-4.96022910773077,-17.4333970061901,
-1247.49485294118));
#160369=CARTESIAN_POINT('Ctrl Pts',(-6.51968959134574,-16.8292587962898,
-1248.98897058824));
#160370=CARTESIAN_POINT('Ctrl Pts',(-8.07915007496071,-16.2251205863895,
-1250.48308823529));
#160371=CARTESIAN_POINT('Ctrl Pts',(-9.50104767561052,-15.3447188656481,
-1251.97720588235));
#160372=CARTESIAN_POINT('Ctrl Pts',(-10.9229452762603,-14.4643171449067,
-1253.47132352941));
#160373=CARTESIAN_POINT('Ctrl Pts',(-12.1588589765331,-13.3376329379985,
-1254.96544117647));
#160374=CARTESIAN_POINT('Ctrl Pts',(-13.3947726768058,-12.2109487310903,
-1256.45955882353));
#160375=CARTESIAN_POINT('Ctrl Pts',(-14.4026149179538,-10.8763499173728,
-1257.95367647059));
#160376=CARTESIAN_POINT('Ctrl Pts',(-15.4104571591017,-9.54175110365538,
-1259.44779411765));
#160377=CARTESIAN_POINT('Ctrl Pts',(-16.1559070823762,-8.04468584505497,
-1260.94191176471));
#160378=CARTESIAN_POINT('Ctrl Pts',(-16.9013570056506,-6.54762058645456,
-1262.43602941176));
#160379=CARTESIAN_POINT('Ctrl Pts',(-17.3590292079831,-4.93906964482095,
-1263.93014705882));
#160380=CARTESIAN_POINT('Ctrl Pts',(-17.8167014103155,-3.33051870318735,
-1265.42426470588));
#160381=CARTESIAN_POINT('Ctrl Pts',(-17.9710104137728,-1.66525935159368,
-1266.91838235294));
#160382=CARTESIAN_POINT('Ctrl Pts',(-18.1253194172301,-1.10985572039171E-15,
-1268.4125));
#160383=CARTESIAN_POINT('Ctrl Pts',(-17.9710104137728,1.66525935159367,
-1269.90661764706));
#160384=CARTESIAN_POINT('Ctrl Pts',(-17.8167014103155,3.33051870318735,
-1271.40073529412));
#160385=CARTESIAN_POINT('Ctrl Pts',(-17.3590292079831,4.93906964482096,
-1272.89485294118));
#160386=CARTESIAN_POINT('Ctrl Pts',(-16.9013570056506,6.54762058645456,
-1274.38897058824));
#160387=CARTESIAN_POINT('Ctrl Pts',(-16.1559070823762,8.04468584505497,
-1275.88308823529));
#160388=CARTESIAN_POINT('Ctrl Pts',(-15.4104571591017,9.54175110365538,
-1277.37720588235));
#160389=CARTESIAN_POINT('Ctrl Pts',(-14.4026149179538,10.8763499173728,
-1278.87132352941));
#160390=CARTESIAN_POINT('Ctrl Pts',(-13.3947726768058,12.2109487310903,
-1280.36544117647));
#160391=CARTESIAN_POINT('Ctrl Pts',(-12.1588589765331,13.3376329379985,
-1281.85955882353));
#160392=CARTESIAN_POINT('Ctrl Pts',(-10.9229452762603,14.4643171449067,
-1283.35367647059));
#160393=CARTESIAN_POINT('Ctrl Pts',(-9.50104767561052,15.3447188656481,
-1284.84779411765));
#160394=CARTESIAN_POINT('Ctrl Pts',(-8.07915007496071,16.2251205863895,
-1286.34191176471));
#160395=CARTESIAN_POINT('Ctrl Pts',(-6.51968959134574,16.8292587962898,
-1287.83602941176));
#160396=CARTESIAN_POINT('Ctrl Pts',(-4.96022910773078,17.4333970061901,
-1289.33014705882));
#160397=CARTESIAN_POINT('Ctrl Pts',(-3.31631129755346,17.7406985030951,
-1290.82426470588));
#160398=CARTESIAN_POINT('Ctrl Pts',(-1.67239348737615,18.048,-1292.31838235294));
#160399=CARTESIAN_POINT('Ctrl Pts',(-2.21024254310115E-15,18.048,-1293.8125));
#160400=CARTESIAN_POINT('Ctrl Pts',(1.67239348737616,18.048,-1295.30661764706));
#160401=CARTESIAN_POINT('Ctrl Pts',(3.31631129755346,17.7406985030951,-1296.80073529412));
#160402=CARTESIAN_POINT('Ctrl Pts',(4.96022910773077,17.4333970061901,-1298.29485294118));
#160403=CARTESIAN_POINT('Ctrl Pts',(6.51968959134575,16.8292587962898,-1299.78897058824));
#160404=CARTESIAN_POINT('Ctrl Pts',(8.07915007496071,16.2251205863895,-1301.28308823529));
#160405=CARTESIAN_POINT('Ctrl Pts',(9.50104767561053,15.3447188656481,-1302.77720588235));
#160406=CARTESIAN_POINT('Ctrl Pts',(10.9229452762603,14.4643171449067,-1304.27132352941));
#160407=CARTESIAN_POINT('Ctrl Pts',(12.1588589765331,13.3376329379985,-1305.76544117647));
#160408=CARTESIAN_POINT('Ctrl Pts',(13.3947726768058,12.2109487310903,-1307.25955882353));
#160409=CARTESIAN_POINT('Ctrl Pts',(14.4026149179538,10.8763499173728,-1308.75367647059));
#160410=CARTESIAN_POINT('Ctrl Pts',(15.4104571591017,9.54175110365538,-1310.24779411765));
#160411=CARTESIAN_POINT('Ctrl Pts',(16.1559070823762,8.04468584505496,-1311.74191176471));
#160412=CARTESIAN_POINT('Ctrl Pts',(16.9013570056506,6.54762058645456,-1313.23602941176));
#160413=CARTESIAN_POINT('Ctrl Pts',(17.3590292079831,4.93906964482096,-1314.73014705882));
#160414=CARTESIAN_POINT('Ctrl Pts',(17.8167014103155,3.33051870318735,-1316.22426470588));
#160415=CARTESIAN_POINT('Ctrl Pts',(17.9710104137728,1.66525935159367,-1317.71838235294));
#160416=CARTESIAN_POINT('Ctrl Pts',(18.1253194172301,3.32956716117513E-15,
-1319.2125));
#160417=CARTESIAN_POINT('Ctrl Pts',(17.9710104137728,-1.66525935159367,
-1320.70661764706));
#160418=CARTESIAN_POINT('Ctrl Pts',(17.8167014103155,-3.33051870318736,
-1322.20073529412));
#160419=CARTESIAN_POINT('Ctrl Pts',(17.3590292079831,-4.93906964482095,
-1323.69485294118));
#160420=CARTESIAN_POINT('Ctrl Pts',(16.9013570056506,-6.54762058645456,
-1325.18897058824));
#160421=CARTESIAN_POINT('Ctrl Pts',(16.1559070823762,-8.04468584505497,
-1326.68308823529));
#160422=CARTESIAN_POINT('Ctrl Pts',(15.4104571591017,-9.54175110365538,
-1328.17720588235));
#160423=CARTESIAN_POINT('Ctrl Pts',(14.4026149179538,-10.8763499173728,
-1329.67132352941));
#160424=CARTESIAN_POINT('Ctrl Pts',(13.3947726768058,-12.2109487310903,
-1331.16544117647));
#160425=CARTESIAN_POINT('Ctrl Pts',(12.1588589765331,-13.3376329379985,
-1332.65955882353));
#160426=CARTESIAN_POINT('Ctrl Pts',(10.9229452762603,-14.4643171449067,
-1334.15367647059));
#160427=CARTESIAN_POINT('Ctrl Pts',(9.50104767561053,-15.3447188656481,
-1335.64779411765));
#160428=CARTESIAN_POINT('Ctrl Pts',(8.07915007496071,-16.2251205863895,
-1337.14191176471));
#160429=CARTESIAN_POINT('Ctrl Pts',(6.51968959134574,-16.8292587962898,
-1338.63602941176));
#160430=CARTESIAN_POINT('Ctrl Pts',(4.96022910773078,-17.4333970061901,
-1340.13014705882));
#160431=CARTESIAN_POINT('Ctrl Pts',(3.31631129755346,-17.7406985030951,
-1341.62426470588));
#160432=CARTESIAN_POINT('Ctrl Pts',(1.67239348737615,-18.048,-1343.11838235294));
#160433=CARTESIAN_POINT('Ctrl Pts',(0.,-18.048,-1344.6125));
#160434=CARTESIAN_POINT('Ctrl Pts',(-1.67239348737615,-18.048,-1346.10661764706));
#160435=CARTESIAN_POINT('Ctrl Pts',(-3.31631129755346,-17.7406985030951,
-1347.60073529412));
#160436=CARTESIAN_POINT('Ctrl Pts',(-4.96022910773077,-17.4333970061901,
-1349.09485294118));
#160437=CARTESIAN_POINT('Ctrl Pts',(-6.51968959134574,-16.8292587962898,
-1350.58897058824));
#160438=CARTESIAN_POINT('Ctrl Pts',(-8.07915007496071,-16.2251205863895,
-1352.08308823529));
#160439=CARTESIAN_POINT('Ctrl Pts',(-9.50104767561052,-15.3447188656481,
-1353.57720588235));
#160440=CARTESIAN_POINT('Ctrl Pts',(-10.9229452762603,-14.4643171449067,
-1355.07132352941));
#160441=CARTESIAN_POINT('Ctrl Pts',(-12.1588589765331,-13.3376329379985,
-1356.56544117647));
#160442=CARTESIAN_POINT('Ctrl Pts',(-13.3947726768058,-12.2109487310903,
-1358.05955882353));
#160443=CARTESIAN_POINT('Ctrl Pts',(-14.4026149179538,-10.8763499173728,
-1359.55367647059));
#160444=CARTESIAN_POINT('Ctrl Pts',(-15.4104571591017,-9.54175110365538,
-1361.04779411765));
#160445=CARTESIAN_POINT('Ctrl Pts',(-16.1559070823762,-8.04468584505497,
-1362.54191176471));
#160446=CARTESIAN_POINT('Ctrl Pts',(-16.9013570056506,-6.54762058645456,
-1364.03602941176));
#160447=CARTESIAN_POINT('Ctrl Pts',(-17.3590292079831,-4.93906964482095,
-1365.53014705882));
#160448=CARTESIAN_POINT('Ctrl Pts',(-17.8167014103155,-3.33051870318735,
-1367.02426470588));
#160449=CARTESIAN_POINT('Ctrl Pts',(-17.9710104137728,-1.66525935159368,
-1368.51838235294));
#160450=CARTESIAN_POINT('Ctrl Pts',(-18.1253194172301,-1.10985572039171E-15,
-1370.0125));
#160451=CARTESIAN_POINT('Ctrl Pts',(-17.9710104137728,1.66525935159367,
-1371.50661764706));
#160452=CARTESIAN_POINT('Ctrl Pts',(-17.8167014103155,3.33051870318735,
-1373.00073529412));
#160453=CARTESIAN_POINT('Ctrl Pts',(-17.3590292079831,4.93906964482096,
-1374.49485294118));
#160454=CARTESIAN_POINT('Ctrl Pts',(-16.9013570056506,6.54762058645456,
-1375.98897058824));
#160455=CARTESIAN_POINT('Ctrl Pts',(-16.1559070823762,8.04468584505497,
-1377.48308823529));
#160456=CARTESIAN_POINT('Ctrl Pts',(-15.4104571591017,9.54175110365538,
-1378.97720588235));
#160457=CARTESIAN_POINT('Ctrl Pts',(-14.4026149179538,10.8763499173728,
-1380.47132352941));
#160458=CARTESIAN_POINT('Ctrl Pts',(-13.3947726768058,12.2109487310903,
-1381.96544117647));
#160459=CARTESIAN_POINT('Ctrl Pts',(-12.1588589765331,13.3376329379985,
-1383.45955882353));
#160460=CARTESIAN_POINT('Ctrl Pts',(-10.9229452762603,14.4643171449067,
-1384.95367647059));
#160461=CARTESIAN_POINT('Ctrl Pts',(-9.50104767561052,15.3447188656481,
-1386.44779411765));
#160462=CARTESIAN_POINT('Ctrl Pts',(-8.07915007496071,16.2251205863895,
-1387.94191176471));
#160463=CARTESIAN_POINT('Ctrl Pts',(-6.51968959134574,16.8292587962898,
-1389.43602941176));
#160464=CARTESIAN_POINT('Ctrl Pts',(-4.96022910773078,17.4333970061901,
-1390.93014705882));
#160465=CARTESIAN_POINT('Ctrl Pts',(-3.31631129755346,17.7406985030951,
-1392.42426470588));
#160466=CARTESIAN_POINT('Ctrl Pts',(-1.67239348737615,18.048,-1393.91838235294));
#160467=CARTESIAN_POINT('Ctrl Pts',(-2.21024254310115E-15,18.048,-1395.4125));
#160468=CARTESIAN_POINT('Ctrl Pts',(1.67239348737616,18.048,-1396.90661764706));
#160469=CARTESIAN_POINT('Ctrl Pts',(3.31631129755346,17.7406985030951,-1398.40073529412));
#160470=CARTESIAN_POINT('Ctrl Pts',(4.96022910773077,17.4333970061901,-1399.89485294118));
#160471=CARTESIAN_POINT('Ctrl Pts',(6.51968959134575,16.8292587962898,-1401.38897058824));
#160472=CARTESIAN_POINT('Ctrl Pts',(8.07915007496071,16.2251205863895,-1402.88308823529));
#160473=CARTESIAN_POINT('Ctrl Pts',(9.50104767561053,15.3447188656481,-1404.37720588235));
#160474=CARTESIAN_POINT('Ctrl Pts',(10.9229452762603,14.4643171449067,-1405.87132352941));
#160475=CARTESIAN_POINT('Ctrl Pts',(12.1588589765331,13.3376329379985,-1407.36544117647));
#160476=CARTESIAN_POINT('Ctrl Pts',(13.3947726768058,12.2109487310903,-1408.85955882353));
#160477=CARTESIAN_POINT('Ctrl Pts',(14.4026149179538,10.8763499173728,-1410.35367647059));
#160478=CARTESIAN_POINT('Ctrl Pts',(15.4104571591017,9.54175110365538,-1411.84779411765));
#160479=CARTESIAN_POINT('Ctrl Pts',(16.1559070823762,8.04468584505496,-1413.34191176471));
#160480=CARTESIAN_POINT('Ctrl Pts',(16.9013570056506,6.54762058645456,-1414.83602941176));
#160481=CARTESIAN_POINT('Ctrl Pts',(17.3590292079831,4.93906964482096,-1416.33014705882));
#160482=CARTESIAN_POINT('Ctrl Pts',(17.8167014103155,3.33051870318735,-1417.82426470588));
#160483=CARTESIAN_POINT('Ctrl Pts',(17.9710104137728,1.66525935159367,-1419.31838235294));
#160484=CARTESIAN_POINT('Ctrl Pts',(18.1253194172301,3.32956716117513E-15,
-1420.8125));
#160485=CARTESIAN_POINT('Ctrl Pts',(17.9710104137728,-1.66525935159367,
-1422.30661764706));
#160486=CARTESIAN_POINT('Ctrl Pts',(17.8167014103155,-3.33051870318736,
-1423.80073529412));
#160487=CARTESIAN_POINT('Ctrl Pts',(17.3590292079831,-4.93906964482095,
-1425.29485294118));
#160488=CARTESIAN_POINT('Ctrl Pts',(16.9013570056506,-6.54762058645456,
-1426.78897058824));
#160489=CARTESIAN_POINT('Ctrl Pts',(16.1559070823762,-8.04468584505497,
-1428.28308823529));
#160490=CARTESIAN_POINT('Ctrl Pts',(15.4104571591017,-9.54175110365538,
-1429.77720588235));
#160491=CARTESIAN_POINT('Ctrl Pts',(14.4026149179538,-10.8763499173728,
-1431.27132352941));
#160492=CARTESIAN_POINT('Ctrl Pts',(13.3947726768058,-12.2109487310903,
-1432.76544117647));
#160493=CARTESIAN_POINT('Ctrl Pts',(12.1588589765331,-13.3376329379985,
-1434.25955882353));
#160494=CARTESIAN_POINT('Ctrl Pts',(10.9229452762603,-14.4643171449067,
-1435.75367647059));
#160495=CARTESIAN_POINT('Ctrl Pts',(9.50104767561053,-15.3447188656481,
-1437.24779411765));
#160496=CARTESIAN_POINT('Ctrl Pts',(8.07915007496071,-16.2251205863895,
-1438.74191176471));
#160497=CARTESIAN_POINT('Ctrl Pts',(6.51968959134574,-16.8292587962898,
-1440.23602941176));
#160498=CARTESIAN_POINT('Ctrl Pts',(4.96022910773078,-17.4333970061901,
-1441.73014705882));
#160499=CARTESIAN_POINT('Ctrl Pts',(3.31631129755346,-17.7406985030951,
-1443.22426470588));
#160500=CARTESIAN_POINT('Ctrl Pts',(1.67239348737615,-18.048,-1444.71838235294));
#160501=CARTESIAN_POINT('Ctrl Pts',(0.,-18.048,-1446.2125));
#160502=CARTESIAN_POINT('Ctrl Pts',(-1.67239348737615,-18.048,-1447.70661764706));
#160503=CARTESIAN_POINT('Ctrl Pts',(-3.31631129755346,-17.7406985030951,
-1449.20073529412));
#160504=CARTESIAN_POINT('Ctrl Pts',(-4.96022910773077,-17.4333970061901,
-1450.69485294118));
#160505=CARTESIAN_POINT('Ctrl Pts',(-6.51968959134574,-16.8292587962898,
-1452.18897058824));
#160506=CARTESIAN_POINT('Ctrl Pts',(-8.07915007496071,-16.2251205863895,
-1453.68308823529));
#160507=CARTESIAN_POINT('Ctrl Pts',(-9.50104767561052,-15.3447188656481,
-1455.17720588235));
#160508=CARTESIAN_POINT('Ctrl Pts',(-10.9229452762603,-14.4643171449067,
-1456.67132352941));
#160509=CARTESIAN_POINT('Ctrl Pts',(-12.1588589765331,-13.3376329379985,
-1458.16544117647));
#160510=CARTESIAN_POINT('Ctrl Pts',(-13.3947726768058,-12.2109487310903,
-1459.65955882353));
#160511=CARTESIAN_POINT('Ctrl Pts',(-14.4026149179538,-10.8763499173728,
-1461.15367647059));
#160512=CARTESIAN_POINT('Ctrl Pts',(-15.4104571591017,-9.54175110365538,
-1462.64779411765));
#160513=CARTESIAN_POINT('Ctrl Pts',(-16.1559070823762,-8.04468584505497,
-1464.14191176471));
#160514=CARTESIAN_POINT('Ctrl Pts',(-16.9013570056506,-6.54762058645456,
-1465.63602941176));
#160515=CARTESIAN_POINT('Ctrl Pts',(-17.3590292079831,-4.93906964482095,
-1467.13014705882));
#160516=CARTESIAN_POINT('Ctrl Pts',(-17.8167014103155,-3.33051870318735,
-1468.62426470588));
#160517=CARTESIAN_POINT('Ctrl Pts',(-17.9710104137728,-1.66525935159368,
-1470.11838235294));
#160518=CARTESIAN_POINT('Ctrl Pts',(-18.1253194172301,-1.10985572039171E-15,
-1471.6125));
#160519=CARTESIAN_POINT('Ctrl Pts',(-17.9710104137728,1.66525935159367,
-1473.10661764706));
#160520=CARTESIAN_POINT('Ctrl Pts',(-17.8167014103155,3.33051870318735,
-1474.60073529412));
#160521=CARTESIAN_POINT('Ctrl Pts',(-17.3590292079831,4.93906964482096,
-1476.09485294118));
#160522=CARTESIAN_POINT('Ctrl Pts',(-16.9013570056506,6.54762058645456,
-1477.58897058824));
#160523=CARTESIAN_POINT('Ctrl Pts',(-16.1559070823762,8.04468584505497,
-1479.08308823529));
#160524=CARTESIAN_POINT('Ctrl Pts',(-15.4104571591017,9.54175110365538,
-1480.57720588235));
#160525=CARTESIAN_POINT('Ctrl Pts',(-14.4026149179538,10.8763499173728,
-1482.07132352941));
#160526=CARTESIAN_POINT('Ctrl Pts',(-13.3947726768058,12.2109487310903,
-1483.56544117647));
#160527=CARTESIAN_POINT('Ctrl Pts',(-12.1588589765331,13.3376329379985,
-1485.05955882353));
#160528=CARTESIAN_POINT('Ctrl Pts',(-10.9229452762603,14.4643171449067,
-1486.55367647059));
#160529=CARTESIAN_POINT('Ctrl Pts',(-9.50104767561052,15.3447188656481,
-1488.04779411765));
#160530=CARTESIAN_POINT('Ctrl Pts',(-8.07915007496071,16.2251205863895,
-1489.54191176471));
#160531=CARTESIAN_POINT('Ctrl Pts',(-6.51968959134574,16.8292587962898,
-1491.03602941176));
#160532=CARTESIAN_POINT('Ctrl Pts',(-4.96022910773078,17.4333970061901,
-1492.53014705882));
#160533=CARTESIAN_POINT('Ctrl Pts',(-3.31631129755346,17.7406985030951,
-1494.02426470588));
#160534=CARTESIAN_POINT('Ctrl Pts',(-1.67239348737615,18.048,-1495.51838235294));
#160535=CARTESIAN_POINT('Ctrl Pts',(-2.21024254310115E-15,18.048,-1497.0125));
#160536=CARTESIAN_POINT('Ctrl Pts',(1.67239348737616,18.048,-1498.50661764706));
#160537=CARTESIAN_POINT('Ctrl Pts',(3.31631129755346,17.7406985030951,-1500.00073529412));
#160538=CARTESIAN_POINT('Ctrl Pts',(4.96022910773077,17.4333970061901,-1501.49485294118));
#160539=CARTESIAN_POINT('Ctrl Pts',(6.51968959134575,16.8292587962898,-1502.98897058824));
#160540=CARTESIAN_POINT('Ctrl Pts',(7.54128438222262,16.4334908658495,-1503.96775961254));
#160541=CARTESIAN_POINT('Ctrl Pts',(8.50750525179181,15.917055581694,-1504.9503325767));
#160542=CARTESIAN_POINT('Ctrl Pts',(0.,-15.,1500.1875));
#160543=CARTESIAN_POINT('Ctrl Pts',(-1.38995469363045,-15.,1498.69338235294));
#160544=CARTESIAN_POINT('Ctrl Pts',(-2.75624276724856,-14.7445964952585,
1497.19926470588));
#160545=CARTESIAN_POINT('Ctrl Pts',(-4.12253084086666,-14.4891929905171,
1495.70514705882));
#160546=CARTESIAN_POINT('Ctrl Pts',(-5.41862499280729,-13.9870834410653,
1494.21102941176));
#160547=CARTESIAN_POINT('Ctrl Pts',(-6.71471914474793,-13.4849738916136,
1492.71691176471));
#160548=CARTESIAN_POINT('Ctrl Pts',(-7.89648244316034,-12.7532570359442,
1491.22279411765));
#160549=CARTESIAN_POINT('Ctrl Pts',(-9.07824574157275,-12.0215401802748,
1489.72867647059));
#160550=CARTESIAN_POINT('Ctrl Pts',(-10.1054346546984,-11.0851337583099,
1488.23455882353));
#160551=CARTESIAN_POINT('Ctrl Pts',(-11.132623567824,-10.148727336345,1486.74044117647));
#160552=CARTESIAN_POINT('Ctrl Pts',(-11.9702584092036,-9.03951954568885,
1485.24632352941));
#160553=CARTESIAN_POINT('Ctrl Pts',(-12.8078932505832,-7.93031175503273,
1483.75220588235));
#160554=CARTESIAN_POINT('Ctrl Pts',(-13.4274493703259,-6.68607533664808,
1482.25808823529));
#160555=CARTESIAN_POINT('Ctrl Pts',(-14.0470054900687,-5.44183891826343,
1480.76397058824));
#160556=CARTESIAN_POINT('Ctrl Pts',(-14.4273846475923,-4.10494485108124,
1479.26985294118));
#160557=CARTESIAN_POINT('Ctrl Pts',(-14.8077638051159,-2.76805078389906,
1477.77573529412));
#160558=CARTESIAN_POINT('Ctrl Pts',(-14.9360126444255,-1.38402539194953,
1476.28161764706));
#160559=CARTESIAN_POINT('Ctrl Pts',(-15.0642614837351,-9.22419980378748E-16,
1474.7875));
#160560=CARTESIAN_POINT('Ctrl Pts',(-14.9360126444255,1.38402539194953,
1473.29338235294));
#160561=CARTESIAN_POINT('Ctrl Pts',(-14.8077638051159,2.76805078389906,
1471.79926470588));
#160562=CARTESIAN_POINT('Ctrl Pts',(-14.4273846475923,4.10494485108124,
1470.30514705882));
#160563=CARTESIAN_POINT('Ctrl Pts',(-14.0470054900687,5.44183891826343,
1468.81102941177));
#160564=CARTESIAN_POINT('Ctrl Pts',(-13.4274493703259,6.68607533664807,
1467.31691176471));
#160565=CARTESIAN_POINT('Ctrl Pts',(-12.8078932505832,7.93031175503273,
1465.82279411765));
#160566=CARTESIAN_POINT('Ctrl Pts',(-11.9702584092036,9.03951954568884,
1464.32867647059));
#160567=CARTESIAN_POINT('Ctrl Pts',(-11.132623567824,10.148727336345,1462.83455882353));
#160568=CARTESIAN_POINT('Ctrl Pts',(-10.1054346546984,11.0851337583099,
1461.34044117647));
#160569=CARTESIAN_POINT('Ctrl Pts',(-9.07824574157275,12.0215401802748,
1459.84632352941));
#160570=CARTESIAN_POINT('Ctrl Pts',(-7.89648244316034,12.7532570359442,
1458.35220588235));
#160571=CARTESIAN_POINT('Ctrl Pts',(-6.71471914474793,13.4849738916136,
1456.85808823529));
#160572=CARTESIAN_POINT('Ctrl Pts',(-5.41862499280729,13.9870834410653,
1455.36397058824));
#160573=CARTESIAN_POINT('Ctrl Pts',(-4.12253084086667,14.4891929905171,
1453.86985294118));
#160574=CARTESIAN_POINT('Ctrl Pts',(-2.75624276724856,14.7445964952585,
1452.37573529412));
#160575=CARTESIAN_POINT('Ctrl Pts',(-1.38995469363044,15.,1450.88161764706));
#160576=CARTESIAN_POINT('Ctrl Pts',(-1.83697019872103E-15,15.,1449.3875));
#160577=CARTESIAN_POINT('Ctrl Pts',(1.38995469363045,15.,1447.89338235294));
#160578=CARTESIAN_POINT('Ctrl Pts',(2.75624276724855,14.7445964952585,1446.39926470588));
#160579=CARTESIAN_POINT('Ctrl Pts',(4.12253084086666,14.4891929905171,1444.90514705882));
#160580=CARTESIAN_POINT('Ctrl Pts',(5.4186249928073,13.9870834410653,1443.41102941176));
#160581=CARTESIAN_POINT('Ctrl Pts',(6.71471914474792,13.4849738916136,1441.91691176471));
#160582=CARTESIAN_POINT('Ctrl Pts',(7.89648244316034,12.7532570359442,1440.42279411765));
#160583=CARTESIAN_POINT('Ctrl Pts',(9.07824574157275,12.0215401802748,1438.92867647059));
#160584=CARTESIAN_POINT('Ctrl Pts',(10.1054346546984,11.0851337583099,1437.43455882353));
#160585=CARTESIAN_POINT('Ctrl Pts',(11.132623567824,10.148727336345,1435.94044117647));
#160586=CARTESIAN_POINT('Ctrl Pts',(11.9702584092036,9.03951954568885,1434.44632352941));
#160587=CARTESIAN_POINT('Ctrl Pts',(12.8078932505832,7.93031175503273,1432.95220588235));
#160588=CARTESIAN_POINT('Ctrl Pts',(13.4274493703259,6.68607533664807,1431.45808823529));
#160589=CARTESIAN_POINT('Ctrl Pts',(14.0470054900687,5.44183891826343,1429.96397058824));
#160590=CARTESIAN_POINT('Ctrl Pts',(14.4273846475923,4.10494485108125,1428.46985294118));
#160591=CARTESIAN_POINT('Ctrl Pts',(14.8077638051159,2.76805078389905,1426.97573529412));
#160592=CARTESIAN_POINT('Ctrl Pts',(14.9360126444255,1.38402539194953,1425.48161764706));
#160593=CARTESIAN_POINT('Ctrl Pts',(15.0642614837351,2.76725994113625E-15,
1423.9875));
#160594=CARTESIAN_POINT('Ctrl Pts',(14.9360126444255,-1.38402539194952,
1422.49338235294));
#160595=CARTESIAN_POINT('Ctrl Pts',(14.8077638051159,-2.76805078389906,
1420.99926470588));
#160596=CARTESIAN_POINT('Ctrl Pts',(14.4273846475923,-4.10494485108124,
1419.50514705882));
#160597=CARTESIAN_POINT('Ctrl Pts',(14.0470054900687,-5.44183891826342,
1418.01102941176));
#160598=CARTESIAN_POINT('Ctrl Pts',(13.4274493703259,-6.68607533664808,
1416.51691176471));
#160599=CARTESIAN_POINT('Ctrl Pts',(12.8078932505832,-7.93031175503273,
1415.02279411765));
#160600=CARTESIAN_POINT('Ctrl Pts',(11.9702584092036,-9.03951954568884,
1413.52867647059));
#160601=CARTESIAN_POINT('Ctrl Pts',(11.132623567824,-10.148727336345,1412.03455882353));
#160602=CARTESIAN_POINT('Ctrl Pts',(10.1054346546984,-11.0851337583099,
1410.54044117647));
#160603=CARTESIAN_POINT('Ctrl Pts',(9.07824574157275,-12.0215401802748,
1409.04632352941));
#160604=CARTESIAN_POINT('Ctrl Pts',(7.89648244316034,-12.7532570359442,
1407.55220588235));
#160605=CARTESIAN_POINT('Ctrl Pts',(6.71471914474792,-13.4849738916136,
1406.05808823529));
#160606=CARTESIAN_POINT('Ctrl Pts',(5.4186249928073,-13.9870834410653,1404.56397058824));
#160607=CARTESIAN_POINT('Ctrl Pts',(4.12253084086667,-14.4891929905171,
1403.06985294118));
#160608=CARTESIAN_POINT('Ctrl Pts',(2.75624276724855,-14.7445964952585,
1401.57573529412));
#160609=CARTESIAN_POINT('Ctrl Pts',(1.38995469363045,-15.,1400.08161764706));
#160610=CARTESIAN_POINT('Ctrl Pts',(0.,-15.,1398.5875));
#160611=CARTESIAN_POINT('Ctrl Pts',(-1.38995469363045,-15.,1397.09338235294));
#160612=CARTESIAN_POINT('Ctrl Pts',(-2.75624276724856,-14.7445964952585,
1395.59926470588));
#160613=CARTESIAN_POINT('Ctrl Pts',(-4.12253084086666,-14.4891929905171,
1394.10514705882));
#160614=CARTESIAN_POINT('Ctrl Pts',(-5.41862499280729,-13.9870834410653,
1392.61102941176));
#160615=CARTESIAN_POINT('Ctrl Pts',(-6.71471914474793,-13.4849738916136,
1391.11691176471));
#160616=CARTESIAN_POINT('Ctrl Pts',(-7.89648244316034,-12.7532570359442,
1389.62279411765));
#160617=CARTESIAN_POINT('Ctrl Pts',(-9.07824574157275,-12.0215401802748,
1388.12867647059));
#160618=CARTESIAN_POINT('Ctrl Pts',(-10.1054346546984,-11.0851337583099,
1386.63455882353));
#160619=CARTESIAN_POINT('Ctrl Pts',(-11.132623567824,-10.148727336345,1385.14044117647));
#160620=CARTESIAN_POINT('Ctrl Pts',(-11.9702584092036,-9.03951954568885,
1383.64632352941));
#160621=CARTESIAN_POINT('Ctrl Pts',(-12.8078932505832,-7.93031175503273,
1382.15220588235));
#160622=CARTESIAN_POINT('Ctrl Pts',(-13.4274493703259,-6.68607533664808,
1380.65808823529));
#160623=CARTESIAN_POINT('Ctrl Pts',(-14.0470054900687,-5.44183891826343,
1379.16397058824));
#160624=CARTESIAN_POINT('Ctrl Pts',(-14.4273846475923,-4.10494485108124,
1377.66985294118));
#160625=CARTESIAN_POINT('Ctrl Pts',(-14.8077638051159,-2.76805078389906,
1376.17573529412));
#160626=CARTESIAN_POINT('Ctrl Pts',(-14.9360126444255,-1.38402539194953,
1374.68161764706));
#160627=CARTESIAN_POINT('Ctrl Pts',(-15.0642614837351,-9.22419980378748E-16,
1373.1875));
#160628=CARTESIAN_POINT('Ctrl Pts',(-14.9360126444255,1.38402539194953,
1371.69338235294));
#160629=CARTESIAN_POINT('Ctrl Pts',(-14.8077638051159,2.76805078389906,
1370.19926470588));
#160630=CARTESIAN_POINT('Ctrl Pts',(-14.4273846475923,4.10494485108124,
1368.70514705882));
#160631=CARTESIAN_POINT('Ctrl Pts',(-14.0470054900687,5.44183891826343,
1367.21102941176));
#160632=CARTESIAN_POINT('Ctrl Pts',(-13.4274493703259,6.68607533664807,
1365.71691176471));
#160633=CARTESIAN_POINT('Ctrl Pts',(-12.8078932505832,7.93031175503273,
1364.22279411765));
#160634=CARTESIAN_POINT('Ctrl Pts',(-11.9702584092036,9.03951954568884,
1362.72867647059));
#160635=CARTESIAN_POINT('Ctrl Pts',(-11.132623567824,10.148727336345,1361.23455882353));
#160636=CARTESIAN_POINT('Ctrl Pts',(-10.1054346546984,11.0851337583099,
1359.74044117647));
#160637=CARTESIAN_POINT('Ctrl Pts',(-9.07824574157275,12.0215401802748,
1358.24632352941));
#160638=CARTESIAN_POINT('Ctrl Pts',(-7.89648244316034,12.7532570359442,
1356.75220588235));
#160639=CARTESIAN_POINT('Ctrl Pts',(-6.71471914474793,13.4849738916136,
1355.25808823529));
#160640=CARTESIAN_POINT('Ctrl Pts',(-5.41862499280729,13.9870834410653,
1353.76397058824));
#160641=CARTESIAN_POINT('Ctrl Pts',(-4.12253084086667,14.4891929905171,
1352.26985294118));
#160642=CARTESIAN_POINT('Ctrl Pts',(-2.75624276724856,14.7445964952585,
1350.77573529412));
#160643=CARTESIAN_POINT('Ctrl Pts',(-1.38995469363044,15.,1349.28161764706));
#160644=CARTESIAN_POINT('Ctrl Pts',(-1.83697019872103E-15,15.,1347.7875));
#160645=CARTESIAN_POINT('Ctrl Pts',(1.38995469363045,15.,1346.29338235294));
#160646=CARTESIAN_POINT('Ctrl Pts',(2.75624276724855,14.7445964952585,1344.79926470588));
#160647=CARTESIAN_POINT('Ctrl Pts',(4.12253084086666,14.4891929905171,1343.30514705882));
#160648=CARTESIAN_POINT('Ctrl Pts',(5.4186249928073,13.9870834410653,1341.81102941176));
#160649=CARTESIAN_POINT('Ctrl Pts',(6.71471914474792,13.4849738916136,1340.31691176471));
#160650=CARTESIAN_POINT('Ctrl Pts',(7.89648244316034,12.7532570359442,1338.82279411765));
#160651=CARTESIAN_POINT('Ctrl Pts',(9.07824574157275,12.0215401802748,1337.32867647059));
#160652=CARTESIAN_POINT('Ctrl Pts',(10.1054346546984,11.0851337583099,1335.83455882353));
#160653=CARTESIAN_POINT('Ctrl Pts',(11.132623567824,10.148727336345,1334.34044117647));
#160654=CARTESIAN_POINT('Ctrl Pts',(11.9702584092036,9.03951954568885,1332.84632352941));
#160655=CARTESIAN_POINT('Ctrl Pts',(12.8078932505832,7.93031175503273,1331.35220588235));
#160656=CARTESIAN_POINT('Ctrl Pts',(13.4274493703259,6.68607533664807,1329.85808823529));
#160657=CARTESIAN_POINT('Ctrl Pts',(14.0470054900687,5.44183891826343,1328.36397058824));
#160658=CARTESIAN_POINT('Ctrl Pts',(14.4273846475923,4.10494485108125,1326.86985294118));
#160659=CARTESIAN_POINT('Ctrl Pts',(14.8077638051159,2.76805078389905,1325.37573529412));
#160660=CARTESIAN_POINT('Ctrl Pts',(14.9360126444255,1.38402539194953,1323.88161764706));
#160661=CARTESIAN_POINT('Ctrl Pts',(15.0642614837351,2.76725994113625E-15,
1322.3875));
#160662=CARTESIAN_POINT('Ctrl Pts',(14.9360126444255,-1.38402539194952,
1320.89338235294));
#160663=CARTESIAN_POINT('Ctrl Pts',(14.8077638051159,-2.76805078389906,
1319.39926470588));
#160664=CARTESIAN_POINT('Ctrl Pts',(14.4273846475923,-4.10494485108124,
1317.90514705882));
#160665=CARTESIAN_POINT('Ctrl Pts',(14.0470054900687,-5.44183891826342,
1316.41102941176));
#160666=CARTESIAN_POINT('Ctrl Pts',(13.4274493703259,-6.68607533664808,
1314.91691176471));
#160667=CARTESIAN_POINT('Ctrl Pts',(12.8078932505832,-7.93031175503273,
1313.42279411765));
#160668=CARTESIAN_POINT('Ctrl Pts',(11.9702584092036,-9.03951954568884,
1311.92867647059));
#160669=CARTESIAN_POINT('Ctrl Pts',(11.132623567824,-10.148727336345,1310.43455882353));
#160670=CARTESIAN_POINT('Ctrl Pts',(10.1054346546984,-11.0851337583099,
1308.94044117647));
#160671=CARTESIAN_POINT('Ctrl Pts',(9.07824574157275,-12.0215401802748,
1307.44632352941));
#160672=CARTESIAN_POINT('Ctrl Pts',(7.89648244316034,-12.7532570359442,
1305.95220588235));
#160673=CARTESIAN_POINT('Ctrl Pts',(6.71471914474792,-13.4849738916136,
1304.45808823529));
#160674=CARTESIAN_POINT('Ctrl Pts',(5.4186249928073,-13.9870834410653,1302.96397058824));
#160675=CARTESIAN_POINT('Ctrl Pts',(4.12253084086667,-14.4891929905171,
1301.46985294118));
#160676=CARTESIAN_POINT('Ctrl Pts',(2.75624276724855,-14.7445964952585,
1299.97573529412));
#160677=CARTESIAN_POINT('Ctrl Pts',(1.38995469363045,-15.,1298.48161764706));
#160678=CARTESIAN_POINT('Ctrl Pts',(0.,-15.,1296.9875));
#160679=CARTESIAN_POINT('Ctrl Pts',(-1.38995469363045,-15.,1295.49338235294));
#160680=CARTESIAN_POINT('Ctrl Pts',(-2.75624276724856,-14.7445964952585,
1293.99926470588));
#160681=CARTESIAN_POINT('Ctrl Pts',(-4.12253084086666,-14.4891929905171,
1292.50514705882));
#160682=CARTESIAN_POINT('Ctrl Pts',(-5.41862499280729,-13.9870834410653,
1291.01102941176));
#160683=CARTESIAN_POINT('Ctrl Pts',(-6.71471914474793,-13.4849738916136,
1289.51691176471));
#160684=CARTESIAN_POINT('Ctrl Pts',(-7.89648244316034,-12.7532570359442,
1288.02279411765));
#160685=CARTESIAN_POINT('Ctrl Pts',(-9.07824574157275,-12.0215401802748,
1286.52867647059));
#160686=CARTESIAN_POINT('Ctrl Pts',(-10.1054346546984,-11.0851337583099,
1285.03455882353));
#160687=CARTESIAN_POINT('Ctrl Pts',(-11.132623567824,-10.148727336345,1283.54044117647));
#160688=CARTESIAN_POINT('Ctrl Pts',(-11.9702584092036,-9.03951954568885,
1282.04632352941));
#160689=CARTESIAN_POINT('Ctrl Pts',(-12.8078932505832,-7.93031175503273,
1280.55220588235));
#160690=CARTESIAN_POINT('Ctrl Pts',(-13.4274493703259,-6.68607533664808,
1279.05808823529));
#160691=CARTESIAN_POINT('Ctrl Pts',(-14.0470054900687,-5.44183891826343,
1277.56397058824));
#160692=CARTESIAN_POINT('Ctrl Pts',(-14.4273846475923,-4.10494485108124,
1276.06985294118));
#160693=CARTESIAN_POINT('Ctrl Pts',(-14.8077638051159,-2.76805078389906,
1274.57573529412));
#160694=CARTESIAN_POINT('Ctrl Pts',(-14.9360126444255,-1.38402539194953,
1273.08161764706));
#160695=CARTESIAN_POINT('Ctrl Pts',(-15.0642614837351,-9.22419980378748E-16,
1271.5875));
#160696=CARTESIAN_POINT('Ctrl Pts',(-14.9360126444255,1.38402539194953,
1270.09338235294));
#160697=CARTESIAN_POINT('Ctrl Pts',(-14.8077638051159,2.76805078389906,
1268.59926470588));
#160698=CARTESIAN_POINT('Ctrl Pts',(-14.4273846475923,4.10494485108124,
1267.10514705882));
#160699=CARTESIAN_POINT('Ctrl Pts',(-14.0470054900687,5.44183891826343,
1265.61102941176));
#160700=CARTESIAN_POINT('Ctrl Pts',(-13.4274493703259,6.68607533664807,
1264.11691176471));
#160701=CARTESIAN_POINT('Ctrl Pts',(-12.8078932505832,7.93031175503273,
1262.62279411765));
#160702=CARTESIAN_POINT('Ctrl Pts',(-11.9702584092036,9.03951954568884,
1261.12867647059));
#160703=CARTESIAN_POINT('Ctrl Pts',(-11.132623567824,10.148727336345,1259.63455882353));
#160704=CARTESIAN_POINT('Ctrl Pts',(-10.1054346546984,11.0851337583099,
1258.14044117647));
#160705=CARTESIAN_POINT('Ctrl Pts',(-9.07824574157275,12.0215401802748,
1256.64632352941));
#160706=CARTESIAN_POINT('Ctrl Pts',(-7.89648244316034,12.7532570359442,
1255.15220588235));
#160707=CARTESIAN_POINT('Ctrl Pts',(-6.71471914474793,13.4849738916136,
1253.65808823529));
#160708=CARTESIAN_POINT('Ctrl Pts',(-5.41862499280729,13.9870834410653,
1252.16397058824));
#160709=CARTESIAN_POINT('Ctrl Pts',(-4.12253084086667,14.4891929905171,
1250.66985294118));
#160710=CARTESIAN_POINT('Ctrl Pts',(-2.75624276724856,14.7445964952585,
1249.17573529412));
#160711=CARTESIAN_POINT('Ctrl Pts',(-1.38995469363044,15.,1247.68161764706));
#160712=CARTESIAN_POINT('Ctrl Pts',(-1.83697019872103E-15,15.,1246.1875));
#160713=CARTESIAN_POINT('Ctrl Pts',(1.38995469363045,15.,1244.69338235294));
#160714=CARTESIAN_POINT('Ctrl Pts',(2.75624276724855,14.7445964952585,1243.19926470588));
#160715=CARTESIAN_POINT('Ctrl Pts',(4.12253084086666,14.4891929905171,1241.70514705882));
#160716=CARTESIAN_POINT('Ctrl Pts',(5.4186249928073,13.9870834410653,1240.21102941176));
#160717=CARTESIAN_POINT('Ctrl Pts',(6.71471914474792,13.4849738916136,1238.71691176471));
#160718=CARTESIAN_POINT('Ctrl Pts',(7.89648244316034,12.7532570359442,1237.22279411765));
#160719=CARTESIAN_POINT('Ctrl Pts',(9.07824574157275,12.0215401802748,1235.72867647059));
#160720=CARTESIAN_POINT('Ctrl Pts',(10.1054346546984,11.0851337583099,1234.23455882353));
#160721=CARTESIAN_POINT('Ctrl Pts',(11.132623567824,10.148727336345,1232.74044117647));
#160722=CARTESIAN_POINT('Ctrl Pts',(11.9702584092036,9.03951954568885,1231.24632352941));
#160723=CARTESIAN_POINT('Ctrl Pts',(12.8078932505832,7.93031175503273,1229.75220588235));
#160724=CARTESIAN_POINT('Ctrl Pts',(13.4274493703259,6.68607533664807,1228.25808823529));
#160725=CARTESIAN_POINT('Ctrl Pts',(14.0470054900687,5.44183891826343,1226.76397058824));
#160726=CARTESIAN_POINT('Ctrl Pts',(14.4273846475923,4.10494485108125,1225.26985294118));
#160727=CARTESIAN_POINT('Ctrl Pts',(14.8077638051159,2.76805078389905,1223.77573529412));
#160728=CARTESIAN_POINT('Ctrl Pts',(14.9360126444255,1.38402539194953,1222.28161764706));
#160729=CARTESIAN_POINT('Ctrl Pts',(15.0642614837351,2.76725994113625E-15,
1220.7875));
#160730=CARTESIAN_POINT('Ctrl Pts',(14.9360126444255,-1.38402539194952,
1219.29338235294));
#160731=CARTESIAN_POINT('Ctrl Pts',(14.8077638051159,-2.76805078389906,
1217.79926470588));
#160732=CARTESIAN_POINT('Ctrl Pts',(14.4273846475923,-4.10494485108124,
1216.30514705882));
#160733=CARTESIAN_POINT('Ctrl Pts',(14.0470054900687,-5.44183891826342,
1214.81102941176));
#160734=CARTESIAN_POINT('Ctrl Pts',(13.4274493703259,-6.68607533664808,
1213.31691176471));
#160735=CARTESIAN_POINT('Ctrl Pts',(12.8078932505832,-7.93031175503273,
1211.82279411765));
#160736=CARTESIAN_POINT('Ctrl Pts',(11.9702584092036,-9.03951954568884,
1210.32867647059));
#160737=CARTESIAN_POINT('Ctrl Pts',(11.132623567824,-10.148727336345,1208.83455882353));
#160738=CARTESIAN_POINT('Ctrl Pts',(10.1054346546984,-11.0851337583099,
1207.34044117647));
#160739=CARTESIAN_POINT('Ctrl Pts',(9.07824574157275,-12.0215401802748,
1205.84632352941));
#160740=CARTESIAN_POINT('Ctrl Pts',(7.89648244316034,-12.7532570359442,
1204.35220588235));
#160741=CARTESIAN_POINT('Ctrl Pts',(6.71471914474792,-13.4849738916136,
1202.85808823529));
#160742=CARTESIAN_POINT('Ctrl Pts',(5.4186249928073,-13.9870834410653,1201.36397058824));
#160743=CARTESIAN_POINT('Ctrl Pts',(4.12253084086667,-14.4891929905171,
1199.86985294118));
#160744=CARTESIAN_POINT('Ctrl Pts',(2.75624276724855,-14.7445964952585,
1198.37573529412));
#160745=CARTESIAN_POINT('Ctrl Pts',(1.38995469363045,-15.,1196.88161764706));
#160746=CARTESIAN_POINT('Ctrl Pts',(0.,-15.,1195.3875));
#160747=CARTESIAN_POINT('Ctrl Pts',(-1.38995469363045,-15.,1193.89338235294));
#160748=CARTESIAN_POINT('Ctrl Pts',(-2.75624276724856,-14.7445964952585,
1192.39926470588));
#160749=CARTESIAN_POINT('Ctrl Pts',(-4.12253084086666,-14.4891929905171,
1190.90514705882));
#160750=CARTESIAN_POINT('Ctrl Pts',(-5.41862499280729,-13.9870834410653,
1189.41102941176));
#160751=CARTESIAN_POINT('Ctrl Pts',(-6.71471914474793,-13.4849738916136,
1187.91691176471));
#160752=CARTESIAN_POINT('Ctrl Pts',(-7.89648244316034,-12.7532570359442,
1186.42279411765));
#160753=CARTESIAN_POINT('Ctrl Pts',(-9.07824574157275,-12.0215401802748,
1184.92867647059));
#160754=CARTESIAN_POINT('Ctrl Pts',(-10.1054346546984,-11.0851337583099,
1183.43455882353));
#160755=CARTESIAN_POINT('Ctrl Pts',(-11.132623567824,-10.148727336345,1181.94044117647));
#160756=CARTESIAN_POINT('Ctrl Pts',(-11.9702584092036,-9.03951954568885,
1180.44632352941));
#160757=CARTESIAN_POINT('Ctrl Pts',(-12.8078932505832,-7.93031175503273,
1178.95220588235));
#160758=CARTESIAN_POINT('Ctrl Pts',(-13.4274493703259,-6.68607533664808,
1177.45808823529));
#160759=CARTESIAN_POINT('Ctrl Pts',(-14.0470054900687,-5.44183891826343,
1175.96397058824));
#160760=CARTESIAN_POINT('Ctrl Pts',(-14.4273846475923,-4.10494485108124,
1174.46985294118));
#160761=CARTESIAN_POINT('Ctrl Pts',(-14.8077638051159,-2.76805078389906,
1172.97573529412));
#160762=CARTESIAN_POINT('Ctrl Pts',(-14.9360126444255,-1.38402539194953,
1171.48161764706));
#160763=CARTESIAN_POINT('Ctrl Pts',(-15.0642614837351,-9.22419980378748E-16,
1169.9875));
#160764=CARTESIAN_POINT('Ctrl Pts',(-14.9360126444255,1.38402539194953,
1168.49338235294));
#160765=CARTESIAN_POINT('Ctrl Pts',(-14.8077638051159,2.76805078389906,
1166.99926470588));
#160766=CARTESIAN_POINT('Ctrl Pts',(-14.4273846475923,4.10494485108124,
1165.50514705882));
#160767=CARTESIAN_POINT('Ctrl Pts',(-14.0470054900687,5.44183891826343,
1164.01102941176));
#160768=CARTESIAN_POINT('Ctrl Pts',(-13.4274493703259,6.68607533664807,
1162.51691176471));
#160769=CARTESIAN_POINT('Ctrl Pts',(-12.8078932505832,7.93031175503273,
1161.02279411765));
#160770=CARTESIAN_POINT('Ctrl Pts',(-11.9702584092036,9.03951954568884,
1159.52867647059));
#160771=CARTESIAN_POINT('Ctrl Pts',(-11.132623567824,10.148727336345,1158.03455882353));
#160772=CARTESIAN_POINT('Ctrl Pts',(-10.1054346546984,11.0851337583099,
1156.54044117647));
#160773=CARTESIAN_POINT('Ctrl Pts',(-9.07824574157275,12.0215401802748,
1155.04632352941));
#160774=CARTESIAN_POINT('Ctrl Pts',(-7.89648244316034,12.7532570359442,
1153.55220588235));
#160775=CARTESIAN_POINT('Ctrl Pts',(-6.71471914474793,13.4849738916136,
1152.05808823529));
#160776=CARTESIAN_POINT('Ctrl Pts',(-5.41862499280729,13.9870834410653,
1150.56397058824));
#160777=CARTESIAN_POINT('Ctrl Pts',(-4.12253084086667,14.4891929905171,
1149.06985294118));
#160778=CARTESIAN_POINT('Ctrl Pts',(-2.75624276724856,14.7445964952585,
1147.57573529412));
#160779=CARTESIAN_POINT('Ctrl Pts',(-1.38995469363044,15.,1146.08161764706));
#160780=CARTESIAN_POINT('Ctrl Pts',(-1.83697019872103E-15,15.,1144.5875));
#160781=CARTESIAN_POINT('Ctrl Pts',(1.38995469363045,15.,1143.09338235294));
#160782=CARTESIAN_POINT('Ctrl Pts',(2.75624276724855,14.7445964952585,1141.59926470588));
#160783=CARTESIAN_POINT('Ctrl Pts',(4.12253084086666,14.4891929905171,1140.10514705882));
#160784=CARTESIAN_POINT('Ctrl Pts',(5.4186249928073,13.9870834410653,1138.61102941176));
#160785=CARTESIAN_POINT('Ctrl Pts',(6.71471914474792,13.4849738916136,1137.11691176471));
#160786=CARTESIAN_POINT('Ctrl Pts',(7.89648244316034,12.7532570359442,1135.62279411765));
#160787=CARTESIAN_POINT('Ctrl Pts',(9.07824574157275,12.0215401802748,1134.12867647059));
#160788=CARTESIAN_POINT('Ctrl Pts',(10.1054346546984,11.0851337583099,1132.63455882353));
#160789=CARTESIAN_POINT('Ctrl Pts',(11.132623567824,10.148727336345,1131.14044117647));
#160790=CARTESIAN_POINT('Ctrl Pts',(11.9702584092036,9.03951954568885,1129.64632352941));
#160791=CARTESIAN_POINT('Ctrl Pts',(12.8078932505832,7.93031175503273,1128.15220588235));
#160792=CARTESIAN_POINT('Ctrl Pts',(13.4274493703259,6.68607533664807,1126.65808823529));
#160793=CARTESIAN_POINT('Ctrl Pts',(14.0470054900687,5.44183891826343,1125.16397058824));
#160794=CARTESIAN_POINT('Ctrl Pts',(14.4273846475923,4.10494485108125,1123.66985294118));
#160795=CARTESIAN_POINT('Ctrl Pts',(14.8077638051159,2.76805078389905,1122.17573529412));
#160796=CARTESIAN_POINT('Ctrl Pts',(14.9360126444255,1.38402539194953,1120.68161764706));
#160797=CARTESIAN_POINT('Ctrl Pts',(15.0642614837351,2.76725994113625E-15,
1119.1875));
#160798=CARTESIAN_POINT('Ctrl Pts',(14.9360126444255,-1.38402539194952,
1117.69338235294));
#160799=CARTESIAN_POINT('Ctrl Pts',(14.8077638051159,-2.76805078389906,
1116.19926470588));
#160800=CARTESIAN_POINT('Ctrl Pts',(14.4273846475923,-4.10494485108124,
1114.70514705882));
#160801=CARTESIAN_POINT('Ctrl Pts',(14.0470054900687,-5.44183891826342,
1113.21102941176));
#160802=CARTESIAN_POINT('Ctrl Pts',(13.4274493703259,-6.68607533664808,
1111.71691176471));
#160803=CARTESIAN_POINT('Ctrl Pts',(12.8078932505832,-7.93031175503273,
1110.22279411765));
#160804=CARTESIAN_POINT('Ctrl Pts',(11.9702584092036,-9.03951954568884,
1108.72867647059));
#160805=CARTESIAN_POINT('Ctrl Pts',(11.132623567824,-10.148727336345,1107.23455882353));
#160806=CARTESIAN_POINT('Ctrl Pts',(10.1054346546984,-11.0851337583099,
1105.74044117647));
#160807=CARTESIAN_POINT('Ctrl Pts',(9.07824574157275,-12.0215401802748,
1104.24632352941));
#160808=CARTESIAN_POINT('Ctrl Pts',(7.89648244316034,-12.7532570359442,
1102.75220588235));
#160809=CARTESIAN_POINT('Ctrl Pts',(6.71471914474792,-13.4849738916136,
1101.25808823529));
#160810=CARTESIAN_POINT('Ctrl Pts',(5.4186249928073,-13.9870834410653,1099.76397058824));
#160811=CARTESIAN_POINT('Ctrl Pts',(4.12253084086667,-14.4891929905171,
1098.26985294118));
#160812=CARTESIAN_POINT('Ctrl Pts',(2.75624276724855,-14.7445964952585,
1096.77573529412));
#160813=CARTESIAN_POINT('Ctrl Pts',(1.38995469363045,-15.,1095.28161764706));
#160814=CARTESIAN_POINT('Ctrl Pts',(0.,-15.,1093.7875));
#160815=CARTESIAN_POINT('Ctrl Pts',(-1.38995469363045,-15.,1092.29338235294));
#160816=CARTESIAN_POINT('Ctrl Pts',(-2.75624276724856,-14.7445964952585,
1090.79926470588));
#160817=CARTESIAN_POINT('Ctrl Pts',(-4.12253084086666,-14.4891929905171,
1089.30514705882));
#160818=CARTESIAN_POINT('Ctrl Pts',(-5.41862499280729,-13.9870834410653,
1087.81102941176));
#160819=CARTESIAN_POINT('Ctrl Pts',(-6.71471914474793,-13.4849738916136,
1086.31691176471));
#160820=CARTESIAN_POINT('Ctrl Pts',(-7.89648244316034,-12.7532570359442,
1084.82279411765));
#160821=CARTESIAN_POINT('Ctrl Pts',(-9.07824574157275,-12.0215401802748,
1083.32867647059));
#160822=CARTESIAN_POINT('Ctrl Pts',(-10.1054346546984,-11.0851337583099,
1081.83455882353));
#160823=CARTESIAN_POINT('Ctrl Pts',(-11.132623567824,-10.148727336345,1080.34044117647));
#160824=CARTESIAN_POINT('Ctrl Pts',(-11.9702584092036,-9.03951954568885,
1078.84632352941));
#160825=CARTESIAN_POINT('Ctrl Pts',(-12.8078932505832,-7.93031175503273,
1077.35220588235));
#160826=CARTESIAN_POINT('Ctrl Pts',(-13.4274493703259,-6.68607533664808,
1075.85808823529));
#160827=CARTESIAN_POINT('Ctrl Pts',(-14.0470054900687,-5.44183891826343,
1074.36397058824));
#160828=CARTESIAN_POINT('Ctrl Pts',(-14.4273846475923,-4.10494485108124,
1072.86985294118));
#160829=CARTESIAN_POINT('Ctrl Pts',(-14.8077638051159,-2.76805078389906,
1071.37573529412));
#160830=CARTESIAN_POINT('Ctrl Pts',(-14.9360126444255,-1.38402539194953,
1069.88161764706));
#160831=CARTESIAN_POINT('Ctrl Pts',(-15.0642614837351,-9.22419980378748E-16,
1068.3875));
#160832=CARTESIAN_POINT('Ctrl Pts',(-14.9360126444255,1.38402539194953,
1066.89338235294));
#160833=CARTESIAN_POINT('Ctrl Pts',(-14.8077638051159,2.76805078389906,
1065.39926470588));
#160834=CARTESIAN_POINT('Ctrl Pts',(-14.4273846475923,4.10494485108124,
1063.90514705882));
#160835=CARTESIAN_POINT('Ctrl Pts',(-14.0470054900687,5.44183891826343,
1062.41102941176));
#160836=CARTESIAN_POINT('Ctrl Pts',(-13.4274493703259,6.68607533664807,
1060.91691176471));
#160837=CARTESIAN_POINT('Ctrl Pts',(-12.8078932505832,7.93031175503273,
1059.42279411765));
#160838=CARTESIAN_POINT('Ctrl Pts',(-11.9702584092036,9.03951954568884,
1057.92867647059));
#160839=CARTESIAN_POINT('Ctrl Pts',(-11.132623567824,10.148727336345,1056.43455882353));
#160840=CARTESIAN_POINT('Ctrl Pts',(-10.1054346546984,11.0851337583099,
1054.94044117647));
#160841=CARTESIAN_POINT('Ctrl Pts',(-9.07824574157275,12.0215401802748,
1053.44632352941));
#160842=CARTESIAN_POINT('Ctrl Pts',(-7.89648244316034,12.7532570359442,
1051.95220588235));
#160843=CARTESIAN_POINT('Ctrl Pts',(-6.71471914474793,13.4849738916136,
1050.45808823529));
#160844=CARTESIAN_POINT('Ctrl Pts',(-5.41862499280729,13.9870834410653,
1048.96397058824));
#160845=CARTESIAN_POINT('Ctrl Pts',(-4.12253084086667,14.4891929905171,
1047.46985294118));
#160846=CARTESIAN_POINT('Ctrl Pts',(-2.75624276724856,14.7445964952585,
1045.97573529412));
#160847=CARTESIAN_POINT('Ctrl Pts',(-1.38995469363044,15.,1044.48161764706));
#160848=CARTESIAN_POINT('Ctrl Pts',(-1.83697019872103E-15,15.,1042.9875));
#160849=CARTESIAN_POINT('Ctrl Pts',(1.38995469363045,15.,1041.49338235294));
#160850=CARTESIAN_POINT('Ctrl Pts',(2.75624276724855,14.7445964952585,1039.99926470588));
#160851=CARTESIAN_POINT('Ctrl Pts',(4.12253084086666,14.4891929905171,1038.50514705882));
#160852=CARTESIAN_POINT('Ctrl Pts',(5.4186249928073,13.9870834410653,1037.01102941176));
#160853=CARTESIAN_POINT('Ctrl Pts',(6.71471914474792,13.4849738916136,1035.51691176471));
#160854=CARTESIAN_POINT('Ctrl Pts',(7.89648244316034,12.7532570359442,1034.02279411765));
#160855=CARTESIAN_POINT('Ctrl Pts',(9.07824574157275,12.0215401802748,1032.52867647059));
#160856=CARTESIAN_POINT('Ctrl Pts',(10.1054346546984,11.0851337583099,1031.03455882353));
#160857=CARTESIAN_POINT('Ctrl Pts',(11.132623567824,10.148727336345,1029.54044117647));
#160858=CARTESIAN_POINT('Ctrl Pts',(11.9702584092036,9.03951954568885,1028.04632352941));
#160859=CARTESIAN_POINT('Ctrl Pts',(12.8078932505832,7.93031175503273,1026.55220588235));
#160860=CARTESIAN_POINT('Ctrl Pts',(13.4274493703259,6.68607533664807,1025.05808823529));
#160861=CARTESIAN_POINT('Ctrl Pts',(14.0470054900687,5.44183891826343,1023.56397058824));
#160862=CARTESIAN_POINT('Ctrl Pts',(14.4273846475923,4.10494485108125,1022.06985294118));
#160863=CARTESIAN_POINT('Ctrl Pts',(14.8077638051159,2.76805078389905,1020.57573529412));
#160864=CARTESIAN_POINT('Ctrl Pts',(14.9360126444255,1.38402539194953,1019.08161764706));
#160865=CARTESIAN_POINT('Ctrl Pts',(15.0642614837351,2.76725994113625E-15,
1017.5875));
#160866=CARTESIAN_POINT('Ctrl Pts',(14.9360126444255,-1.38402539194952,
1016.09338235294));
#160867=CARTESIAN_POINT('Ctrl Pts',(14.8077638051159,-2.76805078389906,
1014.59926470588));
#160868=CARTESIAN_POINT('Ctrl Pts',(14.4273846475923,-4.10494485108124,
1013.10514705882));
#160869=CARTESIAN_POINT('Ctrl Pts',(14.0470054900687,-5.44183891826342,
1011.61102941176));
#160870=CARTESIAN_POINT('Ctrl Pts',(13.4274493703259,-6.68607533664808,
1010.11691176471));
#160871=CARTESIAN_POINT('Ctrl Pts',(12.8078932505832,-7.93031175503273,
1008.62279411765));
#160872=CARTESIAN_POINT('Ctrl Pts',(11.9702584092036,-9.03951954568884,
1007.12867647059));
#160873=CARTESIAN_POINT('Ctrl Pts',(11.132623567824,-10.148727336345,1005.63455882353));
#160874=CARTESIAN_POINT('Ctrl Pts',(10.1054346546984,-11.0851337583099,
1004.14044117647));
#160875=CARTESIAN_POINT('Ctrl Pts',(9.07824574157275,-12.0215401802748,
1002.64632352941));
#160876=CARTESIAN_POINT('Ctrl Pts',(7.89648244316034,-12.7532570359442,
1001.15220588235));
#160877=CARTESIAN_POINT('Ctrl Pts',(6.71471914474792,-13.4849738916136,
999.658088235294));
#160878=CARTESIAN_POINT('Ctrl Pts',(5.4186249928073,-13.9870834410653,998.163970588235));
#160879=CARTESIAN_POINT('Ctrl Pts',(4.12253084086667,-14.4891929905171,
996.669852941177));
#160880=CARTESIAN_POINT('Ctrl Pts',(2.75624276724855,-14.7445964952585,
995.175735294118));
#160881=CARTESIAN_POINT('Ctrl Pts',(1.38995469363045,-15.,993.681617647059));
#160882=CARTESIAN_POINT('Ctrl Pts',(0.,-15.,992.1875));
#160883=CARTESIAN_POINT('Ctrl Pts',(-1.38995469363045,-15.,990.693382352941));
#160884=CARTESIAN_POINT('Ctrl Pts',(-2.75624276724856,-14.7445964952585,
989.199264705882));
#160885=CARTESIAN_POINT('Ctrl Pts',(-4.12253084086666,-14.4891929905171,
987.705147058824));
#160886=CARTESIAN_POINT('Ctrl Pts',(-5.41862499280729,-13.9870834410653,
986.211029411765));
#160887=CARTESIAN_POINT('Ctrl Pts',(-6.71471914474793,-13.4849738916136,
984.716911764706));
#160888=CARTESIAN_POINT('Ctrl Pts',(-7.89648244316034,-12.7532570359442,
983.222794117647));
#160889=CARTESIAN_POINT('Ctrl Pts',(-9.07824574157275,-12.0215401802748,
981.728676470589));
#160890=CARTESIAN_POINT('Ctrl Pts',(-10.1054346546984,-11.0851337583099,
980.234558823529));
#160891=CARTESIAN_POINT('Ctrl Pts',(-11.132623567824,-10.148727336345,978.740441176471));
#160892=CARTESIAN_POINT('Ctrl Pts',(-11.9702584092036,-9.03951954568885,
977.246323529412));
#160893=CARTESIAN_POINT('Ctrl Pts',(-12.8078932505832,-7.93031175503273,
975.752205882353));
#160894=CARTESIAN_POINT('Ctrl Pts',(-13.4274493703259,-6.68607533664808,
974.258088235294));
#160895=CARTESIAN_POINT('Ctrl Pts',(-14.0470054900687,-5.44183891826343,
972.763970588235));
#160896=CARTESIAN_POINT('Ctrl Pts',(-14.4273846475923,-4.10494485108124,
971.269852941177));
#160897=CARTESIAN_POINT('Ctrl Pts',(-14.8077638051159,-2.76805078389906,
969.775735294118));
#160898=CARTESIAN_POINT('Ctrl Pts',(-14.9360126444255,-1.38402539194953,
968.281617647059));
#160899=CARTESIAN_POINT('Ctrl Pts',(-15.0642614837351,-9.22419980378748E-16,
966.7875));
#160900=CARTESIAN_POINT('Ctrl Pts',(-14.9360126444255,1.38402539194953,
965.293382352941));
#160901=CARTESIAN_POINT('Ctrl Pts',(-14.8077638051159,2.76805078389906,
963.799264705882));
#160902=CARTESIAN_POINT('Ctrl Pts',(-14.4273846475923,4.10494485108124,
962.305147058824));
#160903=CARTESIAN_POINT('Ctrl Pts',(-14.0470054900687,5.44183891826343,
960.811029411765));
#160904=CARTESIAN_POINT('Ctrl Pts',(-13.4274493703259,6.68607533664807,
959.316911764706));
#160905=CARTESIAN_POINT('Ctrl Pts',(-12.8078932505832,7.93031175503273,
957.822794117647));
#160906=CARTESIAN_POINT('Ctrl Pts',(-11.9702584092036,9.03951954568884,
956.328676470588));
#160907=CARTESIAN_POINT('Ctrl Pts',(-11.132623567824,10.148727336345,954.834558823529));
#160908=CARTESIAN_POINT('Ctrl Pts',(-10.1054346546984,11.0851337583099,
953.340441176471));
#160909=CARTESIAN_POINT('Ctrl Pts',(-9.07824574157275,12.0215401802748,
951.846323529412));
#160910=CARTESIAN_POINT('Ctrl Pts',(-7.89648244316034,12.7532570359442,
950.352205882353));
#160911=CARTESIAN_POINT('Ctrl Pts',(-6.71471914474793,13.4849738916136,
948.858088235294));
#160912=CARTESIAN_POINT('Ctrl Pts',(-5.41862499280729,13.9870834410653,
947.363970588235));
#160913=CARTESIAN_POINT('Ctrl Pts',(-4.12253084086667,14.4891929905171,
945.869852941177));
#160914=CARTESIAN_POINT('Ctrl Pts',(-2.75624276724856,14.7445964952585,
944.375735294118));
#160915=CARTESIAN_POINT('Ctrl Pts',(-1.38995469363044,15.,942.881617647059));
#160916=CARTESIAN_POINT('Ctrl Pts',(-1.83697019872103E-15,15.,941.3875));
#160917=CARTESIAN_POINT('Ctrl Pts',(1.38995469363045,15.,939.893382352941));
#160918=CARTESIAN_POINT('Ctrl Pts',(2.75624276724855,14.7445964952585,938.399264705882));
#160919=CARTESIAN_POINT('Ctrl Pts',(4.12253084086666,14.4891929905171,936.905147058824));
#160920=CARTESIAN_POINT('Ctrl Pts',(5.4186249928073,13.9870834410653,935.411029411765));
#160921=CARTESIAN_POINT('Ctrl Pts',(6.71471914474792,13.4849738916136,933.916911764706));
#160922=CARTESIAN_POINT('Ctrl Pts',(7.89648244316034,12.7532570359442,932.422794117647));
#160923=CARTESIAN_POINT('Ctrl Pts',(9.07824574157275,12.0215401802748,930.928676470588));
#160924=CARTESIAN_POINT('Ctrl Pts',(10.1054346546984,11.0851337583099,929.43455882353));
#160925=CARTESIAN_POINT('Ctrl Pts',(11.132623567824,10.148727336345,927.94044117647));
#160926=CARTESIAN_POINT('Ctrl Pts',(11.9702584092036,9.03951954568885,926.446323529412));
#160927=CARTESIAN_POINT('Ctrl Pts',(12.8078932505832,7.93031175503273,924.952205882353));
#160928=CARTESIAN_POINT('Ctrl Pts',(13.4274493703259,6.68607533664807,923.458088235294));
#160929=CARTESIAN_POINT('Ctrl Pts',(14.0470054900687,5.44183891826343,921.963970588235));
#160930=CARTESIAN_POINT('Ctrl Pts',(14.4273846475923,4.10494485108125,920.469852941176));
#160931=CARTESIAN_POINT('Ctrl Pts',(14.8077638051159,2.76805078389905,918.975735294118));
#160932=CARTESIAN_POINT('Ctrl Pts',(14.9360126444255,1.38402539194953,917.481617647059));
#160933=CARTESIAN_POINT('Ctrl Pts',(15.0642614837351,2.76725994113625E-15,
915.9875));
#160934=CARTESIAN_POINT('Ctrl Pts',(14.9360126444255,-1.38402539194952,
914.493382352941));
#160935=CARTESIAN_POINT('Ctrl Pts',(14.8077638051159,-2.76805078389906,
912.999264705882));
#160936=CARTESIAN_POINT('Ctrl Pts',(14.4273846475923,-4.10494485108124,
911.505147058824));
#160937=CARTESIAN_POINT('Ctrl Pts',(14.0470054900687,-5.44183891826342,
910.011029411765));
#160938=CARTESIAN_POINT('Ctrl Pts',(13.4274493703259,-6.68607533664808,
908.516911764706));
#160939=CARTESIAN_POINT('Ctrl Pts',(12.8078932505832,-7.93031175503273,
907.022794117647));
#160940=CARTESIAN_POINT('Ctrl Pts',(11.9702584092036,-9.03951954568884,
905.528676470588));
#160941=CARTESIAN_POINT('Ctrl Pts',(11.132623567824,-10.148727336345,904.034558823529));
#160942=CARTESIAN_POINT('Ctrl Pts',(10.1054346546984,-11.0851337583099,
902.540441176471));
#160943=CARTESIAN_POINT('Ctrl Pts',(9.07824574157275,-12.0215401802748,
901.046323529412));
#160944=CARTESIAN_POINT('Ctrl Pts',(7.89648244316034,-12.7532570359442,
899.552205882353));
#160945=CARTESIAN_POINT('Ctrl Pts',(6.71471914474792,-13.4849738916136,
898.058088235294));
#160946=CARTESIAN_POINT('Ctrl Pts',(5.4186249928073,-13.9870834410653,896.563970588235));
#160947=CARTESIAN_POINT('Ctrl Pts',(4.12253084086667,-14.4891929905171,
895.069852941177));
#160948=CARTESIAN_POINT('Ctrl Pts',(2.75624276724855,-14.7445964952585,
893.575735294118));
#160949=CARTESIAN_POINT('Ctrl Pts',(1.38995469363045,-15.,892.081617647059));
#160950=CARTESIAN_POINT('Ctrl Pts',(0.,-15.,890.5875));
#160951=CARTESIAN_POINT('Ctrl Pts',(-1.38995469363045,-15.,889.093382352941));
#160952=CARTESIAN_POINT('Ctrl Pts',(-2.75624276724856,-14.7445964952585,
887.599264705882));
#160953=CARTESIAN_POINT('Ctrl Pts',(-4.12253084086666,-14.4891929905171,
886.105147058824));
#160954=CARTESIAN_POINT('Ctrl Pts',(-5.41862499280729,-13.9870834410653,
884.611029411765));
#160955=CARTESIAN_POINT('Ctrl Pts',(-6.71471914474793,-13.4849738916136,
883.116911764706));
#160956=CARTESIAN_POINT('Ctrl Pts',(-7.89648244316034,-12.7532570359442,
881.622794117647));
#160957=CARTESIAN_POINT('Ctrl Pts',(-9.07824574157275,-12.0215401802748,
880.128676470588));
#160958=CARTESIAN_POINT('Ctrl Pts',(-10.1054346546984,-11.0851337583099,
878.634558823529));
#160959=CARTESIAN_POINT('Ctrl Pts',(-11.132623567824,-10.148727336345,877.140441176471));
#160960=CARTESIAN_POINT('Ctrl Pts',(-11.9702584092036,-9.03951954568885,
875.646323529412));
#160961=CARTESIAN_POINT('Ctrl Pts',(-12.8078932505832,-7.93031175503273,
874.152205882353));
#160962=CARTESIAN_POINT('Ctrl Pts',(-13.4274493703259,-6.68607533664808,
872.658088235294));
#160963=CARTESIAN_POINT('Ctrl Pts',(-14.0470054900687,-5.44183891826343,
871.163970588236));
#160964=CARTESIAN_POINT('Ctrl Pts',(-14.4273846475923,-4.10494485108124,
869.669852941176));
#160965=CARTESIAN_POINT('Ctrl Pts',(-14.8077638051159,-2.76805078389906,
868.175735294118));
#160966=CARTESIAN_POINT('Ctrl Pts',(-14.9360126444255,-1.38402539194953,
866.681617647059));
#160967=CARTESIAN_POINT('Ctrl Pts',(-15.0642614837351,-9.22419980378748E-16,
865.1875));
#160968=CARTESIAN_POINT('Ctrl Pts',(-14.9360126444255,1.38402539194953,
863.693382352941));
#160969=CARTESIAN_POINT('Ctrl Pts',(-14.8077638051159,2.76805078389906,
862.199264705883));
#160970=CARTESIAN_POINT('Ctrl Pts',(-14.4273846475923,4.10494485108124,
860.705147058824));
#160971=CARTESIAN_POINT('Ctrl Pts',(-14.0470054900687,5.44183891826343,
859.211029411765));
#160972=CARTESIAN_POINT('Ctrl Pts',(-13.4274493703259,6.68607533664807,
857.716911764706));
#160973=CARTESIAN_POINT('Ctrl Pts',(-12.8078932505832,7.93031175503273,
856.222794117647));
#160974=CARTESIAN_POINT('Ctrl Pts',(-11.9702584092036,9.03951954568884,
854.728676470588));
#160975=CARTESIAN_POINT('Ctrl Pts',(-11.132623567824,10.148727336345,853.234558823529));
#160976=CARTESIAN_POINT('Ctrl Pts',(-10.1054346546984,11.0851337583099,
851.740441176471));
#160977=CARTESIAN_POINT('Ctrl Pts',(-9.07824574157275,12.0215401802748,
850.246323529412));
#160978=CARTESIAN_POINT('Ctrl Pts',(-7.89648244316034,12.7532570359442,
848.752205882353));
#160979=CARTESIAN_POINT('Ctrl Pts',(-6.71471914474793,13.4849738916136,
847.258088235294));
#160980=CARTESIAN_POINT('Ctrl Pts',(-5.41862499280729,13.9870834410653,
845.763970588235));
#160981=CARTESIAN_POINT('Ctrl Pts',(-4.12253084086667,14.4891929905171,
844.269852941177));
#160982=CARTESIAN_POINT('Ctrl Pts',(-2.75624276724856,14.7445964952585,
842.775735294118));
#160983=CARTESIAN_POINT('Ctrl Pts',(-1.38995469363044,15.,841.281617647059));
#160984=CARTESIAN_POINT('Ctrl Pts',(-1.83697019872103E-15,15.,839.7875));
#160985=CARTESIAN_POINT('Ctrl Pts',(1.38995469363045,15.,838.293382352941));
#160986=CARTESIAN_POINT('Ctrl Pts',(2.75624276724855,14.7445964952585,836.799264705882));
#160987=CARTESIAN_POINT('Ctrl Pts',(4.12253084086666,14.4891929905171,835.305147058824));
#160988=CARTESIAN_POINT('Ctrl Pts',(5.4186249928073,13.9870834410653,833.811029411765));
#160989=CARTESIAN_POINT('Ctrl Pts',(6.71471914474792,13.4849738916136,832.316911764706));
#160990=CARTESIAN_POINT('Ctrl Pts',(7.89648244316034,12.7532570359442,830.822794117647));
#160991=CARTESIAN_POINT('Ctrl Pts',(9.07824574157275,12.0215401802748,829.328676470588));
#160992=CARTESIAN_POINT('Ctrl Pts',(10.1054346546984,11.0851337583099,827.834558823529));
#160993=CARTESIAN_POINT('Ctrl Pts',(11.132623567824,10.148727336345,826.340441176471));
#160994=CARTESIAN_POINT('Ctrl Pts',(11.9702584092036,9.03951954568885,824.846323529412));
#160995=CARTESIAN_POINT('Ctrl Pts',(12.8078932505832,7.93031175503273,823.352205882353));
#160996=CARTESIAN_POINT('Ctrl Pts',(13.4274493703259,6.68607533664807,821.858088235294));
#160997=CARTESIAN_POINT('Ctrl Pts',(14.0470054900687,5.44183891826343,820.363970588236));
#160998=CARTESIAN_POINT('Ctrl Pts',(14.4273846475923,4.10494485108125,818.869852941177));
#160999=CARTESIAN_POINT('Ctrl Pts',(14.8077638051159,2.76805078389905,817.375735294118));
#161000=CARTESIAN_POINT('Ctrl Pts',(14.9360126444255,1.38402539194953,815.881617647059));
#161001=CARTESIAN_POINT('Ctrl Pts',(15.0642614837351,2.76725994113625E-15,
814.3875));
#161002=CARTESIAN_POINT('Ctrl Pts',(14.9360126444255,-1.38402539194952,
812.893382352941));
#161003=CARTESIAN_POINT('Ctrl Pts',(14.8077638051159,-2.76805078389906,
811.399264705883));
#161004=CARTESIAN_POINT('Ctrl Pts',(14.4273846475923,-4.10494485108124,
809.905147058824));
#161005=CARTESIAN_POINT('Ctrl Pts',(14.0470054900687,-5.44183891826342,
808.411029411765));
#161006=CARTESIAN_POINT('Ctrl Pts',(13.4274493703259,-6.68607533664808,
806.916911764706));
#161007=CARTESIAN_POINT('Ctrl Pts',(12.8078932505832,-7.93031175503273,
805.422794117647));
#161008=CARTESIAN_POINT('Ctrl Pts',(11.9702584092036,-9.03951954568884,
803.928676470588));
#161009=CARTESIAN_POINT('Ctrl Pts',(11.132623567824,-10.148727336345,802.434558823529));
#161010=CARTESIAN_POINT('Ctrl Pts',(10.1054346546984,-11.0851337583099,
800.940441176471));
#161011=CARTESIAN_POINT('Ctrl Pts',(9.07824574157275,-12.0215401802748,
799.446323529412));
#161012=CARTESIAN_POINT('Ctrl Pts',(7.89648244316034,-12.7532570359442,
797.952205882353));
#161013=CARTESIAN_POINT('Ctrl Pts',(6.71471914474792,-13.4849738916136,
796.458088235294));
#161014=CARTESIAN_POINT('Ctrl Pts',(5.4186249928073,-13.9870834410653,794.963970588235));
#161015=CARTESIAN_POINT('Ctrl Pts',(4.12253084086667,-14.4891929905171,
793.469852941176));
#161016=CARTESIAN_POINT('Ctrl Pts',(2.75624276724855,-14.7445964952585,
791.975735294118));
#161017=CARTESIAN_POINT('Ctrl Pts',(1.38995469363045,-15.,790.481617647059));
#161018=CARTESIAN_POINT('Ctrl Pts',(0.,-15.,788.9875));
#161019=CARTESIAN_POINT('Ctrl Pts',(-1.38995469363045,-15.,787.493382352941));
#161020=CARTESIAN_POINT('Ctrl Pts',(-2.75624276724856,-14.7445964952585,
785.999264705882));
#161021=CARTESIAN_POINT('Ctrl Pts',(-4.12253084086666,-14.4891929905171,
784.505147058824));
#161022=CARTESIAN_POINT('Ctrl Pts',(-5.41862499280729,-13.9870834410653,
783.011029411765));
#161023=CARTESIAN_POINT('Ctrl Pts',(-6.71471914474793,-13.4849738916136,
781.516911764706));
#161024=CARTESIAN_POINT('Ctrl Pts',(-7.89648244316034,-12.7532570359442,
780.022794117647));
#161025=CARTESIAN_POINT('Ctrl Pts',(-9.07824574157275,-12.0215401802748,
778.528676470588));
#161026=CARTESIAN_POINT('Ctrl Pts',(-10.1054346546984,-11.0851337583099,
777.03455882353));
#161027=CARTESIAN_POINT('Ctrl Pts',(-11.132623567824,-10.148727336345,775.540441176471));
#161028=CARTESIAN_POINT('Ctrl Pts',(-11.9702584092036,-9.03951954568885,
774.046323529412));
#161029=CARTESIAN_POINT('Ctrl Pts',(-12.8078932505832,-7.93031175503273,
772.552205882353));
#161030=CARTESIAN_POINT('Ctrl Pts',(-13.4274493703259,-6.68607533664808,
771.058088235294));
#161031=CARTESIAN_POINT('Ctrl Pts',(-14.0470054900687,-5.44183891826343,
769.563970588235));
#161032=CARTESIAN_POINT('Ctrl Pts',(-14.4273846475923,-4.10494485108124,
768.069852941177));
#161033=CARTESIAN_POINT('Ctrl Pts',(-14.8077638051159,-2.76805078389906,
766.575735294118));
#161034=CARTESIAN_POINT('Ctrl Pts',(-14.9360126444255,-1.38402539194953,
765.081617647059));
#161035=CARTESIAN_POINT('Ctrl Pts',(-15.0642614837351,-9.22419980378748E-16,
763.5875));
#161036=CARTESIAN_POINT('Ctrl Pts',(-14.9360126444255,1.38402539194953,
762.093382352941));
#161037=CARTESIAN_POINT('Ctrl Pts',(-14.8077638051159,2.76805078389906,
760.599264705883));
#161038=CARTESIAN_POINT('Ctrl Pts',(-14.4273846475923,4.10494485108124,
759.105147058824));
#161039=CARTESIAN_POINT('Ctrl Pts',(-14.0470054900687,5.44183891826343,
757.611029411765));
#161040=CARTESIAN_POINT('Ctrl Pts',(-13.4274493703259,6.68607533664807,
756.116911764706));
#161041=CARTESIAN_POINT('Ctrl Pts',(-12.8078932505832,7.93031175503273,
754.622794117647));
#161042=CARTESIAN_POINT('Ctrl Pts',(-11.9702584092036,9.03951954568884,
753.128676470588));
#161043=CARTESIAN_POINT('Ctrl Pts',(-11.132623567824,10.148727336345,751.634558823529));
#161044=CARTESIAN_POINT('Ctrl Pts',(-10.1054346546984,11.0851337583099,
750.140441176471));
#161045=CARTESIAN_POINT('Ctrl Pts',(-9.07824574157275,12.0215401802748,
748.646323529412));
#161046=CARTESIAN_POINT('Ctrl Pts',(-7.89648244316034,12.7532570359442,
747.152205882353));
#161047=CARTESIAN_POINT('Ctrl Pts',(-6.71471914474793,13.4849738916136,
745.658088235294));
#161048=CARTESIAN_POINT('Ctrl Pts',(-5.41862499280729,13.9870834410653,
744.163970588235));
#161049=CARTESIAN_POINT('Ctrl Pts',(-4.12253084086667,14.4891929905171,
742.669852941176));
#161050=CARTESIAN_POINT('Ctrl Pts',(-2.75624276724856,14.7445964952585,
741.175735294118));
#161051=CARTESIAN_POINT('Ctrl Pts',(-1.38995469363044,15.,739.681617647059));
#161052=CARTESIAN_POINT('Ctrl Pts',(-1.83697019872103E-15,15.,738.1875));
#161053=CARTESIAN_POINT('Ctrl Pts',(1.38995469363045,15.,736.693382352941));
#161054=CARTESIAN_POINT('Ctrl Pts',(2.75624276724855,14.7445964952585,735.199264705882));
#161055=CARTESIAN_POINT('Ctrl Pts',(4.12253084086666,14.4891929905171,733.705147058824));
#161056=CARTESIAN_POINT('Ctrl Pts',(5.4186249928073,13.9870834410653,732.211029411765));
#161057=CARTESIAN_POINT('Ctrl Pts',(6.71471914474792,13.4849738916136,730.716911764706));
#161058=CARTESIAN_POINT('Ctrl Pts',(7.89648244316034,12.7532570359442,729.222794117647));
#161059=CARTESIAN_POINT('Ctrl Pts',(9.07824574157275,12.0215401802748,727.728676470588));
#161060=CARTESIAN_POINT('Ctrl Pts',(10.1054346546984,11.0851337583099,726.234558823529));
#161061=CARTESIAN_POINT('Ctrl Pts',(11.132623567824,10.148727336345,724.740441176471));
#161062=CARTESIAN_POINT('Ctrl Pts',(11.9702584092036,9.03951954568885,723.246323529412));
#161063=CARTESIAN_POINT('Ctrl Pts',(12.8078932505832,7.93031175503273,721.752205882353));
#161064=CARTESIAN_POINT('Ctrl Pts',(13.4274493703259,6.68607533664807,720.258088235294));
#161065=CARTESIAN_POINT('Ctrl Pts',(14.0470054900687,5.44183891826343,718.763970588235));
#161066=CARTESIAN_POINT('Ctrl Pts',(14.4273846475923,4.10494485108125,717.269852941177));
#161067=CARTESIAN_POINT('Ctrl Pts',(14.8077638051159,2.76805078389905,715.775735294118));
#161068=CARTESIAN_POINT('Ctrl Pts',(14.9360126444255,1.38402539194953,714.281617647059));
#161069=CARTESIAN_POINT('Ctrl Pts',(15.0642614837351,2.76725994113625E-15,
712.7875));
#161070=CARTESIAN_POINT('Ctrl Pts',(14.9360126444255,-1.38402539194952,
711.293382352941));
#161071=CARTESIAN_POINT('Ctrl Pts',(14.8077638051159,-2.76805078389906,
709.799264705883));
#161072=CARTESIAN_POINT('Ctrl Pts',(14.4273846475923,-4.10494485108124,
708.305147058824));
#161073=CARTESIAN_POINT('Ctrl Pts',(14.0470054900687,-5.44183891826342,
706.811029411765));
#161074=CARTESIAN_POINT('Ctrl Pts',(13.4274493703259,-6.68607533664808,
705.316911764706));
#161075=CARTESIAN_POINT('Ctrl Pts',(12.8078932505832,-7.93031175503273,
703.822794117647));
#161076=CARTESIAN_POINT('Ctrl Pts',(11.9702584092036,-9.03951954568884,
702.328676470588));
#161077=CARTESIAN_POINT('Ctrl Pts',(11.132623567824,-10.148727336345,700.83455882353));
#161078=CARTESIAN_POINT('Ctrl Pts',(10.1054346546984,-11.0851337583099,
699.340441176471));
#161079=CARTESIAN_POINT('Ctrl Pts',(9.07824574157275,-12.0215401802748,
697.846323529412));
#161080=CARTESIAN_POINT('Ctrl Pts',(7.89648244316034,-12.7532570359442,
696.352205882353));
#161081=CARTESIAN_POINT('Ctrl Pts',(6.71471914474792,-13.4849738916136,
694.858088235294));
#161082=CARTESIAN_POINT('Ctrl Pts',(5.4186249928073,-13.9870834410653,693.363970588235));
#161083=CARTESIAN_POINT('Ctrl Pts',(4.12253084086667,-14.4891929905171,
691.869852941177));
#161084=CARTESIAN_POINT('Ctrl Pts',(2.75624276724855,-14.7445964952585,
690.375735294118));
#161085=CARTESIAN_POINT('Ctrl Pts',(1.38995469363045,-15.,688.881617647059));
#161086=CARTESIAN_POINT('Ctrl Pts',(0.,-15.,687.3875));
#161087=CARTESIAN_POINT('Ctrl Pts',(-1.38995469363045,-15.,685.893382352941));
#161088=CARTESIAN_POINT('Ctrl Pts',(-2.75624276724856,-14.7445964952585,
684.399264705883));
#161089=CARTESIAN_POINT('Ctrl Pts',(-4.12253084086666,-14.4891929905171,
682.905147058824));
#161090=CARTESIAN_POINT('Ctrl Pts',(-5.41862499280729,-13.9870834410653,
681.411029411765));
#161091=CARTESIAN_POINT('Ctrl Pts',(-6.71471914474793,-13.4849738916136,
679.916911764706));
#161092=CARTESIAN_POINT('Ctrl Pts',(-7.89648244316034,-12.7532570359442,
678.422794117647));
#161093=CARTESIAN_POINT('Ctrl Pts',(-9.07824574157275,-12.0215401802748,
676.928676470588));
#161094=CARTESIAN_POINT('Ctrl Pts',(-10.1054346546984,-11.0851337583099,
675.434558823529));
#161095=CARTESIAN_POINT('Ctrl Pts',(-11.132623567824,-10.148727336345,673.940441176471));
#161096=CARTESIAN_POINT('Ctrl Pts',(-11.9702584092036,-9.03951954568885,
672.446323529412));
#161097=CARTESIAN_POINT('Ctrl Pts',(-12.8078932505832,-7.93031175503273,
670.952205882353));
#161098=CARTESIAN_POINT('Ctrl Pts',(-13.4274493703259,-6.68607533664808,
669.458088235294));
#161099=CARTESIAN_POINT('Ctrl Pts',(-14.0470054900687,-5.44183891826343,
667.963970588235));
#161100=CARTESIAN_POINT('Ctrl Pts',(-14.4273846475923,-4.10494485108124,
666.469852941176));
#161101=CARTESIAN_POINT('Ctrl Pts',(-14.8077638051159,-2.76805078389906,
664.975735294118));
#161102=CARTESIAN_POINT('Ctrl Pts',(-14.9360126444255,-1.38402539194953,
663.481617647059));
#161103=CARTESIAN_POINT('Ctrl Pts',(-15.0642614837351,-9.22419980378748E-16,
661.9875));
#161104=CARTESIAN_POINT('Ctrl Pts',(-14.9360126444255,1.38402539194953,
660.493382352941));
#161105=CARTESIAN_POINT('Ctrl Pts',(-14.8077638051159,2.76805078389906,
658.999264705882));
#161106=CARTESIAN_POINT('Ctrl Pts',(-14.4273846475923,4.10494485108124,
657.505147058824));
#161107=CARTESIAN_POINT('Ctrl Pts',(-14.0470054900687,5.44183891826343,
656.011029411765));
#161108=CARTESIAN_POINT('Ctrl Pts',(-13.4274493703259,6.68607533664807,
654.516911764706));
#161109=CARTESIAN_POINT('Ctrl Pts',(-12.8078932505832,7.93031175503273,
653.022794117647));
#161110=CARTESIAN_POINT('Ctrl Pts',(-11.9702584092036,9.03951954568884,
651.528676470588));
#161111=CARTESIAN_POINT('Ctrl Pts',(-11.132623567824,10.148727336345,650.03455882353));
#161112=CARTESIAN_POINT('Ctrl Pts',(-10.1054346546984,11.0851337583099,
648.540441176471));
#161113=CARTESIAN_POINT('Ctrl Pts',(-9.07824574157275,12.0215401802748,
647.046323529412));
#161114=CARTESIAN_POINT('Ctrl Pts',(-7.89648244316034,12.7532570359442,
645.552205882353));
#161115=CARTESIAN_POINT('Ctrl Pts',(-6.71471914474793,13.4849738916136,
644.058088235294));
#161116=CARTESIAN_POINT('Ctrl Pts',(-5.41862499280729,13.9870834410653,
642.563970588235));
#161117=CARTESIAN_POINT('Ctrl Pts',(-4.12253084086667,14.4891929905171,
641.069852941176));
#161118=CARTESIAN_POINT('Ctrl Pts',(-2.75624276724856,14.7445964952585,
639.575735294118));
#161119=CARTESIAN_POINT('Ctrl Pts',(-1.38995469363044,15.,638.081617647059));
#161120=CARTESIAN_POINT('Ctrl Pts',(-1.83697019872103E-15,15.,636.5875));
#161121=CARTESIAN_POINT('Ctrl Pts',(1.38995469363045,15.,635.093382352941));
#161122=CARTESIAN_POINT('Ctrl Pts',(2.75624276724855,14.7445964952585,633.599264705882));
#161123=CARTESIAN_POINT('Ctrl Pts',(4.12253084086666,14.4891929905171,632.105147058824));
#161124=CARTESIAN_POINT('Ctrl Pts',(5.4186249928073,13.9870834410653,630.611029411765));
#161125=CARTESIAN_POINT('Ctrl Pts',(6.71471914474792,13.4849738916136,629.116911764706));
#161126=CARTESIAN_POINT('Ctrl Pts',(7.89648244316034,12.7532570359442,627.622794117647));
#161127=CARTESIAN_POINT('Ctrl Pts',(9.07824574157275,12.0215401802748,626.128676470588));
#161128=CARTESIAN_POINT('Ctrl Pts',(10.1054346546984,11.0851337583099,624.634558823529));
#161129=CARTESIAN_POINT('Ctrl Pts',(11.132623567824,10.148727336345,623.140441176471));
#161130=CARTESIAN_POINT('Ctrl Pts',(11.9702584092036,9.03951954568885,621.646323529412));
#161131=CARTESIAN_POINT('Ctrl Pts',(12.8078932505832,7.93031175503273,620.152205882353));
#161132=CARTESIAN_POINT('Ctrl Pts',(13.4274493703259,6.68607533664807,618.658088235294));
#161133=CARTESIAN_POINT('Ctrl Pts',(14.0470054900687,5.44183891826343,617.163970588235));
#161134=CARTESIAN_POINT('Ctrl Pts',(14.4273846475923,4.10494485108125,615.669852941176));
#161135=CARTESIAN_POINT('Ctrl Pts',(14.8077638051159,2.76805078389905,614.175735294118));
#161136=CARTESIAN_POINT('Ctrl Pts',(14.9360126444255,1.38402539194953,612.681617647059));
#161137=CARTESIAN_POINT('Ctrl Pts',(15.0642614837351,2.76725994113625E-15,
611.1875));
#161138=CARTESIAN_POINT('Ctrl Pts',(14.9360126444255,-1.38402539194952,
609.693382352941));
#161139=CARTESIAN_POINT('Ctrl Pts',(14.8077638051159,-2.76805078389906,
608.199264705882));
#161140=CARTESIAN_POINT('Ctrl Pts',(14.4273846475923,-4.10494485108124,
606.705147058824));
#161141=CARTESIAN_POINT('Ctrl Pts',(14.0470054900687,-5.44183891826342,
605.211029411765));
#161142=CARTESIAN_POINT('Ctrl Pts',(13.4274493703259,-6.68607533664808,
603.716911764706));
#161143=CARTESIAN_POINT('Ctrl Pts',(12.8078932505832,-7.93031175503273,
602.222794117647));
#161144=CARTESIAN_POINT('Ctrl Pts',(11.9702584092036,-9.03951954568884,
600.728676470588));
#161145=CARTESIAN_POINT('Ctrl Pts',(11.132623567824,-10.148727336345,599.23455882353));
#161146=CARTESIAN_POINT('Ctrl Pts',(10.1054346546984,-11.0851337583099,
597.740441176471));
#161147=CARTESIAN_POINT('Ctrl Pts',(9.07824574157275,-12.0215401802748,
596.246323529412));
#161148=CARTESIAN_POINT('Ctrl Pts',(7.89648244316034,-12.7532570359442,
594.752205882353));
#161149=CARTESIAN_POINT('Ctrl Pts',(6.71471914474792,-13.4849738916136,
593.258088235294));
#161150=CARTESIAN_POINT('Ctrl Pts',(5.4186249928073,-13.9870834410653,591.763970588235));
#161151=CARTESIAN_POINT('Ctrl Pts',(4.12253084086667,-14.4891929905171,
590.269852941177));
#161152=CARTESIAN_POINT('Ctrl Pts',(2.75624276724855,-14.7445964952585,
588.775735294118));
#161153=CARTESIAN_POINT('Ctrl Pts',(1.38995469363045,-15.,587.281617647059));
#161154=CARTESIAN_POINT('Ctrl Pts',(0.,-15.,585.7875));
#161155=CARTESIAN_POINT('Ctrl Pts',(-1.38995469363045,-15.,584.293382352941));
#161156=CARTESIAN_POINT('Ctrl Pts',(-2.75624276724856,-14.7445964952585,
582.799264705882));
#161157=CARTESIAN_POINT('Ctrl Pts',(-4.12253084086666,-14.4891929905171,
581.305147058824));
#161158=CARTESIAN_POINT('Ctrl Pts',(-5.41862499280729,-13.9870834410653,
579.811029411765));
#161159=CARTESIAN_POINT('Ctrl Pts',(-6.71471914474793,-13.4849738916136,
578.316911764706));
#161160=CARTESIAN_POINT('Ctrl Pts',(-7.89648244316034,-12.7532570359442,
576.822794117647));
#161161=CARTESIAN_POINT('Ctrl Pts',(-9.07824574157275,-12.0215401802748,
575.328676470588));
#161162=CARTESIAN_POINT('Ctrl Pts',(-10.1054346546984,-11.0851337583099,
573.834558823529));
#161163=CARTESIAN_POINT('Ctrl Pts',(-11.132623567824,-10.148727336345,572.340441176471));
#161164=CARTESIAN_POINT('Ctrl Pts',(-11.9702584092036,-9.03951954568885,
570.846323529412));
#161165=CARTESIAN_POINT('Ctrl Pts',(-12.8078932505832,-7.93031175503273,
569.352205882353));
#161166=CARTESIAN_POINT('Ctrl Pts',(-13.4274493703259,-6.68607533664808,
567.858088235294));
#161167=CARTESIAN_POINT('Ctrl Pts',(-14.0470054900687,-5.44183891826343,
566.363970588235));
#161168=CARTESIAN_POINT('Ctrl Pts',(-14.4273846475923,-4.10494485108124,
564.869852941177));
#161169=CARTESIAN_POINT('Ctrl Pts',(-14.8077638051159,-2.76805078389906,
563.375735294118));
#161170=CARTESIAN_POINT('Ctrl Pts',(-14.9360126444255,-1.38402539194953,
561.881617647059));
#161171=CARTESIAN_POINT('Ctrl Pts',(-15.0642614837351,-9.22419980378748E-16,
560.3875));
#161172=CARTESIAN_POINT('Ctrl Pts',(-14.9360126444255,1.38402539194953,
558.893382352941));
#161173=CARTESIAN_POINT('Ctrl Pts',(-14.8077638051159,2.76805078389906,
557.399264705882));
#161174=CARTESIAN_POINT('Ctrl Pts',(-14.4273846475923,4.10494485108124,
555.905147058824));
#161175=CARTESIAN_POINT('Ctrl Pts',(-14.0470054900687,5.44183891826343,
554.411029411765));
#161176=CARTESIAN_POINT('Ctrl Pts',(-13.4274493703259,6.68607533664807,
552.916911764706));
#161177=CARTESIAN_POINT('Ctrl Pts',(-12.8078932505832,7.93031175503273,
551.422794117647));
#161178=CARTESIAN_POINT('Ctrl Pts',(-11.9702584092036,9.03951954568884,
549.928676470588));
#161179=CARTESIAN_POINT('Ctrl Pts',(-11.132623567824,10.148727336345,548.43455882353));
#161180=CARTESIAN_POINT('Ctrl Pts',(-10.1054346546984,11.0851337583099,
546.940441176471));
#161181=CARTESIAN_POINT('Ctrl Pts',(-9.07824574157275,12.0215401802748,
545.446323529412));
#161182=CARTESIAN_POINT('Ctrl Pts',(-7.89648244316034,12.7532570359442,
543.952205882353));
#161183=CARTESIAN_POINT('Ctrl Pts',(-6.71471914474793,13.4849738916136,
542.458088235294));
#161184=CARTESIAN_POINT('Ctrl Pts',(-5.41862499280729,13.9870834410653,
540.963970588235));
#161185=CARTESIAN_POINT('Ctrl Pts',(-4.12253084086667,14.4891929905171,
539.469852941177));
#161186=CARTESIAN_POINT('Ctrl Pts',(-2.75624276724856,14.7445964952585,
537.975735294118));
#161187=CARTESIAN_POINT('Ctrl Pts',(-1.38995469363044,15.,536.481617647059));
#161188=CARTESIAN_POINT('Ctrl Pts',(-1.83697019872103E-15,15.,534.9875));
#161189=CARTESIAN_POINT('Ctrl Pts',(1.38995469363045,15.,533.493382352941));
#161190=CARTESIAN_POINT('Ctrl Pts',(2.75624276724855,14.7445964952585,531.999264705882));
#161191=CARTESIAN_POINT('Ctrl Pts',(4.12253084086666,14.4891929905171,530.505147058824));
#161192=CARTESIAN_POINT('Ctrl Pts',(5.4186249928073,13.9870834410653,529.011029411765));
#161193=CARTESIAN_POINT('Ctrl Pts',(6.71471914474792,13.4849738916136,527.516911764706));
#161194=CARTESIAN_POINT('Ctrl Pts',(7.89648244316034,12.7532570359442,526.022794117647));
#161195=CARTESIAN_POINT('Ctrl Pts',(9.07824574157275,12.0215401802748,524.528676470588));
#161196=CARTESIAN_POINT('Ctrl Pts',(10.1054346546984,11.0851337583099,523.03455882353));
#161197=CARTESIAN_POINT('Ctrl Pts',(11.132623567824,10.148727336345,521.540441176471));
#161198=CARTESIAN_POINT('Ctrl Pts',(11.9702584092036,9.03951954568885,520.046323529412));
#161199=CARTESIAN_POINT('Ctrl Pts',(12.8078932505832,7.93031175503273,518.552205882353));
#161200=CARTESIAN_POINT('Ctrl Pts',(13.4274493703259,6.68607533664807,517.058088235294));
#161201=CARTESIAN_POINT('Ctrl Pts',(14.0470054900687,5.44183891826343,515.563970588235));
#161202=CARTESIAN_POINT('Ctrl Pts',(14.4273846475923,4.10494485108125,514.069852941176));
#161203=CARTESIAN_POINT('Ctrl Pts',(14.8077638051159,2.76805078389905,512.575735294118));
#161204=CARTESIAN_POINT('Ctrl Pts',(14.9360126444255,1.38402539194953,511.081617647059));
#161205=CARTESIAN_POINT('Ctrl Pts',(15.0642614837351,2.76725994113625E-15,
509.5875));
#161206=CARTESIAN_POINT('Ctrl Pts',(14.9360126444255,-1.38402539194952,
508.093382352941));
#161207=CARTESIAN_POINT('Ctrl Pts',(14.8077638051159,-2.76805078389906,
506.599264705882));
#161208=CARTESIAN_POINT('Ctrl Pts',(14.4273846475923,-4.10494485108124,
505.105147058824));
#161209=CARTESIAN_POINT('Ctrl Pts',(14.0470054900687,-5.44183891826342,
503.611029411765));
#161210=CARTESIAN_POINT('Ctrl Pts',(13.4274493703259,-6.68607533664808,
502.116911764706));
#161211=CARTESIAN_POINT('Ctrl Pts',(12.8078932505832,-7.93031175503273,
500.622794117647));
#161212=CARTESIAN_POINT('Ctrl Pts',(11.9702584092036,-9.03951954568884,
499.128676470588));
#161213=CARTESIAN_POINT('Ctrl Pts',(11.132623567824,-10.148727336345,497.63455882353));
#161214=CARTESIAN_POINT('Ctrl Pts',(10.1054346546984,-11.0851337583099,
496.140441176471));
#161215=CARTESIAN_POINT('Ctrl Pts',(9.07824574157275,-12.0215401802748,
494.646323529412));
#161216=CARTESIAN_POINT('Ctrl Pts',(7.89648244316034,-12.7532570359442,
493.152205882353));
#161217=CARTESIAN_POINT('Ctrl Pts',(6.71471914474792,-13.4849738916136,
491.658088235294));
#161218=CARTESIAN_POINT('Ctrl Pts',(5.4186249928073,-13.9870834410653,490.163970588235));
#161219=CARTESIAN_POINT('Ctrl Pts',(4.12253084086667,-14.4891929905171,
488.669852941177));
#161220=CARTESIAN_POINT('Ctrl Pts',(2.75624276724855,-14.7445964952585,
487.175735294118));
#161221=CARTESIAN_POINT('Ctrl Pts',(1.38995469363045,-15.,485.681617647059));
#161222=CARTESIAN_POINT('Ctrl Pts',(0.,-15.,484.1875));
#161223=CARTESIAN_POINT('Ctrl Pts',(-1.38995469363045,-15.,482.693382352941));
#161224=CARTESIAN_POINT('Ctrl Pts',(-2.75624276724856,-14.7445964952585,
481.199264705882));
#161225=CARTESIAN_POINT('Ctrl Pts',(-4.12253084086666,-14.4891929905171,
479.705147058824));
#161226=CARTESIAN_POINT('Ctrl Pts',(-5.41862499280729,-13.9870834410653,
478.211029411765));
#161227=CARTESIAN_POINT('Ctrl Pts',(-6.71471914474793,-13.4849738916136,
476.716911764706));
#161228=CARTESIAN_POINT('Ctrl Pts',(-7.89648244316034,-12.7532570359442,
475.222794117647));
#161229=CARTESIAN_POINT('Ctrl Pts',(-9.07824574157275,-12.0215401802748,
473.728676470588));
#161230=CARTESIAN_POINT('Ctrl Pts',(-10.1054346546984,-11.0851337583099,
472.234558823529));
#161231=CARTESIAN_POINT('Ctrl Pts',(-11.132623567824,-10.148727336345,470.740441176471));
#161232=CARTESIAN_POINT('Ctrl Pts',(-11.9702584092036,-9.03951954568885,
469.246323529412));
#161233=CARTESIAN_POINT('Ctrl Pts',(-12.8078932505832,-7.93031175503273,
467.752205882353));
#161234=CARTESIAN_POINT('Ctrl Pts',(-13.4274493703259,-6.68607533664808,
466.258088235294));
#161235=CARTESIAN_POINT('Ctrl Pts',(-14.0470054900687,-5.44183891826343,
464.763970588236));
#161236=CARTESIAN_POINT('Ctrl Pts',(-14.4273846475923,-4.10494485108124,
463.269852941177));
#161237=CARTESIAN_POINT('Ctrl Pts',(-14.8077638051159,-2.76805078389906,
461.775735294118));
#161238=CARTESIAN_POINT('Ctrl Pts',(-14.9360126444255,-1.38402539194953,
460.281617647059));
#161239=CARTESIAN_POINT('Ctrl Pts',(-15.0642614837351,-9.22419980378748E-16,
458.7875));
#161240=CARTESIAN_POINT('Ctrl Pts',(-14.9360126444255,1.38402539194953,
457.293382352941));
#161241=CARTESIAN_POINT('Ctrl Pts',(-14.8077638051159,2.76805078389906,
455.799264705882));
#161242=CARTESIAN_POINT('Ctrl Pts',(-14.4273846475923,4.10494485108124,
454.305147058824));
#161243=CARTESIAN_POINT('Ctrl Pts',(-14.0470054900687,5.44183891826343,
452.811029411765));
#161244=CARTESIAN_POINT('Ctrl Pts',(-13.4274493703259,6.68607533664807,
451.316911764706));
#161245=CARTESIAN_POINT('Ctrl Pts',(-12.8078932505832,7.93031175503273,
449.822794117647));
#161246=CARTESIAN_POINT('Ctrl Pts',(-11.9702584092036,9.03951954568884,
448.328676470588));
#161247=CARTESIAN_POINT('Ctrl Pts',(-11.132623567824,10.148727336345,446.83455882353));
#161248=CARTESIAN_POINT('Ctrl Pts',(-10.1054346546984,11.0851337583099,
445.340441176471));
#161249=CARTESIAN_POINT('Ctrl Pts',(-9.07824574157275,12.0215401802748,
443.846323529412));
#161250=CARTESIAN_POINT('Ctrl Pts',(-7.89648244316034,12.7532570359442,
442.352205882353));
#161251=CARTESIAN_POINT('Ctrl Pts',(-6.71471914474793,13.4849738916136,
440.858088235294));
#161252=CARTESIAN_POINT('Ctrl Pts',(-5.41862499280729,13.9870834410653,
439.363970588235));
#161253=CARTESIAN_POINT('Ctrl Pts',(-4.12253084086667,14.4891929905171,
437.869852941176));
#161254=CARTESIAN_POINT('Ctrl Pts',(-2.75624276724856,14.7445964952585,
436.375735294118));
#161255=CARTESIAN_POINT('Ctrl Pts',(-1.38995469363044,15.,434.881617647059));
#161256=CARTESIAN_POINT('Ctrl Pts',(-1.83697019872103E-15,15.,433.3875));
#161257=CARTESIAN_POINT('Ctrl Pts',(1.38995469363045,15.,431.893382352941));
#161258=CARTESIAN_POINT('Ctrl Pts',(2.75624276724855,14.7445964952585,430.399264705882));
#161259=CARTESIAN_POINT('Ctrl Pts',(4.12253084086666,14.4891929905171,428.905147058824));
#161260=CARTESIAN_POINT('Ctrl Pts',(5.4186249928073,13.9870834410653,427.411029411765));
#161261=CARTESIAN_POINT('Ctrl Pts',(6.71471914474792,13.4849738916136,425.916911764706));
#161262=CARTESIAN_POINT('Ctrl Pts',(7.89648244316034,12.7532570359442,424.422794117647));
#161263=CARTESIAN_POINT('Ctrl Pts',(9.07824574157275,12.0215401802748,422.928676470588));
#161264=CARTESIAN_POINT('Ctrl Pts',(10.1054346546984,11.0851337583099,421.43455882353));
#161265=CARTESIAN_POINT('Ctrl Pts',(11.132623567824,10.148727336345,419.940441176471));
#161266=CARTESIAN_POINT('Ctrl Pts',(11.9702584092036,9.03951954568885,418.446323529412));
#161267=CARTESIAN_POINT('Ctrl Pts',(12.8078932505832,7.93031175503273,416.952205882353));
#161268=CARTESIAN_POINT('Ctrl Pts',(13.4274493703259,6.68607533664807,415.458088235294));
#161269=CARTESIAN_POINT('Ctrl Pts',(14.0470054900687,5.44183891826343,413.963970588235));
#161270=CARTESIAN_POINT('Ctrl Pts',(14.4273846475923,4.10494485108125,412.469852941177));
#161271=CARTESIAN_POINT('Ctrl Pts',(14.8077638051159,2.76805078389905,410.975735294118));
#161272=CARTESIAN_POINT('Ctrl Pts',(14.9360126444255,1.38402539194953,409.481617647059));
#161273=CARTESIAN_POINT('Ctrl Pts',(15.0642614837351,2.76725994113625E-15,
407.9875));
#161274=CARTESIAN_POINT('Ctrl Pts',(14.9360126444255,-1.38402539194952,
406.493382352941));
#161275=CARTESIAN_POINT('Ctrl Pts',(14.8077638051159,-2.76805078389906,
404.999264705882));
#161276=CARTESIAN_POINT('Ctrl Pts',(14.4273846475923,-4.10494485108124,
403.505147058824));
#161277=CARTESIAN_POINT('Ctrl Pts',(14.0470054900687,-5.44183891826342,
402.011029411765));
#161278=CARTESIAN_POINT('Ctrl Pts',(13.4274493703259,-6.68607533664808,
400.516911764706));
#161279=CARTESIAN_POINT('Ctrl Pts',(12.8078932505832,-7.93031175503273,
399.022794117647));
#161280=CARTESIAN_POINT('Ctrl Pts',(11.9702584092036,-9.03951954568884,
397.528676470588));
#161281=CARTESIAN_POINT('Ctrl Pts',(11.132623567824,-10.148727336345,396.034558823529));
#161282=CARTESIAN_POINT('Ctrl Pts',(10.1054346546984,-11.0851337583099,
394.540441176471));
#161283=CARTESIAN_POINT('Ctrl Pts',(9.07824574157275,-12.0215401802748,
393.046323529412));
#161284=CARTESIAN_POINT('Ctrl Pts',(7.89648244316034,-12.7532570359442,
391.552205882353));
#161285=CARTESIAN_POINT('Ctrl Pts',(6.71471914474792,-13.4849738916136,
390.058088235294));
#161286=CARTESIAN_POINT('Ctrl Pts',(5.4186249928073,-13.9870834410653,388.563970588235));
#161287=CARTESIAN_POINT('Ctrl Pts',(4.12253084086667,-14.4891929905171,
387.069852941177));
#161288=CARTESIAN_POINT('Ctrl Pts',(2.75624276724855,-14.7445964952585,
385.575735294118));
#161289=CARTESIAN_POINT('Ctrl Pts',(1.38995469363045,-15.,384.081617647059));
#161290=CARTESIAN_POINT('Ctrl Pts',(0.,-15.,382.5875));
#161291=CARTESIAN_POINT('Ctrl Pts',(-1.38995469363045,-15.,381.093382352941));
#161292=CARTESIAN_POINT('Ctrl Pts',(-2.75624276724856,-14.7445964952585,
379.599264705882));
#161293=CARTESIAN_POINT('Ctrl Pts',(-4.12253084086666,-14.4891929905171,
378.105147058823));
#161294=CARTESIAN_POINT('Ctrl Pts',(-5.41862499280729,-13.9870834410653,
376.611029411765));
#161295=CARTESIAN_POINT('Ctrl Pts',(-6.71471914474793,-13.4849738916136,
375.116911764706));
#161296=CARTESIAN_POINT('Ctrl Pts',(-7.89648244316034,-12.7532570359442,
373.622794117647));
#161297=CARTESIAN_POINT('Ctrl Pts',(-9.07824574157275,-12.0215401802748,
372.128676470588));
#161298=CARTESIAN_POINT('Ctrl Pts',(-10.1054346546984,-11.0851337583099,
370.634558823529));
#161299=CARTESIAN_POINT('Ctrl Pts',(-11.132623567824,-10.148727336345,369.140441176471));
#161300=CARTESIAN_POINT('Ctrl Pts',(-11.9702584092036,-9.03951954568885,
367.646323529412));
#161301=CARTESIAN_POINT('Ctrl Pts',(-12.8078932505832,-7.93031175503273,
366.152205882353));
#161302=CARTESIAN_POINT('Ctrl Pts',(-13.4274493703259,-6.68607533664808,
364.658088235294));
#161303=CARTESIAN_POINT('Ctrl Pts',(-14.0470054900687,-5.44183891826343,
363.163970588235));
#161304=CARTESIAN_POINT('Ctrl Pts',(-14.4273846475923,-4.10494485108124,
361.669852941177));
#161305=CARTESIAN_POINT('Ctrl Pts',(-14.8077638051159,-2.76805078389906,
360.175735294118));
#161306=CARTESIAN_POINT('Ctrl Pts',(-14.9360126444255,-1.38402539194953,
358.681617647059));
#161307=CARTESIAN_POINT('Ctrl Pts',(-15.0642614837351,-9.22419980378748E-16,
357.1875));
#161308=CARTESIAN_POINT('Ctrl Pts',(-14.9360126444255,1.38402539194953,
355.693382352941));
#161309=CARTESIAN_POINT('Ctrl Pts',(-14.8077638051159,2.76805078389906,
354.199264705883));
#161310=CARTESIAN_POINT('Ctrl Pts',(-14.4273846475923,4.10494485108124,
352.705147058824));
#161311=CARTESIAN_POINT('Ctrl Pts',(-14.0470054900687,5.44183891826343,
351.211029411765));
#161312=CARTESIAN_POINT('Ctrl Pts',(-13.4274493703259,6.68607533664807,
349.716911764706));
#161313=CARTESIAN_POINT('Ctrl Pts',(-12.8078932505832,7.93031175503273,
348.222794117647));
#161314=CARTESIAN_POINT('Ctrl Pts',(-11.9702584092036,9.03951954568884,
346.728676470588));
#161315=CARTESIAN_POINT('Ctrl Pts',(-11.132623567824,10.148727336345,345.234558823529));
#161316=CARTESIAN_POINT('Ctrl Pts',(-10.1054346546984,11.0851337583099,
343.740441176471));
#161317=CARTESIAN_POINT('Ctrl Pts',(-9.07824574157275,12.0215401802748,
342.246323529412));
#161318=CARTESIAN_POINT('Ctrl Pts',(-7.89648244316034,12.7532570359442,
340.752205882353));
#161319=CARTESIAN_POINT('Ctrl Pts',(-6.71471914474793,13.4849738916136,
339.258088235294));
#161320=CARTESIAN_POINT('Ctrl Pts',(-5.41862499280729,13.9870834410653,
337.763970588235));
#161321=CARTESIAN_POINT('Ctrl Pts',(-4.12253084086667,14.4891929905171,
336.269852941177));
#161322=CARTESIAN_POINT('Ctrl Pts',(-2.75624276724856,14.7445964952585,
334.775735294118));
#161323=CARTESIAN_POINT('Ctrl Pts',(-1.38995469363044,15.,333.281617647059));
#161324=CARTESIAN_POINT('Ctrl Pts',(-1.83697019872103E-15,15.,331.7875));
#161325=CARTESIAN_POINT('Ctrl Pts',(1.38995469363045,15.,330.293382352941));
#161326=CARTESIAN_POINT('Ctrl Pts',(2.75624276724855,14.7445964952585,328.799264705882));
#161327=CARTESIAN_POINT('Ctrl Pts',(4.12253084086666,14.4891929905171,327.305147058824));
#161328=CARTESIAN_POINT('Ctrl Pts',(5.4186249928073,13.9870834410653,325.811029411765));
#161329=CARTESIAN_POINT('Ctrl Pts',(6.71471914474792,13.4849738916136,324.316911764706));
#161330=CARTESIAN_POINT('Ctrl Pts',(7.89648244316034,12.7532570359442,322.822794117647));
#161331=CARTESIAN_POINT('Ctrl Pts',(9.07824574157275,12.0215401802748,321.328676470588));
#161332=CARTESIAN_POINT('Ctrl Pts',(10.1054346546984,11.0851337583099,319.834558823529));
#161333=CARTESIAN_POINT('Ctrl Pts',(11.132623567824,10.148727336345,318.340441176471));
#161334=CARTESIAN_POINT('Ctrl Pts',(11.9702584092036,9.03951954568885,316.846323529412));
#161335=CARTESIAN_POINT('Ctrl Pts',(12.8078932505832,7.93031175503273,315.352205882353));
#161336=CARTESIAN_POINT('Ctrl Pts',(13.4274493703259,6.68607533664807,313.858088235294));
#161337=CARTESIAN_POINT('Ctrl Pts',(14.0470054900687,5.44183891826343,312.363970588235));
#161338=CARTESIAN_POINT('Ctrl Pts',(14.4273846475923,4.10494485108125,310.869852941176));
#161339=CARTESIAN_POINT('Ctrl Pts',(14.8077638051159,2.76805078389905,309.375735294118));
#161340=CARTESIAN_POINT('Ctrl Pts',(14.9360126444255,1.38402539194953,307.881617647059));
#161341=CARTESIAN_POINT('Ctrl Pts',(15.0642614837351,2.76725994113625E-15,
306.3875));
#161342=CARTESIAN_POINT('Ctrl Pts',(14.9360126444255,-1.38402539194952,
304.893382352941));
#161343=CARTESIAN_POINT('Ctrl Pts',(14.8077638051159,-2.76805078389906,
303.399264705882));
#161344=CARTESIAN_POINT('Ctrl Pts',(14.4273846475923,-4.10494485108124,
301.905147058824));
#161345=CARTESIAN_POINT('Ctrl Pts',(14.0470054900687,-5.44183891826342,
300.411029411765));
#161346=CARTESIAN_POINT('Ctrl Pts',(13.4274493703259,-6.68607533664808,
298.916911764706));
#161347=CARTESIAN_POINT('Ctrl Pts',(12.8078932505832,-7.93031175503273,
297.422794117647));
#161348=CARTESIAN_POINT('Ctrl Pts',(11.9702584092036,-9.03951954568884,
295.928676470588));
#161349=CARTESIAN_POINT('Ctrl Pts',(11.132623567824,-10.148727336345,294.43455882353));
#161350=CARTESIAN_POINT('Ctrl Pts',(10.1054346546984,-11.0851337583099,
292.940441176471));
#161351=CARTESIAN_POINT('Ctrl Pts',(9.07824574157275,-12.0215401802748,
291.446323529412));
#161352=CARTESIAN_POINT('Ctrl Pts',(7.89648244316034,-12.7532570359442,
289.952205882353));
#161353=CARTESIAN_POINT('Ctrl Pts',(6.71471914474792,-13.4849738916136,
288.458088235294));
#161354=CARTESIAN_POINT('Ctrl Pts',(5.4186249928073,-13.9870834410653,286.963970588235));
#161355=CARTESIAN_POINT('Ctrl Pts',(4.12253084086667,-14.4891929905171,
285.469852941177));
#161356=CARTESIAN_POINT('Ctrl Pts',(2.75624276724855,-14.7445964952585,
283.975735294118));
#161357=CARTESIAN_POINT('Ctrl Pts',(1.38995469363045,-15.,282.481617647059));
#161358=CARTESIAN_POINT('Ctrl Pts',(0.,-15.,280.9875));
#161359=CARTESIAN_POINT('Ctrl Pts',(-1.38995469363045,-15.,279.493382352941));
#161360=CARTESIAN_POINT('Ctrl Pts',(-2.75624276724856,-14.7445964952585,
277.999264705882));
#161361=CARTESIAN_POINT('Ctrl Pts',(-4.12253084086666,-14.4891929905171,
276.505147058824));
#161362=CARTESIAN_POINT('Ctrl Pts',(-5.41862499280729,-13.9870834410653,
275.011029411765));
#161363=CARTESIAN_POINT('Ctrl Pts',(-6.71471914474793,-13.4849738916136,
273.516911764706));
#161364=CARTESIAN_POINT('Ctrl Pts',(-7.89648244316034,-12.7532570359442,
272.022794117647));
#161365=CARTESIAN_POINT('Ctrl Pts',(-9.07824574157275,-12.0215401802748,
270.528676470588));
#161366=CARTESIAN_POINT('Ctrl Pts',(-10.1054346546984,-11.0851337583099,
269.034558823529));
#161367=CARTESIAN_POINT('Ctrl Pts',(-11.132623567824,-10.148727336345,267.540441176471));
#161368=CARTESIAN_POINT('Ctrl Pts',(-11.9702584092036,-9.03951954568885,
266.046323529412));
#161369=CARTESIAN_POINT('Ctrl Pts',(-12.8078932505832,-7.93031175503273,
264.552205882353));
#161370=CARTESIAN_POINT('Ctrl Pts',(-13.4274493703259,-6.68607533664808,
263.058088235294));
#161371=CARTESIAN_POINT('Ctrl Pts',(-14.0470054900687,-5.44183891826343,
261.563970588235));
#161372=CARTESIAN_POINT('Ctrl Pts',(-14.4273846475923,-4.10494485108124,
260.069852941176));
#161373=CARTESIAN_POINT('Ctrl Pts',(-14.8077638051159,-2.76805078389906,
258.575735294118));
#161374=CARTESIAN_POINT('Ctrl Pts',(-14.9360126444255,-1.38402539194953,
257.081617647059));
#161375=CARTESIAN_POINT('Ctrl Pts',(-15.0642614837351,-9.22419980378748E-16,
255.5875));
#161376=CARTESIAN_POINT('Ctrl Pts',(-14.9360126444255,1.38402539194953,
254.093382352941));
#161377=CARTESIAN_POINT('Ctrl Pts',(-14.8077638051159,2.76805078389906,
252.599264705882));
#161378=CARTESIAN_POINT('Ctrl Pts',(-14.4273846475923,4.10494485108124,
251.105147058823));
#161379=CARTESIAN_POINT('Ctrl Pts',(-14.0470054900687,5.44183891826343,
249.611029411765));
#161380=CARTESIAN_POINT('Ctrl Pts',(-13.4274493703259,6.68607533664807,
248.116911764706));
#161381=CARTESIAN_POINT('Ctrl Pts',(-12.8078932505832,7.93031175503273,
246.622794117647));
#161382=CARTESIAN_POINT('Ctrl Pts',(-11.9702584092036,9.03951954568884,
245.128676470588));
#161383=CARTESIAN_POINT('Ctrl Pts',(-11.132623567824,10.148727336345,243.634558823529));
#161384=CARTESIAN_POINT('Ctrl Pts',(-10.1054346546984,11.0851337583099,
242.140441176471));
#161385=CARTESIAN_POINT('Ctrl Pts',(-9.07824574157275,12.0215401802748,
240.646323529412));
#161386=CARTESIAN_POINT('Ctrl Pts',(-7.89648244316034,12.7532570359442,
239.152205882353));
#161387=CARTESIAN_POINT('Ctrl Pts',(-6.71471914474793,13.4849738916136,
237.658088235294));
#161388=CARTESIAN_POINT('Ctrl Pts',(-5.41862499280729,13.9870834410653,
236.163970588235));
#161389=CARTESIAN_POINT('Ctrl Pts',(-4.12253084086667,14.4891929905171,
234.669852941177));
#161390=CARTESIAN_POINT('Ctrl Pts',(-2.75624276724856,14.7445964952585,
233.175735294118));
#161391=CARTESIAN_POINT('Ctrl Pts',(-1.38995469363044,15.,231.681617647059));
#161392=CARTESIAN_POINT('Ctrl Pts',(-1.83697019872103E-15,15.,230.1875));
#161393=CARTESIAN_POINT('Ctrl Pts',(1.38995469363045,15.,228.693382352941));
#161394=CARTESIAN_POINT('Ctrl Pts',(2.75624276724855,14.7445964952585,227.199264705882));
#161395=CARTESIAN_POINT('Ctrl Pts',(4.12253084086666,14.4891929905171,225.705147058824));
#161396=CARTESIAN_POINT('Ctrl Pts',(5.4186249928073,13.9870834410653,224.211029411765));
#161397=CARTESIAN_POINT('Ctrl Pts',(6.71471914474792,13.4849738916136,222.716911764706));
#161398=CARTESIAN_POINT('Ctrl Pts',(7.89648244316034,12.7532570359442,221.222794117647));
#161399=CARTESIAN_POINT('Ctrl Pts',(9.07824574157275,12.0215401802748,219.728676470588));
#161400=CARTESIAN_POINT('Ctrl Pts',(10.1054346546984,11.0851337583099,218.234558823529));
#161401=CARTESIAN_POINT('Ctrl Pts',(11.132623567824,10.148727336345,216.740441176471));
#161402=CARTESIAN_POINT('Ctrl Pts',(11.9702584092036,9.03951954568885,215.246323529412));
#161403=CARTESIAN_POINT('Ctrl Pts',(12.8078932505832,7.93031175503273,213.752205882353));
#161404=CARTESIAN_POINT('Ctrl Pts',(13.4274493703259,6.68607533664807,212.258088235294));
#161405=CARTESIAN_POINT('Ctrl Pts',(14.0470054900687,5.44183891826343,210.763970588235));
#161406=CARTESIAN_POINT('Ctrl Pts',(14.4273846475923,4.10494485108125,209.269852941177));
#161407=CARTESIAN_POINT('Ctrl Pts',(14.8077638051159,2.76805078389905,207.775735294118));
#161408=CARTESIAN_POINT('Ctrl Pts',(14.9360126444255,1.38402539194953,206.281617647059));
#161409=CARTESIAN_POINT('Ctrl Pts',(15.0642614837351,2.76725994113625E-15,
204.7875));
#161410=CARTESIAN_POINT('Ctrl Pts',(14.9360126444255,-1.38402539194952,
203.293382352941));
#161411=CARTESIAN_POINT('Ctrl Pts',(14.8077638051159,-2.76805078389906,
201.799264705882));
#161412=CARTESIAN_POINT('Ctrl Pts',(14.4273846475923,-4.10494485108124,
200.305147058824));
#161413=CARTESIAN_POINT('Ctrl Pts',(14.0470054900687,-5.44183891826342,
198.811029411765));
#161414=CARTESIAN_POINT('Ctrl Pts',(13.4274493703259,-6.68607533664808,
197.316911764706));
#161415=CARTESIAN_POINT('Ctrl Pts',(12.8078932505832,-7.93031175503273,
195.822794117647));
#161416=CARTESIAN_POINT('Ctrl Pts',(11.9702584092036,-9.03951954568884,
194.328676470588));
#161417=CARTESIAN_POINT('Ctrl Pts',(11.132623567824,-10.148727336345,192.834558823529));
#161418=CARTESIAN_POINT('Ctrl Pts',(10.1054346546984,-11.0851337583099,
191.340441176471));
#161419=CARTESIAN_POINT('Ctrl Pts',(9.07824574157275,-12.0215401802748,
189.846323529412));
#161420=CARTESIAN_POINT('Ctrl Pts',(7.89648244316034,-12.7532570359442,
188.352205882353));
#161421=CARTESIAN_POINT('Ctrl Pts',(6.71471914474792,-13.4849738916136,
186.858088235294));
#161422=CARTESIAN_POINT('Ctrl Pts',(5.4186249928073,-13.9870834410653,185.363970588235));
#161423=CARTESIAN_POINT('Ctrl Pts',(4.12253084086667,-14.4891929905171,
183.869852941176));
#161424=CARTESIAN_POINT('Ctrl Pts',(2.75624276724855,-14.7445964952585,
182.375735294118));
#161425=CARTESIAN_POINT('Ctrl Pts',(1.38995469363045,-15.,180.881617647059));
#161426=CARTESIAN_POINT('Ctrl Pts',(0.,-15.,179.3875));
#161427=CARTESIAN_POINT('Ctrl Pts',(-1.38995469363045,-15.,177.893382352941));
#161428=CARTESIAN_POINT('Ctrl Pts',(-2.75624276724856,-14.7445964952585,
176.399264705882));
#161429=CARTESIAN_POINT('Ctrl Pts',(-4.12253084086666,-14.4891929905171,
174.905147058824));
#161430=CARTESIAN_POINT('Ctrl Pts',(-5.41862499280729,-13.9870834410653,
173.411029411765));
#161431=CARTESIAN_POINT('Ctrl Pts',(-6.71471914474793,-13.4849738916136,
171.916911764706));
#161432=CARTESIAN_POINT('Ctrl Pts',(-7.89648244316034,-12.7532570359442,
170.422794117647));
#161433=CARTESIAN_POINT('Ctrl Pts',(-9.07824574157275,-12.0215401802748,
168.928676470588));
#161434=CARTESIAN_POINT('Ctrl Pts',(-10.1054346546984,-11.0851337583099,
167.43455882353));
#161435=CARTESIAN_POINT('Ctrl Pts',(-11.132623567824,-10.148727336345,165.940441176471));
#161436=CARTESIAN_POINT('Ctrl Pts',(-11.9702584092036,-9.03951954568885,
164.446323529412));
#161437=CARTESIAN_POINT('Ctrl Pts',(-12.8078932505832,-7.93031175503273,
162.952205882353));
#161438=CARTESIAN_POINT('Ctrl Pts',(-13.4274493703259,-6.68607533664808,
161.458088235294));
#161439=CARTESIAN_POINT('Ctrl Pts',(-14.0470054900687,-5.44183891826343,
159.963970588235));
#161440=CARTESIAN_POINT('Ctrl Pts',(-14.4273846475923,-4.10494485108124,
158.469852941177));
#161441=CARTESIAN_POINT('Ctrl Pts',(-14.8077638051159,-2.76805078389906,
156.975735294118));
#161442=CARTESIAN_POINT('Ctrl Pts',(-14.9360126444255,-1.38402539194953,
155.481617647059));
#161443=CARTESIAN_POINT('Ctrl Pts',(-15.0642614837351,-9.22419980378748E-16,
153.9875));
#161444=CARTESIAN_POINT('Ctrl Pts',(-14.9360126444255,1.38402539194953,
152.493382352941));
#161445=CARTESIAN_POINT('Ctrl Pts',(-14.8077638051159,2.76805078389906,
150.999264705882));
#161446=CARTESIAN_POINT('Ctrl Pts',(-14.4273846475923,4.10494485108124,
149.505147058824));
#161447=CARTESIAN_POINT('Ctrl Pts',(-14.0470054900687,5.44183891826343,
148.011029411765));
#161448=CARTESIAN_POINT('Ctrl Pts',(-13.4274493703259,6.68607533664807,
146.516911764706));
#161449=CARTESIAN_POINT('Ctrl Pts',(-12.8078932505832,7.93031175503273,
145.022794117647));
#161450=CARTESIAN_POINT('Ctrl Pts',(-11.9702584092036,9.03951954568884,
143.528676470588));
#161451=CARTESIAN_POINT('Ctrl Pts',(-11.132623567824,10.148727336345,142.034558823529));
#161452=CARTESIAN_POINT('Ctrl Pts',(-10.1054346546984,11.0851337583099,
140.540441176471));
#161453=CARTESIAN_POINT('Ctrl Pts',(-9.07824574157275,12.0215401802748,
139.046323529412));
#161454=CARTESIAN_POINT('Ctrl Pts',(-7.89648244316034,12.7532570359442,
137.552205882353));
#161455=CARTESIAN_POINT('Ctrl Pts',(-6.71471914474793,13.4849738916136,
136.058088235294));
#161456=CARTESIAN_POINT('Ctrl Pts',(-5.41862499280729,13.9870834410653,
134.563970588235));
#161457=CARTESIAN_POINT('Ctrl Pts',(-4.12253084086667,14.4891929905171,
133.069852941176));
#161458=CARTESIAN_POINT('Ctrl Pts',(-2.75624276724856,14.7445964952585,
131.575735294118));
#161459=CARTESIAN_POINT('Ctrl Pts',(-1.38995469363044,15.,130.081617647059));
#161460=CARTESIAN_POINT('Ctrl Pts',(-1.83697019872103E-15,15.,128.5875));
#161461=CARTESIAN_POINT('Ctrl Pts',(1.38995469363045,15.,127.093382352941));
#161462=CARTESIAN_POINT('Ctrl Pts',(2.75624276724855,14.7445964952585,125.599264705882));
#161463=CARTESIAN_POINT('Ctrl Pts',(4.12253084086666,14.4891929905171,124.105147058824));
#161464=CARTESIAN_POINT('Ctrl Pts',(5.4186249928073,13.9870834410653,122.611029411765));
#161465=CARTESIAN_POINT('Ctrl Pts',(6.71471914474792,13.4849738916136,121.116911764706));
#161466=CARTESIAN_POINT('Ctrl Pts',(7.89648244316034,12.7532570359442,119.622794117647));
#161467=CARTESIAN_POINT('Ctrl Pts',(9.07824574157275,12.0215401802748,118.128676470588));
#161468=CARTESIAN_POINT('Ctrl Pts',(10.1054346546984,11.0851337583099,116.634558823529));
#161469=CARTESIAN_POINT('Ctrl Pts',(11.132623567824,10.148727336345,115.140441176471));
#161470=CARTESIAN_POINT('Ctrl Pts',(11.9702584092036,9.03951954568885,113.646323529412));
#161471=CARTESIAN_POINT('Ctrl Pts',(12.8078932505832,7.93031175503273,112.152205882353));
#161472=CARTESIAN_POINT('Ctrl Pts',(13.4274493703259,6.68607533664807,110.658088235294));
#161473=CARTESIAN_POINT('Ctrl Pts',(14.0470054900687,5.44183891826343,109.163970588235));
#161474=CARTESIAN_POINT('Ctrl Pts',(14.4273846475923,4.10494485108125,107.669852941177));
#161475=CARTESIAN_POINT('Ctrl Pts',(14.8077638051159,2.76805078389905,106.175735294118));
#161476=CARTESIAN_POINT('Ctrl Pts',(14.9360126444255,1.38402539194953,104.681617647059));
#161477=CARTESIAN_POINT('Ctrl Pts',(15.0642614837351,2.76725994113625E-15,
103.1875));
#161478=CARTESIAN_POINT('Ctrl Pts',(14.9360126444255,-1.38402539194952,
101.693382352941));
#161479=CARTESIAN_POINT('Ctrl Pts',(14.8077638051159,-2.76805078389906,
100.199264705882));
#161480=CARTESIAN_POINT('Ctrl Pts',(14.4273846475923,-4.10494485108124,
98.7051470588236));
#161481=CARTESIAN_POINT('Ctrl Pts',(14.0470054900687,-5.44183891826342,
97.2110294117647));
#161482=CARTESIAN_POINT('Ctrl Pts',(13.4274493703259,-6.68607533664808,
95.7169117647059));
#161483=CARTESIAN_POINT('Ctrl Pts',(12.8078932505832,-7.93031175503273,
94.222794117647));
#161484=CARTESIAN_POINT('Ctrl Pts',(11.9702584092036,-9.03951954568884,
92.7286764705884));
#161485=CARTESIAN_POINT('Ctrl Pts',(11.132623567824,-10.148727336345,91.2345588235295));
#161486=CARTESIAN_POINT('Ctrl Pts',(10.1054346546984,-11.0851337583099,
89.7404411764706));
#161487=CARTESIAN_POINT('Ctrl Pts',(9.07824574157275,-12.0215401802748,
88.2463235294117));
#161488=CARTESIAN_POINT('Ctrl Pts',(7.89648244316034,-12.7532570359442,
86.7522058823529));
#161489=CARTESIAN_POINT('Ctrl Pts',(6.71471914474792,-13.4849738916136,
85.2580882352942));
#161490=CARTESIAN_POINT('Ctrl Pts',(5.4186249928073,-13.9870834410653,83.7639705882354));
#161491=CARTESIAN_POINT('Ctrl Pts',(4.12253084086667,-14.4891929905171,
82.2698529411765));
#161492=CARTESIAN_POINT('Ctrl Pts',(2.75624276724855,-14.7445964952585,
80.7757352941176));
#161493=CARTESIAN_POINT('Ctrl Pts',(1.38995469363045,-15.,79.2816176470588));
#161494=CARTESIAN_POINT('Ctrl Pts',(0.,-15.,77.7875000000001));
#161495=CARTESIAN_POINT('Ctrl Pts',(-1.38995469363045,-15.,76.2933823529413));
#161496=CARTESIAN_POINT('Ctrl Pts',(-2.75624276724856,-14.7445964952585,
74.7992647058824));
#161497=CARTESIAN_POINT('Ctrl Pts',(-4.12253084086666,-14.4891929905171,
73.3051470588235));
#161498=CARTESIAN_POINT('Ctrl Pts',(-5.41862499280729,-13.9870834410653,
71.8110294117647));
#161499=CARTESIAN_POINT('Ctrl Pts',(-6.71471914474793,-13.4849738916136,
70.316911764706));
#161500=CARTESIAN_POINT('Ctrl Pts',(-7.89648244316034,-12.7532570359442,
68.8227941176471));
#161501=CARTESIAN_POINT('Ctrl Pts',(-9.07824574157275,-12.0215401802748,
67.3286764705883));
#161502=CARTESIAN_POINT('Ctrl Pts',(-10.1054346546984,-11.0851337583099,
65.8345588235294));
#161503=CARTESIAN_POINT('Ctrl Pts',(-11.132623567824,-10.148727336345,64.3404411764705));
#161504=CARTESIAN_POINT('Ctrl Pts',(-11.9702584092036,-9.03951954568885,
62.8463235294119));
#161505=CARTESIAN_POINT('Ctrl Pts',(-12.8078932505832,-7.93031175503273,
61.352205882353));
#161506=CARTESIAN_POINT('Ctrl Pts',(-13.4274493703259,-6.68607533664808,
59.8580882352941));
#161507=CARTESIAN_POINT('Ctrl Pts',(-14.0470054900687,-5.44183891826343,
58.3639705882353));
#161508=CARTESIAN_POINT('Ctrl Pts',(-14.4273846475923,-4.10494485108124,
56.8698529411764));
#161509=CARTESIAN_POINT('Ctrl Pts',(-14.8077638051159,-2.76805078389906,
55.3757352941178));
#161510=CARTESIAN_POINT('Ctrl Pts',(-14.9360126444255,-1.38402539194953,
53.8816176470589));
#161511=CARTESIAN_POINT('Ctrl Pts',(-15.0642614837351,-9.22419980378748E-16,
52.3875));
#161512=CARTESIAN_POINT('Ctrl Pts',(-14.9360126444255,1.38402539194953,
50.8933823529412));
#161513=CARTESIAN_POINT('Ctrl Pts',(-14.8077638051159,2.76805078389906,
49.3992647058823));
#161514=CARTESIAN_POINT('Ctrl Pts',(-14.4273846475923,4.10494485108124,
47.9051470588237));
#161515=CARTESIAN_POINT('Ctrl Pts',(-14.0470054900687,5.44183891826343,
46.4110294117648));
#161516=CARTESIAN_POINT('Ctrl Pts',(-13.4274493703259,6.68607533664807,
44.9169117647059));
#161517=CARTESIAN_POINT('Ctrl Pts',(-12.8078932505832,7.93031175503273,
43.422794117647));
#161518=CARTESIAN_POINT('Ctrl Pts',(-11.9702584092036,9.03951954568884,
41.9286764705882));
#161519=CARTESIAN_POINT('Ctrl Pts',(-11.132623567824,10.148727336345,40.4345588235295));
#161520=CARTESIAN_POINT('Ctrl Pts',(-10.1054346546984,11.0851337583099,
38.9404411764707));
#161521=CARTESIAN_POINT('Ctrl Pts',(-9.07824574157275,12.0215401802748,
37.4463235294118));
#161522=CARTESIAN_POINT('Ctrl Pts',(-7.89648244316034,12.7532570359442,
35.9522058823529));
#161523=CARTESIAN_POINT('Ctrl Pts',(-6.71471914474793,13.4849738916136,
34.4580882352941));
#161524=CARTESIAN_POINT('Ctrl Pts',(-5.41862499280729,13.9870834410653,
32.9639705882354));
#161525=CARTESIAN_POINT('Ctrl Pts',(-4.12253084086667,14.4891929905171,
31.4698529411765));
#161526=CARTESIAN_POINT('Ctrl Pts',(-2.75624276724856,14.7445964952585,
29.9757352941177));
#161527=CARTESIAN_POINT('Ctrl Pts',(-1.38995469363044,15.,28.4816176470588));
#161528=CARTESIAN_POINT('Ctrl Pts',(-1.83697019872103E-15,15.,26.9874999999999));
#161529=CARTESIAN_POINT('Ctrl Pts',(1.38995469363045,15.,25.4933823529413));
#161530=CARTESIAN_POINT('Ctrl Pts',(2.75624276724855,14.7445964952585,23.9992647058824));
#161531=CARTESIAN_POINT('Ctrl Pts',(4.12253084086666,14.4891929905171,22.5051470588236));
#161532=CARTESIAN_POINT('Ctrl Pts',(5.4186249928073,13.9870834410653,21.0110294117647));
#161533=CARTESIAN_POINT('Ctrl Pts',(6.71471914474792,13.4849738916136,19.5169117647058));
#161534=CARTESIAN_POINT('Ctrl Pts',(7.89648244316034,12.7532570359442,18.0227941176472));
#161535=CARTESIAN_POINT('Ctrl Pts',(9.07824574157275,12.0215401802748,16.5286764705883));
#161536=CARTESIAN_POINT('Ctrl Pts',(10.1054346546984,11.0851337583099,15.0345588235294));
#161537=CARTESIAN_POINT('Ctrl Pts',(11.132623567824,10.148727336345,13.5404411764706));
#161538=CARTESIAN_POINT('Ctrl Pts',(11.9702584092036,9.03951954568885,12.0463235294117));
#161539=CARTESIAN_POINT('Ctrl Pts',(12.8078932505832,7.93031175503273,10.5522058823531));
#161540=CARTESIAN_POINT('Ctrl Pts',(13.4274493703259,6.68607533664807,9.05808823529419));
#161541=CARTESIAN_POINT('Ctrl Pts',(14.0470054900687,5.44183891826343,7.56397058823533));
#161542=CARTESIAN_POINT('Ctrl Pts',(14.4273846475923,4.10494485108125,6.06985294117646));
#161543=CARTESIAN_POINT('Ctrl Pts',(14.8077638051159,2.76805078389905,4.57573529411759));
#161544=CARTESIAN_POINT('Ctrl Pts',(14.9360126444255,1.38402539194953,3.08161764705894));
#161545=CARTESIAN_POINT('Ctrl Pts',(15.0642614837351,2.76725994113625E-15,
1.58750000000007));
#161546=CARTESIAN_POINT('Ctrl Pts',(14.9360126444255,-1.38402539194952,
0.093382352941207));
#161547=CARTESIAN_POINT('Ctrl Pts',(14.8077638051159,-2.76805078389906,
-1.40073529411766));
#161548=CARTESIAN_POINT('Ctrl Pts',(14.4273846475923,-4.10494485108124,
-2.89485294117653));
#161549=CARTESIAN_POINT('Ctrl Pts',(14.0470054900687,-5.44183891826342,
-4.38897058823517));
#161550=CARTESIAN_POINT('Ctrl Pts',(13.4274493703259,-6.68607533664808,
-5.88308823529404));
#161551=CARTESIAN_POINT('Ctrl Pts',(12.8078932505832,-7.93031175503273,
-7.37720588235291));
#161552=CARTESIAN_POINT('Ctrl Pts',(11.9702584092036,-9.03951954568884,
-8.87132352941178));
#161553=CARTESIAN_POINT('Ctrl Pts',(11.132623567824,-10.148727336345,-10.3654411764706));
#161554=CARTESIAN_POINT('Ctrl Pts',(10.1054346546984,-11.0851337583099,
-11.8595588235293));
#161555=CARTESIAN_POINT('Ctrl Pts',(9.07824574157275,-12.0215401802748,
-13.3536764705882));
#161556=CARTESIAN_POINT('Ctrl Pts',(7.89648244316034,-12.7532570359442,
-14.847794117647));
#161557=CARTESIAN_POINT('Ctrl Pts',(6.71471914474792,-13.4849738916136,
-16.3419117647059));
#161558=CARTESIAN_POINT('Ctrl Pts',(5.4186249928073,-13.9870834410653,-17.8360294117648));
#161559=CARTESIAN_POINT('Ctrl Pts',(4.12253084086667,-14.4891929905171,
-19.3301470588234));
#161560=CARTESIAN_POINT('Ctrl Pts',(2.75624276724855,-14.7445964952585,
-20.8242647058823));
#161561=CARTESIAN_POINT('Ctrl Pts',(1.38995469363045,-15.,-22.3183823529411));
#161562=CARTESIAN_POINT('Ctrl Pts',(0.,-15.,-23.8125));
#161563=CARTESIAN_POINT('Ctrl Pts',(-1.38995469363045,-15.,-25.3066176470589));
#161564=CARTESIAN_POINT('Ctrl Pts',(-2.75624276724856,-14.7445964952585,
-26.8007352941175));
#161565=CARTESIAN_POINT('Ctrl Pts',(-4.12253084086666,-14.4891929905171,
-28.2948529411764));
#161566=CARTESIAN_POINT('Ctrl Pts',(-5.41862499280729,-13.9870834410653,
-29.7889705882353));
#161567=CARTESIAN_POINT('Ctrl Pts',(-6.71471914474793,-13.4849738916136,
-31.2830882352941));
#161568=CARTESIAN_POINT('Ctrl Pts',(-7.89648244316034,-12.7532570359442,
-32.777205882353));
#161569=CARTESIAN_POINT('Ctrl Pts',(-9.07824574157275,-12.0215401802748,
-34.2713235294116));
#161570=CARTESIAN_POINT('Ctrl Pts',(-10.1054346546984,-11.0851337583099,
-35.7654411764705));
#161571=CARTESIAN_POINT('Ctrl Pts',(-11.132623567824,-10.148727336345,-37.2595588235294));
#161572=CARTESIAN_POINT('Ctrl Pts',(-11.9702584092036,-9.03951954568885,
-38.7536764705882));
#161573=CARTESIAN_POINT('Ctrl Pts',(-12.8078932505832,-7.93031175503273,
-40.2477941176471));
#161574=CARTESIAN_POINT('Ctrl Pts',(-13.4274493703259,-6.68607533664808,
-41.7419117647058));
#161575=CARTESIAN_POINT('Ctrl Pts',(-14.0470054900687,-5.44183891826343,
-43.2360294117646));
#161576=CARTESIAN_POINT('Ctrl Pts',(-14.4273846475923,-4.10494485108124,
-44.7301470588235));
#161577=CARTESIAN_POINT('Ctrl Pts',(-14.8077638051159,-2.76805078389906,
-46.2242647058824));
#161578=CARTESIAN_POINT('Ctrl Pts',(-14.9360126444255,-1.38402539194953,
-47.7183823529412));
#161579=CARTESIAN_POINT('Ctrl Pts',(-15.0642614837351,-9.22419980378748E-16,
-49.2124999999999));
#161580=CARTESIAN_POINT('Ctrl Pts',(-14.9360126444255,1.38402539194953,
-50.7066176470587));
#161581=CARTESIAN_POINT('Ctrl Pts',(-14.8077638051159,2.76805078389906,
-52.2007352941176));
#161582=CARTESIAN_POINT('Ctrl Pts',(-14.4273846475923,4.10494485108124,
-53.6948529411765));
#161583=CARTESIAN_POINT('Ctrl Pts',(-14.0470054900687,5.44183891826343,
-55.1889705882354));
#161584=CARTESIAN_POINT('Ctrl Pts',(-13.4274493703259,6.68607533664807,
-56.683088235294));
#161585=CARTESIAN_POINT('Ctrl Pts',(-12.8078932505832,7.93031175503273,
-58.1772058823529));
#161586=CARTESIAN_POINT('Ctrl Pts',(-11.9702584092036,9.03951954568884,
-59.6713235294117));
#161587=CARTESIAN_POINT('Ctrl Pts',(-11.132623567824,10.148727336345,-61.1654411764706));
#161588=CARTESIAN_POINT('Ctrl Pts',(-10.1054346546984,11.0851337583099,
-62.6595588235295));
#161589=CARTESIAN_POINT('Ctrl Pts',(-9.07824574157275,12.0215401802748,
-64.1536764705881));
#161590=CARTESIAN_POINT('Ctrl Pts',(-7.89648244316034,12.7532570359442,
-65.647794117647));
#161591=CARTESIAN_POINT('Ctrl Pts',(-6.71471914474793,13.4849738916136,
-67.1419117647059));
#161592=CARTESIAN_POINT('Ctrl Pts',(-5.41862499280729,13.9870834410653,
-68.6360294117647));
#161593=CARTESIAN_POINT('Ctrl Pts',(-4.12253084086667,14.4891929905171,
-70.1301470588236));
#161594=CARTESIAN_POINT('Ctrl Pts',(-2.75624276724856,14.7445964952585,
-71.6242647058822));
#161595=CARTESIAN_POINT('Ctrl Pts',(-1.38995469363044,15.,-73.1183823529411));
#161596=CARTESIAN_POINT('Ctrl Pts',(-1.83697019872103E-15,15.,-74.6125));
#161597=CARTESIAN_POINT('Ctrl Pts',(1.38995469363045,15.,-76.1066176470589));
#161598=CARTESIAN_POINT('Ctrl Pts',(2.75624276724855,14.7445964952585,-77.6007352941177));
#161599=CARTESIAN_POINT('Ctrl Pts',(4.12253084086666,14.4891929905171,-79.0948529411764));
#161600=CARTESIAN_POINT('Ctrl Pts',(5.4186249928073,13.9870834410653,-80.5889705882352));
#161601=CARTESIAN_POINT('Ctrl Pts',(6.71471914474792,13.4849738916136,-82.0830882352941));
#161602=CARTESIAN_POINT('Ctrl Pts',(7.89648244316034,12.7532570359442,-83.577205882353));
#161603=CARTESIAN_POINT('Ctrl Pts',(9.07824574157275,12.0215401802748,-85.0713235294118));
#161604=CARTESIAN_POINT('Ctrl Pts',(10.1054346546984,11.0851337583099,-86.5654411764705));
#161605=CARTESIAN_POINT('Ctrl Pts',(11.132623567824,10.148727336345,-88.0595588235294));
#161606=CARTESIAN_POINT('Ctrl Pts',(11.9702584092036,9.03951954568885,-89.5536764705882));
#161607=CARTESIAN_POINT('Ctrl Pts',(12.8078932505832,7.93031175503273,-91.0477941176471));
#161608=CARTESIAN_POINT('Ctrl Pts',(13.4274493703259,6.68607533664807,-92.541911764706));
#161609=CARTESIAN_POINT('Ctrl Pts',(14.0470054900687,5.44183891826343,-94.0360294117646));
#161610=CARTESIAN_POINT('Ctrl Pts',(14.4273846475923,4.10494485108125,-95.5301470588235));
#161611=CARTESIAN_POINT('Ctrl Pts',(14.8077638051159,2.76805078389905,-97.0242647058824));
#161612=CARTESIAN_POINT('Ctrl Pts',(14.9360126444255,1.38402539194953,-98.5183823529412));
#161613=CARTESIAN_POINT('Ctrl Pts',(15.0642614837351,2.76725994113625E-15,
-100.0125));
#161614=CARTESIAN_POINT('Ctrl Pts',(14.9360126444255,-1.38402539194952,
-101.506617647059));
#161615=CARTESIAN_POINT('Ctrl Pts',(14.8077638051159,-2.76805078389906,
-103.000735294118));
#161616=CARTESIAN_POINT('Ctrl Pts',(14.4273846475923,-4.10494485108124,
-104.494852941176));
#161617=CARTESIAN_POINT('Ctrl Pts',(14.0470054900687,-5.44183891826342,
-105.988970588235));
#161618=CARTESIAN_POINT('Ctrl Pts',(13.4274493703259,-6.68607533664808,
-107.483088235294));
#161619=CARTESIAN_POINT('Ctrl Pts',(12.8078932505832,-7.93031175503273,
-108.977205882353));
#161620=CARTESIAN_POINT('Ctrl Pts',(11.9702584092036,-9.03951954568884,
-110.471323529412));
#161621=CARTESIAN_POINT('Ctrl Pts',(11.132623567824,-10.148727336345,-111.965441176471));
#161622=CARTESIAN_POINT('Ctrl Pts',(10.1054346546984,-11.0851337583099,
-113.459558823529));
#161623=CARTESIAN_POINT('Ctrl Pts',(9.07824574157275,-12.0215401802748,
-114.953676470588));
#161624=CARTESIAN_POINT('Ctrl Pts',(7.89648244316034,-12.7532570359442,
-116.447794117647));
#161625=CARTESIAN_POINT('Ctrl Pts',(6.71471914474792,-13.4849738916136,
-117.941911764706));
#161626=CARTESIAN_POINT('Ctrl Pts',(5.4186249928073,-13.9870834410653,-119.436029411765));
#161627=CARTESIAN_POINT('Ctrl Pts',(4.12253084086667,-14.4891929905171,
-120.930147058824));
#161628=CARTESIAN_POINT('Ctrl Pts',(2.75624276724855,-14.7445964952585,
-122.424264705882));
#161629=CARTESIAN_POINT('Ctrl Pts',(1.38995469363045,-15.,-123.918382352941));
#161630=CARTESIAN_POINT('Ctrl Pts',(0.,-15.,-125.4125));
#161631=CARTESIAN_POINT('Ctrl Pts',(-1.38995469363045,-15.,-126.906617647059));
#161632=CARTESIAN_POINT('Ctrl Pts',(-2.75624276724856,-14.7445964952585,
-128.400735294118));
#161633=CARTESIAN_POINT('Ctrl Pts',(-4.12253084086666,-14.4891929905171,
-129.894852941177));
#161634=CARTESIAN_POINT('Ctrl Pts',(-5.41862499280729,-13.9870834410653,
-131.388970588235));
#161635=CARTESIAN_POINT('Ctrl Pts',(-6.71471914474793,-13.4849738916136,
-132.883088235294));
#161636=CARTESIAN_POINT('Ctrl Pts',(-7.89648244316034,-12.7532570359442,
-134.377205882353));
#161637=CARTESIAN_POINT('Ctrl Pts',(-9.07824574157275,-12.0215401802748,
-135.871323529412));
#161638=CARTESIAN_POINT('Ctrl Pts',(-10.1054346546984,-11.0851337583099,
-137.365441176471));
#161639=CARTESIAN_POINT('Ctrl Pts',(-11.132623567824,-10.148727336345,-138.859558823529));
#161640=CARTESIAN_POINT('Ctrl Pts',(-11.9702584092036,-9.03951954568885,
-140.353676470588));
#161641=CARTESIAN_POINT('Ctrl Pts',(-12.8078932505832,-7.93031175503273,
-141.847794117647));
#161642=CARTESIAN_POINT('Ctrl Pts',(-13.4274493703259,-6.68607533664808,
-143.341911764706));
#161643=CARTESIAN_POINT('Ctrl Pts',(-14.0470054900687,-5.44183891826343,
-144.836029411765));
#161644=CARTESIAN_POINT('Ctrl Pts',(-14.4273846475923,-4.10494485108124,
-146.330147058823));
#161645=CARTESIAN_POINT('Ctrl Pts',(-14.8077638051159,-2.76805078389906,
-147.824264705882));
#161646=CARTESIAN_POINT('Ctrl Pts',(-14.9360126444255,-1.38402539194953,
-149.318382352941));
#161647=CARTESIAN_POINT('Ctrl Pts',(-15.0642614837351,-9.22419980378748E-16,
-150.8125));
#161648=CARTESIAN_POINT('Ctrl Pts',(-14.9360126444255,1.38402539194953,
-152.306617647059));
#161649=CARTESIAN_POINT('Ctrl Pts',(-14.8077638051159,2.76805078389906,
-153.800735294118));
#161650=CARTESIAN_POINT('Ctrl Pts',(-14.4273846475923,4.10494485108124,
-155.294852941176));
#161651=CARTESIAN_POINT('Ctrl Pts',(-14.0470054900687,5.44183891826343,
-156.788970588235));
#161652=CARTESIAN_POINT('Ctrl Pts',(-13.4274493703259,6.68607533664807,
-158.283088235294));
#161653=CARTESIAN_POINT('Ctrl Pts',(-12.8078932505832,7.93031175503273,
-159.777205882353));
#161654=CARTESIAN_POINT('Ctrl Pts',(-11.9702584092036,9.03951954568884,
-161.271323529412));
#161655=CARTESIAN_POINT('Ctrl Pts',(-11.132623567824,10.148727336345,-162.765441176471));
#161656=CARTESIAN_POINT('Ctrl Pts',(-10.1054346546984,11.0851337583099,
-164.259558823529));
#161657=CARTESIAN_POINT('Ctrl Pts',(-9.07824574157275,12.0215401802748,
-165.753676470588));
#161658=CARTESIAN_POINT('Ctrl Pts',(-7.89648244316034,12.7532570359442,
-167.247794117647));
#161659=CARTESIAN_POINT('Ctrl Pts',(-6.71471914474793,13.4849738916136,
-168.741911764706));
#161660=CARTESIAN_POINT('Ctrl Pts',(-5.41862499280729,13.9870834410653,
-170.236029411765));
#161661=CARTESIAN_POINT('Ctrl Pts',(-4.12253084086667,14.4891929905171,
-171.730147058823));
#161662=CARTESIAN_POINT('Ctrl Pts',(-2.75624276724856,14.7445964952585,
-173.224264705882));
#161663=CARTESIAN_POINT('Ctrl Pts',(-1.38995469363044,15.,-174.718382352941));
#161664=CARTESIAN_POINT('Ctrl Pts',(-1.83697019872103E-15,15.,-176.2125));
#161665=CARTESIAN_POINT('Ctrl Pts',(1.38995469363045,15.,-177.706617647059));
#161666=CARTESIAN_POINT('Ctrl Pts',(2.75624276724855,14.7445964952585,-179.200735294118));
#161667=CARTESIAN_POINT('Ctrl Pts',(4.12253084086666,14.4891929905171,-180.694852941176));
#161668=CARTESIAN_POINT('Ctrl Pts',(5.4186249928073,13.9870834410653,-182.188970588235));
#161669=CARTESIAN_POINT('Ctrl Pts',(6.71471914474792,13.4849738916136,-183.683088235294));
#161670=CARTESIAN_POINT('Ctrl Pts',(7.89648244316034,12.7532570359442,-185.177205882353));
#161671=CARTESIAN_POINT('Ctrl Pts',(9.07824574157275,12.0215401802748,-186.671323529412));
#161672=CARTESIAN_POINT('Ctrl Pts',(10.1054346546984,11.0851337583099,-188.165441176471));
#161673=CARTESIAN_POINT('Ctrl Pts',(11.132623567824,10.148727336345,-189.659558823529));
#161674=CARTESIAN_POINT('Ctrl Pts',(11.9702584092036,9.03951954568885,-191.153676470588));
#161675=CARTESIAN_POINT('Ctrl Pts',(12.8078932505832,7.93031175503273,-192.647794117647));
#161676=CARTESIAN_POINT('Ctrl Pts',(13.4274493703259,6.68607533664807,-194.141911764706));
#161677=CARTESIAN_POINT('Ctrl Pts',(14.0470054900687,5.44183891826343,-195.636029411765));
#161678=CARTESIAN_POINT('Ctrl Pts',(14.4273846475923,4.10494485108125,-197.130147058824));
#161679=CARTESIAN_POINT('Ctrl Pts',(14.8077638051159,2.76805078389905,-198.624264705882));
#161680=CARTESIAN_POINT('Ctrl Pts',(14.9360126444255,1.38402539194953,-200.118382352941));
#161681=CARTESIAN_POINT('Ctrl Pts',(15.0642614837351,2.76725994113625E-15,
-201.6125));
#161682=CARTESIAN_POINT('Ctrl Pts',(14.9360126444255,-1.38402539194952,
-203.106617647059));
#161683=CARTESIAN_POINT('Ctrl Pts',(14.8077638051159,-2.76805078389906,
-204.600735294118));
#161684=CARTESIAN_POINT('Ctrl Pts',(14.4273846475923,-4.10494485108124,
-206.094852941176));
#161685=CARTESIAN_POINT('Ctrl Pts',(14.0470054900687,-5.44183891826342,
-207.588970588235));
#161686=CARTESIAN_POINT('Ctrl Pts',(13.4274493703259,-6.68607533664808,
-209.083088235294));
#161687=CARTESIAN_POINT('Ctrl Pts',(12.8078932505832,-7.93031175503273,
-210.577205882353));
#161688=CARTESIAN_POINT('Ctrl Pts',(11.9702584092036,-9.03951954568884,
-212.071323529412));
#161689=CARTESIAN_POINT('Ctrl Pts',(11.132623567824,-10.148727336345,-213.56544117647));
#161690=CARTESIAN_POINT('Ctrl Pts',(10.1054346546984,-11.0851337583099,
-215.059558823529));
#161691=CARTESIAN_POINT('Ctrl Pts',(9.07824574157275,-12.0215401802748,
-216.553676470588));
#161692=CARTESIAN_POINT('Ctrl Pts',(7.89648244316034,-12.7532570359442,
-218.047794117647));
#161693=CARTESIAN_POINT('Ctrl Pts',(6.71471914474792,-13.4849738916136,
-219.541911764706));
#161694=CARTESIAN_POINT('Ctrl Pts',(5.4186249928073,-13.9870834410653,-221.036029411765));
#161695=CARTESIAN_POINT('Ctrl Pts',(4.12253084086667,-14.4891929905171,
-222.530147058823));
#161696=CARTESIAN_POINT('Ctrl Pts',(2.75624276724855,-14.7445964952585,
-224.024264705882));
#161697=CARTESIAN_POINT('Ctrl Pts',(1.38995469363045,-15.,-225.518382352941));
#161698=CARTESIAN_POINT('Ctrl Pts',(0.,-15.,-227.0125));
#161699=CARTESIAN_POINT('Ctrl Pts',(-1.38995469363045,-15.,-228.506617647059));
#161700=CARTESIAN_POINT('Ctrl Pts',(-2.75624276724856,-14.7445964952585,
-230.000735294118));
#161701=CARTESIAN_POINT('Ctrl Pts',(-4.12253084086666,-14.4891929905171,
-231.494852941176));
#161702=CARTESIAN_POINT('Ctrl Pts',(-5.41862499280729,-13.9870834410653,
-232.988970588235));
#161703=CARTESIAN_POINT('Ctrl Pts',(-6.71471914474793,-13.4849738916136,
-234.483088235294));
#161704=CARTESIAN_POINT('Ctrl Pts',(-7.89648244316034,-12.7532570359442,
-235.977205882353));
#161705=CARTESIAN_POINT('Ctrl Pts',(-9.07824574157275,-12.0215401802748,
-237.471323529412));
#161706=CARTESIAN_POINT('Ctrl Pts',(-10.1054346546984,-11.0851337583099,
-238.965441176471));
#161707=CARTESIAN_POINT('Ctrl Pts',(-11.132623567824,-10.148727336345,-240.459558823529));
#161708=CARTESIAN_POINT('Ctrl Pts',(-11.9702584092036,-9.03951954568885,
-241.953676470588));
#161709=CARTESIAN_POINT('Ctrl Pts',(-12.8078932505832,-7.93031175503273,
-243.447794117647));
#161710=CARTESIAN_POINT('Ctrl Pts',(-13.4274493703259,-6.68607533664808,
-244.941911764706));
#161711=CARTESIAN_POINT('Ctrl Pts',(-14.0470054900687,-5.44183891826343,
-246.436029411765));
#161712=CARTESIAN_POINT('Ctrl Pts',(-14.4273846475923,-4.10494485108124,
-247.930147058824));
#161713=CARTESIAN_POINT('Ctrl Pts',(-14.8077638051159,-2.76805078389906,
-249.424264705882));
#161714=CARTESIAN_POINT('Ctrl Pts',(-14.9360126444255,-1.38402539194953,
-250.918382352941));
#161715=CARTESIAN_POINT('Ctrl Pts',(-15.0642614837351,-9.22419980378748E-16,
-252.4125));
#161716=CARTESIAN_POINT('Ctrl Pts',(-14.9360126444255,1.38402539194953,
-253.906617647059));
#161717=CARTESIAN_POINT('Ctrl Pts',(-14.8077638051159,2.76805078389906,
-255.400735294118));
#161718=CARTESIAN_POINT('Ctrl Pts',(-14.4273846475923,4.10494485108124,
-256.894852941177));
#161719=CARTESIAN_POINT('Ctrl Pts',(-14.0470054900687,5.44183891826343,
-258.388970588235));
#161720=CARTESIAN_POINT('Ctrl Pts',(-13.4274493703259,6.68607533664807,
-259.883088235294));
#161721=CARTESIAN_POINT('Ctrl Pts',(-12.8078932505832,7.93031175503273,
-261.377205882353));
#161722=CARTESIAN_POINT('Ctrl Pts',(-11.9702584092036,9.03951954568884,
-262.871323529412));
#161723=CARTESIAN_POINT('Ctrl Pts',(-11.132623567824,10.148727336345,-264.365441176471));
#161724=CARTESIAN_POINT('Ctrl Pts',(-10.1054346546984,11.0851337583099,
-265.859558823529));
#161725=CARTESIAN_POINT('Ctrl Pts',(-9.07824574157275,12.0215401802748,
-267.353676470588));
#161726=CARTESIAN_POINT('Ctrl Pts',(-7.89648244316034,12.7532570359442,
-268.847794117647));
#161727=CARTESIAN_POINT('Ctrl Pts',(-6.71471914474793,13.4849738916136,
-270.341911764706));
#161728=CARTESIAN_POINT('Ctrl Pts',(-5.41862499280729,13.9870834410653,
-271.836029411765));
#161729=CARTESIAN_POINT('Ctrl Pts',(-4.12253084086667,14.4891929905171,
-273.330147058823));
#161730=CARTESIAN_POINT('Ctrl Pts',(-2.75624276724856,14.7445964952585,
-274.824264705882));
#161731=CARTESIAN_POINT('Ctrl Pts',(-1.38995469363044,15.,-276.318382352941));
#161732=CARTESIAN_POINT('Ctrl Pts',(-1.83697019872103E-15,15.,-277.8125));
#161733=CARTESIAN_POINT('Ctrl Pts',(1.38995469363045,15.,-279.306617647059));
#161734=CARTESIAN_POINT('Ctrl Pts',(2.75624276724855,14.7445964952585,-280.800735294118));
#161735=CARTESIAN_POINT('Ctrl Pts',(4.12253084086666,14.4891929905171,-282.294852941176));
#161736=CARTESIAN_POINT('Ctrl Pts',(5.4186249928073,13.9870834410653,-283.788970588235));
#161737=CARTESIAN_POINT('Ctrl Pts',(6.71471914474792,13.4849738916136,-285.283088235294));
#161738=CARTESIAN_POINT('Ctrl Pts',(7.89648244316034,12.7532570359442,-286.777205882353));
#161739=CARTESIAN_POINT('Ctrl Pts',(9.07824574157275,12.0215401802748,-288.271323529412));
#161740=CARTESIAN_POINT('Ctrl Pts',(10.1054346546984,11.0851337583099,-289.765441176471));
#161741=CARTESIAN_POINT('Ctrl Pts',(11.132623567824,10.148727336345,-291.259558823529));
#161742=CARTESIAN_POINT('Ctrl Pts',(11.9702584092036,9.03951954568885,-292.753676470588));
#161743=CARTESIAN_POINT('Ctrl Pts',(12.8078932505832,7.93031175503273,-294.247794117647));
#161744=CARTESIAN_POINT('Ctrl Pts',(13.4274493703259,6.68607533664807,-295.741911764706));
#161745=CARTESIAN_POINT('Ctrl Pts',(14.0470054900687,5.44183891826343,-297.236029411765));
#161746=CARTESIAN_POINT('Ctrl Pts',(14.4273846475923,4.10494485108125,-298.730147058823));
#161747=CARTESIAN_POINT('Ctrl Pts',(14.8077638051159,2.76805078389905,-300.224264705882));
#161748=CARTESIAN_POINT('Ctrl Pts',(14.9360126444255,1.38402539194953,-301.718382352941));
#161749=CARTESIAN_POINT('Ctrl Pts',(15.0642614837351,2.76725994113625E-15,
-303.2125));
#161750=CARTESIAN_POINT('Ctrl Pts',(14.9360126444255,-1.38402539194952,
-304.706617647059));
#161751=CARTESIAN_POINT('Ctrl Pts',(14.8077638051159,-2.76805078389906,
-306.200735294118));
#161752=CARTESIAN_POINT('Ctrl Pts',(14.4273846475923,-4.10494485108124,
-307.694852941176));
#161753=CARTESIAN_POINT('Ctrl Pts',(14.0470054900687,-5.44183891826342,
-309.188970588235));
#161754=CARTESIAN_POINT('Ctrl Pts',(13.4274493703259,-6.68607533664808,
-310.683088235294));
#161755=CARTESIAN_POINT('Ctrl Pts',(12.8078932505832,-7.93031175503273,
-312.177205882353));
#161756=CARTESIAN_POINT('Ctrl Pts',(11.9702584092036,-9.03951954568884,
-313.671323529412));
#161757=CARTESIAN_POINT('Ctrl Pts',(11.132623567824,-10.148727336345,-315.165441176471));
#161758=CARTESIAN_POINT('Ctrl Pts',(10.1054346546984,-11.0851337583099,
-316.659558823529));
#161759=CARTESIAN_POINT('Ctrl Pts',(9.07824574157275,-12.0215401802748,
-318.153676470588));
#161760=CARTESIAN_POINT('Ctrl Pts',(7.89648244316034,-12.7532570359442,
-319.647794117647));
#161761=CARTESIAN_POINT('Ctrl Pts',(6.71471914474792,-13.4849738916136,
-321.141911764706));
#161762=CARTESIAN_POINT('Ctrl Pts',(5.4186249928073,-13.9870834410653,-322.636029411765));
#161763=CARTESIAN_POINT('Ctrl Pts',(4.12253084086667,-14.4891929905171,
-324.130147058824));
#161764=CARTESIAN_POINT('Ctrl Pts',(2.75624276724855,-14.7445964952585,
-325.624264705882));
#161765=CARTESIAN_POINT('Ctrl Pts',(1.38995469363045,-15.,-327.118382352941));
#161766=CARTESIAN_POINT('Ctrl Pts',(0.,-15.,-328.6125));
#161767=CARTESIAN_POINT('Ctrl Pts',(-1.38995469363045,-15.,-330.106617647059));
#161768=CARTESIAN_POINT('Ctrl Pts',(-2.75624276724856,-14.7445964952585,
-331.600735294118));
#161769=CARTESIAN_POINT('Ctrl Pts',(-4.12253084086666,-14.4891929905171,
-333.094852941176));
#161770=CARTESIAN_POINT('Ctrl Pts',(-5.41862499280729,-13.9870834410653,
-334.588970588235));
#161771=CARTESIAN_POINT('Ctrl Pts',(-6.71471914474793,-13.4849738916136,
-336.083088235294));
#161772=CARTESIAN_POINT('Ctrl Pts',(-7.89648244316034,-12.7532570359442,
-337.577205882353));
#161773=CARTESIAN_POINT('Ctrl Pts',(-9.07824574157275,-12.0215401802748,
-339.071323529412));
#161774=CARTESIAN_POINT('Ctrl Pts',(-10.1054346546984,-11.0851337583099,
-340.56544117647));
#161775=CARTESIAN_POINT('Ctrl Pts',(-11.132623567824,-10.148727336345,-342.059558823529));
#161776=CARTESIAN_POINT('Ctrl Pts',(-11.9702584092036,-9.03951954568885,
-343.553676470588));
#161777=CARTESIAN_POINT('Ctrl Pts',(-12.8078932505832,-7.93031175503273,
-345.047794117647));
#161778=CARTESIAN_POINT('Ctrl Pts',(-13.4274493703259,-6.68607533664808,
-346.541911764706));
#161779=CARTESIAN_POINT('Ctrl Pts',(-14.0470054900687,-5.44183891826343,
-348.036029411765));
#161780=CARTESIAN_POINT('Ctrl Pts',(-14.4273846475923,-4.10494485108124,
-349.530147058823));
#161781=CARTESIAN_POINT('Ctrl Pts',(-14.8077638051159,-2.76805078389906,
-351.024264705883));
#161782=CARTESIAN_POINT('Ctrl Pts',(-14.9360126444255,-1.38402539194953,
-352.518382352941));
#161783=CARTESIAN_POINT('Ctrl Pts',(-15.0642614837351,-9.22419980378748E-16,
-354.0125));
#161784=CARTESIAN_POINT('Ctrl Pts',(-14.9360126444255,1.38402539194953,
-355.506617647059));
#161785=CARTESIAN_POINT('Ctrl Pts',(-14.8077638051159,2.76805078389906,
-357.000735294118));
#161786=CARTESIAN_POINT('Ctrl Pts',(-14.4273846475923,4.10494485108124,
-358.494852941176));
#161787=CARTESIAN_POINT('Ctrl Pts',(-14.0470054900687,5.44183891826343,
-359.988970588235));
#161788=CARTESIAN_POINT('Ctrl Pts',(-13.4274493703259,6.68607533664807,
-361.483088235294));
#161789=CARTESIAN_POINT('Ctrl Pts',(-12.8078932505832,7.93031175503273,
-362.977205882353));
#161790=CARTESIAN_POINT('Ctrl Pts',(-11.9702584092036,9.03951954568884,
-364.471323529412));
#161791=CARTESIAN_POINT('Ctrl Pts',(-11.132623567824,10.148727336345,-365.965441176471));
#161792=CARTESIAN_POINT('Ctrl Pts',(-10.1054346546984,11.0851337583099,
-367.459558823529));
#161793=CARTESIAN_POINT('Ctrl Pts',(-9.07824574157275,12.0215401802748,
-368.953676470588));
#161794=CARTESIAN_POINT('Ctrl Pts',(-7.89648244316034,12.7532570359442,
-370.447794117647));
#161795=CARTESIAN_POINT('Ctrl Pts',(-6.71471914474793,13.4849738916136,
-371.941911764706));
#161796=CARTESIAN_POINT('Ctrl Pts',(-5.41862499280729,13.9870834410653,
-373.436029411765));
#161797=CARTESIAN_POINT('Ctrl Pts',(-4.12253084086667,14.4891929905171,
-374.930147058824));
#161798=CARTESIAN_POINT('Ctrl Pts',(-2.75624276724856,14.7445964952585,
-376.424264705882));
#161799=CARTESIAN_POINT('Ctrl Pts',(-1.38995469363044,15.,-377.918382352941));
#161800=CARTESIAN_POINT('Ctrl Pts',(-1.83697019872103E-15,15.,-379.4125));
#161801=CARTESIAN_POINT('Ctrl Pts',(1.38995469363045,15.,-380.906617647059));
#161802=CARTESIAN_POINT('Ctrl Pts',(2.75624276724855,14.7445964952585,-382.400735294118));
#161803=CARTESIAN_POINT('Ctrl Pts',(4.12253084086666,14.4891929905171,-383.894852941177));
#161804=CARTESIAN_POINT('Ctrl Pts',(5.4186249928073,13.9870834410653,-385.388970588235));
#161805=CARTESIAN_POINT('Ctrl Pts',(6.71471914474792,13.4849738916136,-386.883088235294));
#161806=CARTESIAN_POINT('Ctrl Pts',(7.89648244316034,12.7532570359442,-388.377205882353));
#161807=CARTESIAN_POINT('Ctrl Pts',(9.07824574157275,12.0215401802748,-389.871323529412));
#161808=CARTESIAN_POINT('Ctrl Pts',(10.1054346546984,11.0851337583099,-391.365441176471));
#161809=CARTESIAN_POINT('Ctrl Pts',(11.132623567824,10.148727336345,-392.859558823529));
#161810=CARTESIAN_POINT('Ctrl Pts',(11.9702584092036,9.03951954568885,-394.353676470588));
#161811=CARTESIAN_POINT('Ctrl Pts',(12.8078932505832,7.93031175503273,-395.847794117647));
#161812=CARTESIAN_POINT('Ctrl Pts',(13.4274493703259,6.68607533664807,-397.341911764706));
#161813=CARTESIAN_POINT('Ctrl Pts',(14.0470054900687,5.44183891826343,-398.836029411765));
#161814=CARTESIAN_POINT('Ctrl Pts',(14.4273846475923,4.10494485108125,-400.330147058823));
#161815=CARTESIAN_POINT('Ctrl Pts',(14.8077638051159,2.76805078389905,-401.824264705882));
#161816=CARTESIAN_POINT('Ctrl Pts',(14.9360126444255,1.38402539194953,-403.318382352941));
#161817=CARTESIAN_POINT('Ctrl Pts',(15.0642614837351,2.76725994113625E-15,
-404.8125));
#161818=CARTESIAN_POINT('Ctrl Pts',(14.9360126444255,-1.38402539194952,
-406.306617647059));
#161819=CARTESIAN_POINT('Ctrl Pts',(14.8077638051159,-2.76805078389906,
-407.800735294118));
#161820=CARTESIAN_POINT('Ctrl Pts',(14.4273846475923,-4.10494485108124,
-409.294852941176));
#161821=CARTESIAN_POINT('Ctrl Pts',(14.0470054900687,-5.44183891826342,
-410.788970588235));
#161822=CARTESIAN_POINT('Ctrl Pts',(13.4274493703259,-6.68607533664808,
-412.283088235294));
#161823=CARTESIAN_POINT('Ctrl Pts',(12.8078932505832,-7.93031175503273,
-413.777205882353));
#161824=CARTESIAN_POINT('Ctrl Pts',(11.9702584092036,-9.03951954568884,
-415.271323529412));
#161825=CARTESIAN_POINT('Ctrl Pts',(11.132623567824,-10.148727336345,-416.765441176471));
#161826=CARTESIAN_POINT('Ctrl Pts',(10.1054346546984,-11.0851337583099,
-418.259558823529));
#161827=CARTESIAN_POINT('Ctrl Pts',(9.07824574157275,-12.0215401802748,
-419.753676470588));
#161828=CARTESIAN_POINT('Ctrl Pts',(7.89648244316034,-12.7532570359442,
-421.247794117647));
#161829=CARTESIAN_POINT('Ctrl Pts',(6.71471914474792,-13.4849738916136,
-422.741911764706));
#161830=CARTESIAN_POINT('Ctrl Pts',(5.4186249928073,-13.9870834410653,-424.236029411765));
#161831=CARTESIAN_POINT('Ctrl Pts',(4.12253084086667,-14.4891929905171,
-425.730147058824));
#161832=CARTESIAN_POINT('Ctrl Pts',(2.75624276724855,-14.7445964952585,
-427.224264705882));
#161833=CARTESIAN_POINT('Ctrl Pts',(1.38995469363045,-15.,-428.718382352941));
#161834=CARTESIAN_POINT('Ctrl Pts',(0.,-15.,-430.2125));
#161835=CARTESIAN_POINT('Ctrl Pts',(-1.38995469363045,-15.,-431.706617647059));
#161836=CARTESIAN_POINT('Ctrl Pts',(-2.75624276724856,-14.7445964952585,
-433.200735294118));
#161837=CARTESIAN_POINT('Ctrl Pts',(-4.12253084086666,-14.4891929905171,
-434.694852941176));
#161838=CARTESIAN_POINT('Ctrl Pts',(-5.41862499280729,-13.9870834410653,
-436.188970588235));
#161839=CARTESIAN_POINT('Ctrl Pts',(-6.71471914474793,-13.4849738916136,
-437.683088235294));
#161840=CARTESIAN_POINT('Ctrl Pts',(-7.89648244316034,-12.7532570359442,
-439.177205882353));
#161841=CARTESIAN_POINT('Ctrl Pts',(-9.07824574157275,-12.0215401802748,
-440.671323529412));
#161842=CARTESIAN_POINT('Ctrl Pts',(-10.1054346546984,-11.0851337583099,
-442.165441176471));
#161843=CARTESIAN_POINT('Ctrl Pts',(-11.132623567824,-10.148727336345,-443.65955882353));
#161844=CARTESIAN_POINT('Ctrl Pts',(-11.9702584092036,-9.03951954568885,
-445.153676470588));
#161845=CARTESIAN_POINT('Ctrl Pts',(-12.8078932505832,-7.93031175503273,
-446.647794117647));
#161846=CARTESIAN_POINT('Ctrl Pts',(-13.4274493703259,-6.68607533664808,
-448.141911764706));
#161847=CARTESIAN_POINT('Ctrl Pts',(-14.0470054900687,-5.44183891826343,
-449.636029411765));
#161848=CARTESIAN_POINT('Ctrl Pts',(-14.4273846475923,-4.10494485108124,
-451.130147058824));
#161849=CARTESIAN_POINT('Ctrl Pts',(-14.8077638051159,-2.76805078389906,
-452.624264705882));
#161850=CARTESIAN_POINT('Ctrl Pts',(-14.9360126444255,-1.38402539194953,
-454.118382352941));
#161851=CARTESIAN_POINT('Ctrl Pts',(-15.0642614837351,-9.22419980378748E-16,
-455.6125));
#161852=CARTESIAN_POINT('Ctrl Pts',(-14.9360126444255,1.38402539194953,
-457.106617647059));
#161853=CARTESIAN_POINT('Ctrl Pts',(-14.8077638051159,2.76805078389906,
-458.600735294118));
#161854=CARTESIAN_POINT('Ctrl Pts',(-14.4273846475923,4.10494485108124,
-460.094852941176));
#161855=CARTESIAN_POINT('Ctrl Pts',(-14.0470054900687,5.44183891826343,
-461.588970588235));
#161856=CARTESIAN_POINT('Ctrl Pts',(-13.4274493703259,6.68607533664807,
-463.083088235294));
#161857=CARTESIAN_POINT('Ctrl Pts',(-12.8078932505832,7.93031175503273,
-464.577205882353));
#161858=CARTESIAN_POINT('Ctrl Pts',(-11.9702584092036,9.03951954568884,
-466.071323529412));
#161859=CARTESIAN_POINT('Ctrl Pts',(-11.132623567824,10.148727336345,-467.565441176471));
#161860=CARTESIAN_POINT('Ctrl Pts',(-10.1054346546984,11.0851337583099,
-469.059558823529));
#161861=CARTESIAN_POINT('Ctrl Pts',(-9.07824574157275,12.0215401802748,
-470.553676470588));
#161862=CARTESIAN_POINT('Ctrl Pts',(-7.89648244316034,12.7532570359442,
-472.047794117647));
#161863=CARTESIAN_POINT('Ctrl Pts',(-6.71471914474793,13.4849738916136,
-473.541911764706));
#161864=CARTESIAN_POINT('Ctrl Pts',(-5.41862499280729,13.9870834410653,
-475.036029411765));
#161865=CARTESIAN_POINT('Ctrl Pts',(-4.12253084086667,14.4891929905171,
-476.530147058824));
#161866=CARTESIAN_POINT('Ctrl Pts',(-2.75624276724856,14.7445964952585,
-478.024264705882));
#161867=CARTESIAN_POINT('Ctrl Pts',(-1.38995469363044,15.,-479.518382352941));
#161868=CARTESIAN_POINT('Ctrl Pts',(-1.83697019872103E-15,15.,-481.0125));
#161869=CARTESIAN_POINT('Ctrl Pts',(1.38995469363045,15.,-482.506617647059));
#161870=CARTESIAN_POINT('Ctrl Pts',(2.75624276724855,14.7445964952585,-484.000735294118));
#161871=CARTESIAN_POINT('Ctrl Pts',(4.12253084086666,14.4891929905171,-485.494852941177));
#161872=CARTESIAN_POINT('Ctrl Pts',(5.4186249928073,13.9870834410653,-486.988970588235));
#161873=CARTESIAN_POINT('Ctrl Pts',(6.71471914474792,13.4849738916136,-488.483088235294));
#161874=CARTESIAN_POINT('Ctrl Pts',(7.89648244316034,12.7532570359442,-489.977205882353));
#161875=CARTESIAN_POINT('Ctrl Pts',(9.07824574157275,12.0215401802748,-491.471323529412));
#161876=CARTESIAN_POINT('Ctrl Pts',(10.1054346546984,11.0851337583099,-492.965441176471));
#161877=CARTESIAN_POINT('Ctrl Pts',(11.132623567824,10.148727336345,-494.45955882353));
#161878=CARTESIAN_POINT('Ctrl Pts',(11.9702584092036,9.03951954568885,-495.953676470588));
#161879=CARTESIAN_POINT('Ctrl Pts',(12.8078932505832,7.93031175503273,-497.447794117647));
#161880=CARTESIAN_POINT('Ctrl Pts',(13.4274493703259,6.68607533664807,-498.941911764706));
#161881=CARTESIAN_POINT('Ctrl Pts',(14.0470054900687,5.44183891826343,-500.436029411765));
#161882=CARTESIAN_POINT('Ctrl Pts',(14.4273846475923,4.10494485108125,-501.930147058824));
#161883=CARTESIAN_POINT('Ctrl Pts',(14.8077638051159,2.76805078389905,-503.424264705883));
#161884=CARTESIAN_POINT('Ctrl Pts',(14.9360126444255,1.38402539194953,-504.918382352941));
#161885=CARTESIAN_POINT('Ctrl Pts',(15.0642614837351,2.76725994113625E-15,
-506.4125));
#161886=CARTESIAN_POINT('Ctrl Pts',(14.9360126444255,-1.38402539194952,
-507.906617647059));
#161887=CARTESIAN_POINT('Ctrl Pts',(14.8077638051159,-2.76805078389906,
-509.400735294117));
#161888=CARTESIAN_POINT('Ctrl Pts',(14.4273846475923,-4.10494485108124,
-510.894852941176));
#161889=CARTESIAN_POINT('Ctrl Pts',(14.0470054900687,-5.44183891826342,
-512.388970588235));
#161890=CARTESIAN_POINT('Ctrl Pts',(13.4274493703259,-6.68607533664808,
-513.883088235294));
#161891=CARTESIAN_POINT('Ctrl Pts',(12.8078932505832,-7.93031175503273,
-515.377205882353));
#161892=CARTESIAN_POINT('Ctrl Pts',(11.9702584092036,-9.03951954568884,
-516.871323529412));
#161893=CARTESIAN_POINT('Ctrl Pts',(11.132623567824,-10.148727336345,-518.365441176471));
#161894=CARTESIAN_POINT('Ctrl Pts',(10.1054346546984,-11.0851337583099,
-519.85955882353));
#161895=CARTESIAN_POINT('Ctrl Pts',(9.07824574157275,-12.0215401802748,
-521.353676470588));
#161896=CARTESIAN_POINT('Ctrl Pts',(7.89648244316034,-12.7532570359442,
-522.847794117647));
#161897=CARTESIAN_POINT('Ctrl Pts',(6.71471914474792,-13.4849738916136,
-524.341911764706));
#161898=CARTESIAN_POINT('Ctrl Pts',(5.4186249928073,-13.9870834410653,-525.836029411765));
#161899=CARTESIAN_POINT('Ctrl Pts',(4.12253084086667,-14.4891929905171,
-527.330147058823));
#161900=CARTESIAN_POINT('Ctrl Pts',(2.75624276724855,-14.7445964952585,
-528.824264705882));
#161901=CARTESIAN_POINT('Ctrl Pts',(1.38995469363045,-15.,-530.318382352941));
#161902=CARTESIAN_POINT('Ctrl Pts',(0.,-15.,-531.8125));
#161903=CARTESIAN_POINT('Ctrl Pts',(-1.38995469363045,-15.,-533.306617647059));
#161904=CARTESIAN_POINT('Ctrl Pts',(-2.75624276724856,-14.7445964952585,
-534.800735294118));
#161905=CARTESIAN_POINT('Ctrl Pts',(-4.12253084086666,-14.4891929905171,
-536.294852941177));
#161906=CARTESIAN_POINT('Ctrl Pts',(-5.41862499280729,-13.9870834410653,
-537.788970588235));
#161907=CARTESIAN_POINT('Ctrl Pts',(-6.71471914474793,-13.4849738916136,
-539.283088235294));
#161908=CARTESIAN_POINT('Ctrl Pts',(-7.89648244316034,-12.7532570359442,
-540.777205882353));
#161909=CARTESIAN_POINT('Ctrl Pts',(-9.07824574157275,-12.0215401802748,
-542.271323529412));
#161910=CARTESIAN_POINT('Ctrl Pts',(-10.1054346546984,-11.0851337583099,
-543.765441176471));
#161911=CARTESIAN_POINT('Ctrl Pts',(-11.132623567824,-10.148727336345,-545.259558823529));
#161912=CARTESIAN_POINT('Ctrl Pts',(-11.9702584092036,-9.03951954568885,
-546.753676470588));
#161913=CARTESIAN_POINT('Ctrl Pts',(-12.8078932505832,-7.93031175503273,
-548.247794117647));
#161914=CARTESIAN_POINT('Ctrl Pts',(-13.4274493703259,-6.68607533664808,
-549.741911764706));
#161915=CARTESIAN_POINT('Ctrl Pts',(-14.0470054900687,-5.44183891826343,
-551.236029411765));
#161916=CARTESIAN_POINT('Ctrl Pts',(-14.4273846475923,-4.10494485108124,
-552.730147058823));
#161917=CARTESIAN_POINT('Ctrl Pts',(-14.8077638051159,-2.76805078389906,
-554.224264705882));
#161918=CARTESIAN_POINT('Ctrl Pts',(-14.9360126444255,-1.38402539194953,
-555.718382352941));
#161919=CARTESIAN_POINT('Ctrl Pts',(-15.0642614837351,-9.22419980378748E-16,
-557.2125));
#161920=CARTESIAN_POINT('Ctrl Pts',(-14.9360126444255,1.38402539194953,
-558.706617647059));
#161921=CARTESIAN_POINT('Ctrl Pts',(-14.8077638051159,2.76805078389906,
-560.200735294118));
#161922=CARTESIAN_POINT('Ctrl Pts',(-14.4273846475923,4.10494485108124,
-561.694852941176));
#161923=CARTESIAN_POINT('Ctrl Pts',(-14.0470054900687,5.44183891826343,
-563.188970588235));
#161924=CARTESIAN_POINT('Ctrl Pts',(-13.4274493703259,6.68607533664807,
-564.683088235294));
#161925=CARTESIAN_POINT('Ctrl Pts',(-12.8078932505832,7.93031175503273,
-566.177205882353));
#161926=CARTESIAN_POINT('Ctrl Pts',(-11.9702584092036,9.03951954568884,
-567.671323529412));
#161927=CARTESIAN_POINT('Ctrl Pts',(-11.132623567824,10.148727336345,-569.16544117647));
#161928=CARTESIAN_POINT('Ctrl Pts',(-10.1054346546984,11.0851337583099,
-570.659558823529));
#161929=CARTESIAN_POINT('Ctrl Pts',(-9.07824574157275,12.0215401802748,
-572.153676470588));
#161930=CARTESIAN_POINT('Ctrl Pts',(-7.89648244316034,12.7532570359442,
-573.647794117647));
#161931=CARTESIAN_POINT('Ctrl Pts',(-6.71471914474793,13.4849738916136,
-575.141911764706));
#161932=CARTESIAN_POINT('Ctrl Pts',(-5.41862499280729,13.9870834410653,
-576.636029411765));
#161933=CARTESIAN_POINT('Ctrl Pts',(-4.12253084086667,14.4891929905171,
-578.130147058824));
#161934=CARTESIAN_POINT('Ctrl Pts',(-2.75624276724856,14.7445964952585,
-579.624264705882));
#161935=CARTESIAN_POINT('Ctrl Pts',(-1.38995469363044,15.,-581.118382352941));
#161936=CARTESIAN_POINT('Ctrl Pts',(-1.83697019872103E-15,15.,-582.6125));
#161937=CARTESIAN_POINT('Ctrl Pts',(1.38995469363045,15.,-584.106617647059));
#161938=CARTESIAN_POINT('Ctrl Pts',(2.75624276724855,14.7445964952585,-585.600735294117));
#161939=CARTESIAN_POINT('Ctrl Pts',(4.12253084086666,14.4891929905171,-587.094852941176));
#161940=CARTESIAN_POINT('Ctrl Pts',(5.4186249928073,13.9870834410653,-588.588970588235));
#161941=CARTESIAN_POINT('Ctrl Pts',(6.71471914474792,13.4849738916136,-590.083088235294));
#161942=CARTESIAN_POINT('Ctrl Pts',(7.89648244316034,12.7532570359442,-591.577205882353));
#161943=CARTESIAN_POINT('Ctrl Pts',(9.07824574157275,12.0215401802748,-593.071323529412));
#161944=CARTESIAN_POINT('Ctrl Pts',(10.1054346546984,11.0851337583099,-594.565441176471));
#161945=CARTESIAN_POINT('Ctrl Pts',(11.132623567824,10.148727336345,-596.05955882353));
#161946=CARTESIAN_POINT('Ctrl Pts',(11.9702584092036,9.03951954568885,-597.553676470588));
#161947=CARTESIAN_POINT('Ctrl Pts',(12.8078932505832,7.93031175503273,-599.047794117647));
#161948=CARTESIAN_POINT('Ctrl Pts',(13.4274493703259,6.68607533664807,-600.541911764706));
#161949=CARTESIAN_POINT('Ctrl Pts',(14.0470054900687,5.44183891826343,-602.036029411765));
#161950=CARTESIAN_POINT('Ctrl Pts',(14.4273846475923,4.10494485108125,-603.530147058823));
#161951=CARTESIAN_POINT('Ctrl Pts',(14.8077638051159,2.76805078389905,-605.024264705882));
#161952=CARTESIAN_POINT('Ctrl Pts',(14.9360126444255,1.38402539194953,-606.518382352941));
#161953=CARTESIAN_POINT('Ctrl Pts',(15.0642614837351,2.76725994113625E-15,
-608.0125));
#161954=CARTESIAN_POINT('Ctrl Pts',(14.9360126444255,-1.38402539194952,
-609.506617647059));
#161955=CARTESIAN_POINT('Ctrl Pts',(14.8077638051159,-2.76805078389906,
-611.000735294118));
#161956=CARTESIAN_POINT('Ctrl Pts',(14.4273846475923,-4.10494485108124,
-612.494852941176));
#161957=CARTESIAN_POINT('Ctrl Pts',(14.0470054900687,-5.44183891826342,
-613.988970588235));
#161958=CARTESIAN_POINT('Ctrl Pts',(13.4274493703259,-6.68607533664808,
-615.483088235294));
#161959=CARTESIAN_POINT('Ctrl Pts',(12.8078932505832,-7.93031175503273,
-616.977205882353));
#161960=CARTESIAN_POINT('Ctrl Pts',(11.9702584092036,-9.03951954568884,
-618.471323529412));
#161961=CARTESIAN_POINT('Ctrl Pts',(11.132623567824,-10.148727336345,-619.96544117647));
#161962=CARTESIAN_POINT('Ctrl Pts',(10.1054346546984,-11.0851337583099,
-621.459558823529));
#161963=CARTESIAN_POINT('Ctrl Pts',(9.07824574157275,-12.0215401802748,
-622.953676470588));
#161964=CARTESIAN_POINT('Ctrl Pts',(7.89648244316034,-12.7532570359442,
-624.447794117647));
#161965=CARTESIAN_POINT('Ctrl Pts',(6.71471914474792,-13.4849738916136,
-625.941911764706));
#161966=CARTESIAN_POINT('Ctrl Pts',(5.4186249928073,-13.9870834410653,-627.436029411764));
#161967=CARTESIAN_POINT('Ctrl Pts',(4.12253084086667,-14.4891929905171,
-628.930147058823));
#161968=CARTESIAN_POINT('Ctrl Pts',(2.75624276724855,-14.7445964952585,
-630.424264705882));
#161969=CARTESIAN_POINT('Ctrl Pts',(1.38995469363045,-15.,-631.918382352941));
#161970=CARTESIAN_POINT('Ctrl Pts',(0.,-15.,-633.4125));
#161971=CARTESIAN_POINT('Ctrl Pts',(-1.38995469363045,-15.,-634.906617647059));
#161972=CARTESIAN_POINT('Ctrl Pts',(-2.75624276724856,-14.7445964952585,
-636.400735294118));
#161973=CARTESIAN_POINT('Ctrl Pts',(-4.12253084086666,-14.4891929905171,
-637.894852941177));
#161974=CARTESIAN_POINT('Ctrl Pts',(-5.41862499280729,-13.9870834410653,
-639.388970588235));
#161975=CARTESIAN_POINT('Ctrl Pts',(-6.71471914474793,-13.4849738916136,
-640.883088235294));
#161976=CARTESIAN_POINT('Ctrl Pts',(-7.89648244316034,-12.7532570359442,
-642.377205882353));
#161977=CARTESIAN_POINT('Ctrl Pts',(-9.07824574157275,-12.0215401802748,
-643.871323529412));
#161978=CARTESIAN_POINT('Ctrl Pts',(-10.1054346546984,-11.0851337583099,
-645.36544117647));
#161979=CARTESIAN_POINT('Ctrl Pts',(-11.132623567824,-10.148727336345,-646.859558823529));
#161980=CARTESIAN_POINT('Ctrl Pts',(-11.9702584092036,-9.03951954568885,
-648.353676470588));
#161981=CARTESIAN_POINT('Ctrl Pts',(-12.8078932505832,-7.93031175503273,
-649.847794117647));
#161982=CARTESIAN_POINT('Ctrl Pts',(-13.4274493703259,-6.68607533664808,
-651.341911764706));
#161983=CARTESIAN_POINT('Ctrl Pts',(-14.0470054900687,-5.44183891826343,
-652.836029411765));
#161984=CARTESIAN_POINT('Ctrl Pts',(-14.4273846475923,-4.10494485108124,
-654.330147058824));
#161985=CARTESIAN_POINT('Ctrl Pts',(-14.8077638051159,-2.76805078389906,
-655.824264705882));
#161986=CARTESIAN_POINT('Ctrl Pts',(-14.9360126444255,-1.38402539194953,
-657.318382352941));
#161987=CARTESIAN_POINT('Ctrl Pts',(-15.0642614837351,-9.22419980378748E-16,
-658.8125));
#161988=CARTESIAN_POINT('Ctrl Pts',(-14.9360126444255,1.38402539194953,
-660.306617647059));
#161989=CARTESIAN_POINT('Ctrl Pts',(-14.8077638051159,2.76805078389906,
-661.800735294117));
#161990=CARTESIAN_POINT('Ctrl Pts',(-14.4273846475923,4.10494485108124,
-663.294852941176));
#161991=CARTESIAN_POINT('Ctrl Pts',(-14.0470054900687,5.44183891826343,
-664.788970588236));
#161992=CARTESIAN_POINT('Ctrl Pts',(-13.4274493703259,6.68607533664807,
-666.283088235294));
#161993=CARTESIAN_POINT('Ctrl Pts',(-12.8078932505832,7.93031175503273,
-667.777205882353));
#161994=CARTESIAN_POINT('Ctrl Pts',(-11.9702584092036,9.03951954568884,
-669.271323529412));
#161995=CARTESIAN_POINT('Ctrl Pts',(-11.132623567824,10.148727336345,-670.765441176471));
#161996=CARTESIAN_POINT('Ctrl Pts',(-10.1054346546984,11.0851337583099,
-672.259558823529));
#161997=CARTESIAN_POINT('Ctrl Pts',(-9.07824574157275,12.0215401802748,
-673.753676470588));
#161998=CARTESIAN_POINT('Ctrl Pts',(-7.89648244316034,12.7532570359442,
-675.247794117647));
#161999=CARTESIAN_POINT('Ctrl Pts',(-6.71471914474793,13.4849738916136,
-676.741911764706));
#162000=CARTESIAN_POINT('Ctrl Pts',(-5.41862499280729,13.9870834410653,
-678.236029411765));
#162001=CARTESIAN_POINT('Ctrl Pts',(-4.12253084086667,14.4891929905171,
-679.730147058824));
#162002=CARTESIAN_POINT('Ctrl Pts',(-2.75624276724856,14.7445964952585,
-681.224264705883));
#162003=CARTESIAN_POINT('Ctrl Pts',(-1.38995469363044,15.,-682.718382352941));
#162004=CARTESIAN_POINT('Ctrl Pts',(-1.83697019872103E-15,15.,-684.2125));
#162005=CARTESIAN_POINT('Ctrl Pts',(1.38995469363045,15.,-685.706617647059));
#162006=CARTESIAN_POINT('Ctrl Pts',(2.75624276724855,14.7445964952585,-687.200735294118));
#162007=CARTESIAN_POINT('Ctrl Pts',(4.12253084086666,14.4891929905171,-688.694852941176));
#162008=CARTESIAN_POINT('Ctrl Pts',(5.4186249928073,13.9870834410653,-690.188970588235));
#162009=CARTESIAN_POINT('Ctrl Pts',(6.71471914474792,13.4849738916136,-691.683088235294));
#162010=CARTESIAN_POINT('Ctrl Pts',(7.89648244316034,12.7532570359442,-693.177205882353));
#162011=CARTESIAN_POINT('Ctrl Pts',(9.07824574157275,12.0215401802748,-694.671323529412));
#162012=CARTESIAN_POINT('Ctrl Pts',(10.1054346546984,11.0851337583099,-696.165441176471));
#162013=CARTESIAN_POINT('Ctrl Pts',(11.132623567824,10.148727336345,-697.659558823529));
#162014=CARTESIAN_POINT('Ctrl Pts',(11.9702584092036,9.03951954568885,-699.153676470588));
#162015=CARTESIAN_POINT('Ctrl Pts',(12.8078932505832,7.93031175503273,-700.647794117647));
#162016=CARTESIAN_POINT('Ctrl Pts',(13.4274493703259,6.68607533664807,-702.141911764706));
#162017=CARTESIAN_POINT('Ctrl Pts',(14.0470054900687,5.44183891826343,-703.636029411765));
#162018=CARTESIAN_POINT('Ctrl Pts',(14.4273846475923,4.10494485108125,-705.130147058823));
#162019=CARTESIAN_POINT('Ctrl Pts',(14.8077638051159,2.76805078389905,-706.624264705882));
#162020=CARTESIAN_POINT('Ctrl Pts',(14.9360126444255,1.38402539194953,-708.118382352941));
#162021=CARTESIAN_POINT('Ctrl Pts',(15.0642614837351,2.76725994113625E-15,
-709.6125));
#162022=CARTESIAN_POINT('Ctrl Pts',(14.9360126444255,-1.38402539194952,
-711.106617647059));
#162023=CARTESIAN_POINT('Ctrl Pts',(14.8077638051159,-2.76805078389906,
-712.600735294118));
#162024=CARTESIAN_POINT('Ctrl Pts',(14.4273846475923,-4.10494485108124,
-714.094852941177));
#162025=CARTESIAN_POINT('Ctrl Pts',(14.0470054900687,-5.44183891826342,
-715.588970588235));
#162026=CARTESIAN_POINT('Ctrl Pts',(13.4274493703259,-6.68607533664808,
-717.083088235294));
#162027=CARTESIAN_POINT('Ctrl Pts',(12.8078932505832,-7.93031175503273,
-718.577205882353));
#162028=CARTESIAN_POINT('Ctrl Pts',(11.9702584092036,-9.03951954568884,
-720.071323529412));
#162029=CARTESIAN_POINT('Ctrl Pts',(11.132623567824,-10.148727336345,-721.56544117647));
#162030=CARTESIAN_POINT('Ctrl Pts',(10.1054346546984,-11.0851337583099,
-723.059558823529));
#162031=CARTESIAN_POINT('Ctrl Pts',(9.07824574157275,-12.0215401802748,
-724.553676470588));
#162032=CARTESIAN_POINT('Ctrl Pts',(7.89648244316034,-12.7532570359442,
-726.047794117647));
#162033=CARTESIAN_POINT('Ctrl Pts',(6.71471914474792,-13.4849738916136,
-727.541911764706));
#162034=CARTESIAN_POINT('Ctrl Pts',(5.4186249928073,-13.9870834410653,-729.036029411765));
#162035=CARTESIAN_POINT('Ctrl Pts',(4.12253084086667,-14.4891929905171,
-730.530147058824));
#162036=CARTESIAN_POINT('Ctrl Pts',(2.75624276724855,-14.7445964952585,
-732.024264705882));
#162037=CARTESIAN_POINT('Ctrl Pts',(1.38995469363045,-15.,-733.518382352941));
#162038=CARTESIAN_POINT('Ctrl Pts',(0.,-15.,-735.0125));
#162039=CARTESIAN_POINT('Ctrl Pts',(-1.38995469363045,-15.,-736.506617647059));
#162040=CARTESIAN_POINT('Ctrl Pts',(-2.75624276724856,-14.7445964952585,
-738.000735294118));
#162041=CARTESIAN_POINT('Ctrl Pts',(-4.12253084086666,-14.4891929905171,
-739.494852941177));
#162042=CARTESIAN_POINT('Ctrl Pts',(-5.41862499280729,-13.9870834410653,
-740.988970588235));
#162043=CARTESIAN_POINT('Ctrl Pts',(-6.71471914474793,-13.4849738916136,
-742.483088235294));
#162044=CARTESIAN_POINT('Ctrl Pts',(-7.89648244316034,-12.7532570359442,
-743.977205882353));
#162045=CARTESIAN_POINT('Ctrl Pts',(-9.07824574157275,-12.0215401802748,
-745.471323529412));
#162046=CARTESIAN_POINT('Ctrl Pts',(-10.1054346546984,-11.0851337583099,
-746.96544117647));
#162047=CARTESIAN_POINT('Ctrl Pts',(-11.132623567824,-10.148727336345,-748.459558823529));
#162048=CARTESIAN_POINT('Ctrl Pts',(-11.9702584092036,-9.03951954568885,
-749.953676470588));
#162049=CARTESIAN_POINT('Ctrl Pts',(-12.8078932505832,-7.93031175503273,
-751.447794117647));
#162050=CARTESIAN_POINT('Ctrl Pts',(-13.4274493703259,-6.68607533664808,
-752.941911764706));
#162051=CARTESIAN_POINT('Ctrl Pts',(-14.0470054900687,-5.44183891826343,
-754.436029411765));
#162052=CARTESIAN_POINT('Ctrl Pts',(-14.4273846475923,-4.10494485108124,
-755.930147058824));
#162053=CARTESIAN_POINT('Ctrl Pts',(-14.8077638051159,-2.76805078389906,
-757.424264705882));
#162054=CARTESIAN_POINT('Ctrl Pts',(-14.9360126444255,-1.38402539194953,
-758.918382352941));
#162055=CARTESIAN_POINT('Ctrl Pts',(-15.0642614837351,-9.22419980378748E-16,
-760.4125));
#162056=CARTESIAN_POINT('Ctrl Pts',(-14.9360126444255,1.38402539194953,
-761.906617647059));
#162057=CARTESIAN_POINT('Ctrl Pts',(-14.8077638051159,2.76805078389906,
-763.400735294118));
#162058=CARTESIAN_POINT('Ctrl Pts',(-14.4273846475923,4.10494485108124,
-764.894852941176));
#162059=CARTESIAN_POINT('Ctrl Pts',(-14.0470054900687,5.44183891826343,
-766.388970588235));
#162060=CARTESIAN_POINT('Ctrl Pts',(-13.4274493703259,6.68607533664807,
-767.883088235294));
#162061=CARTESIAN_POINT('Ctrl Pts',(-12.8078932505832,7.93031175503273,
-769.377205882353));
#162062=CARTESIAN_POINT('Ctrl Pts',(-11.9702584092036,9.03951954568884,
-770.871323529412));
#162063=CARTESIAN_POINT('Ctrl Pts',(-11.132623567824,10.148727336345,-772.365441176471));
#162064=CARTESIAN_POINT('Ctrl Pts',(-10.1054346546984,11.0851337583099,
-773.85955882353));
#162065=CARTESIAN_POINT('Ctrl Pts',(-9.07824574157275,12.0215401802748,
-775.353676470589));
#162066=CARTESIAN_POINT('Ctrl Pts',(-7.89648244316034,12.7532570359442,
-776.847794117647));
#162067=CARTESIAN_POINT('Ctrl Pts',(-6.71471914474793,13.4849738916136,
-778.341911764706));
#162068=CARTESIAN_POINT('Ctrl Pts',(-5.41862499280729,13.9870834410653,
-779.836029411765));
#162069=CARTESIAN_POINT('Ctrl Pts',(-4.12253084086667,14.4891929905171,
-781.330147058823));
#162070=CARTESIAN_POINT('Ctrl Pts',(-2.75624276724856,14.7445964952585,
-782.824264705882));
#162071=CARTESIAN_POINT('Ctrl Pts',(-1.38995469363044,15.,-784.318382352941));
#162072=CARTESIAN_POINT('Ctrl Pts',(-1.83697019872103E-15,15.,-785.8125));
#162073=CARTESIAN_POINT('Ctrl Pts',(1.38995469363045,15.,-787.306617647059));
#162074=CARTESIAN_POINT('Ctrl Pts',(2.75624276724855,14.7445964952585,-788.800735294118));
#162075=CARTESIAN_POINT('Ctrl Pts',(4.12253084086666,14.4891929905171,-790.294852941177));
#162076=CARTESIAN_POINT('Ctrl Pts',(5.4186249928073,13.9870834410653,-791.788970588235));
#162077=CARTESIAN_POINT('Ctrl Pts',(6.71471914474792,13.4849738916136,-793.283088235294));
#162078=CARTESIAN_POINT('Ctrl Pts',(7.89648244316034,12.7532570359442,-794.777205882353));
#162079=CARTESIAN_POINT('Ctrl Pts',(9.07824574157275,12.0215401802748,-796.271323529412));
#162080=CARTESIAN_POINT('Ctrl Pts',(10.1054346546984,11.0851337583099,-797.765441176471));
#162081=CARTESIAN_POINT('Ctrl Pts',(11.132623567824,10.148727336345,-799.259558823529));
#162082=CARTESIAN_POINT('Ctrl Pts',(11.9702584092036,9.03951954568885,-800.753676470588));
#162083=CARTESIAN_POINT('Ctrl Pts',(12.8078932505832,7.93031175503273,-802.247794117647));
#162084=CARTESIAN_POINT('Ctrl Pts',(13.4274493703259,6.68607533664807,-803.741911764706));
#162085=CARTESIAN_POINT('Ctrl Pts',(14.0470054900687,5.44183891826343,-805.236029411765));
#162086=CARTESIAN_POINT('Ctrl Pts',(14.4273846475923,4.10494485108125,-806.730147058823));
#162087=CARTESIAN_POINT('Ctrl Pts',(14.8077638051159,2.76805078389905,-808.224264705882));
#162088=CARTESIAN_POINT('Ctrl Pts',(14.9360126444255,1.38402539194953,-809.718382352941));
#162089=CARTESIAN_POINT('Ctrl Pts',(15.0642614837351,2.76725994113625E-15,
-811.2125));
#162090=CARTESIAN_POINT('Ctrl Pts',(14.9360126444255,-1.38402539194952,
-812.706617647059));
#162091=CARTESIAN_POINT('Ctrl Pts',(14.8077638051159,-2.76805078389906,
-814.200735294118));
#162092=CARTESIAN_POINT('Ctrl Pts',(14.4273846475923,-4.10494485108124,
-815.694852941177));
#162093=CARTESIAN_POINT('Ctrl Pts',(14.0470054900687,-5.44183891826342,
-817.188970588235));
#162094=CARTESIAN_POINT('Ctrl Pts',(13.4274493703259,-6.68607533664808,
-818.683088235294));
#162095=CARTESIAN_POINT('Ctrl Pts',(12.8078932505832,-7.93031175503273,
-820.177205882353));
#162096=CARTESIAN_POINT('Ctrl Pts',(11.9702584092036,-9.03951954568884,
-821.671323529412));
#162097=CARTESIAN_POINT('Ctrl Pts',(11.132623567824,-10.148727336345,-823.16544117647));
#162098=CARTESIAN_POINT('Ctrl Pts',(10.1054346546984,-11.0851337583099,
-824.659558823529));
#162099=CARTESIAN_POINT('Ctrl Pts',(9.07824574157275,-12.0215401802748,
-826.153676470588));
#162100=CARTESIAN_POINT('Ctrl Pts',(7.89648244316034,-12.7532570359442,
-827.647794117647));
#162101=CARTESIAN_POINT('Ctrl Pts',(6.71471914474792,-13.4849738916136,
-829.141911764706));
#162102=CARTESIAN_POINT('Ctrl Pts',(5.4186249928073,-13.9870834410653,-830.636029411765));
#162103=CARTESIAN_POINT('Ctrl Pts',(4.12253084086667,-14.4891929905171,
-832.130147058824));
#162104=CARTESIAN_POINT('Ctrl Pts',(2.75624276724855,-14.7445964952585,
-833.624264705883));
#162105=CARTESIAN_POINT('Ctrl Pts',(1.38995469363045,-15.,-835.118382352941));
#162106=CARTESIAN_POINT('Ctrl Pts',(0.,-15.,-836.6125));
#162107=CARTESIAN_POINT('Ctrl Pts',(-1.38995469363045,-15.,-838.106617647059));
#162108=CARTESIAN_POINT('Ctrl Pts',(-2.75624276724856,-14.7445964952585,
-839.600735294118));
#162109=CARTESIAN_POINT('Ctrl Pts',(-4.12253084086666,-14.4891929905171,
-841.094852941176));
#162110=CARTESIAN_POINT('Ctrl Pts',(-5.41862499280729,-13.9870834410653,
-842.588970588235));
#162111=CARTESIAN_POINT('Ctrl Pts',(-6.71471914474793,-13.4849738916136,
-844.083088235294));
#162112=CARTESIAN_POINT('Ctrl Pts',(-7.89648244316034,-12.7532570359442,
-845.577205882353));
#162113=CARTESIAN_POINT('Ctrl Pts',(-9.07824574157275,-12.0215401802748,
-847.071323529412));
#162114=CARTESIAN_POINT('Ctrl Pts',(-10.1054346546984,-11.0851337583099,
-848.565441176471));
#162115=CARTESIAN_POINT('Ctrl Pts',(-11.132623567824,-10.148727336345,-850.05955882353));
#162116=CARTESIAN_POINT('Ctrl Pts',(-11.9702584092036,-9.03951954568885,
-851.553676470588));
#162117=CARTESIAN_POINT('Ctrl Pts',(-12.8078932505832,-7.93031175503273,
-853.047794117647));
#162118=CARTESIAN_POINT('Ctrl Pts',(-13.4274493703259,-6.68607533664808,
-854.541911764706));
#162119=CARTESIAN_POINT('Ctrl Pts',(-14.0470054900687,-5.44183891826343,
-856.036029411765));
#162120=CARTESIAN_POINT('Ctrl Pts',(-14.4273846475923,-4.10494485108124,
-857.530147058824));
#162121=CARTESIAN_POINT('Ctrl Pts',(-14.8077638051159,-2.76805078389906,
-859.024264705882));
#162122=CARTESIAN_POINT('Ctrl Pts',(-14.9360126444255,-1.38402539194953,
-860.518382352941));
#162123=CARTESIAN_POINT('Ctrl Pts',(-15.0642614837351,-9.22419980378748E-16,
-862.0125));
#162124=CARTESIAN_POINT('Ctrl Pts',(-14.9360126444255,1.38402539194953,
-863.506617647059));
#162125=CARTESIAN_POINT('Ctrl Pts',(-14.8077638051159,2.76805078389906,
-865.000735294118));
#162126=CARTESIAN_POINT('Ctrl Pts',(-14.4273846475923,4.10494485108124,
-866.494852941176));
#162127=CARTESIAN_POINT('Ctrl Pts',(-14.0470054900687,5.44183891826343,
-867.988970588235));
#162128=CARTESIAN_POINT('Ctrl Pts',(-13.4274493703259,6.68607533664807,
-869.483088235294));
#162129=CARTESIAN_POINT('Ctrl Pts',(-12.8078932505832,7.93031175503273,
-870.977205882353));
#162130=CARTESIAN_POINT('Ctrl Pts',(-11.9702584092036,9.03951954568884,
-872.471323529412));
#162131=CARTESIAN_POINT('Ctrl Pts',(-11.132623567824,10.148727336345,-873.965441176471));
#162132=CARTESIAN_POINT('Ctrl Pts',(-10.1054346546984,11.0851337583099,
-875.459558823529));
#162133=CARTESIAN_POINT('Ctrl Pts',(-9.07824574157275,12.0215401802748,
-876.953676470588));
#162134=CARTESIAN_POINT('Ctrl Pts',(-7.89648244316034,12.7532570359442,
-878.447794117647));
#162135=CARTESIAN_POINT('Ctrl Pts',(-6.71471914474793,13.4849738916136,
-879.941911764706));
#162136=CARTESIAN_POINT('Ctrl Pts',(-5.41862499280729,13.9870834410653,
-881.436029411765));
#162137=CARTESIAN_POINT('Ctrl Pts',(-4.12253084086667,14.4891929905171,
-882.930147058823));
#162138=CARTESIAN_POINT('Ctrl Pts',(-2.75624276724856,14.7445964952585,
-884.424264705882));
#162139=CARTESIAN_POINT('Ctrl Pts',(-1.38995469363044,15.,-885.918382352941));
#162140=CARTESIAN_POINT('Ctrl Pts',(-1.83697019872103E-15,15.,-887.4125));
#162141=CARTESIAN_POINT('Ctrl Pts',(1.38995469363045,15.,-888.906617647059));
#162142=CARTESIAN_POINT('Ctrl Pts',(2.75624276724855,14.7445964952585,-890.400735294118));
#162143=CARTESIAN_POINT('Ctrl Pts',(4.12253084086666,14.4891929905171,-891.894852941177));
#162144=CARTESIAN_POINT('Ctrl Pts',(5.4186249928073,13.9870834410653,-893.388970588235));
#162145=CARTESIAN_POINT('Ctrl Pts',(6.71471914474792,13.4849738916136,-894.883088235295));
#162146=CARTESIAN_POINT('Ctrl Pts',(7.89648244316034,12.7532570359442,-896.377205882353));
#162147=CARTESIAN_POINT('Ctrl Pts',(9.07824574157275,12.0215401802748,-897.871323529412));
#162148=CARTESIAN_POINT('Ctrl Pts',(10.1054346546984,11.0851337583099,-899.36544117647));
#162149=CARTESIAN_POINT('Ctrl Pts',(11.132623567824,10.148727336345,-900.859558823529));
#162150=CARTESIAN_POINT('Ctrl Pts',(11.9702584092036,9.03951954568885,-902.353676470588));
#162151=CARTESIAN_POINT('Ctrl Pts',(12.8078932505832,7.93031175503273,-903.847794117647));
#162152=CARTESIAN_POINT('Ctrl Pts',(13.4274493703259,6.68607533664807,-905.341911764706));
#162153=CARTESIAN_POINT('Ctrl Pts',(14.0470054900687,5.44183891826343,-906.836029411765));
#162154=CARTESIAN_POINT('Ctrl Pts',(14.4273846475923,4.10494485108125,-908.330147058824));
#162155=CARTESIAN_POINT('Ctrl Pts',(14.8077638051159,2.76805078389905,-909.824264705883));
#162156=CARTESIAN_POINT('Ctrl Pts',(14.9360126444255,1.38402539194953,-911.318382352941));
#162157=CARTESIAN_POINT('Ctrl Pts',(15.0642614837351,2.76725994113625E-15,
-912.8125));
#162158=CARTESIAN_POINT('Ctrl Pts',(14.9360126444255,-1.38402539194952,
-914.306617647059));
#162159=CARTESIAN_POINT('Ctrl Pts',(14.8077638051159,-2.76805078389906,
-915.800735294118));
#162160=CARTESIAN_POINT('Ctrl Pts',(14.4273846475923,-4.10494485108124,
-917.294852941176));
#162161=CARTESIAN_POINT('Ctrl Pts',(14.0470054900687,-5.44183891826342,
-918.788970588235));
#162162=CARTESIAN_POINT('Ctrl Pts',(13.4274493703259,-6.68607533664808,
-920.283088235294));
#162163=CARTESIAN_POINT('Ctrl Pts',(12.8078932505832,-7.93031175503273,
-921.777205882353));
#162164=CARTESIAN_POINT('Ctrl Pts',(11.9702584092036,-9.03951954568884,
-923.271323529412));
#162165=CARTESIAN_POINT('Ctrl Pts',(11.132623567824,-10.148727336345,-924.765441176471));
#162166=CARTESIAN_POINT('Ctrl Pts',(10.1054346546984,-11.0851337583099,
-926.259558823529));
#162167=CARTESIAN_POINT('Ctrl Pts',(9.07824574157275,-12.0215401802748,
-927.753676470588));
#162168=CARTESIAN_POINT('Ctrl Pts',(7.89648244316034,-12.7532570359442,
-929.247794117647));
#162169=CARTESIAN_POINT('Ctrl Pts',(6.71471914474792,-13.4849738916136,
-930.741911764706));
#162170=CARTESIAN_POINT('Ctrl Pts',(5.4186249928073,-13.9870834410653,-932.236029411765));
#162171=CARTESIAN_POINT('Ctrl Pts',(4.12253084086667,-14.4891929905171,
-933.730147058824));
#162172=CARTESIAN_POINT('Ctrl Pts',(2.75624276724855,-14.7445964952585,
-935.224264705882));
#162173=CARTESIAN_POINT('Ctrl Pts',(1.38995469363045,-15.,-936.718382352941));
#162174=CARTESIAN_POINT('Ctrl Pts',(0.,-15.,-938.2125));
#162175=CARTESIAN_POINT('Ctrl Pts',(-1.38995469363045,-15.,-939.706617647059));
#162176=CARTESIAN_POINT('Ctrl Pts',(-2.75624276724856,-14.7445964952585,
-941.200735294117));
#162177=CARTESIAN_POINT('Ctrl Pts',(-4.12253084086666,-14.4891929905171,
-942.694852941176));
#162178=CARTESIAN_POINT('Ctrl Pts',(-5.41862499280729,-13.9870834410653,
-944.188970588235));
#162179=CARTESIAN_POINT('Ctrl Pts',(-6.71471914474793,-13.4849738916136,
-945.683088235294));
#162180=CARTESIAN_POINT('Ctrl Pts',(-7.89648244316034,-12.7532570359442,
-947.177205882353));
#162181=CARTESIAN_POINT('Ctrl Pts',(-9.07824574157275,-12.0215401802748,
-948.671323529412));
#162182=CARTESIAN_POINT('Ctrl Pts',(-10.1054346546984,-11.0851337583099,
-950.165441176471));
#162183=CARTESIAN_POINT('Ctrl Pts',(-11.132623567824,-10.148727336345,-951.65955882353));
#162184=CARTESIAN_POINT('Ctrl Pts',(-11.9702584092036,-9.03951954568885,
-953.153676470588));
#162185=CARTESIAN_POINT('Ctrl Pts',(-12.8078932505832,-7.93031175503273,
-954.647794117647));
#162186=CARTESIAN_POINT('Ctrl Pts',(-13.4274493703259,-6.68607533664808,
-956.141911764706));
#162187=CARTESIAN_POINT('Ctrl Pts',(-14.0470054900687,-5.44183891826343,
-957.636029411764));
#162188=CARTESIAN_POINT('Ctrl Pts',(-14.4273846475923,-4.10494485108124,
-959.130147058823));
#162189=CARTESIAN_POINT('Ctrl Pts',(-14.8077638051159,-2.76805078389906,
-960.624264705882));
#162190=CARTESIAN_POINT('Ctrl Pts',(-14.9360126444255,-1.38402539194953,
-962.118382352941));
#162191=CARTESIAN_POINT('Ctrl Pts',(-15.0642614837351,-9.22419980378748E-16,
-963.6125));
#162192=CARTESIAN_POINT('Ctrl Pts',(-14.9360126444255,1.38402539194953,
-965.106617647059));
#162193=CARTESIAN_POINT('Ctrl Pts',(-14.8077638051159,2.76805078389906,
-966.600735294118));
#162194=CARTESIAN_POINT('Ctrl Pts',(-14.4273846475923,4.10494485108124,
-968.094852941177));
#162195=CARTESIAN_POINT('Ctrl Pts',(-14.0470054900687,5.44183891826343,
-969.588970588235));
#162196=CARTESIAN_POINT('Ctrl Pts',(-13.4274493703259,6.68607533664807,
-971.083088235294));
#162197=CARTESIAN_POINT('Ctrl Pts',(-12.8078932505832,7.93031175503273,
-972.577205882353));
#162198=CARTESIAN_POINT('Ctrl Pts',(-11.9702584092036,9.03951954568884,
-974.071323529412));
#162199=CARTESIAN_POINT('Ctrl Pts',(-11.132623567824,10.148727336345,-975.565441176471));
#162200=CARTESIAN_POINT('Ctrl Pts',(-10.1054346546984,11.0851337583099,
-977.059558823529));
#162201=CARTESIAN_POINT('Ctrl Pts',(-9.07824574157275,12.0215401802748,
-978.553676470588));
#162202=CARTESIAN_POINT('Ctrl Pts',(-7.89648244316034,12.7532570359442,
-980.047794117647));
#162203=CARTESIAN_POINT('Ctrl Pts',(-6.71471914474793,13.4849738916136,
-981.541911764706));
#162204=CARTESIAN_POINT('Ctrl Pts',(-5.41862499280729,13.9870834410653,
-983.036029411765));
#162205=CARTESIAN_POINT('Ctrl Pts',(-4.12253084086667,14.4891929905171,
-984.530147058824));
#162206=CARTESIAN_POINT('Ctrl Pts',(-2.75624276724856,14.7445964952585,
-986.024264705882));
#162207=CARTESIAN_POINT('Ctrl Pts',(-1.38995469363044,15.,-987.518382352941));
#162208=CARTESIAN_POINT('Ctrl Pts',(-1.83697019872103E-15,15.,-989.0125));
#162209=CARTESIAN_POINT('Ctrl Pts',(1.38995469363045,15.,-990.506617647059));
#162210=CARTESIAN_POINT('Ctrl Pts',(2.75624276724855,14.7445964952585,-992.000735294118));
#162211=CARTESIAN_POINT('Ctrl Pts',(4.12253084086666,14.4891929905171,-993.494852941176));
#162212=CARTESIAN_POINT('Ctrl Pts',(5.4186249928073,13.9870834410653,-994.988970588235));
#162213=CARTESIAN_POINT('Ctrl Pts',(6.71471914474792,13.4849738916136,-996.483088235294));
#162214=CARTESIAN_POINT('Ctrl Pts',(7.89648244316034,12.7532570359442,-997.977205882353));
#162215=CARTESIAN_POINT('Ctrl Pts',(9.07824574157275,12.0215401802748,-999.471323529412));
#162216=CARTESIAN_POINT('Ctrl Pts',(10.1054346546984,11.0851337583099,-1000.96544117647));
#162217=CARTESIAN_POINT('Ctrl Pts',(11.132623567824,10.148727336345,-1002.45955882353));
#162218=CARTESIAN_POINT('Ctrl Pts',(11.9702584092036,9.03951954568885,-1003.95367647059));
#162219=CARTESIAN_POINT('Ctrl Pts',(12.8078932505832,7.93031175503273,-1005.44779411765));
#162220=CARTESIAN_POINT('Ctrl Pts',(13.4274493703259,6.68607533664807,-1006.94191176471));
#162221=CARTESIAN_POINT('Ctrl Pts',(14.0470054900687,5.44183891826343,-1008.43602941176));
#162222=CARTESIAN_POINT('Ctrl Pts',(14.4273846475923,4.10494485108125,-1009.93014705882));
#162223=CARTESIAN_POINT('Ctrl Pts',(14.8077638051159,2.76805078389905,-1011.42426470588));
#162224=CARTESIAN_POINT('Ctrl Pts',(14.9360126444255,1.38402539194953,-1012.91838235294));
#162225=CARTESIAN_POINT('Ctrl Pts',(15.0642614837351,2.76725994113625E-15,
-1014.4125));
#162226=CARTESIAN_POINT('Ctrl Pts',(14.9360126444255,-1.38402539194952,
-1015.90661764706));
#162227=CARTESIAN_POINT('Ctrl Pts',(14.8077638051159,-2.76805078389906,
-1017.40073529412));
#162228=CARTESIAN_POINT('Ctrl Pts',(14.4273846475923,-4.10494485108124,
-1018.89485294118));
#162229=CARTESIAN_POINT('Ctrl Pts',(14.0470054900687,-5.44183891826342,
-1020.38897058824));
#162230=CARTESIAN_POINT('Ctrl Pts',(13.4274493703259,-6.68607533664808,
-1021.88308823529));
#162231=CARTESIAN_POINT('Ctrl Pts',(12.8078932505832,-7.93031175503273,
-1023.37720588235));
#162232=CARTESIAN_POINT('Ctrl Pts',(11.9702584092036,-9.03951954568884,
-1024.87132352941));
#162233=CARTESIAN_POINT('Ctrl Pts',(11.132623567824,-10.148727336345,-1026.36544117647));
#162234=CARTESIAN_POINT('Ctrl Pts',(10.1054346546984,-11.0851337583099,
-1027.85955882353));
#162235=CARTESIAN_POINT('Ctrl Pts',(9.07824574157275,-12.0215401802748,
-1029.35367647059));
#162236=CARTESIAN_POINT('Ctrl Pts',(7.89648244316034,-12.7532570359442,
-1030.84779411765));
#162237=CARTESIAN_POINT('Ctrl Pts',(6.71471914474792,-13.4849738916136,
-1032.34191176471));
#162238=CARTESIAN_POINT('Ctrl Pts',(5.4186249928073,-13.9870834410653,-1033.83602941176));
#162239=CARTESIAN_POINT('Ctrl Pts',(4.12253084086667,-14.4891929905171,
-1035.33014705882));
#162240=CARTESIAN_POINT('Ctrl Pts',(2.75624276724855,-14.7445964952585,
-1036.82426470588));
#162241=CARTESIAN_POINT('Ctrl Pts',(1.38995469363045,-15.,-1038.31838235294));
#162242=CARTESIAN_POINT('Ctrl Pts',(0.,-15.,-1039.8125));
#162243=CARTESIAN_POINT('Ctrl Pts',(-1.38995469363045,-15.,-1041.30661764706));
#162244=CARTESIAN_POINT('Ctrl Pts',(-2.75624276724856,-14.7445964952585,
-1042.80073529412));
#162245=CARTESIAN_POINT('Ctrl Pts',(-4.12253084086666,-14.4891929905171,
-1044.29485294118));
#162246=CARTESIAN_POINT('Ctrl Pts',(-5.41862499280729,-13.9870834410653,
-1045.78897058824));
#162247=CARTESIAN_POINT('Ctrl Pts',(-6.71471914474793,-13.4849738916136,
-1047.28308823529));
#162248=CARTESIAN_POINT('Ctrl Pts',(-7.89648244316034,-12.7532570359442,
-1048.77720588235));
#162249=CARTESIAN_POINT('Ctrl Pts',(-9.07824574157275,-12.0215401802748,
-1050.27132352941));
#162250=CARTESIAN_POINT('Ctrl Pts',(-10.1054346546984,-11.0851337583099,
-1051.76544117647));
#162251=CARTESIAN_POINT('Ctrl Pts',(-11.132623567824,-10.148727336345,-1053.25955882353));
#162252=CARTESIAN_POINT('Ctrl Pts',(-11.9702584092036,-9.03951954568885,
-1054.75367647059));
#162253=CARTESIAN_POINT('Ctrl Pts',(-12.8078932505832,-7.93031175503273,
-1056.24779411765));
#162254=CARTESIAN_POINT('Ctrl Pts',(-13.4274493703259,-6.68607533664808,
-1057.74191176471));
#162255=CARTESIAN_POINT('Ctrl Pts',(-14.0470054900687,-5.44183891826343,
-1059.23602941177));
#162256=CARTESIAN_POINT('Ctrl Pts',(-14.4273846475923,-4.10494485108124,
-1060.73014705882));
#162257=CARTESIAN_POINT('Ctrl Pts',(-14.8077638051159,-2.76805078389906,
-1062.22426470588));
#162258=CARTESIAN_POINT('Ctrl Pts',(-14.9360126444255,-1.38402539194953,
-1063.71838235294));
#162259=CARTESIAN_POINT('Ctrl Pts',(-15.0642614837351,-9.22419980378748E-16,
-1065.2125));
#162260=CARTESIAN_POINT('Ctrl Pts',(-14.9360126444255,1.38402539194953,
-1066.70661764706));
#162261=CARTESIAN_POINT('Ctrl Pts',(-14.8077638051159,2.76805078389906,
-1068.20073529412));
#162262=CARTESIAN_POINT('Ctrl Pts',(-14.4273846475923,4.10494485108124,
-1069.69485294118));
#162263=CARTESIAN_POINT('Ctrl Pts',(-14.0470054900687,5.44183891826343,
-1071.18897058824));
#162264=CARTESIAN_POINT('Ctrl Pts',(-13.4274493703259,6.68607533664807,
-1072.68308823529));
#162265=CARTESIAN_POINT('Ctrl Pts',(-12.8078932505832,7.93031175503273,
-1074.17720588235));
#162266=CARTESIAN_POINT('Ctrl Pts',(-11.9702584092036,9.03951954568884,
-1075.67132352941));
#162267=CARTESIAN_POINT('Ctrl Pts',(-11.132623567824,10.148727336345,-1077.16544117647));
#162268=CARTESIAN_POINT('Ctrl Pts',(-10.1054346546984,11.0851337583099,
-1078.65955882353));
#162269=CARTESIAN_POINT('Ctrl Pts',(-9.07824574157275,12.0215401802748,
-1080.15367647059));
#162270=CARTESIAN_POINT('Ctrl Pts',(-7.89648244316034,12.7532570359442,
-1081.64779411765));
#162271=CARTESIAN_POINT('Ctrl Pts',(-6.71471914474793,13.4849738916136,
-1083.14191176471));
#162272=CARTESIAN_POINT('Ctrl Pts',(-5.41862499280729,13.9870834410653,
-1084.63602941176));
#162273=CARTESIAN_POINT('Ctrl Pts',(-4.12253084086667,14.4891929905171,
-1086.13014705882));
#162274=CARTESIAN_POINT('Ctrl Pts',(-2.75624276724856,14.7445964952585,
-1087.62426470588));
#162275=CARTESIAN_POINT('Ctrl Pts',(-1.38995469363044,15.,-1089.11838235294));
#162276=CARTESIAN_POINT('Ctrl Pts',(-1.83697019872103E-15,15.,-1090.6125));
#162277=CARTESIAN_POINT('Ctrl Pts',(1.38995469363045,15.,-1092.10661764706));
#162278=CARTESIAN_POINT('Ctrl Pts',(2.75624276724855,14.7445964952585,-1093.60073529412));
#162279=CARTESIAN_POINT('Ctrl Pts',(4.12253084086666,14.4891929905171,-1095.09485294118));
#162280=CARTESIAN_POINT('Ctrl Pts',(5.4186249928073,13.9870834410653,-1096.58897058824));
#162281=CARTESIAN_POINT('Ctrl Pts',(6.71471914474792,13.4849738916136,-1098.08308823529));
#162282=CARTESIAN_POINT('Ctrl Pts',(7.89648244316034,12.7532570359442,-1099.57720588235));
#162283=CARTESIAN_POINT('Ctrl Pts',(9.07824574157275,12.0215401802748,-1101.07132352941));
#162284=CARTESIAN_POINT('Ctrl Pts',(10.1054346546984,11.0851337583099,-1102.56544117647));
#162285=CARTESIAN_POINT('Ctrl Pts',(11.132623567824,10.148727336345,-1104.05955882353));
#162286=CARTESIAN_POINT('Ctrl Pts',(11.9702584092036,9.03951954568885,-1105.55367647059));
#162287=CARTESIAN_POINT('Ctrl Pts',(12.8078932505832,7.93031175503273,-1107.04779411765));
#162288=CARTESIAN_POINT('Ctrl Pts',(13.4274493703259,6.68607533664807,-1108.54191176471));
#162289=CARTESIAN_POINT('Ctrl Pts',(14.0470054900687,5.44183891826343,-1110.03602941176));
#162290=CARTESIAN_POINT('Ctrl Pts',(14.4273846475923,4.10494485108125,-1111.53014705882));
#162291=CARTESIAN_POINT('Ctrl Pts',(14.8077638051159,2.76805078389905,-1113.02426470588));
#162292=CARTESIAN_POINT('Ctrl Pts',(14.9360126444255,1.38402539194953,-1114.51838235294));
#162293=CARTESIAN_POINT('Ctrl Pts',(15.0642614837351,2.76725994113625E-15,
-1116.0125));
#162294=CARTESIAN_POINT('Ctrl Pts',(14.9360126444255,-1.38402539194952,
-1117.50661764706));
#162295=CARTESIAN_POINT('Ctrl Pts',(14.8077638051159,-2.76805078389906,
-1119.00073529412));
#162296=CARTESIAN_POINT('Ctrl Pts',(14.4273846475923,-4.10494485108124,
-1120.49485294118));
#162297=CARTESIAN_POINT('Ctrl Pts',(14.0470054900687,-5.44183891826342,
-1121.98897058824));
#162298=CARTESIAN_POINT('Ctrl Pts',(13.4274493703259,-6.68607533664808,
-1123.48308823529));
#162299=CARTESIAN_POINT('Ctrl Pts',(12.8078932505832,-7.93031175503273,
-1124.97720588235));
#162300=CARTESIAN_POINT('Ctrl Pts',(11.9702584092036,-9.03951954568884,
-1126.47132352941));
#162301=CARTESIAN_POINT('Ctrl Pts',(11.132623567824,-10.148727336345,-1127.96544117647));
#162302=CARTESIAN_POINT('Ctrl Pts',(10.1054346546984,-11.0851337583099,
-1129.45955882353));
#162303=CARTESIAN_POINT('Ctrl Pts',(9.07824574157275,-12.0215401802748,
-1130.95367647059));
#162304=CARTESIAN_POINT('Ctrl Pts',(7.89648244316034,-12.7532570359442,
-1132.44779411765));
#162305=CARTESIAN_POINT('Ctrl Pts',(6.71471914474792,-13.4849738916136,
-1133.94191176471));
#162306=CARTESIAN_POINT('Ctrl Pts',(5.4186249928073,-13.9870834410653,-1135.43602941176));
#162307=CARTESIAN_POINT('Ctrl Pts',(4.12253084086667,-14.4891929905171,
-1136.93014705882));
#162308=CARTESIAN_POINT('Ctrl Pts',(2.75624276724855,-14.7445964952585,
-1138.42426470588));
#162309=CARTESIAN_POINT('Ctrl Pts',(1.38995469363045,-15.,-1139.91838235294));
#162310=CARTESIAN_POINT('Ctrl Pts',(0.,-15.,-1141.4125));
#162311=CARTESIAN_POINT('Ctrl Pts',(-1.38995469363045,-15.,-1142.90661764706));
#162312=CARTESIAN_POINT('Ctrl Pts',(-2.75624276724856,-14.7445964952585,
-1144.40073529412));
#162313=CARTESIAN_POINT('Ctrl Pts',(-4.12253084086666,-14.4891929905171,
-1145.89485294118));
#162314=CARTESIAN_POINT('Ctrl Pts',(-5.41862499280729,-13.9870834410653,
-1147.38897058824));
#162315=CARTESIAN_POINT('Ctrl Pts',(-6.71471914474793,-13.4849738916136,
-1148.88308823529));
#162316=CARTESIAN_POINT('Ctrl Pts',(-7.89648244316034,-12.7532570359442,
-1150.37720588235));
#162317=CARTESIAN_POINT('Ctrl Pts',(-9.07824574157275,-12.0215401802748,
-1151.87132352941));
#162318=CARTESIAN_POINT('Ctrl Pts',(-10.1054346546984,-11.0851337583099,
-1153.36544117647));
#162319=CARTESIAN_POINT('Ctrl Pts',(-11.132623567824,-10.148727336345,-1154.85955882353));
#162320=CARTESIAN_POINT('Ctrl Pts',(-11.9702584092036,-9.03951954568885,
-1156.35367647059));
#162321=CARTESIAN_POINT('Ctrl Pts',(-12.8078932505832,-7.93031175503273,
-1157.84779411765));
#162322=CARTESIAN_POINT('Ctrl Pts',(-13.4274493703259,-6.68607533664808,
-1159.34191176471));
#162323=CARTESIAN_POINT('Ctrl Pts',(-14.0470054900687,-5.44183891826343,
-1160.83602941176));
#162324=CARTESIAN_POINT('Ctrl Pts',(-14.4273846475923,-4.10494485108124,
-1162.33014705882));
#162325=CARTESIAN_POINT('Ctrl Pts',(-14.8077638051159,-2.76805078389906,
-1163.82426470588));
#162326=CARTESIAN_POINT('Ctrl Pts',(-14.9360126444255,-1.38402539194953,
-1165.31838235294));
#162327=CARTESIAN_POINT('Ctrl Pts',(-15.0642614837351,-9.22419980378748E-16,
-1166.8125));
#162328=CARTESIAN_POINT('Ctrl Pts',(-14.9360126444255,1.38402539194953,
-1168.30661764706));
#162329=CARTESIAN_POINT('Ctrl Pts',(-14.8077638051159,2.76805078389906,
-1169.80073529412));
#162330=CARTESIAN_POINT('Ctrl Pts',(-14.4273846475923,4.10494485108124,
-1171.29485294118));
#162331=CARTESIAN_POINT('Ctrl Pts',(-14.0470054900687,5.44183891826343,
-1172.78897058824));
#162332=CARTESIAN_POINT('Ctrl Pts',(-13.4274493703259,6.68607533664807,
-1174.28308823529));
#162333=CARTESIAN_POINT('Ctrl Pts',(-12.8078932505832,7.93031175503273,
-1175.77720588235));
#162334=CARTESIAN_POINT('Ctrl Pts',(-11.9702584092036,9.03951954568884,
-1177.27132352941));
#162335=CARTESIAN_POINT('Ctrl Pts',(-11.132623567824,10.148727336345,-1178.76544117647));
#162336=CARTESIAN_POINT('Ctrl Pts',(-10.1054346546984,11.0851337583099,
-1180.25955882353));
#162337=CARTESIAN_POINT('Ctrl Pts',(-9.07824574157275,12.0215401802748,
-1181.75367647059));
#162338=CARTESIAN_POINT('Ctrl Pts',(-7.89648244316034,12.7532570359442,
-1183.24779411765));
#162339=CARTESIAN_POINT('Ctrl Pts',(-6.71471914474793,13.4849738916136,
-1184.74191176471));
#162340=CARTESIAN_POINT('Ctrl Pts',(-5.41862499280729,13.9870834410653,
-1186.23602941176));
#162341=CARTESIAN_POINT('Ctrl Pts',(-4.12253084086667,14.4891929905171,
-1187.73014705882));
#162342=CARTESIAN_POINT('Ctrl Pts',(-2.75624276724856,14.7445964952585,
-1189.22426470588));
#162343=CARTESIAN_POINT('Ctrl Pts',(-1.38995469363044,15.,-1190.71838235294));
#162344=CARTESIAN_POINT('Ctrl Pts',(-1.83697019872103E-15,15.,-1192.2125));
#162345=CARTESIAN_POINT('Ctrl Pts',(1.38995469363045,15.,-1193.70661764706));
#162346=CARTESIAN_POINT('Ctrl Pts',(2.75624276724855,14.7445964952585,-1195.20073529412));
#162347=CARTESIAN_POINT('Ctrl Pts',(4.12253084086666,14.4891929905171,-1196.69485294118));
#162348=CARTESIAN_POINT('Ctrl Pts',(5.4186249928073,13.9870834410653,-1198.18897058824));
#162349=CARTESIAN_POINT('Ctrl Pts',(6.71471914474792,13.4849738916136,-1199.68308823529));
#162350=CARTESIAN_POINT('Ctrl Pts',(7.89648244316034,12.7532570359442,-1201.17720588235));
#162351=CARTESIAN_POINT('Ctrl Pts',(9.07824574157275,12.0215401802748,-1202.67132352941));
#162352=CARTESIAN_POINT('Ctrl Pts',(10.1054346546984,11.0851337583099,-1204.16544117647));
#162353=CARTESIAN_POINT('Ctrl Pts',(11.132623567824,10.148727336345,-1205.65955882353));
#162354=CARTESIAN_POINT('Ctrl Pts',(11.9702584092036,9.03951954568885,-1207.15367647059));
#162355=CARTESIAN_POINT('Ctrl Pts',(12.8078932505832,7.93031175503273,-1208.64779411765));
#162356=CARTESIAN_POINT('Ctrl Pts',(13.4274493703259,6.68607533664807,-1210.14191176471));
#162357=CARTESIAN_POINT('Ctrl Pts',(14.0470054900687,5.44183891826343,-1211.63602941176));
#162358=CARTESIAN_POINT('Ctrl Pts',(14.4273846475923,4.10494485108125,-1213.13014705882));
#162359=CARTESIAN_POINT('Ctrl Pts',(14.8077638051159,2.76805078389905,-1214.62426470588));
#162360=CARTESIAN_POINT('Ctrl Pts',(14.9360126444255,1.38402539194953,-1216.11838235294));
#162361=CARTESIAN_POINT('Ctrl Pts',(15.0642614837351,2.76725994113625E-15,
-1217.6125));
#162362=CARTESIAN_POINT('Ctrl Pts',(14.9360126444255,-1.38402539194952,
-1219.10661764706));
#162363=CARTESIAN_POINT('Ctrl Pts',(14.8077638051159,-2.76805078389906,
-1220.60073529412));
#162364=CARTESIAN_POINT('Ctrl Pts',(14.4273846475923,-4.10494485108124,
-1222.09485294118));
#162365=CARTESIAN_POINT('Ctrl Pts',(14.0470054900687,-5.44183891826342,
-1223.58897058824));
#162366=CARTESIAN_POINT('Ctrl Pts',(13.4274493703259,-6.68607533664808,
-1225.08308823529));
#162367=CARTESIAN_POINT('Ctrl Pts',(12.8078932505832,-7.93031175503273,
-1226.57720588235));
#162368=CARTESIAN_POINT('Ctrl Pts',(11.9702584092036,-9.03951954568884,
-1228.07132352941));
#162369=CARTESIAN_POINT('Ctrl Pts',(11.132623567824,-10.148727336345,-1229.56544117647));
#162370=CARTESIAN_POINT('Ctrl Pts',(10.1054346546984,-11.0851337583099,
-1231.05955882353));
#162371=CARTESIAN_POINT('Ctrl Pts',(9.07824574157275,-12.0215401802748,
-1232.55367647059));
#162372=CARTESIAN_POINT('Ctrl Pts',(7.89648244316034,-12.7532570359442,
-1234.04779411765));
#162373=CARTESIAN_POINT('Ctrl Pts',(6.71471914474792,-13.4849738916136,
-1235.54191176471));
#162374=CARTESIAN_POINT('Ctrl Pts',(5.4186249928073,-13.9870834410653,-1237.03602941176));
#162375=CARTESIAN_POINT('Ctrl Pts',(4.12253084086667,-14.4891929905171,
-1238.53014705882));
#162376=CARTESIAN_POINT('Ctrl Pts',(2.75624276724855,-14.7445964952585,
-1240.02426470588));
#162377=CARTESIAN_POINT('Ctrl Pts',(1.38995469363045,-15.,-1241.51838235294));
#162378=CARTESIAN_POINT('Ctrl Pts',(0.,-15.,-1243.0125));
#162379=CARTESIAN_POINT('Ctrl Pts',(-1.38995469363045,-15.,-1244.50661764706));
#162380=CARTESIAN_POINT('Ctrl Pts',(-2.75624276724856,-14.7445964952585,
-1246.00073529412));
#162381=CARTESIAN_POINT('Ctrl Pts',(-4.12253084086666,-14.4891929905171,
-1247.49485294118));
#162382=CARTESIAN_POINT('Ctrl Pts',(-5.41862499280729,-13.9870834410653,
-1248.98897058824));
#162383=CARTESIAN_POINT('Ctrl Pts',(-6.71471914474793,-13.4849738916136,
-1250.48308823529));
#162384=CARTESIAN_POINT('Ctrl Pts',(-7.89648244316034,-12.7532570359442,
-1251.97720588235));
#162385=CARTESIAN_POINT('Ctrl Pts',(-9.07824574157275,-12.0215401802748,
-1253.47132352941));
#162386=CARTESIAN_POINT('Ctrl Pts',(-10.1054346546984,-11.0851337583099,
-1254.96544117647));
#162387=CARTESIAN_POINT('Ctrl Pts',(-11.132623567824,-10.148727336345,-1256.45955882353));
#162388=CARTESIAN_POINT('Ctrl Pts',(-11.9702584092036,-9.03951954568885,
-1257.95367647059));
#162389=CARTESIAN_POINT('Ctrl Pts',(-12.8078932505832,-7.93031175503273,
-1259.44779411765));
#162390=CARTESIAN_POINT('Ctrl Pts',(-13.4274493703259,-6.68607533664808,
-1260.94191176471));
#162391=CARTESIAN_POINT('Ctrl Pts',(-14.0470054900687,-5.44183891826343,
-1262.43602941176));
#162392=CARTESIAN_POINT('Ctrl Pts',(-14.4273846475923,-4.10494485108124,
-1263.93014705882));
#162393=CARTESIAN_POINT('Ctrl Pts',(-14.8077638051159,-2.76805078389906,
-1265.42426470588));
#162394=CARTESIAN_POINT('Ctrl Pts',(-14.9360126444255,-1.38402539194953,
-1266.91838235294));
#162395=CARTESIAN_POINT('Ctrl Pts',(-15.0642614837351,-9.22419980378748E-16,
-1268.4125));
#162396=CARTESIAN_POINT('Ctrl Pts',(-14.9360126444255,1.38402539194953,
-1269.90661764706));
#162397=CARTESIAN_POINT('Ctrl Pts',(-14.8077638051159,2.76805078389906,
-1271.40073529412));
#162398=CARTESIAN_POINT('Ctrl Pts',(-14.4273846475923,4.10494485108124,
-1272.89485294118));
#162399=CARTESIAN_POINT('Ctrl Pts',(-14.0470054900687,5.44183891826343,
-1274.38897058824));
#162400=CARTESIAN_POINT('Ctrl Pts',(-13.4274493703259,6.68607533664807,
-1275.88308823529));
#162401=CARTESIAN_POINT('Ctrl Pts',(-12.8078932505832,7.93031175503273,
-1277.37720588235));
#162402=CARTESIAN_POINT('Ctrl Pts',(-11.9702584092036,9.03951954568884,
-1278.87132352941));
#162403=CARTESIAN_POINT('Ctrl Pts',(-11.132623567824,10.148727336345,-1280.36544117647));
#162404=CARTESIAN_POINT('Ctrl Pts',(-10.1054346546984,11.0851337583099,
-1281.85955882353));
#162405=CARTESIAN_POINT('Ctrl Pts',(-9.07824574157275,12.0215401802748,
-1283.35367647059));
#162406=CARTESIAN_POINT('Ctrl Pts',(-7.89648244316034,12.7532570359442,
-1284.84779411765));
#162407=CARTESIAN_POINT('Ctrl Pts',(-6.71471914474793,13.4849738916136,
-1286.34191176471));
#162408=CARTESIAN_POINT('Ctrl Pts',(-5.41862499280729,13.9870834410653,
-1287.83602941176));
#162409=CARTESIAN_POINT('Ctrl Pts',(-4.12253084086667,14.4891929905171,
-1289.33014705882));
#162410=CARTESIAN_POINT('Ctrl Pts',(-2.75624276724856,14.7445964952585,
-1290.82426470588));
#162411=CARTESIAN_POINT('Ctrl Pts',(-1.38995469363044,15.,-1292.31838235294));
#162412=CARTESIAN_POINT('Ctrl Pts',(-1.83697019872103E-15,15.,-1293.8125));
#162413=CARTESIAN_POINT('Ctrl Pts',(1.38995469363045,15.,-1295.30661764706));
#162414=CARTESIAN_POINT('Ctrl Pts',(2.75624276724855,14.7445964952585,-1296.80073529412));
#162415=CARTESIAN_POINT('Ctrl Pts',(4.12253084086666,14.4891929905171,-1298.29485294118));
#162416=CARTESIAN_POINT('Ctrl Pts',(5.4186249928073,13.9870834410653,-1299.78897058824));
#162417=CARTESIAN_POINT('Ctrl Pts',(6.71471914474792,13.4849738916136,-1301.28308823529));
#162418=CARTESIAN_POINT('Ctrl Pts',(7.89648244316034,12.7532570359442,-1302.77720588235));
#162419=CARTESIAN_POINT('Ctrl Pts',(9.07824574157275,12.0215401802748,-1304.27132352941));
#162420=CARTESIAN_POINT('Ctrl Pts',(10.1054346546984,11.0851337583099,-1305.76544117647));
#162421=CARTESIAN_POINT('Ctrl Pts',(11.132623567824,10.148727336345,-1307.25955882353));
#162422=CARTESIAN_POINT('Ctrl Pts',(11.9702584092036,9.03951954568885,-1308.75367647059));
#162423=CARTESIAN_POINT('Ctrl Pts',(12.8078932505832,7.93031175503273,-1310.24779411765));
#162424=CARTESIAN_POINT('Ctrl Pts',(13.4274493703259,6.68607533664807,-1311.74191176471));
#162425=CARTESIAN_POINT('Ctrl Pts',(14.0470054900687,5.44183891826343,-1313.23602941176));
#162426=CARTESIAN_POINT('Ctrl Pts',(14.4273846475923,4.10494485108125,-1314.73014705882));
#162427=CARTESIAN_POINT('Ctrl Pts',(14.8077638051159,2.76805078389905,-1316.22426470588));
#162428=CARTESIAN_POINT('Ctrl Pts',(14.9360126444255,1.38402539194953,-1317.71838235294));
#162429=CARTESIAN_POINT('Ctrl Pts',(15.0642614837351,2.76725994113625E-15,
-1319.2125));
#162430=CARTESIAN_POINT('Ctrl Pts',(14.9360126444255,-1.38402539194952,
-1320.70661764706));
#162431=CARTESIAN_POINT('Ctrl Pts',(14.8077638051159,-2.76805078389906,
-1322.20073529412));
#162432=CARTESIAN_POINT('Ctrl Pts',(14.4273846475923,-4.10494485108124,
-1323.69485294118));
#162433=CARTESIAN_POINT('Ctrl Pts',(14.0470054900687,-5.44183891826342,
-1325.18897058824));
#162434=CARTESIAN_POINT('Ctrl Pts',(13.4274493703259,-6.68607533664808,
-1326.68308823529));
#162435=CARTESIAN_POINT('Ctrl Pts',(12.8078932505832,-7.93031175503273,
-1328.17720588235));
#162436=CARTESIAN_POINT('Ctrl Pts',(11.9702584092036,-9.03951954568884,
-1329.67132352941));
#162437=CARTESIAN_POINT('Ctrl Pts',(11.132623567824,-10.148727336345,-1331.16544117647));
#162438=CARTESIAN_POINT('Ctrl Pts',(10.1054346546984,-11.0851337583099,
-1332.65955882353));
#162439=CARTESIAN_POINT('Ctrl Pts',(9.07824574157275,-12.0215401802748,
-1334.15367647059));
#162440=CARTESIAN_POINT('Ctrl Pts',(7.89648244316034,-12.7532570359442,
-1335.64779411765));
#162441=CARTESIAN_POINT('Ctrl Pts',(6.71471914474792,-13.4849738916136,
-1337.14191176471));
#162442=CARTESIAN_POINT('Ctrl Pts',(5.4186249928073,-13.9870834410653,-1338.63602941176));
#162443=CARTESIAN_POINT('Ctrl Pts',(4.12253084086667,-14.4891929905171,
-1340.13014705882));
#162444=CARTESIAN_POINT('Ctrl Pts',(2.75624276724855,-14.7445964952585,
-1341.62426470588));
#162445=CARTESIAN_POINT('Ctrl Pts',(1.38995469363045,-15.,-1343.11838235294));
#162446=CARTESIAN_POINT('Ctrl Pts',(0.,-15.,-1344.6125));
#162447=CARTESIAN_POINT('Ctrl Pts',(-1.38995469363045,-15.,-1346.10661764706));
#162448=CARTESIAN_POINT('Ctrl Pts',(-2.75624276724856,-14.7445964952585,
-1347.60073529412));
#162449=CARTESIAN_POINT('Ctrl Pts',(-4.12253084086666,-14.4891929905171,
-1349.09485294118));
#162450=CARTESIAN_POINT('Ctrl Pts',(-5.41862499280729,-13.9870834410653,
-1350.58897058824));
#162451=CARTESIAN_POINT('Ctrl Pts',(-6.71471914474793,-13.4849738916136,
-1352.08308823529));
#162452=CARTESIAN_POINT('Ctrl Pts',(-7.89648244316034,-12.7532570359442,
-1353.57720588235));
#162453=CARTESIAN_POINT('Ctrl Pts',(-9.07824574157275,-12.0215401802748,
-1355.07132352941));
#162454=CARTESIAN_POINT('Ctrl Pts',(-10.1054346546984,-11.0851337583099,
-1356.56544117647));
#162455=CARTESIAN_POINT('Ctrl Pts',(-11.132623567824,-10.148727336345,-1358.05955882353));
#162456=CARTESIAN_POINT('Ctrl Pts',(-11.9702584092036,-9.03951954568885,
-1359.55367647059));
#162457=CARTESIAN_POINT('Ctrl Pts',(-12.8078932505832,-7.93031175503273,
-1361.04779411765));
#162458=CARTESIAN_POINT('Ctrl Pts',(-13.4274493703259,-6.68607533664808,
-1362.54191176471));
#162459=CARTESIAN_POINT('Ctrl Pts',(-14.0470054900687,-5.44183891826343,
-1364.03602941176));
#162460=CARTESIAN_POINT('Ctrl Pts',(-14.4273846475923,-4.10494485108124,
-1365.53014705882));
#162461=CARTESIAN_POINT('Ctrl Pts',(-14.8077638051159,-2.76805078389906,
-1367.02426470588));
#162462=CARTESIAN_POINT('Ctrl Pts',(-14.9360126444255,-1.38402539194953,
-1368.51838235294));
#162463=CARTESIAN_POINT('Ctrl Pts',(-15.0642614837351,-9.22419980378748E-16,
-1370.0125));
#162464=CARTESIAN_POINT('Ctrl Pts',(-14.9360126444255,1.38402539194953,
-1371.50661764706));
#162465=CARTESIAN_POINT('Ctrl Pts',(-14.8077638051159,2.76805078389906,
-1373.00073529412));
#162466=CARTESIAN_POINT('Ctrl Pts',(-14.4273846475923,4.10494485108124,
-1374.49485294118));
#162467=CARTESIAN_POINT('Ctrl Pts',(-14.0470054900687,5.44183891826343,
-1375.98897058824));
#162468=CARTESIAN_POINT('Ctrl Pts',(-13.4274493703259,6.68607533664807,
-1377.48308823529));
#162469=CARTESIAN_POINT('Ctrl Pts',(-12.8078932505832,7.93031175503273,
-1378.97720588235));
#162470=CARTESIAN_POINT('Ctrl Pts',(-11.9702584092036,9.03951954568884,
-1380.47132352941));
#162471=CARTESIAN_POINT('Ctrl Pts',(-11.132623567824,10.148727336345,-1381.96544117647));
#162472=CARTESIAN_POINT('Ctrl Pts',(-10.1054346546984,11.0851337583099,
-1383.45955882353));
#162473=CARTESIAN_POINT('Ctrl Pts',(-9.07824574157275,12.0215401802748,
-1384.95367647059));
#162474=CARTESIAN_POINT('Ctrl Pts',(-7.89648244316034,12.7532570359442,
-1386.44779411765));
#162475=CARTESIAN_POINT('Ctrl Pts',(-6.71471914474793,13.4849738916136,
-1387.94191176471));
#162476=CARTESIAN_POINT('Ctrl Pts',(-5.41862499280729,13.9870834410653,
-1389.43602941176));
#162477=CARTESIAN_POINT('Ctrl Pts',(-4.12253084086667,14.4891929905171,
-1390.93014705882));
#162478=CARTESIAN_POINT('Ctrl Pts',(-2.75624276724856,14.7445964952585,
-1392.42426470588));
#162479=CARTESIAN_POINT('Ctrl Pts',(-1.38995469363044,15.,-1393.91838235294));
#162480=CARTESIAN_POINT('Ctrl Pts',(-1.83697019872103E-15,15.,-1395.4125));
#162481=CARTESIAN_POINT('Ctrl Pts',(1.38995469363045,15.,-1396.90661764706));
#162482=CARTESIAN_POINT('Ctrl Pts',(2.75624276724855,14.7445964952585,-1398.40073529412));
#162483=CARTESIAN_POINT('Ctrl Pts',(4.12253084086666,14.4891929905171,-1399.89485294118));
#162484=CARTESIAN_POINT('Ctrl Pts',(5.4186249928073,13.9870834410653,-1401.38897058824));
#162485=CARTESIAN_POINT('Ctrl Pts',(6.71471914474792,13.4849738916136,-1402.88308823529));
#162486=CARTESIAN_POINT('Ctrl Pts',(7.89648244316034,12.7532570359442,-1404.37720588235));
#162487=CARTESIAN_POINT('Ctrl Pts',(9.07824574157275,12.0215401802748,-1405.87132352941));
#162488=CARTESIAN_POINT('Ctrl Pts',(10.1054346546984,11.0851337583099,-1407.36544117647));
#162489=CARTESIAN_POINT('Ctrl Pts',(11.132623567824,10.148727336345,-1408.85955882353));
#162490=CARTESIAN_POINT('Ctrl Pts',(11.9702584092036,9.03951954568885,-1410.35367647059));
#162491=CARTESIAN_POINT('Ctrl Pts',(12.8078932505832,7.93031175503273,-1411.84779411765));
#162492=CARTESIAN_POINT('Ctrl Pts',(13.4274493703259,6.68607533664807,-1413.34191176471));
#162493=CARTESIAN_POINT('Ctrl Pts',(14.0470054900687,5.44183891826343,-1414.83602941176));
#162494=CARTESIAN_POINT('Ctrl Pts',(14.4273846475923,4.10494485108125,-1416.33014705882));
#162495=CARTESIAN_POINT('Ctrl Pts',(14.8077638051159,2.76805078389905,-1417.82426470588));
#162496=CARTESIAN_POINT('Ctrl Pts',(14.9360126444255,1.38402539194953,-1419.31838235294));
#162497=CARTESIAN_POINT('Ctrl Pts',(15.0642614837351,2.76725994113625E-15,
-1420.8125));
#162498=CARTESIAN_POINT('Ctrl Pts',(14.9360126444255,-1.38402539194952,
-1422.30661764706));
#162499=CARTESIAN_POINT('Ctrl Pts',(14.8077638051159,-2.76805078389906,
-1423.80073529412));
#162500=CARTESIAN_POINT('Ctrl Pts',(14.4273846475923,-4.10494485108124,
-1425.29485294118));
#162501=CARTESIAN_POINT('Ctrl Pts',(14.0470054900687,-5.44183891826342,
-1426.78897058824));
#162502=CARTESIAN_POINT('Ctrl Pts',(13.4274493703259,-6.68607533664808,
-1428.28308823529));
#162503=CARTESIAN_POINT('Ctrl Pts',(12.8078932505832,-7.93031175503273,
-1429.77720588235));
#162504=CARTESIAN_POINT('Ctrl Pts',(11.9702584092036,-9.03951954568884,
-1431.27132352941));
#162505=CARTESIAN_POINT('Ctrl Pts',(11.132623567824,-10.148727336345,-1432.76544117647));
#162506=CARTESIAN_POINT('Ctrl Pts',(10.1054346546984,-11.0851337583099,
-1434.25955882353));
#162507=CARTESIAN_POINT('Ctrl Pts',(9.07824574157275,-12.0215401802748,
-1435.75367647059));
#162508=CARTESIAN_POINT('Ctrl Pts',(7.89648244316034,-12.7532570359442,
-1437.24779411765));
#162509=CARTESIAN_POINT('Ctrl Pts',(6.71471914474792,-13.4849738916136,
-1438.74191176471));
#162510=CARTESIAN_POINT('Ctrl Pts',(5.4186249928073,-13.9870834410653,-1440.23602941176));
#162511=CARTESIAN_POINT('Ctrl Pts',(4.12253084086667,-14.4891929905171,
-1441.73014705882));
#162512=CARTESIAN_POINT('Ctrl Pts',(2.75624276724855,-14.7445964952585,
-1443.22426470588));
#162513=CARTESIAN_POINT('Ctrl Pts',(1.38995469363045,-15.,-1444.71838235294));
#162514=CARTESIAN_POINT('Ctrl Pts',(0.,-15.,-1446.2125));
#162515=CARTESIAN_POINT('Ctrl Pts',(-1.38995469363045,-15.,-1447.70661764706));
#162516=CARTESIAN_POINT('Ctrl Pts',(-2.75624276724856,-14.7445964952585,
-1449.20073529412));
#162517=CARTESIAN_POINT('Ctrl Pts',(-4.12253084086666,-14.4891929905171,
-1450.69485294118));
#162518=CARTESIAN_POINT('Ctrl Pts',(-5.41862499280729,-13.9870834410653,
-1452.18897058824));
#162519=CARTESIAN_POINT('Ctrl Pts',(-6.71471914474793,-13.4849738916136,
-1453.68308823529));
#162520=CARTESIAN_POINT('Ctrl Pts',(-7.89648244316034,-12.7532570359442,
-1455.17720588235));
#162521=CARTESIAN_POINT('Ctrl Pts',(-9.07824574157275,-12.0215401802748,
-1456.67132352941));
#162522=CARTESIAN_POINT('Ctrl Pts',(-10.1054346546984,-11.0851337583099,
-1458.16544117647));
#162523=CARTESIAN_POINT('Ctrl Pts',(-11.132623567824,-10.148727336345,-1459.65955882353));
#162524=CARTESIAN_POINT('Ctrl Pts',(-11.9702584092036,-9.03951954568885,
-1461.15367647059));
#162525=CARTESIAN_POINT('Ctrl Pts',(-12.8078932505832,-7.93031175503273,
-1462.64779411765));
#162526=CARTESIAN_POINT('Ctrl Pts',(-13.4274493703259,-6.68607533664808,
-1464.14191176471));
#162527=CARTESIAN_POINT('Ctrl Pts',(-14.0470054900687,-5.44183891826343,
-1465.63602941176));
#162528=CARTESIAN_POINT('Ctrl Pts',(-14.4273846475923,-4.10494485108124,
-1467.13014705882));
#162529=CARTESIAN_POINT('Ctrl Pts',(-14.8077638051159,-2.76805078389906,
-1468.62426470588));
#162530=CARTESIAN_POINT('Ctrl Pts',(-14.9360126444255,-1.38402539194953,
-1470.11838235294));
#162531=CARTESIAN_POINT('Ctrl Pts',(-15.0642614837351,-9.22419980378748E-16,
-1471.6125));
#162532=CARTESIAN_POINT('Ctrl Pts',(-14.9360126444255,1.38402539194953,
-1473.10661764706));
#162533=CARTESIAN_POINT('Ctrl Pts',(-14.8077638051159,2.76805078389906,
-1474.60073529412));
#162534=CARTESIAN_POINT('Ctrl Pts',(-14.4273846475923,4.10494485108124,
-1476.09485294118));
#162535=CARTESIAN_POINT('Ctrl Pts',(-14.0470054900687,5.44183891826343,
-1477.58897058824));
#162536=CARTESIAN_POINT('Ctrl Pts',(-13.4274493703259,6.68607533664807,
-1479.08308823529));
#162537=CARTESIAN_POINT('Ctrl Pts',(-12.8078932505832,7.93031175503273,
-1480.57720588235));
#162538=CARTESIAN_POINT('Ctrl Pts',(-11.9702584092036,9.03951954568884,
-1482.07132352941));
#162539=CARTESIAN_POINT('Ctrl Pts',(-11.132623567824,10.148727336345,-1483.56544117647));
#162540=CARTESIAN_POINT('Ctrl Pts',(-10.1054346546984,11.0851337583099,
-1485.05955882353));
#162541=CARTESIAN_POINT('Ctrl Pts',(-9.07824574157275,12.0215401802748,
-1486.55367647059));
#162542=CARTESIAN_POINT('Ctrl Pts',(-7.89648244316034,12.7532570359442,
-1488.04779411765));
#162543=CARTESIAN_POINT('Ctrl Pts',(-6.71471914474793,13.4849738916136,
-1489.54191176471));
#162544=CARTESIAN_POINT('Ctrl Pts',(-5.41862499280729,13.9870834410653,
-1491.03602941176));
#162545=CARTESIAN_POINT('Ctrl Pts',(-4.12253084086667,14.4891929905171,
-1492.53014705882));
#162546=CARTESIAN_POINT('Ctrl Pts',(-2.75624276724856,14.7445964952585,
-1494.02426470588));
#162547=CARTESIAN_POINT('Ctrl Pts',(-1.38995469363044,15.,-1495.51838235294));
#162548=CARTESIAN_POINT('Ctrl Pts',(-1.83697019872103E-15,15.,-1497.0125));
#162549=CARTESIAN_POINT('Ctrl Pts',(1.38995469363045,15.,-1498.50661764706));
#162550=CARTESIAN_POINT('Ctrl Pts',(2.75624276724855,14.7445964952585,-1500.00073529412));
#162551=CARTESIAN_POINT('Ctrl Pts',(4.12253084086666,14.4891929905171,-1501.49485294118));
#162552=CARTESIAN_POINT('Ctrl Pts',(5.4186249928073,13.9870834410653,-1502.98897058824));
#162553=CARTESIAN_POINT('Ctrl Pts',(6.26768981235257,13.6581539776009,-1503.96775961254));
#162554=CARTESIAN_POINT('Ctrl Pts',(7.0707324233642,13.2289358225515,-1504.9503325767));
#162555=CARTESIAN_POINT('',(5.07842733458062,-17.3187724682607,692.));
#162556=CARTESIAN_POINT('Ctrl Pts',(4.22076739908463,-14.3939265859884,
691.999999999999));
#162557=CARTESIAN_POINT('Ctrl Pts',(4.36371072147063,-14.881400899031,691.999999999999));
#162558=CARTESIAN_POINT('Ctrl Pts',(4.50665404385759,-15.3688752120733,
692.));
#162559=CARTESIAN_POINT('Ctrl Pts',(4.79254068902232,-16.3438238394976,
692.));
#162560=CARTESIAN_POINT('Ctrl Pts',(4.9354840118019,-16.831298153879,692.000000000001));
#162561=CARTESIAN_POINT('Ctrl Pts',(5.07842733458062,-17.3187724682607,
692.000000000001));
#162562=CARTESIAN_POINT('',(0.,-18.048,1500.1875));
#162563=CARTESIAN_POINT('',(0.,-18.048,1500.1875));
#162564=CARTESIAN_POINT('Ctrl Pts',(0.,-18.048,1500.1875));
#162565=CARTESIAN_POINT('Ctrl Pts',(-1.67239348737614,-18.048,1498.69338235294));
#162566=CARTESIAN_POINT('Ctrl Pts',(-3.31631129755346,-17.7406985030951,
1497.19926470588));
#162567=CARTESIAN_POINT('Ctrl Pts',(-4.96022910773077,-17.4333970061901,
1495.70514705882));
#162568=CARTESIAN_POINT('Ctrl Pts',(-6.51968959134574,-16.8292587962898,
1494.21102941176));
#162569=CARTESIAN_POINT('Ctrl Pts',(-8.07915007496071,-16.2251205863895,
1492.71691176471));
#162570=CARTESIAN_POINT('Ctrl Pts',(-9.50104767561052,-15.3447188656481,
1491.22279411765));
#162571=CARTESIAN_POINT('Ctrl Pts',(-10.9229452762603,-14.4643171449067,
1489.72867647059));
#162572=CARTESIAN_POINT('Ctrl Pts',(-12.1588589765331,-13.3376329379985,
1488.23455882353));
#162573=CARTESIAN_POINT('Ctrl Pts',(-13.3947726768058,-12.2109487310903,
1486.74044117647));
#162574=CARTESIAN_POINT('Ctrl Pts',(-14.4026149179538,-10.8763499173728,
1485.24632352941));
#162575=CARTESIAN_POINT('Ctrl Pts',(-15.4104571591017,-9.54175110365538,
1483.75220588235));
#162576=CARTESIAN_POINT('Ctrl Pts',(-16.1559070823762,-8.04468584505497,
1482.25808823529));
#162577=CARTESIAN_POINT('Ctrl Pts',(-16.9013570056506,-6.54762058645456,
1480.76397058824));
#162578=CARTESIAN_POINT('Ctrl Pts',(-17.3590292079831,-4.93906964482095,
1479.26985294118));
#162579=CARTESIAN_POINT('Ctrl Pts',(-17.8167014103155,-3.33051870318735,
1477.77573529412));
#162580=CARTESIAN_POINT('Ctrl Pts',(-17.9710104137728,-1.66525935159368,
1476.28161764706));
#162581=CARTESIAN_POINT('Ctrl Pts',(-18.1253194172301,-1.10985572039171E-15,
1474.7875));
#162582=CARTESIAN_POINT('Ctrl Pts',(-17.9710104137728,1.66525935159367,
1473.29338235294));
#162583=CARTESIAN_POINT('Ctrl Pts',(-17.8167014103155,3.33051870318735,
1471.79926470588));
#162584=CARTESIAN_POINT('Ctrl Pts',(-17.3590292079831,4.93906964482096,
1470.30514705882));
#162585=CARTESIAN_POINT('Ctrl Pts',(-16.9013570056506,6.54762058645456,
1468.81102941176));
#162586=CARTESIAN_POINT('Ctrl Pts',(-16.1559070823762,8.04468584505497,
1467.31691176471));
#162587=CARTESIAN_POINT('Ctrl Pts',(-15.4104571591017,9.54175110365538,
1465.82279411765));
#162588=CARTESIAN_POINT('Ctrl Pts',(-14.4026149179538,10.8763499173728,
1464.32867647059));
#162589=CARTESIAN_POINT('Ctrl Pts',(-13.3947726768058,12.2109487310903,
1462.83455882353));
#162590=CARTESIAN_POINT('Ctrl Pts',(-12.1588589765331,13.3376329379985,
1461.34044117647));
#162591=CARTESIAN_POINT('Ctrl Pts',(-10.9229452762603,14.4643171449067,
1459.84632352941));
#162592=CARTESIAN_POINT('Ctrl Pts',(-9.50104767561052,15.3447188656481,
1458.35220588235));
#162593=CARTESIAN_POINT('Ctrl Pts',(-8.07915007496071,16.2251205863895,
1456.85808823529));
#162594=CARTESIAN_POINT('Ctrl Pts',(-6.51968959134574,16.8292587962898,
1455.36397058824));
#162595=CARTESIAN_POINT('Ctrl Pts',(-4.96022910773078,17.4333970061901,
1453.86985294118));
#162596=CARTESIAN_POINT('Ctrl Pts',(-3.31631129755346,17.7406985030951,
1452.37573529412));
#162597=CARTESIAN_POINT('Ctrl Pts',(-1.67239348737615,18.048,1450.88161764706));
#162598=CARTESIAN_POINT('Ctrl Pts',(-2.21024254310115E-15,18.048,1449.3875));
#162599=CARTESIAN_POINT('Ctrl Pts',(1.67239348737616,18.048,1447.89338235294));
#162600=CARTESIAN_POINT('Ctrl Pts',(3.31631129755346,17.7406985030951,1446.39926470588));
#162601=CARTESIAN_POINT('Ctrl Pts',(4.96022910773077,17.4333970061901,1444.90514705882));
#162602=CARTESIAN_POINT('Ctrl Pts',(6.51968959134575,16.8292587962898,1443.41102941176));
#162603=CARTESIAN_POINT('Ctrl Pts',(8.07915007496071,16.2251205863895,1441.91691176471));
#162604=CARTESIAN_POINT('Ctrl Pts',(9.50104767561053,15.3447188656481,1440.42279411765));
#162605=CARTESIAN_POINT('Ctrl Pts',(10.9229452762603,14.4643171449067,1438.92867647059));
#162606=CARTESIAN_POINT('Ctrl Pts',(12.1588589765331,13.3376329379985,1437.43455882353));
#162607=CARTESIAN_POINT('Ctrl Pts',(13.3947726768058,12.2109487310903,1435.94044117647));
#162608=CARTESIAN_POINT('Ctrl Pts',(14.4026149179538,10.8763499173728,1434.44632352941));
#162609=CARTESIAN_POINT('Ctrl Pts',(15.4104571591017,9.54175110365539,1432.95220588235));
#162610=CARTESIAN_POINT('Ctrl Pts',(16.1559070823762,8.04468584505496,1431.45808823529));
#162611=CARTESIAN_POINT('Ctrl Pts',(16.9013570056506,6.54762058645456,1429.96397058824));
#162612=CARTESIAN_POINT('Ctrl Pts',(17.3590292079831,4.93906964482096,1428.46985294118));
#162613=CARTESIAN_POINT('Ctrl Pts',(17.8167014103155,3.33051870318735,1426.97573529412));
#162614=CARTESIAN_POINT('Ctrl Pts',(17.9710104137728,1.66525935159367,1425.48161764706));
#162615=CARTESIAN_POINT('Ctrl Pts',(18.1253194172301,3.32956716117513E-15,
1423.9875));
#162616=CARTESIAN_POINT('Ctrl Pts',(17.9710104137728,-1.66525935159367,
1422.49338235294));
#162617=CARTESIAN_POINT('Ctrl Pts',(17.8167014103155,-3.33051870318736,
1420.99926470588));
#162618=CARTESIAN_POINT('Ctrl Pts',(17.3590292079831,-4.93906964482095,
1419.50514705882));
#162619=CARTESIAN_POINT('Ctrl Pts',(16.9013570056506,-6.54762058645456,
1418.01102941176));
#162620=CARTESIAN_POINT('Ctrl Pts',(16.1559070823762,-8.04468584505497,
1416.51691176471));
#162621=CARTESIAN_POINT('Ctrl Pts',(15.4104571591017,-9.54175110365538,
1415.02279411765));
#162622=CARTESIAN_POINT('Ctrl Pts',(14.4026149179538,-10.8763499173728,
1413.52867647059));
#162623=CARTESIAN_POINT('Ctrl Pts',(13.3947726768058,-12.2109487310903,
1412.03455882353));
#162624=CARTESIAN_POINT('Ctrl Pts',(12.1588589765331,-13.3376329379985,
1410.54044117647));
#162625=CARTESIAN_POINT('Ctrl Pts',(10.9229452762603,-14.4643171449067,
1409.04632352941));
#162626=CARTESIAN_POINT('Ctrl Pts',(9.50104767561053,-15.3447188656481,
1407.55220588235));
#162627=CARTESIAN_POINT('Ctrl Pts',(8.07915007496071,-16.2251205863895,
1406.05808823529));
#162628=CARTESIAN_POINT('Ctrl Pts',(6.51968959134574,-16.8292587962898,
1404.56397058824));
#162629=CARTESIAN_POINT('Ctrl Pts',(4.96022910773078,-17.4333970061901,
1403.06985294118));
#162630=CARTESIAN_POINT('Ctrl Pts',(3.31631129755346,-17.7406985030951,
1401.57573529412));
#162631=CARTESIAN_POINT('Ctrl Pts',(1.67239348737615,-18.048,1400.08161764706));
#162632=CARTESIAN_POINT('Ctrl Pts',(0.,-18.048,1398.5875));
#162633=CARTESIAN_POINT('Ctrl Pts',(-1.67239348737615,-18.048,1397.09338235294));
#162634=CARTESIAN_POINT('Ctrl Pts',(-3.31631129755346,-17.7406985030951,
1395.59926470588));
#162635=CARTESIAN_POINT('Ctrl Pts',(-4.96022910773077,-17.4333970061901,
1394.10514705882));
#162636=CARTESIAN_POINT('Ctrl Pts',(-6.51968959134574,-16.8292587962898,
1392.61102941176));
#162637=CARTESIAN_POINT('Ctrl Pts',(-8.07915007496071,-16.2251205863895,
1391.11691176471));
#162638=CARTESIAN_POINT('Ctrl Pts',(-9.50104767561052,-15.3447188656481,
1389.62279411765));
#162639=CARTESIAN_POINT('Ctrl Pts',(-10.9229452762603,-14.4643171449067,
1388.12867647059));
#162640=CARTESIAN_POINT('Ctrl Pts',(-12.1588589765331,-13.3376329379985,
1386.63455882353));
#162641=CARTESIAN_POINT('Ctrl Pts',(-13.3947726768058,-12.2109487310903,
1385.14044117647));
#162642=CARTESIAN_POINT('Ctrl Pts',(-14.4026149179538,-10.8763499173728,
1383.64632352941));
#162643=CARTESIAN_POINT('Ctrl Pts',(-15.4104571591017,-9.54175110365538,
1382.15220588235));
#162644=CARTESIAN_POINT('Ctrl Pts',(-16.1559070823762,-8.04468584505497,
1380.65808823529));
#162645=CARTESIAN_POINT('Ctrl Pts',(-16.9013570056506,-6.54762058645456,
1379.16397058824));
#162646=CARTESIAN_POINT('Ctrl Pts',(-17.3590292079831,-4.93906964482095,
1377.66985294118));
#162647=CARTESIAN_POINT('Ctrl Pts',(-17.8167014103155,-3.33051870318735,
1376.17573529412));
#162648=CARTESIAN_POINT('Ctrl Pts',(-17.9710104137728,-1.66525935159368,
1374.68161764706));
#162649=CARTESIAN_POINT('Ctrl Pts',(-18.1253194172301,-1.10985572039171E-15,
1373.1875));
#162650=CARTESIAN_POINT('Ctrl Pts',(-17.9710104137728,1.66525935159367,
1371.69338235294));
#162651=CARTESIAN_POINT('Ctrl Pts',(-17.8167014103155,3.33051870318735,
1370.19926470588));
#162652=CARTESIAN_POINT('Ctrl Pts',(-17.3590292079831,4.93906964482096,
1368.70514705882));
#162653=CARTESIAN_POINT('Ctrl Pts',(-16.9013570056506,6.54762058645456,
1367.21102941176));
#162654=CARTESIAN_POINT('Ctrl Pts',(-16.1559070823762,8.04468584505497,
1365.71691176471));
#162655=CARTESIAN_POINT('Ctrl Pts',(-15.4104571591017,9.54175110365538,
1364.22279411765));
#162656=CARTESIAN_POINT('Ctrl Pts',(-14.4026149179538,10.8763499173728,
1362.72867647059));
#162657=CARTESIAN_POINT('Ctrl Pts',(-13.3947726768058,12.2109487310903,
1361.23455882353));
#162658=CARTESIAN_POINT('Ctrl Pts',(-12.1588589765331,13.3376329379985,
1359.74044117647));
#162659=CARTESIAN_POINT('Ctrl Pts',(-10.9229452762603,14.4643171449067,
1358.24632352941));
#162660=CARTESIAN_POINT('Ctrl Pts',(-9.50104767561052,15.3447188656481,
1356.75220588235));
#162661=CARTESIAN_POINT('Ctrl Pts',(-8.07915007496071,16.2251205863895,
1355.25808823529));
#162662=CARTESIAN_POINT('Ctrl Pts',(-6.51968959134574,16.8292587962898,
1353.76397058824));
#162663=CARTESIAN_POINT('Ctrl Pts',(-4.96022910773078,17.4333970061901,
1352.26985294118));
#162664=CARTESIAN_POINT('Ctrl Pts',(-3.31631129755346,17.7406985030951,
1350.77573529412));
#162665=CARTESIAN_POINT('Ctrl Pts',(-1.67239348737615,18.048,1349.28161764706));
#162666=CARTESIAN_POINT('Ctrl Pts',(-2.21024254310115E-15,18.048,1347.7875));
#162667=CARTESIAN_POINT('Ctrl Pts',(1.67239348737616,18.048,1346.29338235294));
#162668=CARTESIAN_POINT('Ctrl Pts',(3.31631129755346,17.7406985030951,1344.79926470588));
#162669=CARTESIAN_POINT('Ctrl Pts',(4.96022910773077,17.4333970061901,1343.30514705882));
#162670=CARTESIAN_POINT('Ctrl Pts',(6.51968959134575,16.8292587962898,1341.81102941176));
#162671=CARTESIAN_POINT('Ctrl Pts',(8.07915007496071,16.2251205863895,1340.31691176471));
#162672=CARTESIAN_POINT('Ctrl Pts',(9.50104767561053,15.3447188656481,1338.82279411765));
#162673=CARTESIAN_POINT('Ctrl Pts',(10.9229452762603,14.4643171449067,1337.32867647059));
#162674=CARTESIAN_POINT('Ctrl Pts',(12.1588589765331,13.3376329379985,1335.83455882353));
#162675=CARTESIAN_POINT('Ctrl Pts',(13.3947726768058,12.2109487310903,1334.34044117647));
#162676=CARTESIAN_POINT('Ctrl Pts',(14.4026149179538,10.8763499173728,1332.84632352941));
#162677=CARTESIAN_POINT('Ctrl Pts',(15.4104571591017,9.54175110365539,1331.35220588235));
#162678=CARTESIAN_POINT('Ctrl Pts',(16.1559070823762,8.04468584505496,1329.85808823529));
#162679=CARTESIAN_POINT('Ctrl Pts',(16.9013570056506,6.54762058645456,1328.36397058824));
#162680=CARTESIAN_POINT('Ctrl Pts',(17.3590292079831,4.93906964482096,1326.86985294118));
#162681=CARTESIAN_POINT('Ctrl Pts',(17.8167014103155,3.33051870318735,1325.37573529412));
#162682=CARTESIAN_POINT('Ctrl Pts',(17.9710104137728,1.66525935159367,1323.88161764706));
#162683=CARTESIAN_POINT('Ctrl Pts',(18.1253194172301,3.32956716117513E-15,
1322.3875));
#162684=CARTESIAN_POINT('Ctrl Pts',(17.9710104137728,-1.66525935159367,
1320.89338235294));
#162685=CARTESIAN_POINT('Ctrl Pts',(17.8167014103155,-3.33051870318736,
1319.39926470588));
#162686=CARTESIAN_POINT('Ctrl Pts',(17.3590292079831,-4.93906964482095,
1317.90514705882));
#162687=CARTESIAN_POINT('Ctrl Pts',(16.9013570056506,-6.54762058645456,
1316.41102941176));
#162688=CARTESIAN_POINT('Ctrl Pts',(16.1559070823762,-8.04468584505497,
1314.91691176471));
#162689=CARTESIAN_POINT('Ctrl Pts',(15.4104571591017,-9.54175110365538,
1313.42279411765));
#162690=CARTESIAN_POINT('Ctrl Pts',(14.4026149179538,-10.8763499173728,
1311.92867647059));
#162691=CARTESIAN_POINT('Ctrl Pts',(13.3947726768058,-12.2109487310903,
1310.43455882353));
#162692=CARTESIAN_POINT('Ctrl Pts',(12.1588589765331,-13.3376329379985,
1308.94044117647));
#162693=CARTESIAN_POINT('Ctrl Pts',(10.9229452762603,-14.4643171449067,
1307.44632352941));
#162694=CARTESIAN_POINT('Ctrl Pts',(9.50104767561053,-15.3447188656481,
1305.95220588235));
#162695=CARTESIAN_POINT('Ctrl Pts',(8.07915007496071,-16.2251205863895,
1304.45808823529));
#162696=CARTESIAN_POINT('Ctrl Pts',(6.51968959134574,-16.8292587962898,
1302.96397058824));
#162697=CARTESIAN_POINT('Ctrl Pts',(4.96022910773078,-17.4333970061901,
1301.46985294118));
#162698=CARTESIAN_POINT('Ctrl Pts',(3.31631129755346,-17.7406985030951,
1299.97573529412));
#162699=CARTESIAN_POINT('Ctrl Pts',(1.67239348737615,-18.048,1298.48161764706));
#162700=CARTESIAN_POINT('Ctrl Pts',(0.,-18.048,1296.9875));
#162701=CARTESIAN_POINT('Ctrl Pts',(-1.67239348737615,-18.048,1295.49338235294));
#162702=CARTESIAN_POINT('Ctrl Pts',(-3.31631129755346,-17.7406985030951,
1293.99926470588));
#162703=CARTESIAN_POINT('Ctrl Pts',(-4.96022910773077,-17.4333970061901,
1292.50514705882));
#162704=CARTESIAN_POINT('Ctrl Pts',(-6.51968959134574,-16.8292587962898,
1291.01102941176));
#162705=CARTESIAN_POINT('Ctrl Pts',(-8.07915007496071,-16.2251205863895,
1289.51691176471));
#162706=CARTESIAN_POINT('Ctrl Pts',(-9.50104767561052,-15.3447188656481,
1288.02279411765));
#162707=CARTESIAN_POINT('Ctrl Pts',(-10.9229452762603,-14.4643171449067,
1286.52867647059));
#162708=CARTESIAN_POINT('Ctrl Pts',(-12.1588589765331,-13.3376329379985,
1285.03455882353));
#162709=CARTESIAN_POINT('Ctrl Pts',(-13.3947726768058,-12.2109487310903,
1283.54044117647));
#162710=CARTESIAN_POINT('Ctrl Pts',(-14.4026149179538,-10.8763499173728,
1282.04632352941));
#162711=CARTESIAN_POINT('Ctrl Pts',(-15.4104571591017,-9.54175110365538,
1280.55220588235));
#162712=CARTESIAN_POINT('Ctrl Pts',(-16.1559070823762,-8.04468584505497,
1279.05808823529));
#162713=CARTESIAN_POINT('Ctrl Pts',(-16.9013570056506,-6.54762058645456,
1277.56397058824));
#162714=CARTESIAN_POINT('Ctrl Pts',(-17.3590292079831,-4.93906964482095,
1276.06985294118));
#162715=CARTESIAN_POINT('Ctrl Pts',(-17.8167014103155,-3.33051870318735,
1274.57573529412));
#162716=CARTESIAN_POINT('Ctrl Pts',(-17.9710104137728,-1.66525935159368,
1273.08161764706));
#162717=CARTESIAN_POINT('Ctrl Pts',(-18.1253194172301,-1.10985572039171E-15,
1271.5875));
#162718=CARTESIAN_POINT('Ctrl Pts',(-17.9710104137728,1.66525935159367,
1270.09338235294));
#162719=CARTESIAN_POINT('Ctrl Pts',(-17.8167014103155,3.33051870318735,
1268.59926470588));
#162720=CARTESIAN_POINT('Ctrl Pts',(-17.3590292079831,4.93906964482096,
1267.10514705882));
#162721=CARTESIAN_POINT('Ctrl Pts',(-16.9013570056506,6.54762058645456,
1265.61102941176));
#162722=CARTESIAN_POINT('Ctrl Pts',(-16.1559070823762,8.04468584505497,
1264.11691176471));
#162723=CARTESIAN_POINT('Ctrl Pts',(-15.4104571591017,9.54175110365538,
1262.62279411765));
#162724=CARTESIAN_POINT('Ctrl Pts',(-14.4026149179538,10.8763499173728,
1261.12867647059));
#162725=CARTESIAN_POINT('Ctrl Pts',(-13.3947726768058,12.2109487310903,
1259.63455882353));
#162726=CARTESIAN_POINT('Ctrl Pts',(-12.1588589765331,13.3376329379985,
1258.14044117647));
#162727=CARTESIAN_POINT('Ctrl Pts',(-10.9229452762603,14.4643171449067,
1256.64632352941));
#162728=CARTESIAN_POINT('Ctrl Pts',(-9.50104767561052,15.3447188656481,
1255.15220588235));
#162729=CARTESIAN_POINT('Ctrl Pts',(-8.07915007496071,16.2251205863895,
1253.65808823529));
#162730=CARTESIAN_POINT('Ctrl Pts',(-6.51968959134574,16.8292587962898,
1252.16397058824));
#162731=CARTESIAN_POINT('Ctrl Pts',(-4.96022910773078,17.4333970061901,
1250.66985294118));
#162732=CARTESIAN_POINT('Ctrl Pts',(-3.31631129755346,17.7406985030951,
1249.17573529412));
#162733=CARTESIAN_POINT('Ctrl Pts',(-1.67239348737615,18.048,1247.68161764706));
#162734=CARTESIAN_POINT('Ctrl Pts',(-2.21024254310115E-15,18.048,1246.1875));
#162735=CARTESIAN_POINT('Ctrl Pts',(1.67239348737616,18.048,1244.69338235294));
#162736=CARTESIAN_POINT('Ctrl Pts',(3.31631129755346,17.7406985030951,1243.19926470588));
#162737=CARTESIAN_POINT('Ctrl Pts',(4.96022910773077,17.4333970061901,1241.70514705882));
#162738=CARTESIAN_POINT('Ctrl Pts',(6.51968959134575,16.8292587962898,1240.21102941176));
#162739=CARTESIAN_POINT('Ctrl Pts',(8.07915007496071,16.2251205863895,1238.71691176471));
#162740=CARTESIAN_POINT('Ctrl Pts',(9.50104767561053,15.3447188656481,1237.22279411765));
#162741=CARTESIAN_POINT('Ctrl Pts',(10.9229452762603,14.4643171449067,1235.72867647059));
#162742=CARTESIAN_POINT('Ctrl Pts',(12.1588589765331,13.3376329379985,1234.23455882353));
#162743=CARTESIAN_POINT('Ctrl Pts',(13.3947726768058,12.2109487310903,1232.74044117647));
#162744=CARTESIAN_POINT('Ctrl Pts',(14.4026149179538,10.8763499173728,1231.24632352941));
#162745=CARTESIAN_POINT('Ctrl Pts',(15.4104571591017,9.54175110365539,1229.75220588235));
#162746=CARTESIAN_POINT('Ctrl Pts',(16.1559070823762,8.04468584505496,1228.25808823529));
#162747=CARTESIAN_POINT('Ctrl Pts',(16.9013570056506,6.54762058645456,1226.76397058824));
#162748=CARTESIAN_POINT('Ctrl Pts',(17.3590292079831,4.93906964482096,1225.26985294118));
#162749=CARTESIAN_POINT('Ctrl Pts',(17.8167014103155,3.33051870318735,1223.77573529412));
#162750=CARTESIAN_POINT('Ctrl Pts',(17.9710104137728,1.66525935159367,1222.28161764706));
#162751=CARTESIAN_POINT('Ctrl Pts',(18.1253194172301,3.32956716117513E-15,
1220.7875));
#162752=CARTESIAN_POINT('Ctrl Pts',(17.9710104137728,-1.66525935159367,
1219.29338235294));
#162753=CARTESIAN_POINT('Ctrl Pts',(17.8167014103155,-3.33051870318736,
1217.79926470588));
#162754=CARTESIAN_POINT('Ctrl Pts',(17.3590292079831,-4.93906964482095,
1216.30514705882));
#162755=CARTESIAN_POINT('Ctrl Pts',(16.9013570056506,-6.54762058645456,
1214.81102941176));
#162756=CARTESIAN_POINT('Ctrl Pts',(16.1559070823762,-8.04468584505497,
1213.31691176471));
#162757=CARTESIAN_POINT('Ctrl Pts',(15.4104571591017,-9.54175110365538,
1211.82279411765));
#162758=CARTESIAN_POINT('Ctrl Pts',(14.4026149179538,-10.8763499173728,
1210.32867647059));
#162759=CARTESIAN_POINT('Ctrl Pts',(13.3947726768058,-12.2109487310903,
1208.83455882353));
#162760=CARTESIAN_POINT('Ctrl Pts',(12.1588589765331,-13.3376329379985,
1207.34044117647));
#162761=CARTESIAN_POINT('Ctrl Pts',(10.9229452762603,-14.4643171449067,
1205.84632352941));
#162762=CARTESIAN_POINT('Ctrl Pts',(9.50104767561053,-15.3447188656481,
1204.35220588235));
#162763=CARTESIAN_POINT('Ctrl Pts',(8.07915007496071,-16.2251205863895,
1202.85808823529));
#162764=CARTESIAN_POINT('Ctrl Pts',(6.51968959134574,-16.8292587962898,
1201.36397058824));
#162765=CARTESIAN_POINT('Ctrl Pts',(4.96022910773078,-17.4333970061901,
1199.86985294118));
#162766=CARTESIAN_POINT('Ctrl Pts',(3.31631129755346,-17.7406985030951,
1198.37573529412));
#162767=CARTESIAN_POINT('Ctrl Pts',(1.67239348737615,-18.048,1196.88161764706));
#162768=CARTESIAN_POINT('Ctrl Pts',(0.,-18.048,1195.3875));
#162769=CARTESIAN_POINT('Ctrl Pts',(-1.67239348737615,-18.048,1193.89338235294));
#162770=CARTESIAN_POINT('Ctrl Pts',(-3.31631129755346,-17.7406985030951,
1192.39926470588));
#162771=CARTESIAN_POINT('Ctrl Pts',(-4.96022910773077,-17.4333970061901,
1190.90514705882));
#162772=CARTESIAN_POINT('Ctrl Pts',(-6.51968959134574,-16.8292587962898,
1189.41102941176));
#162773=CARTESIAN_POINT('Ctrl Pts',(-8.07915007496071,-16.2251205863895,
1187.91691176471));
#162774=CARTESIAN_POINT('Ctrl Pts',(-9.50104767561052,-15.3447188656481,
1186.42279411765));
#162775=CARTESIAN_POINT('Ctrl Pts',(-10.9229452762603,-14.4643171449067,
1184.92867647059));
#162776=CARTESIAN_POINT('Ctrl Pts',(-12.1588589765331,-13.3376329379985,
1183.43455882353));
#162777=CARTESIAN_POINT('Ctrl Pts',(-13.3947726768058,-12.2109487310903,
1181.94044117647));
#162778=CARTESIAN_POINT('Ctrl Pts',(-14.4026149179538,-10.8763499173728,
1180.44632352941));
#162779=CARTESIAN_POINT('Ctrl Pts',(-15.4104571591017,-9.54175110365538,
1178.95220588235));
#162780=CARTESIAN_POINT('Ctrl Pts',(-16.1559070823762,-8.04468584505497,
1177.45808823529));
#162781=CARTESIAN_POINT('Ctrl Pts',(-16.9013570056506,-6.54762058645456,
1175.96397058824));
#162782=CARTESIAN_POINT('Ctrl Pts',(-17.3590292079831,-4.93906964482095,
1174.46985294118));
#162783=CARTESIAN_POINT('Ctrl Pts',(-17.8167014103155,-3.33051870318735,
1172.97573529412));
#162784=CARTESIAN_POINT('Ctrl Pts',(-17.9710104137728,-1.66525935159368,
1171.48161764706));
#162785=CARTESIAN_POINT('Ctrl Pts',(-18.1253194172301,-1.10985572039171E-15,
1169.9875));
#162786=CARTESIAN_POINT('Ctrl Pts',(-17.9710104137728,1.66525935159367,
1168.49338235294));
#162787=CARTESIAN_POINT('Ctrl Pts',(-17.8167014103155,3.33051870318735,
1166.99926470588));
#162788=CARTESIAN_POINT('Ctrl Pts',(-17.3590292079831,4.93906964482096,
1165.50514705882));
#162789=CARTESIAN_POINT('Ctrl Pts',(-16.9013570056506,6.54762058645456,
1164.01102941176));
#162790=CARTESIAN_POINT('Ctrl Pts',(-16.1559070823762,8.04468584505497,
1162.51691176471));
#162791=CARTESIAN_POINT('Ctrl Pts',(-15.4104571591017,9.54175110365538,
1161.02279411765));
#162792=CARTESIAN_POINT('Ctrl Pts',(-14.4026149179538,10.8763499173728,
1159.52867647059));
#162793=CARTESIAN_POINT('Ctrl Pts',(-13.3947726768058,12.2109487310903,
1158.03455882353));
#162794=CARTESIAN_POINT('Ctrl Pts',(-12.1588589765331,13.3376329379985,
1156.54044117647));
#162795=CARTESIAN_POINT('Ctrl Pts',(-10.9229452762603,14.4643171449067,
1155.04632352941));
#162796=CARTESIAN_POINT('Ctrl Pts',(-9.50104767561052,15.3447188656481,
1153.55220588235));
#162797=CARTESIAN_POINT('Ctrl Pts',(-8.07915007496071,16.2251205863895,
1152.05808823529));
#162798=CARTESIAN_POINT('Ctrl Pts',(-6.51968959134574,16.8292587962898,
1150.56397058824));
#162799=CARTESIAN_POINT('Ctrl Pts',(-4.96022910773078,17.4333970061901,
1149.06985294118));
#162800=CARTESIAN_POINT('Ctrl Pts',(-3.31631129755346,17.7406985030951,
1147.57573529412));
#162801=CARTESIAN_POINT('Ctrl Pts',(-1.67239348737615,18.048,1146.08161764706));
#162802=CARTESIAN_POINT('Ctrl Pts',(-2.21024254310115E-15,18.048,1144.5875));
#162803=CARTESIAN_POINT('Ctrl Pts',(1.67239348737616,18.048,1143.09338235294));
#162804=CARTESIAN_POINT('Ctrl Pts',(3.31631129755346,17.7406985030951,1141.59926470588));
#162805=CARTESIAN_POINT('Ctrl Pts',(4.96022910773077,17.4333970061901,1140.10514705882));
#162806=CARTESIAN_POINT('Ctrl Pts',(6.51968959134575,16.8292587962898,1138.61102941176));
#162807=CARTESIAN_POINT('Ctrl Pts',(8.07915007496071,16.2251205863895,1137.11691176471));
#162808=CARTESIAN_POINT('Ctrl Pts',(9.50104767561053,15.3447188656481,1135.62279411765));
#162809=CARTESIAN_POINT('Ctrl Pts',(10.9229452762603,14.4643171449067,1134.12867647059));
#162810=CARTESIAN_POINT('Ctrl Pts',(12.1588589765331,13.3376329379985,1132.63455882353));
#162811=CARTESIAN_POINT('Ctrl Pts',(13.3947726768058,12.2109487310903,1131.14044117647));
#162812=CARTESIAN_POINT('Ctrl Pts',(14.4026149179538,10.8763499173728,1129.64632352941));
#162813=CARTESIAN_POINT('Ctrl Pts',(15.4104571591017,9.54175110365539,1128.15220588235));
#162814=CARTESIAN_POINT('Ctrl Pts',(16.1559070823762,8.04468584505496,1126.65808823529));
#162815=CARTESIAN_POINT('Ctrl Pts',(16.9013570056506,6.54762058645456,1125.16397058824));
#162816=CARTESIAN_POINT('Ctrl Pts',(17.3590292079831,4.93906964482096,1123.66985294118));
#162817=CARTESIAN_POINT('Ctrl Pts',(17.8167014103155,3.33051870318735,1122.17573529412));
#162818=CARTESIAN_POINT('Ctrl Pts',(17.9710104137728,1.66525935159367,1120.68161764706));
#162819=CARTESIAN_POINT('Ctrl Pts',(18.1253194172301,3.32956716117513E-15,
1119.1875));
#162820=CARTESIAN_POINT('Ctrl Pts',(17.9710104137728,-1.66525935159367,
1117.69338235294));
#162821=CARTESIAN_POINT('Ctrl Pts',(17.8167014103155,-3.33051870318736,
1116.19926470588));
#162822=CARTESIAN_POINT('Ctrl Pts',(17.3590292079831,-4.93906964482095,
1114.70514705882));
#162823=CARTESIAN_POINT('Ctrl Pts',(16.9013570056506,-6.54762058645456,
1113.21102941176));
#162824=CARTESIAN_POINT('Ctrl Pts',(16.1559070823762,-8.04468584505497,
1111.71691176471));
#162825=CARTESIAN_POINT('Ctrl Pts',(15.4104571591017,-9.54175110365538,
1110.22279411765));
#162826=CARTESIAN_POINT('Ctrl Pts',(14.4026149179538,-10.8763499173728,
1108.72867647059));
#162827=CARTESIAN_POINT('Ctrl Pts',(13.3947726768058,-12.2109487310903,
1107.23455882353));
#162828=CARTESIAN_POINT('Ctrl Pts',(12.1588589765331,-13.3376329379985,
1105.74044117647));
#162829=CARTESIAN_POINT('Ctrl Pts',(10.9229452762603,-14.4643171449067,
1104.24632352941));
#162830=CARTESIAN_POINT('Ctrl Pts',(9.50104767561053,-15.3447188656481,
1102.75220588235));
#162831=CARTESIAN_POINT('Ctrl Pts',(8.07915007496071,-16.2251205863895,
1101.25808823529));
#162832=CARTESIAN_POINT('Ctrl Pts',(6.51968959134574,-16.8292587962898,
1099.76397058824));
#162833=CARTESIAN_POINT('Ctrl Pts',(4.96022910773078,-17.4333970061901,
1098.26985294118));
#162834=CARTESIAN_POINT('Ctrl Pts',(3.31631129755346,-17.7406985030951,
1096.77573529412));
#162835=CARTESIAN_POINT('Ctrl Pts',(1.67239348737615,-18.048,1095.28161764706));
#162836=CARTESIAN_POINT('Ctrl Pts',(0.,-18.048,1093.7875));
#162837=CARTESIAN_POINT('Ctrl Pts',(-1.67239348737615,-18.048,1092.29338235294));
#162838=CARTESIAN_POINT('Ctrl Pts',(-3.31631129755346,-17.7406985030951,
1090.79926470588));
#162839=CARTESIAN_POINT('Ctrl Pts',(-4.96022910773077,-17.4333970061901,
1089.30514705882));
#162840=CARTESIAN_POINT('Ctrl Pts',(-6.51968959134574,-16.8292587962898,
1087.81102941176));
#162841=CARTESIAN_POINT('Ctrl Pts',(-8.07915007496071,-16.2251205863895,
1086.31691176471));
#162842=CARTESIAN_POINT('Ctrl Pts',(-9.50104767561052,-15.3447188656481,
1084.82279411765));
#162843=CARTESIAN_POINT('Ctrl Pts',(-10.9229452762603,-14.4643171449067,
1083.32867647059));
#162844=CARTESIAN_POINT('Ctrl Pts',(-12.1588589765331,-13.3376329379985,
1081.83455882353));
#162845=CARTESIAN_POINT('Ctrl Pts',(-13.3947726768058,-12.2109487310903,
1080.34044117647));
#162846=CARTESIAN_POINT('Ctrl Pts',(-14.4026149179538,-10.8763499173728,
1078.84632352941));
#162847=CARTESIAN_POINT('Ctrl Pts',(-15.4104571591017,-9.54175110365538,
1077.35220588235));
#162848=CARTESIAN_POINT('Ctrl Pts',(-16.1559070823762,-8.04468584505497,
1075.85808823529));
#162849=CARTESIAN_POINT('Ctrl Pts',(-16.9013570056506,-6.54762058645456,
1074.36397058824));
#162850=CARTESIAN_POINT('Ctrl Pts',(-17.3590292079831,-4.93906964482095,
1072.86985294118));
#162851=CARTESIAN_POINT('Ctrl Pts',(-17.8167014103155,-3.33051870318735,
1071.37573529412));
#162852=CARTESIAN_POINT('Ctrl Pts',(-17.9710104137728,-1.66525935159368,
1069.88161764706));
#162853=CARTESIAN_POINT('Ctrl Pts',(-18.1253194172301,-1.10985572039171E-15,
1068.3875));
#162854=CARTESIAN_POINT('Ctrl Pts',(-17.9710104137728,1.66525935159367,
1066.89338235294));
#162855=CARTESIAN_POINT('Ctrl Pts',(-17.8167014103155,3.33051870318735,
1065.39926470588));
#162856=CARTESIAN_POINT('Ctrl Pts',(-17.3590292079831,4.93906964482096,
1063.90514705882));
#162857=CARTESIAN_POINT('Ctrl Pts',(-16.9013570056506,6.54762058645456,
1062.41102941176));
#162858=CARTESIAN_POINT('Ctrl Pts',(-16.1559070823762,8.04468584505497,
1060.91691176471));
#162859=CARTESIAN_POINT('Ctrl Pts',(-15.4104571591017,9.54175110365538,
1059.42279411765));
#162860=CARTESIAN_POINT('Ctrl Pts',(-14.4026149179538,10.8763499173728,
1057.92867647059));
#162861=CARTESIAN_POINT('Ctrl Pts',(-13.3947726768058,12.2109487310903,
1056.43455882353));
#162862=CARTESIAN_POINT('Ctrl Pts',(-12.1588589765331,13.3376329379985,
1054.94044117647));
#162863=CARTESIAN_POINT('Ctrl Pts',(-10.9229452762603,14.4643171449067,
1053.44632352941));
#162864=CARTESIAN_POINT('Ctrl Pts',(-9.50104767561052,15.3447188656481,
1051.95220588235));
#162865=CARTESIAN_POINT('Ctrl Pts',(-8.07915007496071,16.2251205863895,
1050.45808823529));
#162866=CARTESIAN_POINT('Ctrl Pts',(-6.51968959134574,16.8292587962898,
1048.96397058824));
#162867=CARTESIAN_POINT('Ctrl Pts',(-4.96022910773078,17.4333970061901,
1047.46985294118));
#162868=CARTESIAN_POINT('Ctrl Pts',(-3.31631129755346,17.7406985030951,
1045.97573529412));
#162869=CARTESIAN_POINT('Ctrl Pts',(-1.67239348737615,18.048,1044.48161764706));
#162870=CARTESIAN_POINT('Ctrl Pts',(-2.21024254310115E-15,18.048,1042.9875));
#162871=CARTESIAN_POINT('Ctrl Pts',(1.67239348737616,18.048,1041.49338235294));
#162872=CARTESIAN_POINT('Ctrl Pts',(3.31631129755346,17.7406985030951,1039.99926470588));
#162873=CARTESIAN_POINT('Ctrl Pts',(4.96022910773077,17.4333970061901,1038.50514705882));
#162874=CARTESIAN_POINT('Ctrl Pts',(6.51968959134575,16.8292587962898,1037.01102941176));
#162875=CARTESIAN_POINT('Ctrl Pts',(8.07915007496071,16.2251205863895,1035.51691176471));
#162876=CARTESIAN_POINT('Ctrl Pts',(9.50104767561053,15.3447188656481,1034.02279411765));
#162877=CARTESIAN_POINT('Ctrl Pts',(10.9229452762603,14.4643171449067,1032.52867647059));
#162878=CARTESIAN_POINT('Ctrl Pts',(12.1588589765331,13.3376329379985,1031.03455882353));
#162879=CARTESIAN_POINT('Ctrl Pts',(13.3947726768058,12.2109487310903,1029.54044117647));
#162880=CARTESIAN_POINT('Ctrl Pts',(14.4026149179538,10.8763499173728,1028.04632352941));
#162881=CARTESIAN_POINT('Ctrl Pts',(15.4104571591017,9.54175110365539,1026.55220588235));
#162882=CARTESIAN_POINT('Ctrl Pts',(16.1559070823762,8.04468584505496,1025.05808823529));
#162883=CARTESIAN_POINT('Ctrl Pts',(16.9013570056506,6.54762058645456,1023.56397058824));
#162884=CARTESIAN_POINT('Ctrl Pts',(17.3590292079831,4.93906964482096,1022.06985294118));
#162885=CARTESIAN_POINT('Ctrl Pts',(17.8167014103155,3.33051870318735,1020.57573529412));
#162886=CARTESIAN_POINT('Ctrl Pts',(17.9710104137728,1.66525935159367,1019.08161764706));
#162887=CARTESIAN_POINT('Ctrl Pts',(18.1253194172301,3.32956716117513E-15,
1017.5875));
#162888=CARTESIAN_POINT('Ctrl Pts',(17.9710104137728,-1.66525935159367,
1016.09338235294));
#162889=CARTESIAN_POINT('Ctrl Pts',(17.8167014103155,-3.33051870318736,
1014.59926470588));
#162890=CARTESIAN_POINT('Ctrl Pts',(17.3590292079831,-4.93906964482095,
1013.10514705882));
#162891=CARTESIAN_POINT('Ctrl Pts',(16.9013570056506,-6.54762058645456,
1011.61102941177));
#162892=CARTESIAN_POINT('Ctrl Pts',(16.1559070823762,-8.04468584505497,
1010.11691176471));
#162893=CARTESIAN_POINT('Ctrl Pts',(15.4104571591017,-9.54175110365538,
1008.62279411765));
#162894=CARTESIAN_POINT('Ctrl Pts',(14.4026149179538,-10.8763499173728,
1007.12867647059));
#162895=CARTESIAN_POINT('Ctrl Pts',(13.3947726768058,-12.2109487310903,
1005.63455882353));
#162896=CARTESIAN_POINT('Ctrl Pts',(12.1588589765331,-13.3376329379985,
1004.14044117647));
#162897=CARTESIAN_POINT('Ctrl Pts',(10.9229452762603,-14.4643171449067,
1002.64632352941));
#162898=CARTESIAN_POINT('Ctrl Pts',(9.50104767561053,-15.3447188656481,
1001.15220588235));
#162899=CARTESIAN_POINT('Ctrl Pts',(8.07915007496071,-16.2251205863895,
999.658088235294));
#162900=CARTESIAN_POINT('Ctrl Pts',(6.51968959134574,-16.8292587962898,
998.163970588235));
#162901=CARTESIAN_POINT('Ctrl Pts',(4.96022910773078,-17.4333970061901,
996.669852941177));
#162902=CARTESIAN_POINT('Ctrl Pts',(3.31631129755346,-17.7406985030951,
995.175735294118));
#162903=CARTESIAN_POINT('Ctrl Pts',(1.67239348737615,-18.048,993.681617647059));
#162904=CARTESIAN_POINT('Ctrl Pts',(0.,-18.048,992.1875));
#162905=CARTESIAN_POINT('Ctrl Pts',(-1.67239348737615,-18.048,990.693382352941));
#162906=CARTESIAN_POINT('Ctrl Pts',(-3.31631129755346,-17.7406985030951,
989.199264705882));
#162907=CARTESIAN_POINT('Ctrl Pts',(-4.96022910773077,-17.4333970061901,
987.705147058824));
#162908=CARTESIAN_POINT('Ctrl Pts',(-6.51968959134574,-16.8292587962898,
986.211029411765));
#162909=CARTESIAN_POINT('Ctrl Pts',(-8.07915007496071,-16.2251205863895,
984.716911764706));
#162910=CARTESIAN_POINT('Ctrl Pts',(-9.50104767561052,-15.3447188656481,
983.222794117647));
#162911=CARTESIAN_POINT('Ctrl Pts',(-10.9229452762603,-14.4643171449067,
981.728676470589));
#162912=CARTESIAN_POINT('Ctrl Pts',(-12.1588589765331,-13.3376329379985,
980.234558823529));
#162913=CARTESIAN_POINT('Ctrl Pts',(-13.3947726768058,-12.2109487310903,
978.740441176471));
#162914=CARTESIAN_POINT('Ctrl Pts',(-14.4026149179538,-10.8763499173728,
977.246323529412));
#162915=CARTESIAN_POINT('Ctrl Pts',(-15.4104571591017,-9.54175110365538,
975.752205882353));
#162916=CARTESIAN_POINT('Ctrl Pts',(-16.1559070823762,-8.04468584505497,
974.258088235294));
#162917=CARTESIAN_POINT('Ctrl Pts',(-16.9013570056506,-6.54762058645456,
972.763970588235));
#162918=CARTESIAN_POINT('Ctrl Pts',(-17.3590292079831,-4.93906964482095,
971.269852941177));
#162919=CARTESIAN_POINT('Ctrl Pts',(-17.8167014103155,-3.33051870318735,
969.775735294118));
#162920=CARTESIAN_POINT('Ctrl Pts',(-17.9710104137728,-1.66525935159368,
968.281617647059));
#162921=CARTESIAN_POINT('Ctrl Pts',(-18.1253194172301,-1.10985572039171E-15,
966.7875));
#162922=CARTESIAN_POINT('Ctrl Pts',(-17.9710104137728,1.66525935159367,
965.293382352941));
#162923=CARTESIAN_POINT('Ctrl Pts',(-17.8167014103155,3.33051870318735,
963.799264705882));
#162924=CARTESIAN_POINT('Ctrl Pts',(-17.3590292079831,4.93906964482096,
962.305147058824));
#162925=CARTESIAN_POINT('Ctrl Pts',(-16.9013570056506,6.54762058645456,
960.811029411765));
#162926=CARTESIAN_POINT('Ctrl Pts',(-16.1559070823762,8.04468584505497,
959.316911764706));
#162927=CARTESIAN_POINT('Ctrl Pts',(-15.4104571591017,9.54175110365538,
957.822794117647));
#162928=CARTESIAN_POINT('Ctrl Pts',(-14.4026149179538,10.8763499173728,
956.328676470588));
#162929=CARTESIAN_POINT('Ctrl Pts',(-13.3947726768058,12.2109487310903,
954.834558823529));
#162930=CARTESIAN_POINT('Ctrl Pts',(-12.1588589765331,13.3376329379985,
953.340441176471));
#162931=CARTESIAN_POINT('Ctrl Pts',(-10.9229452762603,14.4643171449067,
951.846323529412));
#162932=CARTESIAN_POINT('Ctrl Pts',(-9.50104767561052,15.3447188656481,
950.352205882353));
#162933=CARTESIAN_POINT('Ctrl Pts',(-8.07915007496071,16.2251205863895,
948.858088235294));
#162934=CARTESIAN_POINT('Ctrl Pts',(-6.51968959134574,16.8292587962898,
947.363970588235));
#162935=CARTESIAN_POINT('Ctrl Pts',(-4.96022910773078,17.4333970061901,
945.869852941177));
#162936=CARTESIAN_POINT('Ctrl Pts',(-3.31631129755346,17.7406985030951,
944.375735294118));
#162937=CARTESIAN_POINT('Ctrl Pts',(-1.67239348737615,18.048,942.881617647059));
#162938=CARTESIAN_POINT('Ctrl Pts',(-2.21024254310115E-15,18.048,941.3875));
#162939=CARTESIAN_POINT('Ctrl Pts',(1.67239348737616,18.048,939.893382352941));
#162940=CARTESIAN_POINT('Ctrl Pts',(3.31631129755346,17.7406985030951,938.399264705882));
#162941=CARTESIAN_POINT('Ctrl Pts',(4.96022910773077,17.4333970061901,936.905147058824));
#162942=CARTESIAN_POINT('Ctrl Pts',(6.51968959134575,16.8292587962898,935.411029411765));
#162943=CARTESIAN_POINT('Ctrl Pts',(8.07915007496071,16.2251205863895,933.916911764706));
#162944=CARTESIAN_POINT('Ctrl Pts',(9.50104767561053,15.3447188656481,932.422794117647));
#162945=CARTESIAN_POINT('Ctrl Pts',(10.9229452762603,14.4643171449067,930.928676470588));
#162946=CARTESIAN_POINT('Ctrl Pts',(12.1588589765331,13.3376329379985,929.43455882353));
#162947=CARTESIAN_POINT('Ctrl Pts',(13.3947726768058,12.2109487310903,927.940441176471));
#162948=CARTESIAN_POINT('Ctrl Pts',(14.4026149179538,10.8763499173728,926.446323529412));
#162949=CARTESIAN_POINT('Ctrl Pts',(15.4104571591017,9.54175110365539,924.952205882353));
#162950=CARTESIAN_POINT('Ctrl Pts',(16.1559070823762,8.04468584505496,923.458088235294));
#162951=CARTESIAN_POINT('Ctrl Pts',(16.9013570056506,6.54762058645456,921.963970588235));
#162952=CARTESIAN_POINT('Ctrl Pts',(17.3590292079831,4.93906964482096,920.469852941176));
#162953=CARTESIAN_POINT('Ctrl Pts',(17.8167014103155,3.33051870318735,918.975735294118));
#162954=CARTESIAN_POINT('Ctrl Pts',(17.9710104137728,1.66525935159367,917.481617647059));
#162955=CARTESIAN_POINT('Ctrl Pts',(18.1253194172301,3.32956716117513E-15,
915.9875));
#162956=CARTESIAN_POINT('Ctrl Pts',(17.9710104137728,-1.66525935159367,
914.493382352941));
#162957=CARTESIAN_POINT('Ctrl Pts',(17.8167014103155,-3.33051870318736,
912.999264705882));
#162958=CARTESIAN_POINT('Ctrl Pts',(17.3590292079831,-4.93906964482095,
911.505147058824));
#162959=CARTESIAN_POINT('Ctrl Pts',(16.9013570056506,-6.54762058645456,
910.011029411765));
#162960=CARTESIAN_POINT('Ctrl Pts',(16.1559070823762,-8.04468584505497,
908.516911764706));
#162961=CARTESIAN_POINT('Ctrl Pts',(15.4104571591017,-9.54175110365538,
907.022794117647));
#162962=CARTESIAN_POINT('Ctrl Pts',(14.4026149179538,-10.8763499173728,
905.528676470588));
#162963=CARTESIAN_POINT('Ctrl Pts',(13.3947726768058,-12.2109487310903,
904.034558823529));
#162964=CARTESIAN_POINT('Ctrl Pts',(12.1588589765331,-13.3376329379985,
902.540441176471));
#162965=CARTESIAN_POINT('Ctrl Pts',(10.9229452762603,-14.4643171449067,
901.046323529412));
#162966=CARTESIAN_POINT('Ctrl Pts',(9.50104767561053,-15.3447188656481,
899.552205882353));
#162967=CARTESIAN_POINT('Ctrl Pts',(8.07915007496071,-16.2251205863895,
898.058088235294));
#162968=CARTESIAN_POINT('Ctrl Pts',(6.51968959134574,-16.8292587962898,
896.563970588235));
#162969=CARTESIAN_POINT('Ctrl Pts',(4.96022910773078,-17.4333970061901,
895.069852941177));
#162970=CARTESIAN_POINT('Ctrl Pts',(3.31631129755346,-17.7406985030951,
893.575735294118));
#162971=CARTESIAN_POINT('Ctrl Pts',(1.67239348737615,-18.048,892.081617647059));
#162972=CARTESIAN_POINT('Ctrl Pts',(0.,-18.048,890.5875));
#162973=CARTESIAN_POINT('Ctrl Pts',(-1.67239348737615,-18.048,889.093382352941));
#162974=CARTESIAN_POINT('Ctrl Pts',(-3.31631129755346,-17.7406985030951,
887.599264705882));
#162975=CARTESIAN_POINT('Ctrl Pts',(-4.96022910773077,-17.4333970061901,
886.105147058824));
#162976=CARTESIAN_POINT('Ctrl Pts',(-6.51968959134574,-16.8292587962898,
884.611029411765));
#162977=CARTESIAN_POINT('Ctrl Pts',(-8.07915007496071,-16.2251205863895,
883.116911764706));
#162978=CARTESIAN_POINT('Ctrl Pts',(-9.50104767561052,-15.3447188656481,
881.622794117647));
#162979=CARTESIAN_POINT('Ctrl Pts',(-10.9229452762603,-14.4643171449067,
880.128676470588));
#162980=CARTESIAN_POINT('Ctrl Pts',(-12.1588589765331,-13.3376329379985,
878.634558823529));
#162981=CARTESIAN_POINT('Ctrl Pts',(-13.3947726768058,-12.2109487310903,
877.140441176471));
#162982=CARTESIAN_POINT('Ctrl Pts',(-14.4026149179538,-10.8763499173728,
875.646323529412));
#162983=CARTESIAN_POINT('Ctrl Pts',(-15.4104571591017,-9.54175110365538,
874.152205882353));
#162984=CARTESIAN_POINT('Ctrl Pts',(-16.1559070823762,-8.04468584505497,
872.658088235294));
#162985=CARTESIAN_POINT('Ctrl Pts',(-16.9013570056506,-6.54762058645456,
871.163970588236));
#162986=CARTESIAN_POINT('Ctrl Pts',(-17.3590292079831,-4.93906964482095,
869.669852941176));
#162987=CARTESIAN_POINT('Ctrl Pts',(-17.8167014103155,-3.33051870318735,
868.175735294118));
#162988=CARTESIAN_POINT('Ctrl Pts',(-17.9710104137728,-1.66525935159368,
866.681617647059));
#162989=CARTESIAN_POINT('Ctrl Pts',(-18.1253194172301,-1.10985572039171E-15,
865.1875));
#162990=CARTESIAN_POINT('Ctrl Pts',(-17.9710104137728,1.66525935159367,
863.693382352941));
#162991=CARTESIAN_POINT('Ctrl Pts',(-17.8167014103155,3.33051870318735,
862.199264705882));
#162992=CARTESIAN_POINT('Ctrl Pts',(-17.3590292079831,4.93906964482096,
860.705147058824));
#162993=CARTESIAN_POINT('Ctrl Pts',(-16.9013570056506,6.54762058645456,
859.211029411765));
#162994=CARTESIAN_POINT('Ctrl Pts',(-16.1559070823762,8.04468584505497,
857.716911764706));
#162995=CARTESIAN_POINT('Ctrl Pts',(-15.4104571591017,9.54175110365538,
856.222794117647));
#162996=CARTESIAN_POINT('Ctrl Pts',(-14.4026149179538,10.8763499173728,
854.728676470588));
#162997=CARTESIAN_POINT('Ctrl Pts',(-13.3947726768058,12.2109487310903,
853.234558823529));
#162998=CARTESIAN_POINT('Ctrl Pts',(-12.1588589765331,13.3376329379985,
851.740441176471));
#162999=CARTESIAN_POINT('Ctrl Pts',(-10.9229452762603,14.4643171449067,
850.246323529412));
#163000=CARTESIAN_POINT('Ctrl Pts',(-9.50104767561052,15.3447188656481,
848.752205882353));
#163001=CARTESIAN_POINT('Ctrl Pts',(-8.07915007496071,16.2251205863895,
847.258088235294));
#163002=CARTESIAN_POINT('Ctrl Pts',(-6.51968959134574,16.8292587962898,
845.763970588235));
#163003=CARTESIAN_POINT('Ctrl Pts',(-4.96022910773078,17.4333970061901,
844.269852941177));
#163004=CARTESIAN_POINT('Ctrl Pts',(-3.31631129755346,17.7406985030951,
842.775735294118));
#163005=CARTESIAN_POINT('Ctrl Pts',(-1.67239348737615,18.048,841.281617647059));
#163006=CARTESIAN_POINT('Ctrl Pts',(-2.21024254310115E-15,18.048,839.7875));
#163007=CARTESIAN_POINT('Ctrl Pts',(1.67239348737616,18.048,838.293382352941));
#163008=CARTESIAN_POINT('Ctrl Pts',(3.31631129755346,17.7406985030951,836.799264705882));
#163009=CARTESIAN_POINT('Ctrl Pts',(4.96022910773077,17.4333970061901,835.305147058824));
#163010=CARTESIAN_POINT('Ctrl Pts',(6.51968959134575,16.8292587962898,833.811029411765));
#163011=CARTESIAN_POINT('Ctrl Pts',(8.07915007496071,16.2251205863895,832.316911764706));
#163012=CARTESIAN_POINT('Ctrl Pts',(9.50104767561053,15.3447188656481,830.822794117647));
#163013=CARTESIAN_POINT('Ctrl Pts',(10.9229452762603,14.4643171449067,829.328676470588));
#163014=CARTESIAN_POINT('Ctrl Pts',(12.1588589765331,13.3376329379985,827.834558823529));
#163015=CARTESIAN_POINT('Ctrl Pts',(13.3947726768058,12.2109487310903,826.340441176471));
#163016=CARTESIAN_POINT('Ctrl Pts',(14.4026149179538,10.8763499173728,824.846323529412));
#163017=CARTESIAN_POINT('Ctrl Pts',(15.4104571591017,9.54175110365539,823.352205882353));
#163018=CARTESIAN_POINT('Ctrl Pts',(16.1559070823762,8.04468584505496,821.858088235294));
#163019=CARTESIAN_POINT('Ctrl Pts',(16.9013570056506,6.54762058645456,820.363970588235));
#163020=CARTESIAN_POINT('Ctrl Pts',(17.3590292079831,4.93906964482096,818.869852941177));
#163021=CARTESIAN_POINT('Ctrl Pts',(17.8167014103155,3.33051870318735,817.375735294118));
#163022=CARTESIAN_POINT('Ctrl Pts',(17.9710104137728,1.66525935159367,815.881617647059));
#163023=CARTESIAN_POINT('Ctrl Pts',(18.1253194172301,3.32956716117513E-15,
814.3875));
#163024=CARTESIAN_POINT('Ctrl Pts',(17.9710104137728,-1.66525935159367,
812.893382352941));
#163025=CARTESIAN_POINT('Ctrl Pts',(17.8167014103155,-3.33051870318736,
811.399264705883));
#163026=CARTESIAN_POINT('Ctrl Pts',(17.3590292079831,-4.93906964482095,
809.905147058824));
#163027=CARTESIAN_POINT('Ctrl Pts',(16.9013570056506,-6.54762058645456,
808.411029411765));
#163028=CARTESIAN_POINT('Ctrl Pts',(16.1559070823762,-8.04468584505497,
806.916911764706));
#163029=CARTESIAN_POINT('Ctrl Pts',(15.4104571591017,-9.54175110365538,
805.422794117647));
#163030=CARTESIAN_POINT('Ctrl Pts',(14.4026149179538,-10.8763499173728,
803.928676470588));
#163031=CARTESIAN_POINT('Ctrl Pts',(13.3947726768058,-12.2109487310903,
802.434558823529));
#163032=CARTESIAN_POINT('Ctrl Pts',(12.1588589765331,-13.3376329379985,
800.940441176471));
#163033=CARTESIAN_POINT('Ctrl Pts',(10.9229452762603,-14.4643171449067,
799.446323529412));
#163034=CARTESIAN_POINT('Ctrl Pts',(9.50104767561053,-15.3447188656481,
797.952205882353));
#163035=CARTESIAN_POINT('Ctrl Pts',(8.07915007496071,-16.2251205863895,
796.458088235294));
#163036=CARTESIAN_POINT('Ctrl Pts',(6.51968959134574,-16.8292587962898,
794.963970588235));
#163037=CARTESIAN_POINT('Ctrl Pts',(4.96022910773078,-17.4333970061901,
793.469852941176));
#163038=CARTESIAN_POINT('Ctrl Pts',(3.31631129755346,-17.7406985030951,
791.975735294118));
#163039=CARTESIAN_POINT('Ctrl Pts',(1.67239348737615,-18.048,790.481617647059));
#163040=CARTESIAN_POINT('Ctrl Pts',(0.,-18.048,788.9875));
#163041=CARTESIAN_POINT('Ctrl Pts',(-1.67239348737615,-18.048,787.493382352941));
#163042=CARTESIAN_POINT('Ctrl Pts',(-3.31631129755346,-17.7406985030951,
785.999264705882));
#163043=CARTESIAN_POINT('Ctrl Pts',(-4.96022910773077,-17.4333970061901,
784.505147058824));
#163044=CARTESIAN_POINT('Ctrl Pts',(-6.51968959134574,-16.8292587962898,
783.011029411765));
#163045=CARTESIAN_POINT('Ctrl Pts',(-8.07915007496071,-16.2251205863895,
781.516911764706));
#163046=CARTESIAN_POINT('Ctrl Pts',(-9.50104767561052,-15.3447188656481,
780.022794117647));
#163047=CARTESIAN_POINT('Ctrl Pts',(-10.9229452762603,-14.4643171449067,
778.528676470588));
#163048=CARTESIAN_POINT('Ctrl Pts',(-12.1588589765331,-13.3376329379985,
777.03455882353));
#163049=CARTESIAN_POINT('Ctrl Pts',(-13.3947726768058,-12.2109487310903,
775.540441176471));
#163050=CARTESIAN_POINT('Ctrl Pts',(-14.4026149179538,-10.8763499173728,
774.046323529412));
#163051=CARTESIAN_POINT('Ctrl Pts',(-15.4104571591017,-9.54175110365538,
772.552205882353));
#163052=CARTESIAN_POINT('Ctrl Pts',(-16.1559070823762,-8.04468584505497,
771.058088235294));
#163053=CARTESIAN_POINT('Ctrl Pts',(-16.9013570056506,-6.54762058645456,
769.563970588235));
#163054=CARTESIAN_POINT('Ctrl Pts',(-17.3590292079831,-4.93906964482095,
768.069852941177));
#163055=CARTESIAN_POINT('Ctrl Pts',(-17.8167014103155,-3.33051870318735,
766.575735294118));
#163056=CARTESIAN_POINT('Ctrl Pts',(-17.9710104137728,-1.66525935159368,
765.081617647059));
#163057=CARTESIAN_POINT('Ctrl Pts',(-18.1253194172301,-1.10985572039171E-15,
763.5875));
#163058=CARTESIAN_POINT('Ctrl Pts',(-17.9710104137728,1.66525935159367,
762.093382352941));
#163059=CARTESIAN_POINT('Ctrl Pts',(-17.8167014103155,3.33051870318735,
760.599264705883));
#163060=CARTESIAN_POINT('Ctrl Pts',(-17.3590292079831,4.93906964482096,
759.105147058824));
#163061=CARTESIAN_POINT('Ctrl Pts',(-16.9013570056506,6.54762058645456,
757.611029411765));
#163062=CARTESIAN_POINT('Ctrl Pts',(-16.1559070823762,8.04468584505497,
756.116911764706));
#163063=CARTESIAN_POINT('Ctrl Pts',(-15.4104571591017,9.54175110365538,
754.622794117647));
#163064=CARTESIAN_POINT('Ctrl Pts',(-14.4026149179538,10.8763499173728,
753.128676470588));
#163065=CARTESIAN_POINT('Ctrl Pts',(-13.3947726768058,12.2109487310903,
751.634558823529));
#163066=CARTESIAN_POINT('Ctrl Pts',(-12.1588589765331,13.3376329379985,
750.140441176471));
#163067=CARTESIAN_POINT('Ctrl Pts',(-10.9229452762603,14.4643171449067,
748.646323529412));
#163068=CARTESIAN_POINT('Ctrl Pts',(-9.50104767561052,15.3447188656481,
747.152205882353));
#163069=CARTESIAN_POINT('Ctrl Pts',(-8.07915007496071,16.2251205863895,
745.658088235294));
#163070=CARTESIAN_POINT('Ctrl Pts',(-6.51968959134574,16.8292587962898,
744.163970588235));
#163071=CARTESIAN_POINT('Ctrl Pts',(-4.96022910773078,17.4333970061901,
742.669852941176));
#163072=CARTESIAN_POINT('Ctrl Pts',(-3.31631129755346,17.7406985030951,
741.175735294118));
#163073=CARTESIAN_POINT('Ctrl Pts',(-1.67239348737615,18.048,739.681617647059));
#163074=CARTESIAN_POINT('Ctrl Pts',(-2.21024254310115E-15,18.048,738.1875));
#163075=CARTESIAN_POINT('Ctrl Pts',(1.67239348737616,18.048,736.693382352941));
#163076=CARTESIAN_POINT('Ctrl Pts',(3.31631129755346,17.7406985030951,735.199264705882));
#163077=CARTESIAN_POINT('Ctrl Pts',(4.96022910773077,17.4333970061901,733.705147058824));
#163078=CARTESIAN_POINT('Ctrl Pts',(6.51968959134575,16.8292587962898,732.211029411765));
#163079=CARTESIAN_POINT('Ctrl Pts',(8.07915007496071,16.2251205863895,730.716911764706));
#163080=CARTESIAN_POINT('Ctrl Pts',(9.50104767561053,15.3447188656481,729.222794117647));
#163081=CARTESIAN_POINT('Ctrl Pts',(10.9229452762603,14.4643171449067,727.728676470588));
#163082=CARTESIAN_POINT('Ctrl Pts',(12.1588589765331,13.3376329379985,726.234558823529));
#163083=CARTESIAN_POINT('Ctrl Pts',(13.3947726768058,12.2109487310903,724.740441176471));
#163084=CARTESIAN_POINT('Ctrl Pts',(14.4026149179538,10.8763499173728,723.246323529412));
#163085=CARTESIAN_POINT('Ctrl Pts',(15.4104571591017,9.54175110365539,721.752205882353));
#163086=CARTESIAN_POINT('Ctrl Pts',(16.1559070823762,8.04468584505496,720.258088235294));
#163087=CARTESIAN_POINT('Ctrl Pts',(16.9013570056506,6.54762058645456,718.763970588235));
#163088=CARTESIAN_POINT('Ctrl Pts',(17.3590292079831,4.93906964482096,717.269852941177));
#163089=CARTESIAN_POINT('Ctrl Pts',(17.8167014103155,3.33051870318735,715.775735294118));
#163090=CARTESIAN_POINT('Ctrl Pts',(17.9710104137728,1.66525935159367,714.281617647059));
#163091=CARTESIAN_POINT('Ctrl Pts',(18.1253194172301,3.32956716117513E-15,
712.7875));
#163092=CARTESIAN_POINT('Ctrl Pts',(17.9710104137728,-1.66525935159367,
711.293382352941));
#163093=CARTESIAN_POINT('Ctrl Pts',(17.8167014103155,-3.33051870318736,
709.799264705882));
#163094=CARTESIAN_POINT('Ctrl Pts',(17.3590292079831,-4.93906964482095,
708.305147058824));
#163095=CARTESIAN_POINT('Ctrl Pts',(16.9013570056506,-6.54762058645456,
706.811029411765));
#163096=CARTESIAN_POINT('Ctrl Pts',(16.1559070823762,-8.04468584505497,
705.316911764706));
#163097=CARTESIAN_POINT('Ctrl Pts',(15.4104571591017,-9.54175110365538,
703.822794117647));
#163098=CARTESIAN_POINT('Ctrl Pts',(14.4026149179538,-10.8763499173728,
702.328676470588));
#163099=CARTESIAN_POINT('Ctrl Pts',(13.3947726768058,-12.2109487310903,
700.83455882353));
#163100=CARTESIAN_POINT('Ctrl Pts',(12.1588589765331,-13.3376329379985,
699.340441176471));
#163101=CARTESIAN_POINT('Ctrl Pts',(10.9229452762603,-14.4643171449067,
697.846323529412));
#163102=CARTESIAN_POINT('Ctrl Pts',(9.50104767561053,-15.3447188656481,
696.352205882353));
#163103=CARTESIAN_POINT('Ctrl Pts',(8.07915007496071,-16.2251205863895,
694.858088235294));
#163104=CARTESIAN_POINT('Ctrl Pts',(6.51968959134574,-16.8292587962898,
693.363970588235));
#163105=CARTESIAN_POINT('Ctrl Pts',(5.80938874487777,-17.1044308101911,
692.683432004168));
#163106=CARTESIAN_POINT('Ctrl Pts',(5.07842733458062,-17.3187724682607,
692.));
#163107=CARTESIAN_POINT('Ctrl Pts',(0.,-18.048,1500.28886941341));
#163108=CARTESIAN_POINT('Ctrl Pts',(-1.67239348737615,-18.048,1498.79475176635));
#163109=CARTESIAN_POINT('Ctrl Pts',(-3.31631129755346,-17.7406985030951,
1497.30063411929));
#163110=CARTESIAN_POINT('Ctrl Pts',(-4.96022910773077,-17.4333970061901,
1495.80651647223));
#163111=CARTESIAN_POINT('Ctrl Pts',(-6.51968959134574,-16.8292587962898,
1494.31239882517));
#163112=CARTESIAN_POINT('Ctrl Pts',(-8.07915007496071,-16.2251205863895,
1492.81828117811));
#163113=CARTESIAN_POINT('Ctrl Pts',(-9.50104767561052,-15.3447188656481,
1491.32416353106));
#163114=CARTESIAN_POINT('Ctrl Pts',(-10.9229452762603,-14.4643171449067,
1489.830045884));
#163115=CARTESIAN_POINT('Ctrl Pts',(-12.1588589765331,-13.3376329379985,
1488.33592823694));
#163116=CARTESIAN_POINT('Ctrl Pts',(-13.3947726768058,-12.2109487310903,
1486.84181058988));
#163117=CARTESIAN_POINT('Ctrl Pts',(-14.4026149179538,-10.8763499173728,
1485.34769294282));
#163118=CARTESIAN_POINT('Ctrl Pts',(-15.4104571591017,-9.54175110365538,
1483.85357529576));
#163119=CARTESIAN_POINT('Ctrl Pts',(-16.1559070823762,-8.04468584505497,
1482.3594576487));
#163120=CARTESIAN_POINT('Ctrl Pts',(-16.9013570056506,-6.54762058645456,
1480.86534000164));
#163121=CARTESIAN_POINT('Ctrl Pts',(-17.3590292079831,-4.93906964482095,
1479.37122235458));
#163122=CARTESIAN_POINT('Ctrl Pts',(-17.8167014103155,-3.33051870318735,
1477.87710470753));
#163123=CARTESIAN_POINT('Ctrl Pts',(-17.9710104137728,-1.66525935159368,
1476.38298706047));
#163124=CARTESIAN_POINT('Ctrl Pts',(-18.1253194172301,-1.10985572039171E-15,
1474.88886941341));
#163125=CARTESIAN_POINT('Ctrl Pts',(-17.9710104137728,1.66525935159367,
1473.39475176635));
#163126=CARTESIAN_POINT('Ctrl Pts',(-17.8167014103155,3.33051870318735,
1471.90063411929));
#163127=CARTESIAN_POINT('Ctrl Pts',(-17.3590292079831,4.93906964482096,
1470.40651647223));
#163128=CARTESIAN_POINT('Ctrl Pts',(-16.9013570056506,6.54762058645456,
1468.91239882517));
#163129=CARTESIAN_POINT('Ctrl Pts',(-16.1559070823762,8.04468584505497,
1467.41828117811));
#163130=CARTESIAN_POINT('Ctrl Pts',(-15.4104571591017,9.54175110365538,
1465.92416353106));
#163131=CARTESIAN_POINT('Ctrl Pts',(-14.4026149179538,10.8763499173728,
1464.430045884));
#163132=CARTESIAN_POINT('Ctrl Pts',(-13.3947726768058,12.2109487310903,
1462.93592823694));
#163133=CARTESIAN_POINT('Ctrl Pts',(-12.1588589765331,13.3376329379985,
1461.44181058988));
#163134=CARTESIAN_POINT('Ctrl Pts',(-10.9229452762603,14.4643171449067,
1459.94769294282));
#163135=CARTESIAN_POINT('Ctrl Pts',(-9.50104767561052,15.3447188656481,
1458.45357529576));
#163136=CARTESIAN_POINT('Ctrl Pts',(-8.07915007496071,16.2251205863895,
1456.9594576487));
#163137=CARTESIAN_POINT('Ctrl Pts',(-6.51968959134574,16.8292587962898,
1455.46534000164));
#163138=CARTESIAN_POINT('Ctrl Pts',(-4.96022910773078,17.4333970061901,
1453.97122235458));
#163139=CARTESIAN_POINT('Ctrl Pts',(-3.31631129755346,17.7406985030951,
1452.47710470753));
#163140=CARTESIAN_POINT('Ctrl Pts',(-1.67239348737615,18.048,1450.98298706047));
#163141=CARTESIAN_POINT('Ctrl Pts',(-2.21024254310115E-15,18.048,1449.48886941341));
#163142=CARTESIAN_POINT('Ctrl Pts',(1.67239348737616,18.048,1447.99475176635));
#163143=CARTESIAN_POINT('Ctrl Pts',(3.31631129755346,17.7406985030951,1446.50063411929));
#163144=CARTESIAN_POINT('Ctrl Pts',(4.96022910773077,17.4333970061901,1445.00651647223));
#163145=CARTESIAN_POINT('Ctrl Pts',(6.51968959134575,16.8292587962898,1443.51239882517));
#163146=CARTESIAN_POINT('Ctrl Pts',(8.07915007496071,16.2251205863895,1442.01828117811));
#163147=CARTESIAN_POINT('Ctrl Pts',(9.50104767561053,15.3447188656481,1440.52416353105));
#163148=CARTESIAN_POINT('Ctrl Pts',(10.9229452762603,14.4643171449067,1439.030045884));
#163149=CARTESIAN_POINT('Ctrl Pts',(12.1588589765331,13.3376329379985,1437.53592823694));
#163150=CARTESIAN_POINT('Ctrl Pts',(13.3947726768058,12.2109487310903,1436.04181058988));
#163151=CARTESIAN_POINT('Ctrl Pts',(14.4026149179538,10.8763499173728,1434.54769294282));
#163152=CARTESIAN_POINT('Ctrl Pts',(15.4104571591017,9.54175110365538,1433.05357529576));
#163153=CARTESIAN_POINT('Ctrl Pts',(16.1559070823762,8.04468584505496,1431.5594576487));
#163154=CARTESIAN_POINT('Ctrl Pts',(16.9013570056506,6.54762058645456,1430.06534000164));
#163155=CARTESIAN_POINT('Ctrl Pts',(17.3590292079831,4.93906964482096,1428.57122235458));
#163156=CARTESIAN_POINT('Ctrl Pts',(17.8167014103155,3.33051870318735,1427.07710470753));
#163157=CARTESIAN_POINT('Ctrl Pts',(17.9710104137728,1.66525935159367,1425.58298706047));
#163158=CARTESIAN_POINT('Ctrl Pts',(18.1253194172301,3.32956716117513E-15,
1424.08886941341));
#163159=CARTESIAN_POINT('Ctrl Pts',(17.9710104137728,-1.66525935159367,
1422.59475176635));
#163160=CARTESIAN_POINT('Ctrl Pts',(17.8167014103155,-3.33051870318736,
1421.10063411929));
#163161=CARTESIAN_POINT('Ctrl Pts',(17.3590292079831,-4.93906964482095,
1419.60651647223));
#163162=CARTESIAN_POINT('Ctrl Pts',(16.9013570056506,-6.54762058645456,
1418.11239882517));
#163163=CARTESIAN_POINT('Ctrl Pts',(16.1559070823762,-8.04468584505497,
1416.61828117811));
#163164=CARTESIAN_POINT('Ctrl Pts',(15.4104571591017,-9.54175110365538,
1415.12416353105));
#163165=CARTESIAN_POINT('Ctrl Pts',(14.4026149179538,-10.8763499173728,
1413.630045884));
#163166=CARTESIAN_POINT('Ctrl Pts',(13.3947726768058,-12.2109487310903,
1412.13592823694));
#163167=CARTESIAN_POINT('Ctrl Pts',(12.1588589765331,-13.3376329379985,
1410.64181058988));
#163168=CARTESIAN_POINT('Ctrl Pts',(10.9229452762603,-14.4643171449067,
1409.14769294282));
#163169=CARTESIAN_POINT('Ctrl Pts',(9.50104767561053,-15.3447188656481,
1407.65357529576));
#163170=CARTESIAN_POINT('Ctrl Pts',(8.07915007496071,-16.2251205863895,
1406.1594576487));
#163171=CARTESIAN_POINT('Ctrl Pts',(6.51968959134574,-16.8292587962898,
1404.66534000164));
#163172=CARTESIAN_POINT('Ctrl Pts',(4.96022910773078,-17.4333970061901,
1403.17122235458));
#163173=CARTESIAN_POINT('Ctrl Pts',(3.31631129755346,-17.7406985030951,
1401.67710470753));
#163174=CARTESIAN_POINT('Ctrl Pts',(1.67239348737615,-18.048,1400.18298706047));
#163175=CARTESIAN_POINT('Ctrl Pts',(0.,-18.048,1398.68886941341));
#163176=CARTESIAN_POINT('Ctrl Pts',(-1.67239348737615,-18.048,1397.19475176635));
#163177=CARTESIAN_POINT('Ctrl Pts',(-3.31631129755346,-17.7406985030951,
1395.70063411929));
#163178=CARTESIAN_POINT('Ctrl Pts',(-4.96022910773077,-17.4333970061901,
1394.20651647223));
#163179=CARTESIAN_POINT('Ctrl Pts',(-6.51968959134574,-16.8292587962898,
1392.71239882517));
#163180=CARTESIAN_POINT('Ctrl Pts',(-8.07915007496071,-16.2251205863895,
1391.21828117811));
#163181=CARTESIAN_POINT('Ctrl Pts',(-9.50104767561052,-15.3447188656481,
1389.72416353105));
#163182=CARTESIAN_POINT('Ctrl Pts',(-10.9229452762603,-14.4643171449067,
1388.230045884));
#163183=CARTESIAN_POINT('Ctrl Pts',(-12.1588589765331,-13.3376329379985,
1386.73592823694));
#163184=CARTESIAN_POINT('Ctrl Pts',(-13.3947726768058,-12.2109487310903,
1385.24181058988));
#163185=CARTESIAN_POINT('Ctrl Pts',(-14.4026149179538,-10.8763499173728,
1383.74769294282));
#163186=CARTESIAN_POINT('Ctrl Pts',(-15.4104571591017,-9.54175110365538,
1382.25357529576));
#163187=CARTESIAN_POINT('Ctrl Pts',(-16.1559070823762,-8.04468584505497,
1380.7594576487));
#163188=CARTESIAN_POINT('Ctrl Pts',(-16.9013570056506,-6.54762058645456,
1379.26534000164));
#163189=CARTESIAN_POINT('Ctrl Pts',(-17.3590292079831,-4.93906964482095,
1377.77122235458));
#163190=CARTESIAN_POINT('Ctrl Pts',(-17.8167014103155,-3.33051870318735,
1376.27710470753));
#163191=CARTESIAN_POINT('Ctrl Pts',(-17.9710104137728,-1.66525935159368,
1374.78298706047));
#163192=CARTESIAN_POINT('Ctrl Pts',(-18.1253194172301,-1.10985572039171E-15,
1373.28886941341));
#163193=CARTESIAN_POINT('Ctrl Pts',(-17.9710104137728,1.66525935159367,
1371.79475176635));
#163194=CARTESIAN_POINT('Ctrl Pts',(-17.8167014103155,3.33051870318735,
1370.30063411929));
#163195=CARTESIAN_POINT('Ctrl Pts',(-17.3590292079831,4.93906964482096,
1368.80651647223));
#163196=CARTESIAN_POINT('Ctrl Pts',(-16.9013570056506,6.54762058645456,
1367.31239882517));
#163197=CARTESIAN_POINT('Ctrl Pts',(-16.1559070823762,8.04468584505497,
1365.81828117811));
#163198=CARTESIAN_POINT('Ctrl Pts',(-15.4104571591017,9.54175110365538,
1364.32416353105));
#163199=CARTESIAN_POINT('Ctrl Pts',(-14.4026149179538,10.8763499173728,
1362.830045884));
#163200=CARTESIAN_POINT('Ctrl Pts',(-13.3947726768058,12.2109487310903,
1361.33592823694));
#163201=CARTESIAN_POINT('Ctrl Pts',(-12.1588589765331,13.3376329379985,
1359.84181058988));
#163202=CARTESIAN_POINT('Ctrl Pts',(-10.9229452762603,14.4643171449067,
1358.34769294282));
#163203=CARTESIAN_POINT('Ctrl Pts',(-9.50104767561052,15.3447188656481,
1356.85357529576));
#163204=CARTESIAN_POINT('Ctrl Pts',(-8.07915007496071,16.2251205863895,
1355.3594576487));
#163205=CARTESIAN_POINT('Ctrl Pts',(-6.51968959134574,16.8292587962898,
1353.86534000164));
#163206=CARTESIAN_POINT('Ctrl Pts',(-4.96022910773078,17.4333970061901,
1352.37122235458));
#163207=CARTESIAN_POINT('Ctrl Pts',(-3.31631129755346,17.7406985030951,
1350.87710470753));
#163208=CARTESIAN_POINT('Ctrl Pts',(-1.67239348737615,18.048,1349.38298706047));
#163209=CARTESIAN_POINT('Ctrl Pts',(-2.21024254310115E-15,18.048,1347.88886941341));
#163210=CARTESIAN_POINT('Ctrl Pts',(1.67239348737616,18.048,1346.39475176635));
#163211=CARTESIAN_POINT('Ctrl Pts',(3.31631129755346,17.7406985030951,1344.90063411929));
#163212=CARTESIAN_POINT('Ctrl Pts',(4.96022910773077,17.4333970061901,1343.40651647223));
#163213=CARTESIAN_POINT('Ctrl Pts',(6.51968959134575,16.8292587962898,1341.91239882517));
#163214=CARTESIAN_POINT('Ctrl Pts',(8.07915007496071,16.2251205863895,1340.41828117811));
#163215=CARTESIAN_POINT('Ctrl Pts',(9.50104767561053,15.3447188656481,1338.92416353106));
#163216=CARTESIAN_POINT('Ctrl Pts',(10.9229452762603,14.4643171449067,1337.430045884));
#163217=CARTESIAN_POINT('Ctrl Pts',(12.1588589765331,13.3376329379985,1335.93592823694));
#163218=CARTESIAN_POINT('Ctrl Pts',(13.3947726768058,12.2109487310903,1334.44181058988));
#163219=CARTESIAN_POINT('Ctrl Pts',(14.4026149179538,10.8763499173728,1332.94769294282));
#163220=CARTESIAN_POINT('Ctrl Pts',(15.4104571591017,9.54175110365538,1331.45357529576));
#163221=CARTESIAN_POINT('Ctrl Pts',(16.1559070823762,8.04468584505496,1329.9594576487));
#163222=CARTESIAN_POINT('Ctrl Pts',(16.9013570056506,6.54762058645456,1328.46534000164));
#163223=CARTESIAN_POINT('Ctrl Pts',(17.3590292079831,4.93906964482096,1326.97122235458));
#163224=CARTESIAN_POINT('Ctrl Pts',(17.8167014103155,3.33051870318735,1325.47710470753));
#163225=CARTESIAN_POINT('Ctrl Pts',(17.9710104137728,1.66525935159367,1323.98298706047));
#163226=CARTESIAN_POINT('Ctrl Pts',(18.1253194172301,3.32956716117513E-15,
1322.48886941341));
#163227=CARTESIAN_POINT('Ctrl Pts',(17.9710104137728,-1.66525935159367,
1320.99475176635));
#163228=CARTESIAN_POINT('Ctrl Pts',(17.8167014103155,-3.33051870318736,
1319.50063411929));
#163229=CARTESIAN_POINT('Ctrl Pts',(17.3590292079831,-4.93906964482095,
1318.00651647223));
#163230=CARTESIAN_POINT('Ctrl Pts',(16.9013570056506,-6.54762058645456,
1316.51239882517));
#163231=CARTESIAN_POINT('Ctrl Pts',(16.1559070823762,-8.04468584505497,
1315.01828117811));
#163232=CARTESIAN_POINT('Ctrl Pts',(15.4104571591017,-9.54175110365538,
1313.52416353105));
#163233=CARTESIAN_POINT('Ctrl Pts',(14.4026149179538,-10.8763499173728,
1312.030045884));
#163234=CARTESIAN_POINT('Ctrl Pts',(13.3947726768058,-12.2109487310903,
1310.53592823694));
#163235=CARTESIAN_POINT('Ctrl Pts',(12.1588589765331,-13.3376329379985,
1309.04181058988));
#163236=CARTESIAN_POINT('Ctrl Pts',(10.9229452762603,-14.4643171449067,
1307.54769294282));
#163237=CARTESIAN_POINT('Ctrl Pts',(9.50104767561053,-15.3447188656481,
1306.05357529576));
#163238=CARTESIAN_POINT('Ctrl Pts',(8.07915007496071,-16.2251205863895,
1304.5594576487));
#163239=CARTESIAN_POINT('Ctrl Pts',(6.51968959134574,-16.8292587962898,
1303.06534000164));
#163240=CARTESIAN_POINT('Ctrl Pts',(4.96022910773078,-17.4333970061901,
1301.57122235458));
#163241=CARTESIAN_POINT('Ctrl Pts',(3.31631129755346,-17.7406985030951,
1300.07710470753));
#163242=CARTESIAN_POINT('Ctrl Pts',(1.67239348737615,-18.048,1298.58298706047));
#163243=CARTESIAN_POINT('Ctrl Pts',(0.,-18.048,1297.08886941341));
#163244=CARTESIAN_POINT('Ctrl Pts',(-1.67239348737615,-18.048,1295.59475176635));
#163245=CARTESIAN_POINT('Ctrl Pts',(-3.31631129755346,-17.7406985030951,
1294.10063411929));
#163246=CARTESIAN_POINT('Ctrl Pts',(-4.96022910773077,-17.4333970061901,
1292.60651647223));
#163247=CARTESIAN_POINT('Ctrl Pts',(-6.51968959134574,-16.8292587962898,
1291.11239882517));
#163248=CARTESIAN_POINT('Ctrl Pts',(-8.07915007496071,-16.2251205863895,
1289.61828117811));
#163249=CARTESIAN_POINT('Ctrl Pts',(-9.50104767561052,-15.3447188656481,
1288.12416353105));
#163250=CARTESIAN_POINT('Ctrl Pts',(-10.9229452762603,-14.4643171449067,
1286.630045884));
#163251=CARTESIAN_POINT('Ctrl Pts',(-12.1588589765331,-13.3376329379985,
1285.13592823694));
#163252=CARTESIAN_POINT('Ctrl Pts',(-13.3947726768058,-12.2109487310903,
1283.64181058988));
#163253=CARTESIAN_POINT('Ctrl Pts',(-14.4026149179538,-10.8763499173728,
1282.14769294282));
#163254=CARTESIAN_POINT('Ctrl Pts',(-15.4104571591017,-9.54175110365538,
1280.65357529576));
#163255=CARTESIAN_POINT('Ctrl Pts',(-16.1559070823762,-8.04468584505497,
1279.1594576487));
#163256=CARTESIAN_POINT('Ctrl Pts',(-16.9013570056506,-6.54762058645456,
1277.66534000164));
#163257=CARTESIAN_POINT('Ctrl Pts',(-17.3590292079831,-4.93906964482095,
1276.17122235458));
#163258=CARTESIAN_POINT('Ctrl Pts',(-17.8167014103155,-3.33051870318735,
1274.67710470753));
#163259=CARTESIAN_POINT('Ctrl Pts',(-17.9710104137728,-1.66525935159368,
1273.18298706047));
#163260=CARTESIAN_POINT('Ctrl Pts',(-18.1253194172301,-1.10985572039171E-15,
1271.68886941341));
#163261=CARTESIAN_POINT('Ctrl Pts',(-17.9710104137728,1.66525935159367,
1270.19475176635));
#163262=CARTESIAN_POINT('Ctrl Pts',(-17.8167014103155,3.33051870318735,
1268.70063411929));
#163263=CARTESIAN_POINT('Ctrl Pts',(-17.3590292079831,4.93906964482096,
1267.20651647223));
#163264=CARTESIAN_POINT('Ctrl Pts',(-16.9013570056506,6.54762058645456,
1265.71239882517));
#163265=CARTESIAN_POINT('Ctrl Pts',(-16.1559070823762,8.04468584505497,
1264.21828117811));
#163266=CARTESIAN_POINT('Ctrl Pts',(-15.4104571591017,9.54175110365538,
1262.72416353105));
#163267=CARTESIAN_POINT('Ctrl Pts',(-14.4026149179538,10.8763499173728,
1261.230045884));
#163268=CARTESIAN_POINT('Ctrl Pts',(-13.3947726768058,12.2109487310903,
1259.73592823694));
#163269=CARTESIAN_POINT('Ctrl Pts',(-12.1588589765331,13.3376329379985,
1258.24181058988));
#163270=CARTESIAN_POINT('Ctrl Pts',(-10.9229452762603,14.4643171449067,
1256.74769294282));
#163271=CARTESIAN_POINT('Ctrl Pts',(-9.50104767561052,15.3447188656481,
1255.25357529576));
#163272=CARTESIAN_POINT('Ctrl Pts',(-8.07915007496071,16.2251205863895,
1253.7594576487));
#163273=CARTESIAN_POINT('Ctrl Pts',(-6.51968959134574,16.8292587962898,
1252.26534000164));
#163274=CARTESIAN_POINT('Ctrl Pts',(-4.96022910773078,17.4333970061901,
1250.77122235458));
#163275=CARTESIAN_POINT('Ctrl Pts',(-3.31631129755346,17.7406985030951,
1249.27710470753));
#163276=CARTESIAN_POINT('Ctrl Pts',(-1.67239348737615,18.048,1247.78298706047));
#163277=CARTESIAN_POINT('Ctrl Pts',(-2.21024254310115E-15,18.048,1246.28886941341));
#163278=CARTESIAN_POINT('Ctrl Pts',(1.67239348737616,18.048,1244.79475176635));
#163279=CARTESIAN_POINT('Ctrl Pts',(3.31631129755346,17.7406985030951,1243.30063411929));
#163280=CARTESIAN_POINT('Ctrl Pts',(4.96022910773077,17.4333970061901,1241.80651647223));
#163281=CARTESIAN_POINT('Ctrl Pts',(6.51968959134575,16.8292587962898,1240.31239882517));
#163282=CARTESIAN_POINT('Ctrl Pts',(8.07915007496071,16.2251205863895,1238.81828117811));
#163283=CARTESIAN_POINT('Ctrl Pts',(9.50104767561053,15.3447188656481,1237.32416353105));
#163284=CARTESIAN_POINT('Ctrl Pts',(10.9229452762603,14.4643171449067,1235.830045884));
#163285=CARTESIAN_POINT('Ctrl Pts',(12.1588589765331,13.3376329379985,1234.33592823694));
#163286=CARTESIAN_POINT('Ctrl Pts',(13.3947726768058,12.2109487310903,1232.84181058988));
#163287=CARTESIAN_POINT('Ctrl Pts',(14.4026149179538,10.8763499173728,1231.34769294282));
#163288=CARTESIAN_POINT('Ctrl Pts',(15.4104571591017,9.54175110365538,1229.85357529576));
#163289=CARTESIAN_POINT('Ctrl Pts',(16.1559070823762,8.04468584505496,1228.3594576487));
#163290=CARTESIAN_POINT('Ctrl Pts',(16.9013570056506,6.54762058645456,1226.86534000164));
#163291=CARTESIAN_POINT('Ctrl Pts',(17.3590292079831,4.93906964482096,1225.37122235458));
#163292=CARTESIAN_POINT('Ctrl Pts',(17.8167014103155,3.33051870318735,1223.87710470753));
#163293=CARTESIAN_POINT('Ctrl Pts',(17.9710104137728,1.66525935159367,1222.38298706047));
#163294=CARTESIAN_POINT('Ctrl Pts',(18.1253194172301,3.32956716117513E-15,
1220.88886941341));
#163295=CARTESIAN_POINT('Ctrl Pts',(17.9710104137728,-1.66525935159367,
1219.39475176635));
#163296=CARTESIAN_POINT('Ctrl Pts',(17.8167014103155,-3.33051870318736,
1217.90063411929));
#163297=CARTESIAN_POINT('Ctrl Pts',(17.3590292079831,-4.93906964482095,
1216.40651647223));
#163298=CARTESIAN_POINT('Ctrl Pts',(16.9013570056506,-6.54762058645456,
1214.91239882517));
#163299=CARTESIAN_POINT('Ctrl Pts',(16.1559070823762,-8.04468584505497,
1213.41828117811));
#163300=CARTESIAN_POINT('Ctrl Pts',(15.4104571591017,-9.54175110365538,
1211.92416353105));
#163301=CARTESIAN_POINT('Ctrl Pts',(14.4026149179538,-10.8763499173728,
1210.430045884));
#163302=CARTESIAN_POINT('Ctrl Pts',(13.3947726768058,-12.2109487310903,
1208.93592823694));
#163303=CARTESIAN_POINT('Ctrl Pts',(12.1588589765331,-13.3376329379985,
1207.44181058988));
#163304=CARTESIAN_POINT('Ctrl Pts',(10.9229452762603,-14.4643171449067,
1205.94769294282));
#163305=CARTESIAN_POINT('Ctrl Pts',(9.50104767561053,-15.3447188656481,
1204.45357529576));
#163306=CARTESIAN_POINT('Ctrl Pts',(8.07915007496071,-16.2251205863895,
1202.9594576487));
#163307=CARTESIAN_POINT('Ctrl Pts',(6.51968959134574,-16.8292587962898,
1201.46534000164));
#163308=CARTESIAN_POINT('Ctrl Pts',(4.96022910773078,-17.4333970061901,
1199.97122235458));
#163309=CARTESIAN_POINT('Ctrl Pts',(3.31631129755346,-17.7406985030951,
1198.47710470753));
#163310=CARTESIAN_POINT('Ctrl Pts',(1.67239348737615,-18.048,1196.98298706047));
#163311=CARTESIAN_POINT('Ctrl Pts',(0.,-18.048,1195.48886941341));
#163312=CARTESIAN_POINT('Ctrl Pts',(-1.67239348737615,-18.048,1193.99475176635));
#163313=CARTESIAN_POINT('Ctrl Pts',(-3.31631129755346,-17.7406985030951,
1192.50063411929));
#163314=CARTESIAN_POINT('Ctrl Pts',(-4.96022910773077,-17.4333970061901,
1191.00651647223));
#163315=CARTESIAN_POINT('Ctrl Pts',(-6.51968959134574,-16.8292587962898,
1189.51239882517));
#163316=CARTESIAN_POINT('Ctrl Pts',(-8.07915007496071,-16.2251205863895,
1188.01828117811));
#163317=CARTESIAN_POINT('Ctrl Pts',(-9.50104767561052,-15.3447188656481,
1186.52416353105));
#163318=CARTESIAN_POINT('Ctrl Pts',(-10.9229452762603,-14.4643171449067,
1185.030045884));
#163319=CARTESIAN_POINT('Ctrl Pts',(-12.1588589765331,-13.3376329379985,
1183.53592823694));
#163320=CARTESIAN_POINT('Ctrl Pts',(-13.3947726768058,-12.2109487310903,
1182.04181058988));
#163321=CARTESIAN_POINT('Ctrl Pts',(-14.4026149179538,-10.8763499173728,
1180.54769294282));
#163322=CARTESIAN_POINT('Ctrl Pts',(-15.4104571591017,-9.54175110365538,
1179.05357529576));
#163323=CARTESIAN_POINT('Ctrl Pts',(-16.1559070823762,-8.04468584505497,
1177.5594576487));
#163324=CARTESIAN_POINT('Ctrl Pts',(-16.9013570056506,-6.54762058645456,
1176.06534000164));
#163325=CARTESIAN_POINT('Ctrl Pts',(-17.3590292079831,-4.93906964482095,
1174.57122235458));
#163326=CARTESIAN_POINT('Ctrl Pts',(-17.8167014103155,-3.33051870318735,
1173.07710470753));
#163327=CARTESIAN_POINT('Ctrl Pts',(-17.9710104137728,-1.66525935159368,
1171.58298706047));
#163328=CARTESIAN_POINT('Ctrl Pts',(-18.1253194172301,-1.10985572039171E-15,
1170.08886941341));
#163329=CARTESIAN_POINT('Ctrl Pts',(-17.9710104137728,1.66525935159367,
1168.59475176635));
#163330=CARTESIAN_POINT('Ctrl Pts',(-17.8167014103155,3.33051870318735,
1167.10063411929));
#163331=CARTESIAN_POINT('Ctrl Pts',(-17.3590292079831,4.93906964482096,
1165.60651647223));
#163332=CARTESIAN_POINT('Ctrl Pts',(-16.9013570056506,6.54762058645456,
1164.11239882517));
#163333=CARTESIAN_POINT('Ctrl Pts',(-16.1559070823762,8.04468584505497,
1162.61828117811));
#163334=CARTESIAN_POINT('Ctrl Pts',(-15.4104571591017,9.54175110365538,
1161.12416353106));
#163335=CARTESIAN_POINT('Ctrl Pts',(-14.4026149179538,10.8763499173728,
1159.630045884));
#163336=CARTESIAN_POINT('Ctrl Pts',(-13.3947726768058,12.2109487310903,
1158.13592823694));
#163337=CARTESIAN_POINT('Ctrl Pts',(-12.1588589765331,13.3376329379985,
1156.64181058988));
#163338=CARTESIAN_POINT('Ctrl Pts',(-10.9229452762603,14.4643171449067,
1155.14769294282));
#163339=CARTESIAN_POINT('Ctrl Pts',(-9.50104767561052,15.3447188656481,
1153.65357529576));
#163340=CARTESIAN_POINT('Ctrl Pts',(-8.07915007496071,16.2251205863895,
1152.1594576487));
#163341=CARTESIAN_POINT('Ctrl Pts',(-6.51968959134574,16.8292587962898,
1150.66534000164));
#163342=CARTESIAN_POINT('Ctrl Pts',(-4.96022910773078,17.4333970061901,
1149.17122235458));
#163343=CARTESIAN_POINT('Ctrl Pts',(-3.31631129755346,17.7406985030951,
1147.67710470753));
#163344=CARTESIAN_POINT('Ctrl Pts',(-1.67239348737615,18.048,1146.18298706047));
#163345=CARTESIAN_POINT('Ctrl Pts',(-2.21024254310115E-15,18.048,1144.68886941341));
#163346=CARTESIAN_POINT('Ctrl Pts',(1.67239348737616,18.048,1143.19475176635));
#163347=CARTESIAN_POINT('Ctrl Pts',(3.31631129755346,17.7406985030951,1141.70063411929));
#163348=CARTESIAN_POINT('Ctrl Pts',(4.96022910773077,17.4333970061901,1140.20651647223));
#163349=CARTESIAN_POINT('Ctrl Pts',(6.51968959134575,16.8292587962898,1138.71239882517));
#163350=CARTESIAN_POINT('Ctrl Pts',(8.07915007496071,16.2251205863895,1137.21828117811));
#163351=CARTESIAN_POINT('Ctrl Pts',(9.50104767561053,15.3447188656481,1135.72416353105));
#163352=CARTESIAN_POINT('Ctrl Pts',(10.9229452762603,14.4643171449067,1134.230045884));
#163353=CARTESIAN_POINT('Ctrl Pts',(12.1588589765331,13.3376329379985,1132.73592823694));
#163354=CARTESIAN_POINT('Ctrl Pts',(13.3947726768058,12.2109487310903,1131.24181058988));
#163355=CARTESIAN_POINT('Ctrl Pts',(14.4026149179538,10.8763499173728,1129.74769294282));
#163356=CARTESIAN_POINT('Ctrl Pts',(15.4104571591017,9.54175110365538,1128.25357529576));
#163357=CARTESIAN_POINT('Ctrl Pts',(16.1559070823762,8.04468584505496,1126.7594576487));
#163358=CARTESIAN_POINT('Ctrl Pts',(16.9013570056506,6.54762058645456,1125.26534000164));
#163359=CARTESIAN_POINT('Ctrl Pts',(17.3590292079831,4.93906964482096,1123.77122235458));
#163360=CARTESIAN_POINT('Ctrl Pts',(17.8167014103155,3.33051870318735,1122.27710470753));
#163361=CARTESIAN_POINT('Ctrl Pts',(17.9710104137728,1.66525935159367,1120.78298706047));
#163362=CARTESIAN_POINT('Ctrl Pts',(18.1253194172301,3.32956716117513E-15,
1119.28886941341));
#163363=CARTESIAN_POINT('Ctrl Pts',(17.9710104137728,-1.66525935159367,
1117.79475176635));
#163364=CARTESIAN_POINT('Ctrl Pts',(17.8167014103155,-3.33051870318736,
1116.30063411929));
#163365=CARTESIAN_POINT('Ctrl Pts',(17.3590292079831,-4.93906964482095,
1114.80651647223));
#163366=CARTESIAN_POINT('Ctrl Pts',(16.9013570056506,-6.54762058645456,
1113.31239882517));
#163367=CARTESIAN_POINT('Ctrl Pts',(16.1559070823762,-8.04468584505497,
1111.81828117811));
#163368=CARTESIAN_POINT('Ctrl Pts',(15.4104571591017,-9.54175110365538,
1110.32416353105));
#163369=CARTESIAN_POINT('Ctrl Pts',(14.4026149179538,-10.8763499173728,
1108.830045884));
#163370=CARTESIAN_POINT('Ctrl Pts',(13.3947726768058,-12.2109487310903,
1107.33592823694));
#163371=CARTESIAN_POINT('Ctrl Pts',(12.1588589765331,-13.3376329379985,
1105.84181058988));
#163372=CARTESIAN_POINT('Ctrl Pts',(10.9229452762603,-14.4643171449067,
1104.34769294282));
#163373=CARTESIAN_POINT('Ctrl Pts',(9.50104767561053,-15.3447188656481,
1102.85357529576));
#163374=CARTESIAN_POINT('Ctrl Pts',(8.07915007496071,-16.2251205863895,
1101.3594576487));
#163375=CARTESIAN_POINT('Ctrl Pts',(6.51968959134574,-16.8292587962898,
1099.86534000164));
#163376=CARTESIAN_POINT('Ctrl Pts',(4.96022910773078,-17.4333970061901,
1098.37122235458));
#163377=CARTESIAN_POINT('Ctrl Pts',(3.31631129755346,-17.7406985030951,
1096.87710470753));
#163378=CARTESIAN_POINT('Ctrl Pts',(1.67239348737615,-18.048,1095.38298706047));
#163379=CARTESIAN_POINT('Ctrl Pts',(0.,-18.048,1093.88886941341));
#163380=CARTESIAN_POINT('Ctrl Pts',(-1.67239348737615,-18.048,1092.39475176635));
#163381=CARTESIAN_POINT('Ctrl Pts',(-3.31631129755346,-17.7406985030951,
1090.90063411929));
#163382=CARTESIAN_POINT('Ctrl Pts',(-4.96022910773077,-17.4333970061901,
1089.40651647223));
#163383=CARTESIAN_POINT('Ctrl Pts',(-6.51968959134574,-16.8292587962898,
1087.91239882517));
#163384=CARTESIAN_POINT('Ctrl Pts',(-8.07915007496071,-16.2251205863895,
1086.41828117811));
#163385=CARTESIAN_POINT('Ctrl Pts',(-9.50104767561052,-15.3447188656481,
1084.92416353106));
#163386=CARTESIAN_POINT('Ctrl Pts',(-10.9229452762603,-14.4643171449067,
1083.430045884));
#163387=CARTESIAN_POINT('Ctrl Pts',(-12.1588589765331,-13.3376329379985,
1081.93592823694));
#163388=CARTESIAN_POINT('Ctrl Pts',(-13.3947726768058,-12.2109487310903,
1080.44181058988));
#163389=CARTESIAN_POINT('Ctrl Pts',(-14.4026149179538,-10.8763499173728,
1078.94769294282));
#163390=CARTESIAN_POINT('Ctrl Pts',(-15.4104571591017,-9.54175110365538,
1077.45357529576));
#163391=CARTESIAN_POINT('Ctrl Pts',(-16.1559070823762,-8.04468584505497,
1075.9594576487));
#163392=CARTESIAN_POINT('Ctrl Pts',(-16.9013570056506,-6.54762058645456,
1074.46534000164));
#163393=CARTESIAN_POINT('Ctrl Pts',(-17.3590292079831,-4.93906964482095,
1072.97122235458));
#163394=CARTESIAN_POINT('Ctrl Pts',(-17.8167014103155,-3.33051870318735,
1071.47710470753));
#163395=CARTESIAN_POINT('Ctrl Pts',(-17.9710104137728,-1.66525935159368,
1069.98298706047));
#163396=CARTESIAN_POINT('Ctrl Pts',(-18.1253194172301,-1.10985572039171E-15,
1068.48886941341));
#163397=CARTESIAN_POINT('Ctrl Pts',(-17.9710104137728,1.66525935159367,
1066.99475176635));
#163398=CARTESIAN_POINT('Ctrl Pts',(-17.8167014103155,3.33051870318735,
1065.50063411929));
#163399=CARTESIAN_POINT('Ctrl Pts',(-17.3590292079831,4.93906964482096,
1064.00651647223));
#163400=CARTESIAN_POINT('Ctrl Pts',(-16.9013570056506,6.54762058645456,
1062.51239882517));
#163401=CARTESIAN_POINT('Ctrl Pts',(-16.1559070823762,8.04468584505497,
1061.01828117811));
#163402=CARTESIAN_POINT('Ctrl Pts',(-15.4104571591017,9.54175110365538,
1059.52416353105));
#163403=CARTESIAN_POINT('Ctrl Pts',(-14.4026149179538,10.8763499173728,
1058.030045884));
#163404=CARTESIAN_POINT('Ctrl Pts',(-13.3947726768058,12.2109487310903,
1056.53592823694));
#163405=CARTESIAN_POINT('Ctrl Pts',(-12.1588589765331,13.3376329379985,
1055.04181058988));
#163406=CARTESIAN_POINT('Ctrl Pts',(-10.9229452762603,14.4643171449067,
1053.54769294282));
#163407=CARTESIAN_POINT('Ctrl Pts',(-9.50104767561052,15.3447188656481,
1052.05357529576));
#163408=CARTESIAN_POINT('Ctrl Pts',(-8.07915007496071,16.2251205863895,
1050.5594576487));
#163409=CARTESIAN_POINT('Ctrl Pts',(-6.51968959134574,16.8292587962898,
1049.06534000164));
#163410=CARTESIAN_POINT('Ctrl Pts',(-4.96022910773078,17.4333970061901,
1047.57122235458));
#163411=CARTESIAN_POINT('Ctrl Pts',(-3.31631129755346,17.7406985030951,
1046.07710470753));
#163412=CARTESIAN_POINT('Ctrl Pts',(-1.67239348737615,18.048,1044.58298706047));
#163413=CARTESIAN_POINT('Ctrl Pts',(-2.21024254310115E-15,18.048,1043.08886941341));
#163414=CARTESIAN_POINT('Ctrl Pts',(1.67239348737616,18.048,1041.59475176635));
#163415=CARTESIAN_POINT('Ctrl Pts',(3.31631129755346,17.7406985030951,1040.10063411929));
#163416=CARTESIAN_POINT('Ctrl Pts',(4.96022910773077,17.4333970061901,1038.60651647223));
#163417=CARTESIAN_POINT('Ctrl Pts',(6.51968959134575,16.8292587962898,1037.11239882517));
#163418=CARTESIAN_POINT('Ctrl Pts',(8.07915007496071,16.2251205863895,1035.61828117811));
#163419=CARTESIAN_POINT('Ctrl Pts',(9.50104767561053,15.3447188656481,1034.12416353105));
#163420=CARTESIAN_POINT('Ctrl Pts',(10.9229452762603,14.4643171449067,1032.630045884));
#163421=CARTESIAN_POINT('Ctrl Pts',(12.1588589765331,13.3376329379985,1031.13592823694));
#163422=CARTESIAN_POINT('Ctrl Pts',(13.3947726768058,12.2109487310903,1029.64181058988));
#163423=CARTESIAN_POINT('Ctrl Pts',(14.4026149179538,10.8763499173728,1028.14769294282));
#163424=CARTESIAN_POINT('Ctrl Pts',(15.4104571591017,9.54175110365538,1026.65357529576));
#163425=CARTESIAN_POINT('Ctrl Pts',(16.1559070823762,8.04468584505496,1025.1594576487));
#163426=CARTESIAN_POINT('Ctrl Pts',(16.9013570056506,6.54762058645456,1023.66534000164));
#163427=CARTESIAN_POINT('Ctrl Pts',(17.3590292079831,4.93906964482096,1022.17122235458));
#163428=CARTESIAN_POINT('Ctrl Pts',(17.8167014103155,3.33051870318735,1020.67710470753));
#163429=CARTESIAN_POINT('Ctrl Pts',(17.9710104137728,1.66525935159367,1019.18298706047));
#163430=CARTESIAN_POINT('Ctrl Pts',(18.1253194172301,3.32956716117513E-15,
1017.68886941341));
#163431=CARTESIAN_POINT('Ctrl Pts',(17.9710104137728,-1.66525935159367,
1016.19475176635));
#163432=CARTESIAN_POINT('Ctrl Pts',(17.8167014103155,-3.33051870318736,
1014.70063411929));
#163433=CARTESIAN_POINT('Ctrl Pts',(17.3590292079831,-4.93906964482095,
1013.20651647223));
#163434=CARTESIAN_POINT('Ctrl Pts',(16.9013570056506,-6.54762058645456,
1011.71239882517));
#163435=CARTESIAN_POINT('Ctrl Pts',(16.1559070823762,-8.04468584505497,
1010.21828117811));
#163436=CARTESIAN_POINT('Ctrl Pts',(15.4104571591017,-9.54175110365538,
1008.72416353105));
#163437=CARTESIAN_POINT('Ctrl Pts',(14.4026149179538,-10.8763499173728,
1007.230045884));
#163438=CARTESIAN_POINT('Ctrl Pts',(13.3947726768058,-12.2109487310903,
1005.73592823694));
#163439=CARTESIAN_POINT('Ctrl Pts',(12.1588589765331,-13.3376329379985,
1004.24181058988));
#163440=CARTESIAN_POINT('Ctrl Pts',(10.9229452762603,-14.4643171449067,
1002.74769294282));
#163441=CARTESIAN_POINT('Ctrl Pts',(9.50104767561053,-15.3447188656481,
1001.25357529576));
#163442=CARTESIAN_POINT('Ctrl Pts',(8.07915007496071,-16.2251205863895,
999.759457648702));
#163443=CARTESIAN_POINT('Ctrl Pts',(6.51968959134574,-16.8292587962898,
998.265340001643));
#163444=CARTESIAN_POINT('Ctrl Pts',(4.96022910773078,-17.4333970061901,
996.771222354585));
#163445=CARTESIAN_POINT('Ctrl Pts',(3.31631129755346,-17.7406985030951,
995.277104707525));
#163446=CARTESIAN_POINT('Ctrl Pts',(1.67239348737615,-18.048,993.782987060467));
#163447=CARTESIAN_POINT('Ctrl Pts',(0.,-18.048,992.288869413408));
#163448=CARTESIAN_POINT('Ctrl Pts',(-1.67239348737615,-18.048,990.794751766349));
#163449=CARTESIAN_POINT('Ctrl Pts',(-3.31631129755346,-17.7406985030951,
989.30063411929));
#163450=CARTESIAN_POINT('Ctrl Pts',(-4.96022910773077,-17.4333970061901,
987.806516472232));
#163451=CARTESIAN_POINT('Ctrl Pts',(-6.51968959134574,-16.8292587962898,
986.312398825173));
#163452=CARTESIAN_POINT('Ctrl Pts',(-8.07915007496071,-16.2251205863895,
984.818281178114));
#163453=CARTESIAN_POINT('Ctrl Pts',(-9.50104767561052,-15.3447188656481,
983.324163531055));
#163454=CARTESIAN_POINT('Ctrl Pts',(-10.9229452762603,-14.4643171449067,
981.830045883996));
#163455=CARTESIAN_POINT('Ctrl Pts',(-12.1588589765331,-13.3376329379985,
980.335928236937));
#163456=CARTESIAN_POINT('Ctrl Pts',(-13.3947726768058,-12.2109487310903,
978.841810589878));
#163457=CARTESIAN_POINT('Ctrl Pts',(-14.4026149179538,-10.8763499173728,
977.34769294282));
#163458=CARTESIAN_POINT('Ctrl Pts',(-15.4104571591017,-9.54175110365538,
975.853575295761));
#163459=CARTESIAN_POINT('Ctrl Pts',(-16.1559070823762,-8.04468584505497,
974.359457648702));
#163460=CARTESIAN_POINT('Ctrl Pts',(-16.9013570056506,-6.54762058645456,
972.865340001643));
#163461=CARTESIAN_POINT('Ctrl Pts',(-17.3590292079831,-4.93906964482095,
971.371222354584));
#163462=CARTESIAN_POINT('Ctrl Pts',(-17.8167014103155,-3.33051870318735,
969.877104707525));
#163463=CARTESIAN_POINT('Ctrl Pts',(-17.9710104137728,-1.66525935159368,
968.382987060467));
#163464=CARTESIAN_POINT('Ctrl Pts',(-18.1253194172301,-1.10985572039171E-15,
966.888869413408));
#163465=CARTESIAN_POINT('Ctrl Pts',(-17.9710104137728,1.66525935159367,
965.394751766349));
#163466=CARTESIAN_POINT('Ctrl Pts',(-17.8167014103155,3.33051870318735,
963.90063411929));
#163467=CARTESIAN_POINT('Ctrl Pts',(-17.3590292079831,4.93906964482096,
962.406516472231));
#163468=CARTESIAN_POINT('Ctrl Pts',(-16.9013570056506,6.54762058645456,
960.912398825173));
#163469=CARTESIAN_POINT('Ctrl Pts',(-16.1559070823762,8.04468584505497,
959.418281178114));
#163470=CARTESIAN_POINT('Ctrl Pts',(-15.4104571591017,9.54175110365538,
957.924163531055));
#163471=CARTESIAN_POINT('Ctrl Pts',(-14.4026149179538,10.8763499173728,
956.430045883996));
#163472=CARTESIAN_POINT('Ctrl Pts',(-13.3947726768058,12.2109487310903,
954.935928236937));
#163473=CARTESIAN_POINT('Ctrl Pts',(-12.1588589765331,13.3376329379985,
953.441810589878));
#163474=CARTESIAN_POINT('Ctrl Pts',(-10.9229452762603,14.4643171449067,
951.94769294282));
#163475=CARTESIAN_POINT('Ctrl Pts',(-9.50104767561052,15.3447188656481,
950.453575295761));
#163476=CARTESIAN_POINT('Ctrl Pts',(-8.07915007496071,16.2251205863895,
948.959457648702));
#163477=CARTESIAN_POINT('Ctrl Pts',(-6.51968959134574,16.8292587962898,
947.465340001643));
#163478=CARTESIAN_POINT('Ctrl Pts',(-4.96022910773078,17.4333970061901,
945.971222354585));
#163479=CARTESIAN_POINT('Ctrl Pts',(-3.31631129755346,17.7406985030951,
944.477104707526));
#163480=CARTESIAN_POINT('Ctrl Pts',(-1.67239348737615,18.048,942.982987060467));
#163481=CARTESIAN_POINT('Ctrl Pts',(-2.21024254310115E-15,18.048,941.488869413408));
#163482=CARTESIAN_POINT('Ctrl Pts',(1.67239348737616,18.048,939.994751766349));
#163483=CARTESIAN_POINT('Ctrl Pts',(3.31631129755346,17.7406985030951,938.50063411929));
#163484=CARTESIAN_POINT('Ctrl Pts',(4.96022910773077,17.4333970061901,937.006516472232));
#163485=CARTESIAN_POINT('Ctrl Pts',(6.51968959134575,16.8292587962898,935.512398825173));
#163486=CARTESIAN_POINT('Ctrl Pts',(8.07915007496071,16.2251205863895,934.018281178114));
#163487=CARTESIAN_POINT('Ctrl Pts',(9.50104767561053,15.3447188656481,932.524163531055));
#163488=CARTESIAN_POINT('Ctrl Pts',(10.9229452762603,14.4643171449067,931.030045883996));
#163489=CARTESIAN_POINT('Ctrl Pts',(12.1588589765331,13.3376329379985,929.535928236937));
#163490=CARTESIAN_POINT('Ctrl Pts',(13.3947726768058,12.2109487310903,928.041810589879));
#163491=CARTESIAN_POINT('Ctrl Pts',(14.4026149179538,10.8763499173728,926.54769294282));
#163492=CARTESIAN_POINT('Ctrl Pts',(15.4104571591017,9.54175110365538,925.053575295761));
#163493=CARTESIAN_POINT('Ctrl Pts',(16.1559070823762,8.04468584505496,923.559457648702));
#163494=CARTESIAN_POINT('Ctrl Pts',(16.9013570056506,6.54762058645456,922.065340001643));
#163495=CARTESIAN_POINT('Ctrl Pts',(17.3590292079831,4.93906964482096,920.571222354584));
#163496=CARTESIAN_POINT('Ctrl Pts',(17.8167014103155,3.33051870318735,919.077104707525));
#163497=CARTESIAN_POINT('Ctrl Pts',(17.9710104137728,1.66525935159367,917.582987060467));
#163498=CARTESIAN_POINT('Ctrl Pts',(18.1253194172301,3.32956716117513E-15,
916.088869413408));
#163499=CARTESIAN_POINT('Ctrl Pts',(17.9710104137728,-1.66525935159367,
914.594751766349));
#163500=CARTESIAN_POINT('Ctrl Pts',(17.8167014103155,-3.33051870318736,
913.10063411929));
#163501=CARTESIAN_POINT('Ctrl Pts',(17.3590292079831,-4.93906964482095,
911.606516472231));
#163502=CARTESIAN_POINT('Ctrl Pts',(16.9013570056506,-6.54762058645456,
910.112398825173));
#163503=CARTESIAN_POINT('Ctrl Pts',(16.1559070823762,-8.04468584505497,
908.618281178114));
#163504=CARTESIAN_POINT('Ctrl Pts',(15.4104571591017,-9.54175110365538,
907.124163531055));
#163505=CARTESIAN_POINT('Ctrl Pts',(14.4026149179538,-10.8763499173728,
905.630045883996));
#163506=CARTESIAN_POINT('Ctrl Pts',(13.3947726768058,-12.2109487310903,
904.135928236937));
#163507=CARTESIAN_POINT('Ctrl Pts',(12.1588589765331,-13.3376329379985,
902.641810589878));
#163508=CARTESIAN_POINT('Ctrl Pts',(10.9229452762603,-14.4643171449067,
901.14769294282));
#163509=CARTESIAN_POINT('Ctrl Pts',(9.50104767561053,-15.3447188656481,
899.653575295761));
#163510=CARTESIAN_POINT('Ctrl Pts',(8.07915007496071,-16.2251205863895,
898.159457648702));
#163511=CARTESIAN_POINT('Ctrl Pts',(6.51968959134574,-16.8292587962898,
896.665340001643));
#163512=CARTESIAN_POINT('Ctrl Pts',(4.96022910773078,-17.4333970061901,
895.171222354584));
#163513=CARTESIAN_POINT('Ctrl Pts',(3.31631129755346,-17.7406985030951,
893.677104707526));
#163514=CARTESIAN_POINT('Ctrl Pts',(1.67239348737615,-18.048,892.182987060467));
#163515=CARTESIAN_POINT('Ctrl Pts',(0.,-18.048,890.688869413408));
#163516=CARTESIAN_POINT('Ctrl Pts',(-1.67239348737615,-18.048,889.194751766349));
#163517=CARTESIAN_POINT('Ctrl Pts',(-3.31631129755346,-17.7406985030951,
887.70063411929));
#163518=CARTESIAN_POINT('Ctrl Pts',(-4.96022910773077,-17.4333970061901,
886.206516472232));
#163519=CARTESIAN_POINT('Ctrl Pts',(-6.51968959134574,-16.8292587962898,
884.712398825172));
#163520=CARTESIAN_POINT('Ctrl Pts',(-8.07915007496071,-16.2251205863895,
883.218281178114));
#163521=CARTESIAN_POINT('Ctrl Pts',(-9.50104767561052,-15.3447188656481,
881.724163531055));
#163522=CARTESIAN_POINT('Ctrl Pts',(-10.9229452762603,-14.4643171449067,
880.230045883996));
#163523=CARTESIAN_POINT('Ctrl Pts',(-12.1588589765331,-13.3376329379985,
878.735928236937));
#163524=CARTESIAN_POINT('Ctrl Pts',(-13.3947726768058,-12.2109487310903,
877.241810589879));
#163525=CARTESIAN_POINT('Ctrl Pts',(-14.4026149179538,-10.8763499173728,
875.74769294282));
#163526=CARTESIAN_POINT('Ctrl Pts',(-15.4104571591017,-9.54175110365538,
874.253575295761));
#163527=CARTESIAN_POINT('Ctrl Pts',(-16.1559070823762,-8.04468584505497,
872.759457648702));
#163528=CARTESIAN_POINT('Ctrl Pts',(-16.9013570056506,-6.54762058645456,
871.265340001643));
#163529=CARTESIAN_POINT('Ctrl Pts',(-17.3590292079831,-4.93906964482095,
869.771222354584));
#163530=CARTESIAN_POINT('Ctrl Pts',(-17.8167014103155,-3.33051870318735,
868.277104707525));
#163531=CARTESIAN_POINT('Ctrl Pts',(-17.9710104137728,-1.66525935159368,
866.782987060467));
#163532=CARTESIAN_POINT('Ctrl Pts',(-18.1253194172301,-1.10985572039171E-15,
865.288869413408));
#163533=CARTESIAN_POINT('Ctrl Pts',(-17.9710104137728,1.66525935159367,
863.794751766349));
#163534=CARTESIAN_POINT('Ctrl Pts',(-17.8167014103155,3.33051870318735,
862.30063411929));
#163535=CARTESIAN_POINT('Ctrl Pts',(-17.3590292079831,4.93906964482096,
860.806516472231));
#163536=CARTESIAN_POINT('Ctrl Pts',(-16.9013570056506,6.54762058645456,
859.312398825173));
#163537=CARTESIAN_POINT('Ctrl Pts',(-16.1559070823762,8.04468584505497,
857.818281178114));
#163538=CARTESIAN_POINT('Ctrl Pts',(-15.4104571591017,9.54175110365538,
856.324163531055));
#163539=CARTESIAN_POINT('Ctrl Pts',(-14.4026149179538,10.8763499173728,
854.830045883996));
#163540=CARTESIAN_POINT('Ctrl Pts',(-13.3947726768058,12.2109487310903,
853.335928236937));
#163541=CARTESIAN_POINT('Ctrl Pts',(-12.1588589765331,13.3376329379985,
851.841810589878));
#163542=CARTESIAN_POINT('Ctrl Pts',(-10.9229452762603,14.4643171449067,
850.34769294282));
#163543=CARTESIAN_POINT('Ctrl Pts',(-9.50104767561052,15.3447188656481,
848.853575295761));
#163544=CARTESIAN_POINT('Ctrl Pts',(-8.07915007496071,16.2251205863895,
847.359457648702));
#163545=CARTESIAN_POINT('Ctrl Pts',(-6.51968959134574,16.8292587962898,
845.865340001643));
#163546=CARTESIAN_POINT('Ctrl Pts',(-4.96022910773078,17.4333970061901,
844.371222354584));
#163547=CARTESIAN_POINT('Ctrl Pts',(-3.31631129755346,17.7406985030951,
842.877104707525));
#163548=CARTESIAN_POINT('Ctrl Pts',(-1.67239348737615,18.048,841.382987060467));
#163549=CARTESIAN_POINT('Ctrl Pts',(-2.21024254310115E-15,18.048,839.888869413408));
#163550=CARTESIAN_POINT('Ctrl Pts',(1.67239348737616,18.048,838.394751766349));
#163551=CARTESIAN_POINT('Ctrl Pts',(3.31631129755346,17.7406985030951,836.90063411929));
#163552=CARTESIAN_POINT('Ctrl Pts',(4.96022910773077,17.4333970061901,835.406516472232));
#163553=CARTESIAN_POINT('Ctrl Pts',(6.51968959134575,16.8292587962898,833.912398825173));
#163554=CARTESIAN_POINT('Ctrl Pts',(8.07915007496071,16.2251205863895,832.418281178114));
#163555=CARTESIAN_POINT('Ctrl Pts',(9.50104767561053,15.3447188656481,830.924163531055));
#163556=CARTESIAN_POINT('Ctrl Pts',(10.9229452762603,14.4643171449067,829.430045883996));
#163557=CARTESIAN_POINT('Ctrl Pts',(12.1588589765331,13.3376329379985,827.935928236937));
#163558=CARTESIAN_POINT('Ctrl Pts',(13.3947726768058,12.2109487310903,826.441810589879));
#163559=CARTESIAN_POINT('Ctrl Pts',(14.4026149179538,10.8763499173728,824.94769294282));
#163560=CARTESIAN_POINT('Ctrl Pts',(15.4104571591017,9.54175110365538,823.453575295761));
#163561=CARTESIAN_POINT('Ctrl Pts',(16.1559070823762,8.04468584505496,821.959457648702));
#163562=CARTESIAN_POINT('Ctrl Pts',(16.9013570056506,6.54762058645456,820.465340001643));
#163563=CARTESIAN_POINT('Ctrl Pts',(17.3590292079831,4.93906964482096,818.971222354584));
#163564=CARTESIAN_POINT('Ctrl Pts',(17.8167014103155,3.33051870318735,817.477104707526));
#163565=CARTESIAN_POINT('Ctrl Pts',(17.9710104137728,1.66525935159367,815.982987060467));
#163566=CARTESIAN_POINT('Ctrl Pts',(18.1253194172301,3.32956716117513E-15,
814.488869413408));
#163567=CARTESIAN_POINT('Ctrl Pts',(17.9710104137728,-1.66525935159367,
812.994751766349));
#163568=CARTESIAN_POINT('Ctrl Pts',(17.8167014103155,-3.33051870318736,
811.50063411929));
#163569=CARTESIAN_POINT('Ctrl Pts',(17.3590292079831,-4.93906964482095,
810.006516472231));
#163570=CARTESIAN_POINT('Ctrl Pts',(16.9013570056506,-6.54762058645456,
808.512398825172));
#163571=CARTESIAN_POINT('Ctrl Pts',(16.1559070823762,-8.04468584505497,
807.018281178114));
#163572=CARTESIAN_POINT('Ctrl Pts',(15.4104571591017,-9.54175110365538,
805.524163531055));
#163573=CARTESIAN_POINT('Ctrl Pts',(14.4026149179538,-10.8763499173728,
804.030045883996));
#163574=CARTESIAN_POINT('Ctrl Pts',(13.3947726768058,-12.2109487310903,
802.535928236937));
#163575=CARTESIAN_POINT('Ctrl Pts',(12.1588589765331,-13.3376329379985,
801.041810589878));
#163576=CARTESIAN_POINT('Ctrl Pts',(10.9229452762603,-14.4643171449067,
799.54769294282));
#163577=CARTESIAN_POINT('Ctrl Pts',(9.50104767561053,-15.3447188656481,
798.053575295761));
#163578=CARTESIAN_POINT('Ctrl Pts',(8.07915007496071,-16.2251205863895,
796.559457648702));
#163579=CARTESIAN_POINT('Ctrl Pts',(6.51968959134574,-16.8292587962898,
795.065340001643));
#163580=CARTESIAN_POINT('Ctrl Pts',(4.96022910773078,-17.4333970061901,
793.571222354584));
#163581=CARTESIAN_POINT('Ctrl Pts',(3.31631129755346,-17.7406985030951,
792.077104707525));
#163582=CARTESIAN_POINT('Ctrl Pts',(1.67239348737615,-18.048,790.582987060467));
#163583=CARTESIAN_POINT('Ctrl Pts',(0.,-18.048,789.088869413408));
#163584=CARTESIAN_POINT('Ctrl Pts',(-1.67239348737615,-18.048,787.594751766349));
#163585=CARTESIAN_POINT('Ctrl Pts',(-3.31631129755346,-17.7406985030951,
786.10063411929));
#163586=CARTESIAN_POINT('Ctrl Pts',(-4.96022910773077,-17.4333970061901,
784.606516472231));
#163587=CARTESIAN_POINT('Ctrl Pts',(-6.51968959134574,-16.8292587962898,
783.112398825173));
#163588=CARTESIAN_POINT('Ctrl Pts',(-8.07915007496071,-16.2251205863895,
781.618281178114));
#163589=CARTESIAN_POINT('Ctrl Pts',(-9.50104767561052,-15.3447188656481,
780.124163531055));
#163590=CARTESIAN_POINT('Ctrl Pts',(-10.9229452762603,-14.4643171449067,
778.630045883996));
#163591=CARTESIAN_POINT('Ctrl Pts',(-12.1588589765331,-13.3376329379985,
777.135928236937));
#163592=CARTESIAN_POINT('Ctrl Pts',(-13.3947726768058,-12.2109487310903,
775.641810589879));
#163593=CARTESIAN_POINT('Ctrl Pts',(-14.4026149179538,-10.8763499173728,
774.14769294282));
#163594=CARTESIAN_POINT('Ctrl Pts',(-15.4104571591017,-9.54175110365538,
772.653575295761));
#163595=CARTESIAN_POINT('Ctrl Pts',(-16.1559070823762,-8.04468584505497,
771.159457648702));
#163596=CARTESIAN_POINT('Ctrl Pts',(-16.9013570056506,-6.54762058645456,
769.665340001643));
#163597=CARTESIAN_POINT('Ctrl Pts',(-17.3590292079831,-4.93906964482095,
768.171222354584));
#163598=CARTESIAN_POINT('Ctrl Pts',(-17.8167014103155,-3.33051870318735,
766.677104707526));
#163599=CARTESIAN_POINT('Ctrl Pts',(-17.9710104137728,-1.66525935159368,
765.182987060467));
#163600=CARTESIAN_POINT('Ctrl Pts',(-18.1253194172301,-1.10985572039171E-15,
763.688869413408));
#163601=CARTESIAN_POINT('Ctrl Pts',(-17.9710104137728,1.66525935159367,
762.194751766349));
#163602=CARTESIAN_POINT('Ctrl Pts',(-17.8167014103155,3.33051870318735,
760.70063411929));
#163603=CARTESIAN_POINT('Ctrl Pts',(-17.3590292079831,4.93906964482096,
759.206516472231));
#163604=CARTESIAN_POINT('Ctrl Pts',(-16.9013570056506,6.54762058645456,
757.712398825172));
#163605=CARTESIAN_POINT('Ctrl Pts',(-16.1559070823762,8.04468584505497,
756.218281178114));
#163606=CARTESIAN_POINT('Ctrl Pts',(-15.4104571591017,9.54175110365538,
754.724163531055));
#163607=CARTESIAN_POINT('Ctrl Pts',(-14.4026149179538,10.8763499173728,
753.230045883996));
#163608=CARTESIAN_POINT('Ctrl Pts',(-13.3947726768058,12.2109487310903,
751.735928236937));
#163609=CARTESIAN_POINT('Ctrl Pts',(-12.1588589765331,13.3376329379985,
750.241810589878));
#163610=CARTESIAN_POINT('Ctrl Pts',(-10.9229452762603,14.4643171449067,
748.74769294282));
#163611=CARTESIAN_POINT('Ctrl Pts',(-9.50104767561052,15.3447188656481,
747.253575295761));
#163612=CARTESIAN_POINT('Ctrl Pts',(-8.07915007496071,16.2251205863895,
745.759457648702));
#163613=CARTESIAN_POINT('Ctrl Pts',(-6.51968959134574,16.8292587962898,
744.265340001643));
#163614=CARTESIAN_POINT('Ctrl Pts',(-4.96022910773078,17.4333970061901,
742.771222354584));
#163615=CARTESIAN_POINT('Ctrl Pts',(-3.31631129755346,17.7406985030951,
741.277104707525));
#163616=CARTESIAN_POINT('Ctrl Pts',(-1.67239348737615,18.048,739.782987060467));
#163617=CARTESIAN_POINT('Ctrl Pts',(-2.21024254310115E-15,18.048,738.288869413408));
#163618=CARTESIAN_POINT('Ctrl Pts',(1.67239348737616,18.048,736.794751766349));
#163619=CARTESIAN_POINT('Ctrl Pts',(3.31631129755346,17.7406985030951,735.30063411929));
#163620=CARTESIAN_POINT('Ctrl Pts',(4.96022910773077,17.4333970061901,733.806516472231));
#163621=CARTESIAN_POINT('Ctrl Pts',(6.51968959134575,16.8292587962898,732.312398825173));
#163622=CARTESIAN_POINT('Ctrl Pts',(8.07915007496071,16.2251205863895,730.818281178114));
#163623=CARTESIAN_POINT('Ctrl Pts',(9.50104767561053,15.3447188656481,729.324163531055));
#163624=CARTESIAN_POINT('Ctrl Pts',(10.9229452762603,14.4643171449067,727.830045883996));
#163625=CARTESIAN_POINT('Ctrl Pts',(12.1588589765331,13.3376329379985,726.335928236937));
#163626=CARTESIAN_POINT('Ctrl Pts',(13.3947726768058,12.2109487310903,724.841810589879));
#163627=CARTESIAN_POINT('Ctrl Pts',(14.4026149179538,10.8763499173728,723.34769294282));
#163628=CARTESIAN_POINT('Ctrl Pts',(15.4104571591017,9.54175110365538,721.853575295761));
#163629=CARTESIAN_POINT('Ctrl Pts',(16.1559070823762,8.04468584505496,720.359457648702));
#163630=CARTESIAN_POINT('Ctrl Pts',(16.9013570056506,6.54762058645456,718.865340001643));
#163631=CARTESIAN_POINT('Ctrl Pts',(17.3590292079831,4.93906964482096,717.371222354584));
#163632=CARTESIAN_POINT('Ctrl Pts',(17.8167014103155,3.33051870318735,715.877104707526));
#163633=CARTESIAN_POINT('Ctrl Pts',(17.9710104137728,1.66525935159367,714.382987060467));
#163634=CARTESIAN_POINT('Ctrl Pts',(18.1253194172301,3.32956716117513E-15,
712.888869413408));
#163635=CARTESIAN_POINT('Ctrl Pts',(17.9710104137728,-1.66525935159367,
711.394751766349));
#163636=CARTESIAN_POINT('Ctrl Pts',(17.8167014103155,-3.33051870318736,
709.90063411929));
#163637=CARTESIAN_POINT('Ctrl Pts',(17.3590292079831,-4.93906964482095,
708.406516472231));
#163638=CARTESIAN_POINT('Ctrl Pts',(16.9013570056506,-6.54762058645456,
706.912398825173));
#163639=CARTESIAN_POINT('Ctrl Pts',(16.1559070823762,-8.04468584505497,
705.418281178114));
#163640=CARTESIAN_POINT('Ctrl Pts',(15.4104571591017,-9.54175110365538,
703.924163531055));
#163641=CARTESIAN_POINT('Ctrl Pts',(14.4026149179538,-10.8763499173728,
702.430045883996));
#163642=CARTESIAN_POINT('Ctrl Pts',(13.3947726768058,-12.2109487310903,
700.935928236937));
#163643=CARTESIAN_POINT('Ctrl Pts',(12.1588589765331,-13.3376329379985,
699.441810589878));
#163644=CARTESIAN_POINT('Ctrl Pts',(10.9229452762603,-14.4643171449067,
697.94769294282));
#163645=CARTESIAN_POINT('Ctrl Pts',(9.50104767561053,-15.3447188656481,
696.453575295761));
#163646=CARTESIAN_POINT('Ctrl Pts',(8.07915007496071,-16.2251205863895,
694.959457648702));
#163647=CARTESIAN_POINT('Ctrl Pts',(6.51968959134574,-16.8292587962898,
693.465340001643));
#163648=CARTESIAN_POINT('Ctrl Pts',(4.96022910773078,-17.4333970061901,
691.971222354584));
#163649=CARTESIAN_POINT('Ctrl Pts',(3.31631129755346,-17.7406985030951,
690.477104707526));
#163650=CARTESIAN_POINT('Ctrl Pts',(1.67239348737615,-18.048,688.982987060467));
#163651=CARTESIAN_POINT('Ctrl Pts',(0.,-18.048,687.488869413408));
#163652=CARTESIAN_POINT('Ctrl Pts',(-1.67239348737615,-18.048,685.994751766349));
#163653=CARTESIAN_POINT('Ctrl Pts',(-3.31631129755346,-17.7406985030951,
684.50063411929));
#163654=CARTESIAN_POINT('Ctrl Pts',(-4.96022910773077,-17.4333970061901,
683.006516472232));
#163655=CARTESIAN_POINT('Ctrl Pts',(-6.51968959134574,-16.8292587962898,
681.512398825172));
#163656=CARTESIAN_POINT('Ctrl Pts',(-8.07915007496071,-16.2251205863895,
680.018281178114));
#163657=CARTESIAN_POINT('Ctrl Pts',(-9.50104767561052,-15.3447188656481,
678.524163531055));
#163658=CARTESIAN_POINT('Ctrl Pts',(-10.9229452762603,-14.4643171449067,
677.030045883996));
#163659=CARTESIAN_POINT('Ctrl Pts',(-12.1588589765331,-13.3376329379985,
675.535928236937));
#163660=CARTESIAN_POINT('Ctrl Pts',(-13.3947726768058,-12.2109487310903,
674.041810589878));
#163661=CARTESIAN_POINT('Ctrl Pts',(-14.4026149179538,-10.8763499173728,
672.54769294282));
#163662=CARTESIAN_POINT('Ctrl Pts',(-15.4104571591017,-9.54175110365538,
671.053575295761));
#163663=CARTESIAN_POINT('Ctrl Pts',(-16.1559070823762,-8.04468584505497,
669.559457648702));
#163664=CARTESIAN_POINT('Ctrl Pts',(-16.9013570056506,-6.54762058645456,
668.065340001643));
#163665=CARTESIAN_POINT('Ctrl Pts',(-17.3590292079831,-4.93906964482095,
666.571222354584));
#163666=CARTESIAN_POINT('Ctrl Pts',(-17.8167014103155,-3.33051870318735,
665.077104707526));
#163667=CARTESIAN_POINT('Ctrl Pts',(-17.9710104137728,-1.66525935159368,
663.582987060467));
#163668=CARTESIAN_POINT('Ctrl Pts',(-18.1253194172301,-1.10985572039171E-15,
662.088869413408));
#163669=CARTESIAN_POINT('Ctrl Pts',(-17.9710104137728,1.66525935159367,
660.594751766349));
#163670=CARTESIAN_POINT('Ctrl Pts',(-17.8167014103155,3.33051870318735,
659.10063411929));
#163671=CARTESIAN_POINT('Ctrl Pts',(-17.3590292079831,4.93906964482096,
657.606516472231));
#163672=CARTESIAN_POINT('Ctrl Pts',(-16.9013570056506,6.54762058645456,
656.112398825172));
#163673=CARTESIAN_POINT('Ctrl Pts',(-16.1559070823762,8.04468584505497,
654.618281178114));
#163674=CARTESIAN_POINT('Ctrl Pts',(-15.4104571591017,9.54175110365538,
653.124163531055));
#163675=CARTESIAN_POINT('Ctrl Pts',(-14.4026149179538,10.8763499173728,
651.630045883996));
#163676=CARTESIAN_POINT('Ctrl Pts',(-13.3947726768058,12.2109487310903,
650.135928236937));
#163677=CARTESIAN_POINT('Ctrl Pts',(-12.1588589765331,13.3376329379985,
648.641810589878));
#163678=CARTESIAN_POINT('Ctrl Pts',(-10.9229452762603,14.4643171449067,
647.14769294282));
#163679=CARTESIAN_POINT('Ctrl Pts',(-9.50104767561052,15.3447188656481,
645.653575295761));
#163680=CARTESIAN_POINT('Ctrl Pts',(-8.07915007496071,16.2251205863895,
644.159457648702));
#163681=CARTESIAN_POINT('Ctrl Pts',(-6.51968959134574,16.8292587962898,
642.665340001643));
#163682=CARTESIAN_POINT('Ctrl Pts',(-4.96022910773078,17.4333970061901,
641.171222354584));
#163683=CARTESIAN_POINT('Ctrl Pts',(-3.31631129755346,17.7406985030951,
639.677104707525));
#163684=CARTESIAN_POINT('Ctrl Pts',(-1.67239348737615,18.048,638.182987060467));
#163685=CARTESIAN_POINT('Ctrl Pts',(-2.21024254310115E-15,18.048,636.688869413408));
#163686=CARTESIAN_POINT('Ctrl Pts',(1.67239348737616,18.048,635.194751766349));
#163687=CARTESIAN_POINT('Ctrl Pts',(3.31631129755346,17.7406985030951,633.70063411929));
#163688=CARTESIAN_POINT('Ctrl Pts',(4.96022910773077,17.4333970061901,632.206516472231));
#163689=CARTESIAN_POINT('Ctrl Pts',(6.51968959134575,16.8292587962898,630.712398825172));
#163690=CARTESIAN_POINT('Ctrl Pts',(8.07915007496071,16.2251205863895,629.218281178114));
#163691=CARTESIAN_POINT('Ctrl Pts',(9.50104767561053,15.3447188656481,627.724163531055));
#163692=CARTESIAN_POINT('Ctrl Pts',(10.9229452762603,14.4643171449067,626.230045883996));
#163693=CARTESIAN_POINT('Ctrl Pts',(12.1588589765331,13.3376329379985,624.735928236937));
#163694=CARTESIAN_POINT('Ctrl Pts',(13.3947726768058,12.2109487310903,623.241810589878));
#163695=CARTESIAN_POINT('Ctrl Pts',(14.4026149179538,10.8763499173728,621.74769294282));
#163696=CARTESIAN_POINT('Ctrl Pts',(15.4104571591017,9.54175110365538,620.253575295761));
#163697=CARTESIAN_POINT('Ctrl Pts',(16.1559070823762,8.04468584505496,618.759457648702));
#163698=CARTESIAN_POINT('Ctrl Pts',(16.9013570056506,6.54762058645456,617.265340001643));
#163699=CARTESIAN_POINT('Ctrl Pts',(17.3590292079831,4.93906964482096,615.771222354584));
#163700=CARTESIAN_POINT('Ctrl Pts',(17.8167014103155,3.33051870318735,614.277104707526));
#163701=CARTESIAN_POINT('Ctrl Pts',(17.9710104137728,1.66525935159367,612.782987060467));
#163702=CARTESIAN_POINT('Ctrl Pts',(18.1253194172301,3.32956716117513E-15,
611.288869413408));
#163703=CARTESIAN_POINT('Ctrl Pts',(17.9710104137728,-1.66525935159367,
609.794751766349));
#163704=CARTESIAN_POINT('Ctrl Pts',(17.8167014103155,-3.33051870318736,
608.30063411929));
#163705=CARTESIAN_POINT('Ctrl Pts',(17.3590292079831,-4.93906964482095,
606.806516472231));
#163706=CARTESIAN_POINT('Ctrl Pts',(16.9013570056506,-6.54762058645456,
605.312398825173));
#163707=CARTESIAN_POINT('Ctrl Pts',(16.1559070823762,-8.04468584505497,
603.818281178114));
#163708=CARTESIAN_POINT('Ctrl Pts',(15.4104571591017,-9.54175110365538,
602.324163531055));
#163709=CARTESIAN_POINT('Ctrl Pts',(14.4026149179538,-10.8763499173728,
600.830045883996));
#163710=CARTESIAN_POINT('Ctrl Pts',(13.3947726768058,-12.2109487310903,
599.335928236937));
#163711=CARTESIAN_POINT('Ctrl Pts',(12.1588589765331,-13.3376329379985,
597.841810589878));
#163712=CARTESIAN_POINT('Ctrl Pts',(10.9229452762603,-14.4643171449067,
596.34769294282));
#163713=CARTESIAN_POINT('Ctrl Pts',(9.50104767561053,-15.3447188656481,
594.853575295761));
#163714=CARTESIAN_POINT('Ctrl Pts',(8.07915007496071,-16.2251205863895,
593.359457648702));
#163715=CARTESIAN_POINT('Ctrl Pts',(6.51968959134574,-16.8292587962898,
591.865340001643));
#163716=CARTESIAN_POINT('Ctrl Pts',(4.96022910773078,-17.4333970061901,
590.371222354584));
#163717=CARTESIAN_POINT('Ctrl Pts',(3.31631129755346,-17.7406985030951,
588.877104707525));
#163718=CARTESIAN_POINT('Ctrl Pts',(1.67239348737615,-18.048,587.382987060467));
#163719=CARTESIAN_POINT('Ctrl Pts',(0.,-18.048,585.888869413408));
#163720=CARTESIAN_POINT('Ctrl Pts',(-1.67239348737615,-18.048,584.394751766349));
#163721=CARTESIAN_POINT('Ctrl Pts',(-3.31631129755346,-17.7406985030951,
582.90063411929));
#163722=CARTESIAN_POINT('Ctrl Pts',(-4.96022910773077,-17.4333970061901,
581.406516472231));
#163723=CARTESIAN_POINT('Ctrl Pts',(-6.51968959134574,-16.8292587962898,
579.912398825173));
#163724=CARTESIAN_POINT('Ctrl Pts',(-8.07915007496071,-16.2251205863895,
578.418281178114));
#163725=CARTESIAN_POINT('Ctrl Pts',(-9.50104767561052,-15.3447188656481,
576.924163531055));
#163726=CARTESIAN_POINT('Ctrl Pts',(-10.9229452762603,-14.4643171449067,
575.430045883996));
#163727=CARTESIAN_POINT('Ctrl Pts',(-12.1588589765331,-13.3376329379985,
573.935928236937));
#163728=CARTESIAN_POINT('Ctrl Pts',(-13.3947726768058,-12.2109487310903,
572.441810589879));
#163729=CARTESIAN_POINT('Ctrl Pts',(-14.4026149179538,-10.8763499173728,
570.94769294282));
#163730=CARTESIAN_POINT('Ctrl Pts',(-15.4104571591017,-9.54175110365538,
569.453575295761));
#163731=CARTESIAN_POINT('Ctrl Pts',(-16.1559070823762,-8.04468584505497,
567.959457648702));
#163732=CARTESIAN_POINT('Ctrl Pts',(-16.9013570056506,-6.54762058645456,
566.465340001643));
#163733=CARTESIAN_POINT('Ctrl Pts',(-17.3590292079831,-4.93906964482095,
564.971222354584));
#163734=CARTESIAN_POINT('Ctrl Pts',(-17.8167014103155,-3.33051870318735,
563.477104707526));
#163735=CARTESIAN_POINT('Ctrl Pts',(-17.9710104137728,-1.66525935159368,
561.982987060467));
#163736=CARTESIAN_POINT('Ctrl Pts',(-18.1253194172301,-1.10985572039171E-15,
560.488869413408));
#163737=CARTESIAN_POINT('Ctrl Pts',(-17.9710104137728,1.66525935159367,
558.994751766349));
#163738=CARTESIAN_POINT('Ctrl Pts',(-17.8167014103155,3.33051870318735,
557.50063411929));
#163739=CARTESIAN_POINT('Ctrl Pts',(-17.3590292079831,4.93906964482096,
556.006516472231));
#163740=CARTESIAN_POINT('Ctrl Pts',(-16.9013570056506,6.54762058645456,
554.512398825173));
#163741=CARTESIAN_POINT('Ctrl Pts',(-16.1559070823762,8.04468584505497,
553.018281178114));
#163742=CARTESIAN_POINT('Ctrl Pts',(-15.4104571591017,9.54175110365538,
551.524163531055));
#163743=CARTESIAN_POINT('Ctrl Pts',(-14.4026149179538,10.8763499173728,
550.030045883996));
#163744=CARTESIAN_POINT('Ctrl Pts',(-13.3947726768058,12.2109487310903,
548.535928236937));
#163745=CARTESIAN_POINT('Ctrl Pts',(-12.1588589765331,13.3376329379985,
547.041810589878));
#163746=CARTESIAN_POINT('Ctrl Pts',(-10.9229452762603,14.4643171449067,
545.54769294282));
#163747=CARTESIAN_POINT('Ctrl Pts',(-9.50104767561052,15.3447188656481,
544.053575295761));
#163748=CARTESIAN_POINT('Ctrl Pts',(-8.07915007496071,16.2251205863895,
542.559457648702));
#163749=CARTESIAN_POINT('Ctrl Pts',(-6.51968959134574,16.8292587962898,
541.065340001643));
#163750=CARTESIAN_POINT('Ctrl Pts',(-4.96022910773078,17.4333970061901,
539.571222354584));
#163751=CARTESIAN_POINT('Ctrl Pts',(-3.31631129755346,17.7406985030951,
538.077104707525));
#163752=CARTESIAN_POINT('Ctrl Pts',(-1.67239348737615,18.048,536.582987060467));
#163753=CARTESIAN_POINT('Ctrl Pts',(-2.21024254310115E-15,18.048,535.088869413408));
#163754=CARTESIAN_POINT('Ctrl Pts',(1.67239348737616,18.048,533.594751766349));
#163755=CARTESIAN_POINT('Ctrl Pts',(3.31631129755346,17.7406985030951,532.10063411929));
#163756=CARTESIAN_POINT('Ctrl Pts',(4.96022910773077,17.4333970061901,530.606516472231));
#163757=CARTESIAN_POINT('Ctrl Pts',(6.51968959134575,16.8292587962898,529.112398825172));
#163758=CARTESIAN_POINT('Ctrl Pts',(8.07915007496071,16.2251205863895,527.618281178114));
#163759=CARTESIAN_POINT('Ctrl Pts',(9.50104767561053,15.3447188656481,526.124163531055));
#163760=CARTESIAN_POINT('Ctrl Pts',(10.9229452762603,14.4643171449067,524.630045883996));
#163761=CARTESIAN_POINT('Ctrl Pts',(12.1588589765331,13.3376329379985,523.135928236937));
#163762=CARTESIAN_POINT('Ctrl Pts',(13.3947726768058,12.2109487310903,521.641810589878));
#163763=CARTESIAN_POINT('Ctrl Pts',(14.4026149179538,10.8763499173728,520.14769294282));
#163764=CARTESIAN_POINT('Ctrl Pts',(15.4104571591017,9.54175110365538,518.653575295761));
#163765=CARTESIAN_POINT('Ctrl Pts',(16.1559070823762,8.04468584505496,517.159457648702));
#163766=CARTESIAN_POINT('Ctrl Pts',(16.9013570056506,6.54762058645456,515.665340001643));
#163767=CARTESIAN_POINT('Ctrl Pts',(17.3590292079831,4.93906964482096,514.171222354584));
#163768=CARTESIAN_POINT('Ctrl Pts',(17.8167014103155,3.33051870318735,512.677104707525));
#163769=CARTESIAN_POINT('Ctrl Pts',(17.9710104137728,1.66525935159367,511.182987060467));
#163770=CARTESIAN_POINT('Ctrl Pts',(18.1253194172301,3.32956716117513E-15,
509.688869413408));
#163771=CARTESIAN_POINT('Ctrl Pts',(17.9710104137728,-1.66525935159367,
508.194751766349));
#163772=CARTESIAN_POINT('Ctrl Pts',(17.8167014103155,-3.33051870318736,
506.70063411929));
#163773=CARTESIAN_POINT('Ctrl Pts',(17.3590292079831,-4.93906964482095,
505.206516472231));
#163774=CARTESIAN_POINT('Ctrl Pts',(16.9013570056506,-6.54762058645456,
503.712398825173));
#163775=CARTESIAN_POINT('Ctrl Pts',(16.1559070823762,-8.04468584505497,
502.218281178114));
#163776=CARTESIAN_POINT('Ctrl Pts',(15.4104571591017,-9.54175110365538,
500.724163531055));
#163777=CARTESIAN_POINT('Ctrl Pts',(14.4026149179538,-10.8763499173728,
499.230045883996));
#163778=CARTESIAN_POINT('Ctrl Pts',(13.3947726768058,-12.2109487310903,
497.735928236937));
#163779=CARTESIAN_POINT('Ctrl Pts',(12.1588589765331,-13.3376329379985,
496.241810589879));
#163780=CARTESIAN_POINT('Ctrl Pts',(10.9229452762603,-14.4643171449067,
494.74769294282));
#163781=CARTESIAN_POINT('Ctrl Pts',(9.50104767561053,-15.3447188656481,
493.253575295761));
#163782=CARTESIAN_POINT('Ctrl Pts',(8.07915007496071,-16.2251205863895,
491.759457648702));
#163783=CARTESIAN_POINT('Ctrl Pts',(6.51968959134574,-16.8292587962898,
490.265340001643));
#163784=CARTESIAN_POINT('Ctrl Pts',(4.96022910773078,-17.4333970061901,
488.771222354584));
#163785=CARTESIAN_POINT('Ctrl Pts',(3.31631129755346,-17.7406985030951,
487.277104707526));
#163786=CARTESIAN_POINT('Ctrl Pts',(1.67239348737615,-18.048,485.782987060467));
#163787=CARTESIAN_POINT('Ctrl Pts',(0.,-18.048,484.288869413408));
#163788=CARTESIAN_POINT('Ctrl Pts',(-1.67239348737615,-18.048,482.794751766349));
#163789=CARTESIAN_POINT('Ctrl Pts',(-3.31631129755346,-17.7406985030951,
481.30063411929));
#163790=CARTESIAN_POINT('Ctrl Pts',(-4.96022910773077,-17.4333970061901,
479.806516472231));
#163791=CARTESIAN_POINT('Ctrl Pts',(-6.51968959134574,-16.8292587962898,
478.312398825173));
#163792=CARTESIAN_POINT('Ctrl Pts',(-8.07915007496071,-16.2251205863895,
476.818281178114));
#163793=CARTESIAN_POINT('Ctrl Pts',(-9.50104767561052,-15.3447188656481,
475.324163531055));
#163794=CARTESIAN_POINT('Ctrl Pts',(-10.9229452762603,-14.4643171449067,
473.830045883996));
#163795=CARTESIAN_POINT('Ctrl Pts',(-12.1588589765331,-13.3376329379985,
472.335928236937));
#163796=CARTESIAN_POINT('Ctrl Pts',(-13.3947726768058,-12.2109487310903,
470.841810589878));
#163797=CARTESIAN_POINT('Ctrl Pts',(-14.4026149179538,-10.8763499173728,
469.34769294282));
#163798=CARTESIAN_POINT('Ctrl Pts',(-15.4104571591017,-9.54175110365538,
467.853575295761));
#163799=CARTESIAN_POINT('Ctrl Pts',(-16.1559070823762,-8.04468584505497,
466.359457648702));
#163800=CARTESIAN_POINT('Ctrl Pts',(-16.9013570056506,-6.54762058645456,
464.865340001643));
#163801=CARTESIAN_POINT('Ctrl Pts',(-17.3590292079831,-4.93906964482095,
463.371222354584));
#163802=CARTESIAN_POINT('Ctrl Pts',(-17.8167014103155,-3.33051870318735,
461.877104707525));
#163803=CARTESIAN_POINT('Ctrl Pts',(-17.9710104137728,-1.66525935159368,
460.382987060467));
#163804=CARTESIAN_POINT('Ctrl Pts',(-18.1253194172301,-1.10985572039171E-15,
458.888869413408));
#163805=CARTESIAN_POINT('Ctrl Pts',(-17.9710104137728,1.66525935159367,
457.394751766349));
#163806=CARTESIAN_POINT('Ctrl Pts',(-17.8167014103155,3.33051870318735,
455.90063411929));
#163807=CARTESIAN_POINT('Ctrl Pts',(-17.3590292079831,4.93906964482096,
454.406516472231));
#163808=CARTESIAN_POINT('Ctrl Pts',(-16.9013570056506,6.54762058645456,
452.912398825173));
#163809=CARTESIAN_POINT('Ctrl Pts',(-16.1559070823762,8.04468584505497,
451.418281178114));
#163810=CARTESIAN_POINT('Ctrl Pts',(-15.4104571591017,9.54175110365538,
449.924163531055));
#163811=CARTESIAN_POINT('Ctrl Pts',(-14.4026149179538,10.8763499173728,
448.430045883996));
#163812=CARTESIAN_POINT('Ctrl Pts',(-13.3947726768058,12.2109487310903,
446.935928236937));
#163813=CARTESIAN_POINT('Ctrl Pts',(-12.1588589765331,13.3376329379985,
445.441810589878));
#163814=CARTESIAN_POINT('Ctrl Pts',(-10.9229452762603,14.4643171449067,
443.94769294282));
#163815=CARTESIAN_POINT('Ctrl Pts',(-9.50104767561052,15.3447188656481,
442.453575295761));
#163816=CARTESIAN_POINT('Ctrl Pts',(-8.07915007496071,16.2251205863895,
440.959457648702));
#163817=CARTESIAN_POINT('Ctrl Pts',(-6.51968959134574,16.8292587962898,
439.465340001643));
#163818=CARTESIAN_POINT('Ctrl Pts',(-4.96022910773078,17.4333970061901,
437.971222354584));
#163819=CARTESIAN_POINT('Ctrl Pts',(-3.31631129755346,17.7406985030951,
436.477104707526));
#163820=CARTESIAN_POINT('Ctrl Pts',(-1.67239348737615,18.048,434.982987060467));
#163821=CARTESIAN_POINT('Ctrl Pts',(-2.21024254310115E-15,18.048,433.488869413408));
#163822=CARTESIAN_POINT('Ctrl Pts',(1.67239348737616,18.048,431.994751766349));
#163823=CARTESIAN_POINT('Ctrl Pts',(3.31631129755346,17.7406985030951,430.50063411929));
#163824=CARTESIAN_POINT('Ctrl Pts',(4.96022910773077,17.4333970061901,429.006516472231));
#163825=CARTESIAN_POINT('Ctrl Pts',(6.51968959134575,16.8292587962898,427.512398825173));
#163826=CARTESIAN_POINT('Ctrl Pts',(8.07915007496071,16.2251205863895,426.018281178114));
#163827=CARTESIAN_POINT('Ctrl Pts',(9.50104767561053,15.3447188656481,424.524163531055));
#163828=CARTESIAN_POINT('Ctrl Pts',(10.9229452762603,14.4643171449067,423.030045883996));
#163829=CARTESIAN_POINT('Ctrl Pts',(12.1588589765331,13.3376329379985,421.535928236937));
#163830=CARTESIAN_POINT('Ctrl Pts',(13.3947726768058,12.2109487310903,420.041810589879));
#163831=CARTESIAN_POINT('Ctrl Pts',(14.4026149179538,10.8763499173728,418.54769294282));
#163832=CARTESIAN_POINT('Ctrl Pts',(15.4104571591017,9.54175110365538,417.053575295761));
#163833=CARTESIAN_POINT('Ctrl Pts',(16.1559070823762,8.04468584505496,415.559457648702));
#163834=CARTESIAN_POINT('Ctrl Pts',(16.9013570056506,6.54762058645456,414.065340001643));
#163835=CARTESIAN_POINT('Ctrl Pts',(17.3590292079831,4.93906964482096,412.571222354584));
#163836=CARTESIAN_POINT('Ctrl Pts',(17.8167014103155,3.33051870318735,411.077104707526));
#163837=CARTESIAN_POINT('Ctrl Pts',(17.9710104137728,1.66525935159367,409.582987060467));
#163838=CARTESIAN_POINT('Ctrl Pts',(18.1253194172301,3.32956716117513E-15,
408.088869413408));
#163839=CARTESIAN_POINT('Ctrl Pts',(17.9710104137728,-1.66525935159367,
406.594751766349));
#163840=CARTESIAN_POINT('Ctrl Pts',(17.8167014103155,-3.33051870318736,
405.10063411929));
#163841=CARTESIAN_POINT('Ctrl Pts',(17.3590292079831,-4.93906964482095,
403.606516472231));
#163842=CARTESIAN_POINT('Ctrl Pts',(16.9013570056506,-6.54762058645456,
402.112398825173));
#163843=CARTESIAN_POINT('Ctrl Pts',(16.1559070823762,-8.04468584505497,
400.618281178114));
#163844=CARTESIAN_POINT('Ctrl Pts',(15.4104571591017,-9.54175110365538,
399.124163531055));
#163845=CARTESIAN_POINT('Ctrl Pts',(14.4026149179538,-10.8763499173728,
397.630045883996));
#163846=CARTESIAN_POINT('Ctrl Pts',(13.3947726768058,-12.2109487310903,
396.135928236937));
#163847=CARTESIAN_POINT('Ctrl Pts',(12.1588589765331,-13.3376329379985,
394.641810589878));
#163848=CARTESIAN_POINT('Ctrl Pts',(10.9229452762603,-14.4643171449067,
393.147692942819));
#163849=CARTESIAN_POINT('Ctrl Pts',(9.50104767561053,-15.3447188656481,
391.653575295761));
#163850=CARTESIAN_POINT('Ctrl Pts',(8.07915007496071,-16.2251205863895,
390.159457648702));
#163851=CARTESIAN_POINT('Ctrl Pts',(6.51968959134574,-16.8292587962898,
388.665340001643));
#163852=CARTESIAN_POINT('Ctrl Pts',(4.96022910773078,-17.4333970061901,
387.171222354584));
#163853=CARTESIAN_POINT('Ctrl Pts',(3.31631129755346,-17.7406985030951,
385.677104707525));
#163854=CARTESIAN_POINT('Ctrl Pts',(1.67239348737615,-18.048,384.182987060467));
#163855=CARTESIAN_POINT('Ctrl Pts',(0.,-18.048,382.688869413408));
#163856=CARTESIAN_POINT('Ctrl Pts',(-1.67239348737615,-18.048,381.194751766349));
#163857=CARTESIAN_POINT('Ctrl Pts',(-3.31631129755346,-17.7406985030951,
379.70063411929));
#163858=CARTESIAN_POINT('Ctrl Pts',(-4.96022910773077,-17.4333970061901,
378.206516472231));
#163859=CARTESIAN_POINT('Ctrl Pts',(-6.51968959134574,-16.8292587962898,
376.712398825173));
#163860=CARTESIAN_POINT('Ctrl Pts',(-8.07915007496071,-16.2251205863895,
375.218281178114));
#163861=CARTESIAN_POINT('Ctrl Pts',(-9.50104767561052,-15.3447188656481,
373.724163531055));
#163862=CARTESIAN_POINT('Ctrl Pts',(-10.9229452762603,-14.4643171449067,
372.230045883996));
#163863=CARTESIAN_POINT('Ctrl Pts',(-12.1588589765331,-13.3376329379985,
370.735928236937));
#163864=CARTESIAN_POINT('Ctrl Pts',(-13.3947726768058,-12.2109487310903,
369.241810589879));
#163865=CARTESIAN_POINT('Ctrl Pts',(-14.4026149179538,-10.8763499173728,
367.74769294282));
#163866=CARTESIAN_POINT('Ctrl Pts',(-15.4104571591017,-9.54175110365538,
366.253575295761));
#163867=CARTESIAN_POINT('Ctrl Pts',(-16.1559070823762,-8.04468584505497,
364.759457648702));
#163868=CARTESIAN_POINT('Ctrl Pts',(-16.9013570056506,-6.54762058645456,
363.265340001643));
#163869=CARTESIAN_POINT('Ctrl Pts',(-17.3590292079831,-4.93906964482095,
361.771222354584));
#163870=CARTESIAN_POINT('Ctrl Pts',(-17.8167014103155,-3.33051870318735,
360.277104707525));
#163871=CARTESIAN_POINT('Ctrl Pts',(-17.9710104137728,-1.66525935159368,
358.782987060467));
#163872=CARTESIAN_POINT('Ctrl Pts',(-18.1253194172301,-1.10985572039171E-15,
357.288869413408));
#163873=CARTESIAN_POINT('Ctrl Pts',(-17.9710104137728,1.66525935159367,
355.794751766349));
#163874=CARTESIAN_POINT('Ctrl Pts',(-17.8167014103155,3.33051870318735,
354.30063411929));
#163875=CARTESIAN_POINT('Ctrl Pts',(-17.3590292079831,4.93906964482096,
352.806516472231));
#163876=CARTESIAN_POINT('Ctrl Pts',(-16.9013570056506,6.54762058645456,
351.312398825173));
#163877=CARTESIAN_POINT('Ctrl Pts',(-16.1559070823762,8.04468584505497,
349.818281178114));
#163878=CARTESIAN_POINT('Ctrl Pts',(-15.4104571591017,9.54175110365538,
348.324163531055));
#163879=CARTESIAN_POINT('Ctrl Pts',(-14.4026149179538,10.8763499173728,
346.830045883996));
#163880=CARTESIAN_POINT('Ctrl Pts',(-13.3947726768058,12.2109487310903,
345.335928236937));
#163881=CARTESIAN_POINT('Ctrl Pts',(-12.1588589765331,13.3376329379985,
343.841810589878));
#163882=CARTESIAN_POINT('Ctrl Pts',(-10.9229452762603,14.4643171449067,
342.34769294282));
#163883=CARTESIAN_POINT('Ctrl Pts',(-9.50104767561052,15.3447188656481,
340.853575295761));
#163884=CARTESIAN_POINT('Ctrl Pts',(-8.07915007496071,16.2251205863895,
339.359457648702));
#163885=CARTESIAN_POINT('Ctrl Pts',(-6.51968959134574,16.8292587962898,
337.865340001643));
#163886=CARTESIAN_POINT('Ctrl Pts',(-4.96022910773078,17.4333970061901,
336.371222354584));
#163887=CARTESIAN_POINT('Ctrl Pts',(-3.31631129755346,17.7406985030951,
334.877104707525));
#163888=CARTESIAN_POINT('Ctrl Pts',(-1.67239348737615,18.048,333.382987060467));
#163889=CARTESIAN_POINT('Ctrl Pts',(-2.21024254310115E-15,18.048,331.888869413408));
#163890=CARTESIAN_POINT('Ctrl Pts',(1.67239348737616,18.048,330.394751766349));
#163891=CARTESIAN_POINT('Ctrl Pts',(3.31631129755346,17.7406985030951,328.90063411929));
#163892=CARTESIAN_POINT('Ctrl Pts',(4.96022910773077,17.4333970061901,327.406516472231));
#163893=CARTESIAN_POINT('Ctrl Pts',(6.51968959134575,16.8292587962898,325.912398825172));
#163894=CARTESIAN_POINT('Ctrl Pts',(8.07915007496071,16.2251205863895,324.418281178114));
#163895=CARTESIAN_POINT('Ctrl Pts',(9.50104767561053,15.3447188656481,322.924163531055));
#163896=CARTESIAN_POINT('Ctrl Pts',(10.9229452762603,14.4643171449067,321.430045883996));
#163897=CARTESIAN_POINT('Ctrl Pts',(12.1588589765331,13.3376329379985,319.935928236937));
#163898=CARTESIAN_POINT('Ctrl Pts',(13.3947726768058,12.2109487310903,318.441810589878));
#163899=CARTESIAN_POINT('Ctrl Pts',(14.4026149179538,10.8763499173728,316.94769294282));
#163900=CARTESIAN_POINT('Ctrl Pts',(15.4104571591017,9.54175110365538,315.453575295761));
#163901=CARTESIAN_POINT('Ctrl Pts',(16.1559070823762,8.04468584505496,313.959457648702));
#163902=CARTESIAN_POINT('Ctrl Pts',(16.9013570056506,6.54762058645456,312.465340001643));
#163903=CARTESIAN_POINT('Ctrl Pts',(17.3590292079831,4.93906964482096,310.971222354584));
#163904=CARTESIAN_POINT('Ctrl Pts',(17.8167014103155,3.33051870318735,309.477104707526));
#163905=CARTESIAN_POINT('Ctrl Pts',(17.9710104137728,1.66525935159367,307.982987060467));
#163906=CARTESIAN_POINT('Ctrl Pts',(18.1253194172301,3.32956716117513E-15,
306.488869413408));
#163907=CARTESIAN_POINT('Ctrl Pts',(17.9710104137728,-1.66525935159367,
304.994751766349));
#163908=CARTESIAN_POINT('Ctrl Pts',(17.8167014103155,-3.33051870318736,
303.50063411929));
#163909=CARTESIAN_POINT('Ctrl Pts',(17.3590292079831,-4.93906964482095,
302.006516472231));
#163910=CARTESIAN_POINT('Ctrl Pts',(16.9013570056506,-6.54762058645456,
300.512398825173));
#163911=CARTESIAN_POINT('Ctrl Pts',(16.1559070823762,-8.04468584505497,
299.018281178114));
#163912=CARTESIAN_POINT('Ctrl Pts',(15.4104571591017,-9.54175110365538,
297.524163531055));
#163913=CARTESIAN_POINT('Ctrl Pts',(14.4026149179538,-10.8763499173728,
296.030045883996));
#163914=CARTESIAN_POINT('Ctrl Pts',(13.3947726768058,-12.2109487310903,
294.535928236937));
#163915=CARTESIAN_POINT('Ctrl Pts',(12.1588589765331,-13.3376329379985,
293.041810589878));
#163916=CARTESIAN_POINT('Ctrl Pts',(10.9229452762603,-14.4643171449067,
291.54769294282));
#163917=CARTESIAN_POINT('Ctrl Pts',(9.50104767561053,-15.3447188656481,
290.053575295761));
#163918=CARTESIAN_POINT('Ctrl Pts',(8.07915007496071,-16.2251205863895,
288.559457648702));
#163919=CARTESIAN_POINT('Ctrl Pts',(6.51968959134574,-16.8292587962898,
287.065340001643));
#163920=CARTESIAN_POINT('Ctrl Pts',(4.96022910773078,-17.4333970061901,
285.571222354584));
#163921=CARTESIAN_POINT('Ctrl Pts',(3.31631129755346,-17.7406985030951,
284.077104707525));
#163922=CARTESIAN_POINT('Ctrl Pts',(1.67239348737615,-18.048,282.582987060467));
#163923=CARTESIAN_POINT('Ctrl Pts',(0.,-18.048,281.088869413408));
#163924=CARTESIAN_POINT('Ctrl Pts',(-1.67239348737615,-18.048,279.594751766349));
#163925=CARTESIAN_POINT('Ctrl Pts',(-3.31631129755346,-17.7406985030951,
278.10063411929));
#163926=CARTESIAN_POINT('Ctrl Pts',(-4.96022910773077,-17.4333970061901,
276.606516472231));
#163927=CARTESIAN_POINT('Ctrl Pts',(-6.51968959134574,-16.8292587962898,
275.112398825172));
#163928=CARTESIAN_POINT('Ctrl Pts',(-8.07915007496071,-16.2251205863895,
273.618281178114));
#163929=CARTESIAN_POINT('Ctrl Pts',(-9.50104767561052,-15.3447188656481,
272.124163531055));
#163930=CARTESIAN_POINT('Ctrl Pts',(-10.9229452762603,-14.4643171449067,
270.630045883996));
#163931=CARTESIAN_POINT('Ctrl Pts',(-12.1588589765331,-13.3376329379985,
269.135928236937));
#163932=CARTESIAN_POINT('Ctrl Pts',(-13.3947726768058,-12.2109487310903,
267.641810589878));
#163933=CARTESIAN_POINT('Ctrl Pts',(-14.4026149179538,-10.8763499173728,
266.14769294282));
#163934=CARTESIAN_POINT('Ctrl Pts',(-15.4104571591017,-9.54175110365538,
264.653575295761));
#163935=CARTESIAN_POINT('Ctrl Pts',(-16.1559070823762,-8.04468584505497,
263.159457648702));
#163936=CARTESIAN_POINT('Ctrl Pts',(-16.9013570056506,-6.54762058645456,
261.665340001643));
#163937=CARTESIAN_POINT('Ctrl Pts',(-17.3590292079831,-4.93906964482095,
260.171222354584));
#163938=CARTESIAN_POINT('Ctrl Pts',(-17.8167014103155,-3.33051870318735,
258.677104707525));
#163939=CARTESIAN_POINT('Ctrl Pts',(-17.9710104137728,-1.66525935159368,
257.182987060467));
#163940=CARTESIAN_POINT('Ctrl Pts',(-18.1253194172301,-1.10985572039171E-15,
255.688869413408));
#163941=CARTESIAN_POINT('Ctrl Pts',(-17.9710104137728,1.66525935159367,
254.194751766349));
#163942=CARTESIAN_POINT('Ctrl Pts',(-17.8167014103155,3.33051870318735,
252.70063411929));
#163943=CARTESIAN_POINT('Ctrl Pts',(-17.3590292079831,4.93906964482096,
251.206516472231));
#163944=CARTESIAN_POINT('Ctrl Pts',(-16.9013570056506,6.54762058645456,
249.712398825173));
#163945=CARTESIAN_POINT('Ctrl Pts',(-16.1559070823762,8.04468584505497,
248.218281178114));
#163946=CARTESIAN_POINT('Ctrl Pts',(-15.4104571591017,9.54175110365538,
246.724163531055));
#163947=CARTESIAN_POINT('Ctrl Pts',(-14.4026149179538,10.8763499173728,
245.230045883996));
#163948=CARTESIAN_POINT('Ctrl Pts',(-13.3947726768058,12.2109487310903,
243.735928236937));
#163949=CARTESIAN_POINT('Ctrl Pts',(-12.1588589765331,13.3376329379985,
242.241810589878));
#163950=CARTESIAN_POINT('Ctrl Pts',(-10.9229452762603,14.4643171449067,
240.74769294282));
#163951=CARTESIAN_POINT('Ctrl Pts',(-9.50104767561052,15.3447188656481,
239.253575295761));
#163952=CARTESIAN_POINT('Ctrl Pts',(-8.07915007496071,16.2251205863895,
237.759457648702));
#163953=CARTESIAN_POINT('Ctrl Pts',(-6.51968959134574,16.8292587962898,
236.265340001643));
#163954=CARTESIAN_POINT('Ctrl Pts',(-4.96022910773078,17.4333970061901,
234.771222354584));
#163955=CARTESIAN_POINT('Ctrl Pts',(-3.31631129755346,17.7406985030951,
233.277104707525));
#163956=CARTESIAN_POINT('Ctrl Pts',(-1.67239348737615,18.048,231.782987060467));
#163957=CARTESIAN_POINT('Ctrl Pts',(-2.21024254310115E-15,18.048,230.288869413408));
#163958=CARTESIAN_POINT('Ctrl Pts',(1.67239348737616,18.048,228.794751766349));
#163959=CARTESIAN_POINT('Ctrl Pts',(3.31631129755346,17.7406985030951,227.30063411929));
#163960=CARTESIAN_POINT('Ctrl Pts',(4.96022910773077,17.4333970061901,225.806516472231));
#163961=CARTESIAN_POINT('Ctrl Pts',(6.51968959134575,16.8292587962898,224.312398825173));
#163962=CARTESIAN_POINT('Ctrl Pts',(8.07915007496071,16.2251205863895,222.818281178114));
#163963=CARTESIAN_POINT('Ctrl Pts',(9.50104767561053,15.3447188656481,221.324163531055));
#163964=CARTESIAN_POINT('Ctrl Pts',(10.9229452762603,14.4643171449067,219.830045883996));
#163965=CARTESIAN_POINT('Ctrl Pts',(12.1588589765331,13.3376329379985,218.335928236937));
#163966=CARTESIAN_POINT('Ctrl Pts',(13.3947726768058,12.2109487310903,216.841810589878));
#163967=CARTESIAN_POINT('Ctrl Pts',(14.4026149179538,10.8763499173728,215.34769294282));
#163968=CARTESIAN_POINT('Ctrl Pts',(15.4104571591017,9.54175110365538,213.853575295761));
#163969=CARTESIAN_POINT('Ctrl Pts',(16.1559070823762,8.04468584505496,212.359457648702));
#163970=CARTESIAN_POINT('Ctrl Pts',(16.9013570056506,6.54762058645456,210.865340001643));
#163971=CARTESIAN_POINT('Ctrl Pts',(17.3590292079831,4.93906964482096,209.371222354584));
#163972=CARTESIAN_POINT('Ctrl Pts',(17.8167014103155,3.33051870318735,207.877104707525));
#163973=CARTESIAN_POINT('Ctrl Pts',(17.9710104137728,1.66525935159367,206.382987060467));
#163974=CARTESIAN_POINT('Ctrl Pts',(18.1253194172301,3.32956716117513E-15,
204.888869413408));
#163975=CARTESIAN_POINT('Ctrl Pts',(17.9710104137728,-1.66525935159367,
203.394751766349));
#163976=CARTESIAN_POINT('Ctrl Pts',(17.8167014103155,-3.33051870318736,
201.90063411929));
#163977=CARTESIAN_POINT('Ctrl Pts',(17.3590292079831,-4.93906964482095,
200.406516472231));
#163978=CARTESIAN_POINT('Ctrl Pts',(16.9013570056506,-6.54762058645456,
198.912398825172));
#163979=CARTESIAN_POINT('Ctrl Pts',(16.1559070823762,-8.04468584505497,
197.418281178114));
#163980=CARTESIAN_POINT('Ctrl Pts',(15.4104571591017,-9.54175110365538,
195.924163531055));
#163981=CARTESIAN_POINT('Ctrl Pts',(14.4026149179538,-10.8763499173728,
194.430045883996));
#163982=CARTESIAN_POINT('Ctrl Pts',(13.3947726768058,-12.2109487310903,
192.935928236937));
#163983=CARTESIAN_POINT('Ctrl Pts',(12.1588589765331,-13.3376329379985,
191.441810589878));
#163984=CARTESIAN_POINT('Ctrl Pts',(10.9229452762603,-14.4643171449067,
189.94769294282));
#163985=CARTESIAN_POINT('Ctrl Pts',(9.50104767561053,-15.3447188656481,
188.453575295761));
#163986=CARTESIAN_POINT('Ctrl Pts',(8.07915007496071,-16.2251205863895,
186.959457648702));
#163987=CARTESIAN_POINT('Ctrl Pts',(6.51968959134574,-16.8292587962898,
185.465340001643));
#163988=CARTESIAN_POINT('Ctrl Pts',(4.96022910773078,-17.4333970061901,
183.971222354584));
#163989=CARTESIAN_POINT('Ctrl Pts',(3.31631129755346,-17.7406985030951,
182.477104707526));
#163990=CARTESIAN_POINT('Ctrl Pts',(1.67239348737615,-18.048,180.982987060467));
#163991=CARTESIAN_POINT('Ctrl Pts',(0.,-18.048,179.488869413408));
#163992=CARTESIAN_POINT('Ctrl Pts',(-1.67239348737615,-18.048,177.994751766349));
#163993=CARTESIAN_POINT('Ctrl Pts',(-3.31631129755346,-17.7406985030951,
176.50063411929));
#163994=CARTESIAN_POINT('Ctrl Pts',(-4.96022910773077,-17.4333970061901,
175.006516472231));
#163995=CARTESIAN_POINT('Ctrl Pts',(-6.51968959134574,-16.8292587962898,
173.512398825173));
#163996=CARTESIAN_POINT('Ctrl Pts',(-8.07915007496071,-16.2251205863895,
172.018281178114));
#163997=CARTESIAN_POINT('Ctrl Pts',(-9.50104767561052,-15.3447188656481,
170.524163531055));
#163998=CARTESIAN_POINT('Ctrl Pts',(-10.9229452762603,-14.4643171449067,
169.030045883996));
#163999=CARTESIAN_POINT('Ctrl Pts',(-12.1588589765331,-13.3376329379985,
167.535928236937));
#164000=CARTESIAN_POINT('Ctrl Pts',(-13.3947726768058,-12.2109487310903,
166.041810589878));
#164001=CARTESIAN_POINT('Ctrl Pts',(-14.4026149179538,-10.8763499173728,
164.54769294282));
#164002=CARTESIAN_POINT('Ctrl Pts',(-15.4104571591017,-9.54175110365538,
163.053575295761));
#164003=CARTESIAN_POINT('Ctrl Pts',(-16.1559070823762,-8.04468584505497,
161.559457648702));
#164004=CARTESIAN_POINT('Ctrl Pts',(-16.9013570056506,-6.54762058645456,
160.065340001643));
#164005=CARTESIAN_POINT('Ctrl Pts',(-17.3590292079831,-4.93906964482095,
158.571222354584));
#164006=CARTESIAN_POINT('Ctrl Pts',(-17.8167014103155,-3.33051870318735,
157.077104707525));
#164007=CARTESIAN_POINT('Ctrl Pts',(-17.9710104137728,-1.66525935159368,
155.582987060467));
#164008=CARTESIAN_POINT('Ctrl Pts',(-18.1253194172301,-1.10985572039171E-15,
154.088869413408));
#164009=CARTESIAN_POINT('Ctrl Pts',(-17.9710104137728,1.66525935159367,
152.594751766349));
#164010=CARTESIAN_POINT('Ctrl Pts',(-17.8167014103155,3.33051870318735,
151.10063411929));
#164011=CARTESIAN_POINT('Ctrl Pts',(-17.3590292079831,4.93906964482096,
149.606516472231));
#164012=CARTESIAN_POINT('Ctrl Pts',(-16.9013570056506,6.54762058645456,
148.112398825172));
#164013=CARTESIAN_POINT('Ctrl Pts',(-16.1559070823762,8.04468584505497,
146.618281178114));
#164014=CARTESIAN_POINT('Ctrl Pts',(-15.4104571591017,9.54175110365538,
145.124163531055));
#164015=CARTESIAN_POINT('Ctrl Pts',(-14.4026149179538,10.8763499173728,
143.630045883996));
#164016=CARTESIAN_POINT('Ctrl Pts',(-13.3947726768058,12.2109487310903,
142.135928236937));
#164017=CARTESIAN_POINT('Ctrl Pts',(-12.1588589765331,13.3376329379985,
140.641810589878));
#164018=CARTESIAN_POINT('Ctrl Pts',(-10.9229452762603,14.4643171449067,
139.147692942819));
#164019=CARTESIAN_POINT('Ctrl Pts',(-9.50104767561052,15.3447188656481,
137.653575295761));
#164020=CARTESIAN_POINT('Ctrl Pts',(-8.07915007496071,16.2251205863895,
136.159457648702));
#164021=CARTESIAN_POINT('Ctrl Pts',(-6.51968959134574,16.8292587962898,
134.665340001643));
#164022=CARTESIAN_POINT('Ctrl Pts',(-4.96022910773078,17.4333970061901,
133.171222354584));
#164023=CARTESIAN_POINT('Ctrl Pts',(-3.31631129755346,17.7406985030951,
131.677104707525));
#164024=CARTESIAN_POINT('Ctrl Pts',(-1.67239348737615,18.048,130.182987060467));
#164025=CARTESIAN_POINT('Ctrl Pts',(-2.21024254310115E-15,18.048,128.688869413408));
#164026=CARTESIAN_POINT('Ctrl Pts',(1.67239348737616,18.048,127.194751766349));
#164027=CARTESIAN_POINT('Ctrl Pts',(3.31631129755346,17.7406985030951,125.70063411929));
#164028=CARTESIAN_POINT('Ctrl Pts',(4.96022910773077,17.4333970061901,124.206516472231));
#164029=CARTESIAN_POINT('Ctrl Pts',(6.51968959134575,16.8292587962898,122.712398825173));
#164030=CARTESIAN_POINT('Ctrl Pts',(8.07915007496071,16.2251205863895,121.218281178114));
#164031=CARTESIAN_POINT('Ctrl Pts',(9.50104767561053,15.3447188656481,119.724163531055));
#164032=CARTESIAN_POINT('Ctrl Pts',(10.9229452762603,14.4643171449067,118.230045883996));
#164033=CARTESIAN_POINT('Ctrl Pts',(12.1588589765331,13.3376329379985,116.735928236937));
#164034=CARTESIAN_POINT('Ctrl Pts',(13.3947726768058,12.2109487310903,115.241810589878));
#164035=CARTESIAN_POINT('Ctrl Pts',(14.4026149179538,10.8763499173728,113.74769294282));
#164036=CARTESIAN_POINT('Ctrl Pts',(15.4104571591017,9.54175110365538,112.253575295761));
#164037=CARTESIAN_POINT('Ctrl Pts',(16.1559070823762,8.04468584505496,110.759457648702));
#164038=CARTESIAN_POINT('Ctrl Pts',(16.9013570056506,6.54762058645456,109.265340001643));
#164039=CARTESIAN_POINT('Ctrl Pts',(17.3590292079831,4.93906964482096,107.771222354584));
#164040=CARTESIAN_POINT('Ctrl Pts',(17.8167014103155,3.33051870318735,106.277104707526));
#164041=CARTESIAN_POINT('Ctrl Pts',(17.9710104137728,1.66525935159367,104.782987060467));
#164042=CARTESIAN_POINT('Ctrl Pts',(18.1253194172301,3.32956716117513E-15,
103.288869413408));
#164043=CARTESIAN_POINT('Ctrl Pts',(17.9710104137728,-1.66525935159367,
101.794751766349));
#164044=CARTESIAN_POINT('Ctrl Pts',(17.8167014103155,-3.33051870318736,
100.30063411929));
#164045=CARTESIAN_POINT('Ctrl Pts',(17.3590292079831,-4.93906964482095,
98.8065164722314));
#164046=CARTESIAN_POINT('Ctrl Pts',(16.9013570056506,-6.54762058645456,
97.3123988251725));
#164047=CARTESIAN_POINT('Ctrl Pts',(16.1559070823762,-8.04468584505497,
95.8182811781136));
#164048=CARTESIAN_POINT('Ctrl Pts',(15.4104571591017,-9.54175110365538,
94.3241635310548));
#164049=CARTESIAN_POINT('Ctrl Pts',(14.4026149179538,-10.8763499173728,
92.8300458839961));
#164050=CARTESIAN_POINT('Ctrl Pts',(13.3947726768058,-12.2109487310903,
91.3359282369372));
#164051=CARTESIAN_POINT('Ctrl Pts',(12.1588589765331,-13.3376329379985,
89.8418105898784));
#164052=CARTESIAN_POINT('Ctrl Pts',(10.9229452762603,-14.4643171449067,
88.3476929428195));
#164053=CARTESIAN_POINT('Ctrl Pts',(9.50104767561053,-15.3447188656481,
86.8535752957606));
#164054=CARTESIAN_POINT('Ctrl Pts',(8.07915007496071,-16.2251205863895,
85.359457648702));
#164055=CARTESIAN_POINT('Ctrl Pts',(6.51968959134574,-16.8292587962898,
83.8653400016432));
#164056=CARTESIAN_POINT('Ctrl Pts',(4.96022910773078,-17.4333970061901,
82.3712223545843));
#164057=CARTESIAN_POINT('Ctrl Pts',(3.31631129755346,-17.7406985030951,
80.8771047075254));
#164058=CARTESIAN_POINT('Ctrl Pts',(1.67239348737615,-18.048,79.3829870604665));
#164059=CARTESIAN_POINT('Ctrl Pts',(0.,-18.048,77.8888694134079));
#164060=CARTESIAN_POINT('Ctrl Pts',(-1.67239348737615,-18.048,76.394751766349));
#164061=CARTESIAN_POINT('Ctrl Pts',(-3.31631129755346,-17.7406985030951,
74.9006341192902));
#164062=CARTESIAN_POINT('Ctrl Pts',(-4.96022910773077,-17.4333970061901,
73.4065164722313));
#164063=CARTESIAN_POINT('Ctrl Pts',(-6.51968959134574,-16.8292587962898,
71.9123988251724));
#164064=CARTESIAN_POINT('Ctrl Pts',(-8.07915007496071,-16.2251205863895,
70.4182811781138));
#164065=CARTESIAN_POINT('Ctrl Pts',(-9.50104767561052,-15.3447188656481,
68.9241635310549));
#164066=CARTESIAN_POINT('Ctrl Pts',(-10.9229452762603,-14.4643171449067,
67.430045883996));
#164067=CARTESIAN_POINT('Ctrl Pts',(-12.1588589765331,-13.3376329379985,
65.9359282369372));
#164068=CARTESIAN_POINT('Ctrl Pts',(-13.3947726768058,-12.2109487310903,
64.4418105898783));
#164069=CARTESIAN_POINT('Ctrl Pts',(-14.4026149179538,-10.8763499173728,
62.9476929428197));
#164070=CARTESIAN_POINT('Ctrl Pts',(-15.4104571591017,-9.54175110365538,
61.4535752957608));
#164071=CARTESIAN_POINT('Ctrl Pts',(-16.1559070823762,-8.04468584505497,
59.9594576487019));
#164072=CARTESIAN_POINT('Ctrl Pts',(-16.9013570056506,-6.54762058645456,
58.4653400016431));
#164073=CARTESIAN_POINT('Ctrl Pts',(-17.3590292079831,-4.93906964482095,
56.9712223545842));
#164074=CARTESIAN_POINT('Ctrl Pts',(-17.8167014103155,-3.33051870318735,
55.4771047075255));
#164075=CARTESIAN_POINT('Ctrl Pts',(-17.9710104137728,-1.66525935159368,
53.9829870604667));
#164076=CARTESIAN_POINT('Ctrl Pts',(-18.1253194172301,-1.10985572039171E-15,
52.4888694134078));
#164077=CARTESIAN_POINT('Ctrl Pts',(-17.9710104137728,1.66525935159367,
50.9947517663489));
#164078=CARTESIAN_POINT('Ctrl Pts',(-17.8167014103155,3.33051870318735,
49.5006341192901));
#164079=CARTESIAN_POINT('Ctrl Pts',(-17.3590292079831,4.93906964482096,
48.0065164722314));
#164080=CARTESIAN_POINT('Ctrl Pts',(-16.9013570056506,6.54762058645456,
46.5123988251726));
#164081=CARTESIAN_POINT('Ctrl Pts',(-16.1559070823762,8.04468584505497,
45.0182811781137));
#164082=CARTESIAN_POINT('Ctrl Pts',(-15.4104571591017,9.54175110365538,
43.5241635310548));
#164083=CARTESIAN_POINT('Ctrl Pts',(-14.4026149179538,10.8763499173728,
42.0300458839959));
#164084=CARTESIAN_POINT('Ctrl Pts',(-13.3947726768058,12.2109487310903,
40.5359282369373));
#164085=CARTESIAN_POINT('Ctrl Pts',(-12.1588589765331,13.3376329379985,
39.0418105898784));
#164086=CARTESIAN_POINT('Ctrl Pts',(-10.9229452762603,14.4643171449067,
37.5476929428196));
#164087=CARTESIAN_POINT('Ctrl Pts',(-9.50104767561052,15.3447188656481,
36.0535752957607));
#164088=CARTESIAN_POINT('Ctrl Pts',(-8.07915007496071,16.2251205863895,
34.5594576487018));
#164089=CARTESIAN_POINT('Ctrl Pts',(-6.51968959134574,16.8292587962898,
33.0653400016432));
#164090=CARTESIAN_POINT('Ctrl Pts',(-4.96022910773078,17.4333970061901,
31.5712223545843));
#164091=CARTESIAN_POINT('Ctrl Pts',(-3.31631129755346,17.7406985030951,
30.0771047075255));
#164092=CARTESIAN_POINT('Ctrl Pts',(-1.67239348737615,18.048,28.5829870604666));
#164093=CARTESIAN_POINT('Ctrl Pts',(-2.21024254310115E-15,18.048,27.0888694134077));
#164094=CARTESIAN_POINT('Ctrl Pts',(1.67239348737616,18.048,25.5947517663491));
#164095=CARTESIAN_POINT('Ctrl Pts',(3.31631129755346,17.7406985030951,24.1006341192902));
#164096=CARTESIAN_POINT('Ctrl Pts',(4.96022910773077,17.4333970061901,22.6065164722313));
#164097=CARTESIAN_POINT('Ctrl Pts',(6.51968959134575,16.8292587962898,21.1123988251725));
#164098=CARTESIAN_POINT('Ctrl Pts',(8.07915007496071,16.2251205863895,19.6182811781136));
#164099=CARTESIAN_POINT('Ctrl Pts',(9.50104767561053,15.3447188656481,18.1241635310549));
#164100=CARTESIAN_POINT('Ctrl Pts',(10.9229452762603,14.4643171449067,16.6300458839961));
#164101=CARTESIAN_POINT('Ctrl Pts',(12.1588589765331,13.3376329379985,15.1359282369372));
#164102=CARTESIAN_POINT('Ctrl Pts',(13.3947726768058,12.2109487310903,13.6418105898783));
#164103=CARTESIAN_POINT('Ctrl Pts',(14.4026149179538,10.8763499173728,12.1476929428195));
#164104=CARTESIAN_POINT('Ctrl Pts',(15.4104571591017,9.54175110365538,10.6535752957608));
#164105=CARTESIAN_POINT('Ctrl Pts',(16.1559070823762,8.04468584505496,9.15945764870196));
#164106=CARTESIAN_POINT('Ctrl Pts',(16.9013570056506,6.54762058645456,7.6653400016431));
#164107=CARTESIAN_POINT('Ctrl Pts',(17.3590292079831,4.93906964482096,6.17122235458423));
#164108=CARTESIAN_POINT('Ctrl Pts',(17.8167014103155,3.33051870318735,4.67710470752536));
#164109=CARTESIAN_POINT('Ctrl Pts',(17.9710104137728,1.66525935159367,3.18298706046671));
#164110=CARTESIAN_POINT('Ctrl Pts',(18.1253194172301,3.32956716117513E-15,
1.68886941340785));
#164111=CARTESIAN_POINT('Ctrl Pts',(17.9710104137728,-1.66525935159367,
0.194751766348977));
#164112=CARTESIAN_POINT('Ctrl Pts',(17.8167014103155,-3.33051870318736,
-1.29936588070989));
#164113=CARTESIAN_POINT('Ctrl Pts',(17.3590292079831,-4.93906964482095,
-2.79348352776876));
#164114=CARTESIAN_POINT('Ctrl Pts',(16.9013570056506,-6.54762058645456,
-4.2876011748274));
#164115=CARTESIAN_POINT('Ctrl Pts',(16.1559070823762,-8.04468584505497,
-5.78171882188627));
#164116=CARTESIAN_POINT('Ctrl Pts',(15.4104571591017,-9.54175110365538,
-7.27583646894514));
#164117=CARTESIAN_POINT('Ctrl Pts',(14.4026149179538,-10.8763499173728,
-8.76995411600401));
#164118=CARTESIAN_POINT('Ctrl Pts',(13.3947726768058,-12.2109487310903,
-10.2640717630629));
#164119=CARTESIAN_POINT('Ctrl Pts',(12.1588589765331,-13.3376329379985,
-11.7581894101215));
#164120=CARTESIAN_POINT('Ctrl Pts',(10.9229452762603,-14.4643171449067,
-13.2523070571804));
#164121=CARTESIAN_POINT('Ctrl Pts',(9.50104767561053,-15.3447188656481,
-14.7464247042393));
#164122=CARTESIAN_POINT('Ctrl Pts',(8.07915007496071,-16.2251205863895,
-16.2405423512981));
#164123=CARTESIAN_POINT('Ctrl Pts',(6.51968959134574,-16.8292587962898,
-17.734659998357));
#164124=CARTESIAN_POINT('Ctrl Pts',(4.96022910773078,-17.4333970061901,
-19.2287776454156));
#164125=CARTESIAN_POINT('Ctrl Pts',(3.31631129755346,-17.7406985030951,
-20.7228952924745));
#164126=CARTESIAN_POINT('Ctrl Pts',(1.67239348737615,-18.048,-22.2170129395334));
#164127=CARTESIAN_POINT('Ctrl Pts',(0.,-18.048,-23.7111305865922));
#164128=CARTESIAN_POINT('Ctrl Pts',(-1.67239348737615,-18.048,-25.2052482336511));
#164129=CARTESIAN_POINT('Ctrl Pts',(-3.31631129755346,-17.7406985030951,
-26.6993658807098));
#164130=CARTESIAN_POINT('Ctrl Pts',(-4.96022910773077,-17.4333970061901,
-28.1934835277686));
#164131=CARTESIAN_POINT('Ctrl Pts',(-6.51968959134574,-16.8292587962898,
-29.6876011748275));
#164132=CARTESIAN_POINT('Ctrl Pts',(-8.07915007496071,-16.2251205863895,
-31.1817188218864));
#164133=CARTESIAN_POINT('Ctrl Pts',(-9.50104767561052,-15.3447188656481,
-32.6758364689452));
#164134=CARTESIAN_POINT('Ctrl Pts',(-10.9229452762603,-14.4643171449067,
-34.1699541160039));
#164135=CARTESIAN_POINT('Ctrl Pts',(-12.1588589765331,-13.3376329379985,
-35.6640717630627));
#164136=CARTESIAN_POINT('Ctrl Pts',(-13.3947726768058,-12.2109487310903,
-37.1581894101216));
#164137=CARTESIAN_POINT('Ctrl Pts',(-14.4026149179538,-10.8763499173728,
-38.6523070571805));
#164138=CARTESIAN_POINT('Ctrl Pts',(-15.4104571591017,-9.54175110365538,
-40.1464247042394));
#164139=CARTESIAN_POINT('Ctrl Pts',(-16.1559070823762,-8.04468584505497,
-41.640542351298));
#164140=CARTESIAN_POINT('Ctrl Pts',(-16.9013570056506,-6.54762058645456,
-43.1346599983569));
#164141=CARTESIAN_POINT('Ctrl Pts',(-17.3590292079831,-4.93906964482095,
-44.6287776454157));
#164142=CARTESIAN_POINT('Ctrl Pts',(-17.8167014103155,-3.33051870318735,
-46.1228952924746));
#164143=CARTESIAN_POINT('Ctrl Pts',(-17.9710104137728,-1.66525935159368,
-47.6170129395335));
#164144=CARTESIAN_POINT('Ctrl Pts',(-18.1253194172301,-1.10985572039171E-15,
-49.1111305865921));
#164145=CARTESIAN_POINT('Ctrl Pts',(-17.9710104137728,1.66525935159367,
-50.605248233651));
#164146=CARTESIAN_POINT('Ctrl Pts',(-17.8167014103155,3.33051870318735,
-52.0993658807098));
#164147=CARTESIAN_POINT('Ctrl Pts',(-17.3590292079831,4.93906964482096,
-53.5934835277687));
#164148=CARTESIAN_POINT('Ctrl Pts',(-16.9013570056506,6.54762058645456,
-55.0876011748276));
#164149=CARTESIAN_POINT('Ctrl Pts',(-16.1559070823762,8.04468584505497,
-56.5817188218862));
#164150=CARTESIAN_POINT('Ctrl Pts',(-15.4104571591017,9.54175110365538,
-58.0758364689451));
#164151=CARTESIAN_POINT('Ctrl Pts',(-14.4026149179538,10.8763499173728,
-59.569954116004));
#164152=CARTESIAN_POINT('Ctrl Pts',(-13.3947726768058,12.2109487310903,
-61.0640717630628));
#164153=CARTESIAN_POINT('Ctrl Pts',(-12.1588589765331,13.3376329379985,
-62.5581894101217));
#164154=CARTESIAN_POINT('Ctrl Pts',(-10.9229452762603,14.4643171449067,
-64.0523070571803));
#164155=CARTESIAN_POINT('Ctrl Pts',(-9.50104767561052,15.3447188656481,
-65.5464247042392));
#164156=CARTESIAN_POINT('Ctrl Pts',(-8.07915007496071,16.2251205863895,
-67.0405423512981));
#164157=CARTESIAN_POINT('Ctrl Pts',(-6.51968959134574,16.8292587962898,
-68.5346599983569));
#164158=CARTESIAN_POINT('Ctrl Pts',(-4.96022910773078,17.4333970061901,
-70.0287776454158));
#164159=CARTESIAN_POINT('Ctrl Pts',(-3.31631129755346,17.7406985030951,
-71.5228952924745));
#164160=CARTESIAN_POINT('Ctrl Pts',(-1.67239348737615,18.048,-73.0170129395333));
#164161=CARTESIAN_POINT('Ctrl Pts',(-2.21024254310115E-15,18.048,-74.5111305865922));
#164162=CARTESIAN_POINT('Ctrl Pts',(1.67239348737616,18.048,-76.0052482336511));
#164163=CARTESIAN_POINT('Ctrl Pts',(3.31631129755346,17.7406985030951,-77.4993658807099));
#164164=CARTESIAN_POINT('Ctrl Pts',(4.96022910773077,17.4333970061901,-78.9934835277686));
#164165=CARTESIAN_POINT('Ctrl Pts',(6.51968959134575,16.8292587962898,-80.4876011748274));
#164166=CARTESIAN_POINT('Ctrl Pts',(8.07915007496071,16.2251205863895,-81.9817188218863));
#164167=CARTESIAN_POINT('Ctrl Pts',(9.50104767561053,15.3447188656481,-83.4758364689452));
#164168=CARTESIAN_POINT('Ctrl Pts',(10.9229452762603,14.4643171449067,-84.9699541160041));
#164169=CARTESIAN_POINT('Ctrl Pts',(12.1588589765331,13.3376329379985,-86.4640717630627));
#164170=CARTESIAN_POINT('Ctrl Pts',(13.3947726768058,12.2109487310903,-87.9581894101216));
#164171=CARTESIAN_POINT('Ctrl Pts',(14.4026149179538,10.8763499173728,-89.4523070571804));
#164172=CARTESIAN_POINT('Ctrl Pts',(15.4104571591017,9.54175110365538,-90.9464247042393));
#164173=CARTESIAN_POINT('Ctrl Pts',(16.1559070823762,8.04468584505496,-92.4405423512982));
#164174=CARTESIAN_POINT('Ctrl Pts',(16.9013570056506,6.54762058645456,-93.9346599983568));
#164175=CARTESIAN_POINT('Ctrl Pts',(17.3590292079831,4.93906964482096,-95.4287776454157));
#164176=CARTESIAN_POINT('Ctrl Pts',(17.8167014103155,3.33051870318735,-96.9228952924745));
#164177=CARTESIAN_POINT('Ctrl Pts',(17.9710104137728,1.66525935159367,-98.4170129395334));
#164178=CARTESIAN_POINT('Ctrl Pts',(18.1253194172301,3.32956716117513E-15,
-99.9111305865923));
#164179=CARTESIAN_POINT('Ctrl Pts',(17.9710104137728,-1.66525935159367,
-101.405248233651));
#164180=CARTESIAN_POINT('Ctrl Pts',(17.8167014103155,-3.33051870318736,
-102.89936588071));
#164181=CARTESIAN_POINT('Ctrl Pts',(17.3590292079831,-4.93906964482095,
-104.393483527769));
#164182=CARTESIAN_POINT('Ctrl Pts',(16.9013570056506,-6.54762058645456,
-105.887601174828));
#164183=CARTESIAN_POINT('Ctrl Pts',(16.1559070823762,-8.04468584505497,
-107.381718821886));
#164184=CARTESIAN_POINT('Ctrl Pts',(15.4104571591017,-9.54175110365538,
-108.875836468945));
#164185=CARTESIAN_POINT('Ctrl Pts',(14.4026149179538,-10.8763499173728,
-110.369954116004));
#164186=CARTESIAN_POINT('Ctrl Pts',(13.3947726768058,-12.2109487310903,
-111.864071763063));
#164187=CARTESIAN_POINT('Ctrl Pts',(12.1588589765331,-13.3376329379985,
-113.358189410122));
#164188=CARTESIAN_POINT('Ctrl Pts',(10.9229452762603,-14.4643171449067,
-114.852307057181));
#164189=CARTESIAN_POINT('Ctrl Pts',(9.50104767561053,-15.3447188656481,
-116.346424704239));
#164190=CARTESIAN_POINT('Ctrl Pts',(8.07915007496071,-16.2251205863895,
-117.840542351298));
#164191=CARTESIAN_POINT('Ctrl Pts',(6.51968959134574,-16.8292587962898,
-119.334659998357));
#164192=CARTESIAN_POINT('Ctrl Pts',(4.96022910773078,-17.4333970061901,
-120.828777645416));
#164193=CARTESIAN_POINT('Ctrl Pts',(3.31631129755346,-17.7406985030951,
-122.322895292475));
#164194=CARTESIAN_POINT('Ctrl Pts',(1.67239348737615,-18.048,-123.817012939533));
#164195=CARTESIAN_POINT('Ctrl Pts',(0.,-18.048,-125.311130586592));
#164196=CARTESIAN_POINT('Ctrl Pts',(-1.67239348737615,-18.048,-126.805248233651));
#164197=CARTESIAN_POINT('Ctrl Pts',(-3.31631129755346,-17.7406985030951,
-128.29936588071));
#164198=CARTESIAN_POINT('Ctrl Pts',(-4.96022910773077,-17.4333970061901,
-129.793483527769));
#164199=CARTESIAN_POINT('Ctrl Pts',(-6.51968959134574,-16.8292587962898,
-131.287601174827));
#164200=CARTESIAN_POINT('Ctrl Pts',(-8.07915007496071,-16.2251205863895,
-132.781718821886));
#164201=CARTESIAN_POINT('Ctrl Pts',(-9.50104767561052,-15.3447188656481,
-134.275836468945));
#164202=CARTESIAN_POINT('Ctrl Pts',(-10.9229452762603,-14.4643171449067,
-135.769954116004));
#164203=CARTESIAN_POINT('Ctrl Pts',(-12.1588589765331,-13.3376329379985,
-137.264071763063));
#164204=CARTESIAN_POINT('Ctrl Pts',(-13.3947726768058,-12.2109487310903,
-138.758189410122));
#164205=CARTESIAN_POINT('Ctrl Pts',(-14.4026149179538,-10.8763499173728,
-140.25230705718));
#164206=CARTESIAN_POINT('Ctrl Pts',(-15.4104571591017,-9.54175110365538,
-141.746424704239));
#164207=CARTESIAN_POINT('Ctrl Pts',(-16.1559070823762,-8.04468584505497,
-143.240542351298));
#164208=CARTESIAN_POINT('Ctrl Pts',(-16.9013570056506,-6.54762058645456,
-144.734659998357));
#164209=CARTESIAN_POINT('Ctrl Pts',(-17.3590292079831,-4.93906964482095,
-146.228777645416));
#164210=CARTESIAN_POINT('Ctrl Pts',(-17.8167014103155,-3.33051870318735,
-147.722895292475));
#164211=CARTESIAN_POINT('Ctrl Pts',(-17.9710104137728,-1.66525935159368,
-149.217012939533));
#164212=CARTESIAN_POINT('Ctrl Pts',(-18.1253194172301,-1.10985572039171E-15,
-150.711130586592));
#164213=CARTESIAN_POINT('Ctrl Pts',(-17.9710104137728,1.66525935159367,
-152.205248233651));
#164214=CARTESIAN_POINT('Ctrl Pts',(-17.8167014103155,3.33051870318735,
-153.69936588071));
#164215=CARTESIAN_POINT('Ctrl Pts',(-17.3590292079831,4.93906964482096,
-155.193483527769));
#164216=CARTESIAN_POINT('Ctrl Pts',(-16.9013570056506,6.54762058645456,
-156.687601174828));
#164217=CARTESIAN_POINT('Ctrl Pts',(-16.1559070823762,8.04468584505497,
-158.181718821886));
#164218=CARTESIAN_POINT('Ctrl Pts',(-15.4104571591017,9.54175110365538,
-159.675836468945));
#164219=CARTESIAN_POINT('Ctrl Pts',(-14.4026149179538,10.8763499173728,
-161.169954116004));
#164220=CARTESIAN_POINT('Ctrl Pts',(-13.3947726768058,12.2109487310903,
-162.664071763063));
#164221=CARTESIAN_POINT('Ctrl Pts',(-12.1588589765331,13.3376329379985,
-164.158189410122));
#164222=CARTESIAN_POINT('Ctrl Pts',(-10.9229452762603,14.4643171449067,
-165.65230705718));
#164223=CARTESIAN_POINT('Ctrl Pts',(-9.50104767561052,15.3447188656481,
-167.146424704239));
#164224=CARTESIAN_POINT('Ctrl Pts',(-8.07915007496071,16.2251205863895,
-168.640542351298));
#164225=CARTESIAN_POINT('Ctrl Pts',(-6.51968959134574,16.8292587962898,
-170.134659998357));
#164226=CARTESIAN_POINT('Ctrl Pts',(-4.96022910773078,17.4333970061901,
-171.628777645416));
#164227=CARTESIAN_POINT('Ctrl Pts',(-3.31631129755346,17.7406985030951,
-173.122895292475));
#164228=CARTESIAN_POINT('Ctrl Pts',(-1.67239348737615,18.048,-174.617012939534));
#164229=CARTESIAN_POINT('Ctrl Pts',(-2.21024254310115E-15,18.048,-176.111130586592));
#164230=CARTESIAN_POINT('Ctrl Pts',(1.67239348737616,18.048,-177.605248233651));
#164231=CARTESIAN_POINT('Ctrl Pts',(3.31631129755346,17.7406985030951,-179.09936588071));
#164232=CARTESIAN_POINT('Ctrl Pts',(4.96022910773077,17.4333970061901,-180.593483527769));
#164233=CARTESIAN_POINT('Ctrl Pts',(6.51968959134575,16.8292587962898,-182.087601174828));
#164234=CARTESIAN_POINT('Ctrl Pts',(8.07915007496071,16.2251205863895,-183.581718821886));
#164235=CARTESIAN_POINT('Ctrl Pts',(9.50104767561053,15.3447188656481,-185.075836468945));
#164236=CARTESIAN_POINT('Ctrl Pts',(10.9229452762603,14.4643171449067,-186.569954116004));
#164237=CARTESIAN_POINT('Ctrl Pts',(12.1588589765331,13.3376329379985,-188.064071763063));
#164238=CARTESIAN_POINT('Ctrl Pts',(13.3947726768058,12.2109487310903,-189.558189410122));
#164239=CARTESIAN_POINT('Ctrl Pts',(14.4026149179538,10.8763499173728,-191.05230705718));
#164240=CARTESIAN_POINT('Ctrl Pts',(15.4104571591017,9.54175110365538,-192.546424704239));
#164241=CARTESIAN_POINT('Ctrl Pts',(16.1559070823762,8.04468584505496,-194.040542351298));
#164242=CARTESIAN_POINT('Ctrl Pts',(16.9013570056506,6.54762058645456,-195.534659998357));
#164243=CARTESIAN_POINT('Ctrl Pts',(17.3590292079831,4.93906964482096,-197.028777645416));
#164244=CARTESIAN_POINT('Ctrl Pts',(17.8167014103155,3.33051870318735,-198.522895292475));
#164245=CARTESIAN_POINT('Ctrl Pts',(17.9710104137728,1.66525935159367,-200.017012939533));
#164246=CARTESIAN_POINT('Ctrl Pts',(18.1253194172301,3.32956716117513E-15,
-201.511130586592));
#164247=CARTESIAN_POINT('Ctrl Pts',(17.9710104137728,-1.66525935159367,
-203.005248233651));
#164248=CARTESIAN_POINT('Ctrl Pts',(17.8167014103155,-3.33051870318736,
-204.49936588071));
#164249=CARTESIAN_POINT('Ctrl Pts',(17.3590292079831,-4.93906964482095,
-205.993483527769));
#164250=CARTESIAN_POINT('Ctrl Pts',(16.9013570056506,-6.54762058645456,
-207.487601174827));
#164251=CARTESIAN_POINT('Ctrl Pts',(16.1559070823762,-8.04468584505497,
-208.981718821886));
#164252=CARTESIAN_POINT('Ctrl Pts',(15.4104571591017,-9.54175110365538,
-210.475836468945));
#164253=CARTESIAN_POINT('Ctrl Pts',(14.4026149179538,-10.8763499173728,
-211.969954116004));
#164254=CARTESIAN_POINT('Ctrl Pts',(13.3947726768058,-12.2109487310903,
-213.464071763063));
#164255=CARTESIAN_POINT('Ctrl Pts',(12.1588589765331,-13.3376329379985,
-214.958189410122));
#164256=CARTESIAN_POINT('Ctrl Pts',(10.9229452762603,-14.4643171449067,
-216.45230705718));
#164257=CARTESIAN_POINT('Ctrl Pts',(9.50104767561053,-15.3447188656481,
-217.946424704239));
#164258=CARTESIAN_POINT('Ctrl Pts',(8.07915007496071,-16.2251205863895,
-219.440542351298));
#164259=CARTESIAN_POINT('Ctrl Pts',(6.51968959134574,-16.8292587962898,
-220.934659998357));
#164260=CARTESIAN_POINT('Ctrl Pts',(4.96022910773078,-17.4333970061901,
-222.428777645416));
#164261=CARTESIAN_POINT('Ctrl Pts',(3.31631129755346,-17.7406985030951,
-223.922895292475));
#164262=CARTESIAN_POINT('Ctrl Pts',(1.67239348737615,-18.048,-225.417012939533));
#164263=CARTESIAN_POINT('Ctrl Pts',(0.,-18.048,-226.911130586592));
#164264=CARTESIAN_POINT('Ctrl Pts',(-1.67239348737615,-18.048,-228.405248233651));
#164265=CARTESIAN_POINT('Ctrl Pts',(-3.31631129755346,-17.7406985030951,
-229.89936588071));
#164266=CARTESIAN_POINT('Ctrl Pts',(-4.96022910773077,-17.4333970061901,
-231.393483527769));
#164267=CARTESIAN_POINT('Ctrl Pts',(-6.51968959134574,-16.8292587962898,
-232.887601174828));
#164268=CARTESIAN_POINT('Ctrl Pts',(-8.07915007496071,-16.2251205863895,
-234.381718821886));
#164269=CARTESIAN_POINT('Ctrl Pts',(-9.50104767561052,-15.3447188656481,
-235.875836468945));
#164270=CARTESIAN_POINT('Ctrl Pts',(-10.9229452762603,-14.4643171449067,
-237.369954116004));
#164271=CARTESIAN_POINT('Ctrl Pts',(-12.1588589765331,-13.3376329379985,
-238.864071763063));
#164272=CARTESIAN_POINT('Ctrl Pts',(-13.3947726768058,-12.2109487310903,
-240.358189410122));
#164273=CARTESIAN_POINT('Ctrl Pts',(-14.4026149179538,-10.8763499173728,
-241.852307057181));
#164274=CARTESIAN_POINT('Ctrl Pts',(-15.4104571591017,-9.54175110365538,
-243.346424704239));
#164275=CARTESIAN_POINT('Ctrl Pts',(-16.1559070823762,-8.04468584505497,
-244.840542351298));
#164276=CARTESIAN_POINT('Ctrl Pts',(-16.9013570056506,-6.54762058645456,
-246.334659998357));
#164277=CARTESIAN_POINT('Ctrl Pts',(-17.3590292079831,-4.93906964482095,
-247.828777645416));
#164278=CARTESIAN_POINT('Ctrl Pts',(-17.8167014103155,-3.33051870318735,
-249.322895292475));
#164279=CARTESIAN_POINT('Ctrl Pts',(-17.9710104137728,-1.66525935159368,
-250.817012939533));
#164280=CARTESIAN_POINT('Ctrl Pts',(-18.1253194172301,-1.10985572039171E-15,
-252.311130586592));
#164281=CARTESIAN_POINT('Ctrl Pts',(-17.9710104137728,1.66525935159367,
-253.805248233651));
#164282=CARTESIAN_POINT('Ctrl Pts',(-17.8167014103155,3.33051870318735,
-255.29936588071));
#164283=CARTESIAN_POINT('Ctrl Pts',(-17.3590292079831,4.93906964482096,
-256.793483527769));
#164284=CARTESIAN_POINT('Ctrl Pts',(-16.9013570056506,6.54762058645456,
-258.287601174827));
#164285=CARTESIAN_POINT('Ctrl Pts',(-16.1559070823762,8.04468584505497,
-259.781718821886));
#164286=CARTESIAN_POINT('Ctrl Pts',(-15.4104571591017,9.54175110365538,
-261.275836468945));
#164287=CARTESIAN_POINT('Ctrl Pts',(-14.4026149179538,10.8763499173728,
-262.769954116004));
#164288=CARTESIAN_POINT('Ctrl Pts',(-13.3947726768058,12.2109487310903,
-264.264071763063));
#164289=CARTESIAN_POINT('Ctrl Pts',(-12.1588589765331,13.3376329379985,
-265.758189410122));
#164290=CARTESIAN_POINT('Ctrl Pts',(-10.9229452762603,14.4643171449067,
-267.25230705718));
#164291=CARTESIAN_POINT('Ctrl Pts',(-9.50104767561052,15.3447188656481,
-268.746424704239));
#164292=CARTESIAN_POINT('Ctrl Pts',(-8.07915007496071,16.2251205863895,
-270.240542351298));
#164293=CARTESIAN_POINT('Ctrl Pts',(-6.51968959134574,16.8292587962898,
-271.734659998357));
#164294=CARTESIAN_POINT('Ctrl Pts',(-4.96022910773078,17.4333970061901,
-273.228777645416));
#164295=CARTESIAN_POINT('Ctrl Pts',(-3.31631129755346,17.7406985030951,
-274.722895292475));
#164296=CARTESIAN_POINT('Ctrl Pts',(-1.67239348737615,18.048,-276.217012939533));
#164297=CARTESIAN_POINT('Ctrl Pts',(-2.21024254310115E-15,18.048,-277.711130586592));
#164298=CARTESIAN_POINT('Ctrl Pts',(1.67239348737616,18.048,-279.205248233651));
#164299=CARTESIAN_POINT('Ctrl Pts',(3.31631129755346,17.7406985030951,-280.69936588071));
#164300=CARTESIAN_POINT('Ctrl Pts',(4.96022910773077,17.4333970061901,-282.193483527769));
#164301=CARTESIAN_POINT('Ctrl Pts',(6.51968959134575,16.8292587962898,-283.687601174827));
#164302=CARTESIAN_POINT('Ctrl Pts',(8.07915007496071,16.2251205863895,-285.181718821886));
#164303=CARTESIAN_POINT('Ctrl Pts',(9.50104767561053,15.3447188656481,-286.675836468945));
#164304=CARTESIAN_POINT('Ctrl Pts',(10.9229452762603,14.4643171449067,-288.169954116004));
#164305=CARTESIAN_POINT('Ctrl Pts',(12.1588589765331,13.3376329379985,-289.664071763063));
#164306=CARTESIAN_POINT('Ctrl Pts',(13.3947726768058,12.2109487310903,-291.158189410122));
#164307=CARTESIAN_POINT('Ctrl Pts',(14.4026149179538,10.8763499173728,-292.652307057181));
#164308=CARTESIAN_POINT('Ctrl Pts',(15.4104571591017,9.54175110365538,-294.146424704239));
#164309=CARTESIAN_POINT('Ctrl Pts',(16.1559070823762,8.04468584505496,-295.640542351298));
#164310=CARTESIAN_POINT('Ctrl Pts',(16.9013570056506,6.54762058645456,-297.134659998357));
#164311=CARTESIAN_POINT('Ctrl Pts',(17.3590292079831,4.93906964482096,-298.628777645416));
#164312=CARTESIAN_POINT('Ctrl Pts',(17.8167014103155,3.33051870318735,-300.122895292475));
#164313=CARTESIAN_POINT('Ctrl Pts',(17.9710104137728,1.66525935159367,-301.617012939533));
#164314=CARTESIAN_POINT('Ctrl Pts',(18.1253194172301,3.32956716117513E-15,
-303.111130586592));
#164315=CARTESIAN_POINT('Ctrl Pts',(17.9710104137728,-1.66525935159367,
-304.605248233651));
#164316=CARTESIAN_POINT('Ctrl Pts',(17.8167014103155,-3.33051870318736,
-306.09936588071));
#164317=CARTESIAN_POINT('Ctrl Pts',(17.3590292079831,-4.93906964482095,
-307.593483527769));
#164318=CARTESIAN_POINT('Ctrl Pts',(16.9013570056506,-6.54762058645456,
-309.087601174828));
#164319=CARTESIAN_POINT('Ctrl Pts',(16.1559070823762,-8.04468584505497,
-310.581718821886));
#164320=CARTESIAN_POINT('Ctrl Pts',(15.4104571591017,-9.54175110365538,
-312.075836468945));
#164321=CARTESIAN_POINT('Ctrl Pts',(14.4026149179538,-10.8763499173728,
-313.569954116004));
#164322=CARTESIAN_POINT('Ctrl Pts',(13.3947726768058,-12.2109487310903,
-315.064071763063));
#164323=CARTESIAN_POINT('Ctrl Pts',(12.1588589765331,-13.3376329379985,
-316.558189410122));
#164324=CARTESIAN_POINT('Ctrl Pts',(10.9229452762603,-14.4643171449067,
-318.05230705718));
#164325=CARTESIAN_POINT('Ctrl Pts',(9.50104767561053,-15.3447188656481,
-319.546424704239));
#164326=CARTESIAN_POINT('Ctrl Pts',(8.07915007496071,-16.2251205863895,
-321.040542351298));
#164327=CARTESIAN_POINT('Ctrl Pts',(6.51968959134574,-16.8292587962898,
-322.534659998357));
#164328=CARTESIAN_POINT('Ctrl Pts',(4.96022910773078,-17.4333970061901,
-324.028777645416));
#164329=CARTESIAN_POINT('Ctrl Pts',(3.31631129755346,-17.7406985030951,
-325.522895292474));
#164330=CARTESIAN_POINT('Ctrl Pts',(1.67239348737615,-18.048,-327.017012939533));
#164331=CARTESIAN_POINT('Ctrl Pts',(0.,-18.048,-328.511130586592));
#164332=CARTESIAN_POINT('Ctrl Pts',(-1.67239348737615,-18.048,-330.005248233651));
#164333=CARTESIAN_POINT('Ctrl Pts',(-3.31631129755346,-17.7406985030951,
-331.49936588071));
#164334=CARTESIAN_POINT('Ctrl Pts',(-4.96022910773077,-17.4333970061901,
-332.993483527769));
#164335=CARTESIAN_POINT('Ctrl Pts',(-6.51968959134574,-16.8292587962898,
-334.487601174827));
#164336=CARTESIAN_POINT('Ctrl Pts',(-8.07915007496071,-16.2251205863895,
-335.981718821886));
#164337=CARTESIAN_POINT('Ctrl Pts',(-9.50104767561052,-15.3447188656481,
-337.475836468945));
#164338=CARTESIAN_POINT('Ctrl Pts',(-10.9229452762603,-14.4643171449067,
-338.969954116004));
#164339=CARTESIAN_POINT('Ctrl Pts',(-12.1588589765331,-13.3376329379985,
-340.464071763063));
#164340=CARTESIAN_POINT('Ctrl Pts',(-13.3947726768058,-12.2109487310903,
-341.958189410122));
#164341=CARTESIAN_POINT('Ctrl Pts',(-14.4026149179538,-10.8763499173728,
-343.45230705718));
#164342=CARTESIAN_POINT('Ctrl Pts',(-15.4104571591017,-9.54175110365538,
-344.946424704239));
#164343=CARTESIAN_POINT('Ctrl Pts',(-16.1559070823762,-8.04468584505497,
-346.440542351298));
#164344=CARTESIAN_POINT('Ctrl Pts',(-16.9013570056506,-6.54762058645456,
-347.934659998357));
#164345=CARTESIAN_POINT('Ctrl Pts',(-17.3590292079831,-4.93906964482095,
-349.428777645416));
#164346=CARTESIAN_POINT('Ctrl Pts',(-17.8167014103155,-3.33051870318735,
-350.922895292475));
#164347=CARTESIAN_POINT('Ctrl Pts',(-17.9710104137728,-1.66525935159368,
-352.417012939533));
#164348=CARTESIAN_POINT('Ctrl Pts',(-18.1253194172301,-1.10985572039171E-15,
-353.911130586592));
#164349=CARTESIAN_POINT('Ctrl Pts',(-17.9710104137728,1.66525935159367,
-355.405248233651));
#164350=CARTESIAN_POINT('Ctrl Pts',(-17.8167014103155,3.33051870318735,
-356.89936588071));
#164351=CARTESIAN_POINT('Ctrl Pts',(-17.3590292079831,4.93906964482096,
-358.393483527769));
#164352=CARTESIAN_POINT('Ctrl Pts',(-16.9013570056506,6.54762058645456,
-359.887601174828));
#164353=CARTESIAN_POINT('Ctrl Pts',(-16.1559070823762,8.04468584505497,
-361.381718821886));
#164354=CARTESIAN_POINT('Ctrl Pts',(-15.4104571591017,9.54175110365538,
-362.875836468945));
#164355=CARTESIAN_POINT('Ctrl Pts',(-14.4026149179538,10.8763499173728,
-364.369954116004));
#164356=CARTESIAN_POINT('Ctrl Pts',(-13.3947726768058,12.2109487310903,
-365.864071763063));
#164357=CARTESIAN_POINT('Ctrl Pts',(-12.1588589765331,13.3376329379985,
-367.358189410122));
#164358=CARTESIAN_POINT('Ctrl Pts',(-10.9229452762603,14.4643171449067,
-368.85230705718));
#164359=CARTESIAN_POINT('Ctrl Pts',(-9.50104767561052,15.3447188656481,
-370.346424704239));
#164360=CARTESIAN_POINT('Ctrl Pts',(-8.07915007496071,16.2251205863895,
-371.840542351298));
#164361=CARTESIAN_POINT('Ctrl Pts',(-6.51968959134574,16.8292587962898,
-373.334659998357));
#164362=CARTESIAN_POINT('Ctrl Pts',(-4.96022910773078,17.4333970061901,
-374.828777645416));
#164363=CARTESIAN_POINT('Ctrl Pts',(-3.31631129755346,17.7406985030951,
-376.322895292475));
#164364=CARTESIAN_POINT('Ctrl Pts',(-1.67239348737615,18.048,-377.817012939533));
#164365=CARTESIAN_POINT('Ctrl Pts',(-2.21024254310115E-15,18.048,-379.311130586592));
#164366=CARTESIAN_POINT('Ctrl Pts',(1.67239348737616,18.048,-380.805248233651));
#164367=CARTESIAN_POINT('Ctrl Pts',(3.31631129755346,17.7406985030951,-382.29936588071));
#164368=CARTESIAN_POINT('Ctrl Pts',(4.96022910773077,17.4333970061901,-383.793483527769));
#164369=CARTESIAN_POINT('Ctrl Pts',(6.51968959134575,16.8292587962898,-385.287601174827));
#164370=CARTESIAN_POINT('Ctrl Pts',(8.07915007496071,16.2251205863895,-386.781718821886));
#164371=CARTESIAN_POINT('Ctrl Pts',(9.50104767561053,15.3447188656481,-388.275836468945));
#164372=CARTESIAN_POINT('Ctrl Pts',(10.9229452762603,14.4643171449067,-389.769954116004));
#164373=CARTESIAN_POINT('Ctrl Pts',(12.1588589765331,13.3376329379985,-391.264071763063));
#164374=CARTESIAN_POINT('Ctrl Pts',(13.3947726768058,12.2109487310903,-392.758189410122));
#164375=CARTESIAN_POINT('Ctrl Pts',(14.4026149179538,10.8763499173728,-394.25230705718));
#164376=CARTESIAN_POINT('Ctrl Pts',(15.4104571591017,9.54175110365538,-395.746424704239));
#164377=CARTESIAN_POINT('Ctrl Pts',(16.1559070823762,8.04468584505496,-397.240542351298));
#164378=CARTESIAN_POINT('Ctrl Pts',(16.9013570056506,6.54762058645456,-398.734659998357));
#164379=CARTESIAN_POINT('Ctrl Pts',(17.3590292079831,4.93906964482096,-400.228777645416));
#164380=CARTESIAN_POINT('Ctrl Pts',(17.8167014103155,3.33051870318735,-401.722895292475));
#164381=CARTESIAN_POINT('Ctrl Pts',(17.9710104137728,1.66525935159367,-403.217012939533));
#164382=CARTESIAN_POINT('Ctrl Pts',(18.1253194172301,3.32956716117513E-15,
-404.711130586592));
#164383=CARTESIAN_POINT('Ctrl Pts',(17.9710104137728,-1.66525935159367,
-406.205248233651));
#164384=CARTESIAN_POINT('Ctrl Pts',(17.8167014103155,-3.33051870318736,
-407.69936588071));
#164385=CARTESIAN_POINT('Ctrl Pts',(17.3590292079831,-4.93906964482095,
-409.193483527769));
#164386=CARTESIAN_POINT('Ctrl Pts',(16.9013570056506,-6.54762058645456,
-410.687601174828));
#164387=CARTESIAN_POINT('Ctrl Pts',(16.1559070823762,-8.04468584505497,
-412.181718821886));
#164388=CARTESIAN_POINT('Ctrl Pts',(15.4104571591017,-9.54175110365538,
-413.675836468945));
#164389=CARTESIAN_POINT('Ctrl Pts',(14.4026149179538,-10.8763499173728,
-415.169954116004));
#164390=CARTESIAN_POINT('Ctrl Pts',(13.3947726768058,-12.2109487310903,
-416.664071763063));
#164391=CARTESIAN_POINT('Ctrl Pts',(12.1588589765331,-13.3376329379985,
-418.158189410122));
#164392=CARTESIAN_POINT('Ctrl Pts',(10.9229452762603,-14.4643171449067,
-419.652307057181));
#164393=CARTESIAN_POINT('Ctrl Pts',(9.50104767561053,-15.3447188656481,
-421.146424704239));
#164394=CARTESIAN_POINT('Ctrl Pts',(8.07915007496071,-16.2251205863895,
-422.640542351298));
#164395=CARTESIAN_POINT('Ctrl Pts',(6.51968959134574,-16.8292587962898,
-424.134659998357));
#164396=CARTESIAN_POINT('Ctrl Pts',(4.96022910773078,-17.4333970061901,
-425.628777645416));
#164397=CARTESIAN_POINT('Ctrl Pts',(3.31631129755346,-17.7406985030951,
-427.122895292475));
#164398=CARTESIAN_POINT('Ctrl Pts',(1.67239348737615,-18.048,-428.617012939534));
#164399=CARTESIAN_POINT('Ctrl Pts',(0.,-18.048,-430.111130586592));
#164400=CARTESIAN_POINT('Ctrl Pts',(-1.67239348737615,-18.048,-431.605248233651));
#164401=CARTESIAN_POINT('Ctrl Pts',(-3.31631129755346,-17.7406985030951,
-433.09936588071));
#164402=CARTESIAN_POINT('Ctrl Pts',(-4.96022910773077,-17.4333970061901,
-434.593483527769));
#164403=CARTESIAN_POINT('Ctrl Pts',(-6.51968959134574,-16.8292587962898,
-436.087601174828));
#164404=CARTESIAN_POINT('Ctrl Pts',(-8.07915007496071,-16.2251205863895,
-437.581718821886));
#164405=CARTESIAN_POINT('Ctrl Pts',(-9.50104767561052,-15.3447188656481,
-439.075836468945));
#164406=CARTESIAN_POINT('Ctrl Pts',(-10.9229452762603,-14.4643171449067,
-440.569954116004));
#164407=CARTESIAN_POINT('Ctrl Pts',(-12.1588589765331,-13.3376329379985,
-442.064071763063));
#164408=CARTESIAN_POINT('Ctrl Pts',(-13.3947726768058,-12.2109487310903,
-443.558189410122));
#164409=CARTESIAN_POINT('Ctrl Pts',(-14.4026149179538,-10.8763499173728,
-445.05230705718));
#164410=CARTESIAN_POINT('Ctrl Pts',(-15.4104571591017,-9.54175110365538,
-446.546424704239));
#164411=CARTESIAN_POINT('Ctrl Pts',(-16.1559070823762,-8.04468584505497,
-448.040542351298));
#164412=CARTESIAN_POINT('Ctrl Pts',(-16.9013570056506,-6.54762058645456,
-449.534659998357));
#164413=CARTESIAN_POINT('Ctrl Pts',(-17.3590292079831,-4.93906964482095,
-451.028777645416));
#164414=CARTESIAN_POINT('Ctrl Pts',(-17.8167014103155,-3.33051870318735,
-452.522895292475));
#164415=CARTESIAN_POINT('Ctrl Pts',(-17.9710104137728,-1.66525935159368,
-454.017012939533));
#164416=CARTESIAN_POINT('Ctrl Pts',(-18.1253194172301,-1.10985572039171E-15,
-455.511130586592));
#164417=CARTESIAN_POINT('Ctrl Pts',(-17.9710104137728,1.66525935159367,
-457.005248233651));
#164418=CARTESIAN_POINT('Ctrl Pts',(-17.8167014103155,3.33051870318735,
-458.49936588071));
#164419=CARTESIAN_POINT('Ctrl Pts',(-17.3590292079831,4.93906964482096,
-459.993483527769));
#164420=CARTESIAN_POINT('Ctrl Pts',(-16.9013570056506,6.54762058645456,
-461.487601174828));
#164421=CARTESIAN_POINT('Ctrl Pts',(-16.1559070823762,8.04468584505497,
-462.981718821886));
#164422=CARTESIAN_POINT('Ctrl Pts',(-15.4104571591017,9.54175110365538,
-464.475836468945));
#164423=CARTESIAN_POINT('Ctrl Pts',(-14.4026149179538,10.8763499173728,
-465.969954116004));
#164424=CARTESIAN_POINT('Ctrl Pts',(-13.3947726768058,12.2109487310903,
-467.464071763063));
#164425=CARTESIAN_POINT('Ctrl Pts',(-12.1588589765331,13.3376329379985,
-468.958189410122));
#164426=CARTESIAN_POINT('Ctrl Pts',(-10.9229452762603,14.4643171449067,
-470.45230705718));
#164427=CARTESIAN_POINT('Ctrl Pts',(-9.50104767561052,15.3447188656481,
-471.946424704239));
#164428=CARTESIAN_POINT('Ctrl Pts',(-8.07915007496071,16.2251205863895,
-473.440542351298));
#164429=CARTESIAN_POINT('Ctrl Pts',(-6.51968959134574,16.8292587962898,
-474.934659998357));
#164430=CARTESIAN_POINT('Ctrl Pts',(-4.96022910773078,17.4333970061901,
-476.428777645416));
#164431=CARTESIAN_POINT('Ctrl Pts',(-3.31631129755346,17.7406985030951,
-477.922895292475));
#164432=CARTESIAN_POINT('Ctrl Pts',(-1.67239348737615,18.048,-479.417012939533));
#164433=CARTESIAN_POINT('Ctrl Pts',(-2.21024254310115E-15,18.048,-480.911130586592));
#164434=CARTESIAN_POINT('Ctrl Pts',(1.67239348737616,18.048,-482.405248233651));
#164435=CARTESIAN_POINT('Ctrl Pts',(3.31631129755346,17.7406985030951,-483.89936588071));
#164436=CARTESIAN_POINT('Ctrl Pts',(4.96022910773077,17.4333970061901,-485.393483527769));
#164437=CARTESIAN_POINT('Ctrl Pts',(6.51968959134575,16.8292587962898,-486.887601174828));
#164438=CARTESIAN_POINT('Ctrl Pts',(8.07915007496071,16.2251205863895,-488.381718821887));
#164439=CARTESIAN_POINT('Ctrl Pts',(9.50104767561053,15.3447188656481,-489.875836468945));
#164440=CARTESIAN_POINT('Ctrl Pts',(10.9229452762603,14.4643171449067,-491.369954116004));
#164441=CARTESIAN_POINT('Ctrl Pts',(12.1588589765331,13.3376329379985,-492.864071763063));
#164442=CARTESIAN_POINT('Ctrl Pts',(13.3947726768058,12.2109487310903,-494.358189410122));
#164443=CARTESIAN_POINT('Ctrl Pts',(14.4026149179538,10.8763499173728,-495.852307057181));
#164444=CARTESIAN_POINT('Ctrl Pts',(15.4104571591017,9.54175110365538,-497.346424704239));
#164445=CARTESIAN_POINT('Ctrl Pts',(16.1559070823762,8.04468584505496,-498.840542351298));
#164446=CARTESIAN_POINT('Ctrl Pts',(16.9013570056506,6.54762058645456,-500.334659998357));
#164447=CARTESIAN_POINT('Ctrl Pts',(17.3590292079831,4.93906964482096,-501.828777645416));
#164448=CARTESIAN_POINT('Ctrl Pts',(17.8167014103155,3.33051870318735,-503.322895292475));
#164449=CARTESIAN_POINT('Ctrl Pts',(17.9710104137728,1.66525935159367,-504.817012939534));
#164450=CARTESIAN_POINT('Ctrl Pts',(18.1253194172301,3.32956716117513E-15,
-506.311130586592));
#164451=CARTESIAN_POINT('Ctrl Pts',(17.9710104137728,-1.66525935159367,
-507.805248233651));
#164452=CARTESIAN_POINT('Ctrl Pts',(17.8167014103155,-3.33051870318736,
-509.29936588071));
#164453=CARTESIAN_POINT('Ctrl Pts',(17.3590292079831,-4.93906964482095,
-510.793483527769));
#164454=CARTESIAN_POINT('Ctrl Pts',(16.9013570056506,-6.54762058645456,
-512.287601174828));
#164455=CARTESIAN_POINT('Ctrl Pts',(16.1559070823762,-8.04468584505497,
-513.781718821886));
#164456=CARTESIAN_POINT('Ctrl Pts',(15.4104571591017,-9.54175110365538,
-515.275836468945));
#164457=CARTESIAN_POINT('Ctrl Pts',(14.4026149179538,-10.8763499173728,
-516.769954116004));
#164458=CARTESIAN_POINT('Ctrl Pts',(13.3947726768058,-12.2109487310903,
-518.264071763063));
#164459=CARTESIAN_POINT('Ctrl Pts',(12.1588589765331,-13.3376329379985,
-519.758189410122));
#164460=CARTESIAN_POINT('Ctrl Pts',(10.9229452762603,-14.4643171449067,
-521.252307057181));
#164461=CARTESIAN_POINT('Ctrl Pts',(9.50104767561053,-15.3447188656481,
-522.746424704239));
#164462=CARTESIAN_POINT('Ctrl Pts',(8.07915007496071,-16.2251205863895,
-524.240542351298));
#164463=CARTESIAN_POINT('Ctrl Pts',(6.51968959134574,-16.8292587962898,
-525.734659998357));
#164464=CARTESIAN_POINT('Ctrl Pts',(4.96022910773078,-17.4333970061901,
-527.228777645416));
#164465=CARTESIAN_POINT('Ctrl Pts',(3.31631129755346,-17.7406985030951,
-528.722895292475));
#164466=CARTESIAN_POINT('Ctrl Pts',(1.67239348737615,-18.048,-530.217012939533));
#164467=CARTESIAN_POINT('Ctrl Pts',(0.,-18.048,-531.711130586592));
#164468=CARTESIAN_POINT('Ctrl Pts',(-1.67239348737615,-18.048,-533.205248233651));
#164469=CARTESIAN_POINT('Ctrl Pts',(-3.31631129755346,-17.7406985030951,
-534.69936588071));
#164470=CARTESIAN_POINT('Ctrl Pts',(-4.96022910773077,-17.4333970061901,
-536.193483527769));
#164471=CARTESIAN_POINT('Ctrl Pts',(-6.51968959134574,-16.8292587962898,
-537.687601174827));
#164472=CARTESIAN_POINT('Ctrl Pts',(-8.07915007496071,-16.2251205863895,
-539.181718821886));
#164473=CARTESIAN_POINT('Ctrl Pts',(-9.50104767561052,-15.3447188656481,
-540.675836468945));
#164474=CARTESIAN_POINT('Ctrl Pts',(-10.9229452762603,-14.4643171449067,
-542.169954116004));
#164475=CARTESIAN_POINT('Ctrl Pts',(-12.1588589765331,-13.3376329379985,
-543.664071763063));
#164476=CARTESIAN_POINT('Ctrl Pts',(-13.3947726768058,-12.2109487310903,
-545.158189410122));
#164477=CARTESIAN_POINT('Ctrl Pts',(-14.4026149179538,-10.8763499173728,
-546.65230705718));
#164478=CARTESIAN_POINT('Ctrl Pts',(-15.4104571591017,-9.54175110365538,
-548.14642470424));
#164479=CARTESIAN_POINT('Ctrl Pts',(-16.1559070823762,-8.04468584505497,
-549.640542351298));
#164480=CARTESIAN_POINT('Ctrl Pts',(-16.9013570056506,-6.54762058645456,
-551.134659998357));
#164481=CARTESIAN_POINT('Ctrl Pts',(-17.3590292079831,-4.93906964482095,
-552.628777645416));
#164482=CARTESIAN_POINT('Ctrl Pts',(-17.8167014103155,-3.33051870318735,
-554.122895292474));
#164483=CARTESIAN_POINT('Ctrl Pts',(-17.9710104137728,-1.66525935159368,
-555.617012939533));
#164484=CARTESIAN_POINT('Ctrl Pts',(-18.1253194172301,-1.10985572039171E-15,
-557.111130586592));
#164485=CARTESIAN_POINT('Ctrl Pts',(-17.9710104137728,1.66525935159367,
-558.605248233651));
#164486=CARTESIAN_POINT('Ctrl Pts',(-17.8167014103155,3.33051870318735,
-560.09936588071));
#164487=CARTESIAN_POINT('Ctrl Pts',(-17.3590292079831,4.93906964482096,
-561.593483527769));
#164488=CARTESIAN_POINT('Ctrl Pts',(-16.9013570056506,6.54762058645456,
-563.087601174828));
#164489=CARTESIAN_POINT('Ctrl Pts',(-16.1559070823762,8.04468584505497,
-564.581718821887));
#164490=CARTESIAN_POINT('Ctrl Pts',(-15.4104571591017,9.54175110365538,
-566.075836468945));
#164491=CARTESIAN_POINT('Ctrl Pts',(-14.4026149179538,10.8763499173728,
-567.569954116004));
#164492=CARTESIAN_POINT('Ctrl Pts',(-13.3947726768058,12.2109487310903,
-569.064071763063));
#164493=CARTESIAN_POINT('Ctrl Pts',(-12.1588589765331,13.3376329379985,
-570.558189410121));
#164494=CARTESIAN_POINT('Ctrl Pts',(-10.9229452762603,14.4643171449067,
-572.05230705718));
#164495=CARTESIAN_POINT('Ctrl Pts',(-9.50104767561052,15.3447188656481,
-573.546424704239));
#164496=CARTESIAN_POINT('Ctrl Pts',(-8.07915007496071,16.2251205863895,
-575.040542351298));
#164497=CARTESIAN_POINT('Ctrl Pts',(-6.51968959134574,16.8292587962898,
-576.534659998357));
#164498=CARTESIAN_POINT('Ctrl Pts',(-4.96022910773078,17.4333970061901,
-578.028777645416));
#164499=CARTESIAN_POINT('Ctrl Pts',(-3.31631129755346,17.7406985030951,
-579.522895292475));
#164500=CARTESIAN_POINT('Ctrl Pts',(-1.67239348737615,18.048,-581.017012939534));
#164501=CARTESIAN_POINT('Ctrl Pts',(-2.21024254310115E-15,18.048,-582.511130586592));
#164502=CARTESIAN_POINT('Ctrl Pts',(1.67239348737616,18.048,-584.005248233651));
#164503=CARTESIAN_POINT('Ctrl Pts',(3.31631129755346,17.7406985030951,-585.49936588071));
#164504=CARTESIAN_POINT('Ctrl Pts',(4.96022910773077,17.4333970061901,-586.993483527769));
#164505=CARTESIAN_POINT('Ctrl Pts',(6.51968959134575,16.8292587962898,-588.487601174827));
#164506=CARTESIAN_POINT('Ctrl Pts',(8.07915007496071,16.2251205863895,-589.981718821886));
#164507=CARTESIAN_POINT('Ctrl Pts',(9.50104767561053,15.3447188656481,-591.475836468945));
#164508=CARTESIAN_POINT('Ctrl Pts',(10.9229452762603,14.4643171449067,-592.969954116004));
#164509=CARTESIAN_POINT('Ctrl Pts',(12.1588589765331,13.3376329379985,-594.464071763063));
#164510=CARTESIAN_POINT('Ctrl Pts',(13.3947726768058,12.2109487310903,-595.958189410122));
#164511=CARTESIAN_POINT('Ctrl Pts',(14.4026149179538,10.8763499173728,-597.45230705718));
#164512=CARTESIAN_POINT('Ctrl Pts',(15.4104571591017,9.54175110365538,-598.946424704239));
#164513=CARTESIAN_POINT('Ctrl Pts',(16.1559070823762,8.04468584505496,-600.440542351298));
#164514=CARTESIAN_POINT('Ctrl Pts',(16.9013570056506,6.54762058645456,-601.934659998357));
#164515=CARTESIAN_POINT('Ctrl Pts',(17.3590292079831,4.93906964482096,-603.428777645416));
#164516=CARTESIAN_POINT('Ctrl Pts',(17.8167014103155,3.33051870318735,-604.922895292475));
#164517=CARTESIAN_POINT('Ctrl Pts',(17.9710104137728,1.66525935159367,-606.417012939533));
#164518=CARTESIAN_POINT('Ctrl Pts',(18.1253194172301,3.32956716117513E-15,
-607.911130586592));
#164519=CARTESIAN_POINT('Ctrl Pts',(17.9710104137728,-1.66525935159367,
-609.405248233651));
#164520=CARTESIAN_POINT('Ctrl Pts',(17.8167014103155,-3.33051870318736,
-610.89936588071));
#164521=CARTESIAN_POINT('Ctrl Pts',(17.3590292079831,-4.93906964482095,
-612.393483527768));
#164522=CARTESIAN_POINT('Ctrl Pts',(16.9013570056506,-6.54762058645456,
-613.887601174828));
#164523=CARTESIAN_POINT('Ctrl Pts',(16.1559070823762,-8.04468584505497,
-615.381718821886));
#164524=CARTESIAN_POINT('Ctrl Pts',(15.4104571591017,-9.54175110365538,
-616.875836468945));
#164525=CARTESIAN_POINT('Ctrl Pts',(14.4026149179538,-10.8763499173728,
-618.369954116004));
#164526=CARTESIAN_POINT('Ctrl Pts',(13.3947726768058,-12.2109487310903,
-619.864071763063));
#164527=CARTESIAN_POINT('Ctrl Pts',(12.1588589765331,-13.3376329379985,
-621.358189410122));
#164528=CARTESIAN_POINT('Ctrl Pts',(10.9229452762603,-14.4643171449067,
-622.852307057181));
#164529=CARTESIAN_POINT('Ctrl Pts',(9.50104767561053,-15.3447188656481,
-624.346424704239));
#164530=CARTESIAN_POINT('Ctrl Pts',(8.07915007496071,-16.2251205863895,
-625.840542351298));
#164531=CARTESIAN_POINT('Ctrl Pts',(6.51968959134574,-16.8292587962898,
-627.334659998357));
#164532=CARTESIAN_POINT('Ctrl Pts',(4.96022910773078,-17.4333970061901,
-628.828777645416));
#164533=CARTESIAN_POINT('Ctrl Pts',(3.31631129755346,-17.7406985030951,
-630.322895292474));
#164534=CARTESIAN_POINT('Ctrl Pts',(1.67239348737615,-18.048,-631.817012939533));
#164535=CARTESIAN_POINT('Ctrl Pts',(0.,-18.048,-633.311130586592));
#164536=CARTESIAN_POINT('Ctrl Pts',(-1.67239348737615,-18.048,-634.805248233651));
#164537=CARTESIAN_POINT('Ctrl Pts',(-3.31631129755346,-17.7406985030951,
-636.29936588071));
#164538=CARTESIAN_POINT('Ctrl Pts',(-4.96022910773077,-17.4333970061901,
-637.793483527769));
#164539=CARTESIAN_POINT('Ctrl Pts',(-6.51968959134574,-16.8292587962898,
-639.287601174828));
#164540=CARTESIAN_POINT('Ctrl Pts',(-8.07915007496071,-16.2251205863895,
-640.781718821886));
#164541=CARTESIAN_POINT('Ctrl Pts',(-9.50104767561052,-15.3447188656481,
-642.275836468945));
#164542=CARTESIAN_POINT('Ctrl Pts',(-10.9229452762603,-14.4643171449067,
-643.769954116004));
#164543=CARTESIAN_POINT('Ctrl Pts',(-12.1588589765331,-13.3376329379985,
-645.264071763063));
#164544=CARTESIAN_POINT('Ctrl Pts',(-13.3947726768058,-12.2109487310903,
-646.758189410122));
#164545=CARTESIAN_POINT('Ctrl Pts',(-14.4026149179538,-10.8763499173728,
-648.25230705718));
#164546=CARTESIAN_POINT('Ctrl Pts',(-15.4104571591017,-9.54175110365538,
-649.746424704239));
#164547=CARTESIAN_POINT('Ctrl Pts',(-16.1559070823762,-8.04468584505497,
-651.240542351298));
#164548=CARTESIAN_POINT('Ctrl Pts',(-16.9013570056506,-6.54762058645456,
-652.734659998357));
#164549=CARTESIAN_POINT('Ctrl Pts',(-17.3590292079831,-4.93906964482095,
-654.228777645416));
#164550=CARTESIAN_POINT('Ctrl Pts',(-17.8167014103155,-3.33051870318735,
-655.722895292475));
#164551=CARTESIAN_POINT('Ctrl Pts',(-17.9710104137728,-1.66525935159368,
-657.217012939533));
#164552=CARTESIAN_POINT('Ctrl Pts',(-18.1253194172301,-1.10985572039171E-15,
-658.711130586592));
#164553=CARTESIAN_POINT('Ctrl Pts',(-17.9710104137728,1.66525935159367,
-660.205248233651));
#164554=CARTESIAN_POINT('Ctrl Pts',(-17.8167014103155,3.33051870318735,
-661.69936588071));
#164555=CARTESIAN_POINT('Ctrl Pts',(-17.3590292079831,4.93906964482096,
-663.193483527769));
#164556=CARTESIAN_POINT('Ctrl Pts',(-16.9013570056506,6.54762058645456,
-664.687601174827));
#164557=CARTESIAN_POINT('Ctrl Pts',(-16.1559070823762,8.04468584505497,
-666.181718821887));
#164558=CARTESIAN_POINT('Ctrl Pts',(-15.4104571591017,9.54175110365538,
-667.675836468945));
#164559=CARTESIAN_POINT('Ctrl Pts',(-14.4026149179538,10.8763499173728,
-669.169954116004));
#164560=CARTESIAN_POINT('Ctrl Pts',(-13.3947726768058,12.2109487310903,
-670.664071763063));
#164561=CARTESIAN_POINT('Ctrl Pts',(-12.1588589765331,13.3376329379985,
-672.158189410121));
#164562=CARTESIAN_POINT('Ctrl Pts',(-10.9229452762603,14.4643171449067,
-673.65230705718));
#164563=CARTESIAN_POINT('Ctrl Pts',(-9.50104767561052,15.3447188656481,
-675.146424704239));
#164564=CARTESIAN_POINT('Ctrl Pts',(-8.07915007496071,16.2251205863895,
-676.640542351298));
#164565=CARTESIAN_POINT('Ctrl Pts',(-6.51968959134574,16.8292587962898,
-678.134659998357));
#164566=CARTESIAN_POINT('Ctrl Pts',(-4.96022910773078,17.4333970061901,
-679.628777645416));
#164567=CARTESIAN_POINT('Ctrl Pts',(-3.31631129755346,17.7406985030951,
-681.122895292475));
#164568=CARTESIAN_POINT('Ctrl Pts',(-1.67239348737615,18.048,-682.617012939534));
#164569=CARTESIAN_POINT('Ctrl Pts',(-2.21024254310115E-15,18.048,-684.111130586592));
#164570=CARTESIAN_POINT('Ctrl Pts',(1.67239348737616,18.048,-685.605248233651));
#164571=CARTESIAN_POINT('Ctrl Pts',(3.31631129755346,17.7406985030951,-687.09936588071));
#164572=CARTESIAN_POINT('Ctrl Pts',(4.96022910773077,17.4333970061901,-688.593483527769));
#164573=CARTESIAN_POINT('Ctrl Pts',(6.51968959134575,16.8292587962898,-690.087601174827));
#164574=CARTESIAN_POINT('Ctrl Pts',(8.07915007496071,16.2251205863895,-691.581718821886));
#164575=CARTESIAN_POINT('Ctrl Pts',(9.50104767561053,15.3447188656481,-693.075836468945));
#164576=CARTESIAN_POINT('Ctrl Pts',(10.9229452762603,14.4643171449067,-694.569954116004));
#164577=CARTESIAN_POINT('Ctrl Pts',(12.1588589765331,13.3376329379985,-696.064071763063));
#164578=CARTESIAN_POINT('Ctrl Pts',(13.3947726768058,12.2109487310903,-697.558189410122));
#164579=CARTESIAN_POINT('Ctrl Pts',(14.4026149179538,10.8763499173728,-699.052307057181));
#164580=CARTESIAN_POINT('Ctrl Pts',(15.4104571591017,9.54175110365538,-700.546424704239));
#164581=CARTESIAN_POINT('Ctrl Pts',(16.1559070823762,8.04468584505496,-702.040542351298));
#164582=CARTESIAN_POINT('Ctrl Pts',(16.9013570056506,6.54762058645456,-703.534659998357));
#164583=CARTESIAN_POINT('Ctrl Pts',(17.3590292079831,4.93906964482096,-705.028777645416));
#164584=CARTESIAN_POINT('Ctrl Pts',(17.8167014103155,3.33051870318735,-706.522895292475));
#164585=CARTESIAN_POINT('Ctrl Pts',(17.9710104137728,1.66525935159367,-708.017012939533));
#164586=CARTESIAN_POINT('Ctrl Pts',(18.1253194172301,3.32956716117513E-15,
-709.511130586592));
#164587=CARTESIAN_POINT('Ctrl Pts',(17.9710104137728,-1.66525935159367,
-711.005248233651));
#164588=CARTESIAN_POINT('Ctrl Pts',(17.8167014103155,-3.33051870318736,
-712.49936588071));
#164589=CARTESIAN_POINT('Ctrl Pts',(17.3590292079831,-4.93906964482095,
-713.993483527769));
#164590=CARTESIAN_POINT('Ctrl Pts',(16.9013570056506,-6.54762058645456,
-715.487601174828));
#164591=CARTESIAN_POINT('Ctrl Pts',(16.1559070823762,-8.04468584505497,
-716.981718821886));
#164592=CARTESIAN_POINT('Ctrl Pts',(15.4104571591017,-9.54175110365538,
-718.475836468945));
#164593=CARTESIAN_POINT('Ctrl Pts',(14.4026149179538,-10.8763499173728,
-719.969954116004));
#164594=CARTESIAN_POINT('Ctrl Pts',(13.3947726768058,-12.2109487310903,
-721.464071763063));
#164595=CARTESIAN_POINT('Ctrl Pts',(12.1588589765331,-13.3376329379985,
-722.958189410122));
#164596=CARTESIAN_POINT('Ctrl Pts',(10.9229452762603,-14.4643171449067,
-724.452307057181));
#164597=CARTESIAN_POINT('Ctrl Pts',(9.50104767561053,-15.3447188656481,
-725.946424704239));
#164598=CARTESIAN_POINT('Ctrl Pts',(8.07915007496071,-16.2251205863895,
-727.440542351298));
#164599=CARTESIAN_POINT('Ctrl Pts',(6.51968959134574,-16.8292587962898,
-728.934659998357));
#164600=CARTESIAN_POINT('Ctrl Pts',(4.96022910773078,-17.4333970061901,
-730.428777645416));
#164601=CARTESIAN_POINT('Ctrl Pts',(3.31631129755346,-17.7406985030951,
-731.922895292474));
#164602=CARTESIAN_POINT('Ctrl Pts',(1.67239348737615,-18.048,-733.417012939533));
#164603=CARTESIAN_POINT('Ctrl Pts',(0.,-18.048,-734.911130586592));
#164604=CARTESIAN_POINT('Ctrl Pts',(-1.67239348737615,-18.048,-736.405248233651));
#164605=CARTESIAN_POINT('Ctrl Pts',(-3.31631129755346,-17.7406985030951,
-737.89936588071));
#164606=CARTESIAN_POINT('Ctrl Pts',(-4.96022910773077,-17.4333970061901,
-739.393483527769));
#164607=CARTESIAN_POINT('Ctrl Pts',(-6.51968959134574,-16.8292587962898,
-740.887601174828));
#164608=CARTESIAN_POINT('Ctrl Pts',(-8.07915007496071,-16.2251205863895,
-742.381718821887));
#164609=CARTESIAN_POINT('Ctrl Pts',(-9.50104767561052,-15.3447188656481,
-743.875836468945));
#164610=CARTESIAN_POINT('Ctrl Pts',(-10.9229452762603,-14.4643171449067,
-745.369954116004));
#164611=CARTESIAN_POINT('Ctrl Pts',(-12.1588589765331,-13.3376329379985,
-746.864071763063));
#164612=CARTESIAN_POINT('Ctrl Pts',(-13.3947726768058,-12.2109487310903,
-748.358189410122));
#164613=CARTESIAN_POINT('Ctrl Pts',(-14.4026149179538,-10.8763499173728,
-749.85230705718));
#164614=CARTESIAN_POINT('Ctrl Pts',(-15.4104571591017,-9.54175110365538,
-751.346424704239));
#164615=CARTESIAN_POINT('Ctrl Pts',(-16.1559070823762,-8.04468584505497,
-752.840542351298));
#164616=CARTESIAN_POINT('Ctrl Pts',(-16.9013570056506,-6.54762058645456,
-754.334659998357));
#164617=CARTESIAN_POINT('Ctrl Pts',(-17.3590292079831,-4.93906964482095,
-755.828777645416));
#164618=CARTESIAN_POINT('Ctrl Pts',(-17.8167014103155,-3.33051870318735,
-757.322895292475));
#164619=CARTESIAN_POINT('Ctrl Pts',(-17.9710104137728,-1.66525935159368,
-758.817012939534));
#164620=CARTESIAN_POINT('Ctrl Pts',(-18.1253194172301,-1.10985572039171E-15,
-760.311130586593));
#164621=CARTESIAN_POINT('Ctrl Pts',(-17.9710104137728,1.66525935159367,
-761.805248233651));
#164622=CARTESIAN_POINT('Ctrl Pts',(-17.8167014103155,3.33051870318735,
-763.29936588071));
#164623=CARTESIAN_POINT('Ctrl Pts',(-17.3590292079831,4.93906964482096,
-764.793483527769));
#164624=CARTESIAN_POINT('Ctrl Pts',(-16.9013570056506,6.54762058645456,
-766.287601174827));
#164625=CARTESIAN_POINT('Ctrl Pts',(-16.1559070823762,8.04468584505497,
-767.781718821886));
#164626=CARTESIAN_POINT('Ctrl Pts',(-15.4104571591017,9.54175110365538,
-769.275836468945));
#164627=CARTESIAN_POINT('Ctrl Pts',(-14.4026149179538,10.8763499173728,
-770.769954116004));
#164628=CARTESIAN_POINT('Ctrl Pts',(-13.3947726768058,12.2109487310903,
-772.264071763063));
#164629=CARTESIAN_POINT('Ctrl Pts',(-12.1588589765331,13.3376329379985,
-773.758189410122));
#164630=CARTESIAN_POINT('Ctrl Pts',(-10.9229452762603,14.4643171449067,
-775.252307057181));
#164631=CARTESIAN_POINT('Ctrl Pts',(-9.50104767561052,15.3447188656481,
-776.746424704239));
#164632=CARTESIAN_POINT('Ctrl Pts',(-8.07915007496071,16.2251205863895,
-778.240542351298));
#164633=CARTESIAN_POINT('Ctrl Pts',(-6.51968959134574,16.8292587962898,
-779.734659998357));
#164634=CARTESIAN_POINT('Ctrl Pts',(-4.96022910773078,17.4333970061901,
-781.228777645416));
#164635=CARTESIAN_POINT('Ctrl Pts',(-3.31631129755346,17.7406985030951,
-782.722895292475));
#164636=CARTESIAN_POINT('Ctrl Pts',(-1.67239348737615,18.048,-784.217012939534));
#164637=CARTESIAN_POINT('Ctrl Pts',(-2.21024254310115E-15,18.048,-785.711130586592));
#164638=CARTESIAN_POINT('Ctrl Pts',(1.67239348737616,18.048,-787.205248233651));
#164639=CARTESIAN_POINT('Ctrl Pts',(3.31631129755346,17.7406985030951,-788.69936588071));
#164640=CARTESIAN_POINT('Ctrl Pts',(4.96022910773077,17.4333970061901,-790.193483527769));
#164641=CARTESIAN_POINT('Ctrl Pts',(6.51968959134575,16.8292587962898,-791.687601174827));
#164642=CARTESIAN_POINT('Ctrl Pts',(8.07915007496071,16.2251205863895,-793.181718821886));
#164643=CARTESIAN_POINT('Ctrl Pts',(9.50104767561053,15.3447188656481,-794.675836468945));
#164644=CARTESIAN_POINT('Ctrl Pts',(10.9229452762603,14.4643171449067,-796.169954116004));
#164645=CARTESIAN_POINT('Ctrl Pts',(12.1588589765331,13.3376329379985,-797.664071763063));
#164646=CARTESIAN_POINT('Ctrl Pts',(13.3947726768058,12.2109487310903,-799.158189410122));
#164647=CARTESIAN_POINT('Ctrl Pts',(14.4026149179538,10.8763499173728,-800.65230705718));
#164648=CARTESIAN_POINT('Ctrl Pts',(15.4104571591017,9.54175110365538,-802.146424704239));
#164649=CARTESIAN_POINT('Ctrl Pts',(16.1559070823762,8.04468584505496,-803.640542351298));
#164650=CARTESIAN_POINT('Ctrl Pts',(16.9013570056506,6.54762058645456,-805.134659998357));
#164651=CARTESIAN_POINT('Ctrl Pts',(17.3590292079831,4.93906964482096,-806.628777645416));
#164652=CARTESIAN_POINT('Ctrl Pts',(17.8167014103155,3.33051870318735,-808.122895292474));
#164653=CARTESIAN_POINT('Ctrl Pts',(17.9710104137728,1.66525935159367,-809.617012939533));
#164654=CARTESIAN_POINT('Ctrl Pts',(18.1253194172301,3.32956716117513E-15,
-811.111130586592));
#164655=CARTESIAN_POINT('Ctrl Pts',(17.9710104137728,-1.66525935159367,
-812.605248233651));
#164656=CARTESIAN_POINT('Ctrl Pts',(17.8167014103155,-3.33051870318736,
-814.09936588071));
#164657=CARTESIAN_POINT('Ctrl Pts',(17.3590292079831,-4.93906964482095,
-815.593483527769));
#164658=CARTESIAN_POINT('Ctrl Pts',(16.9013570056506,-6.54762058645456,
-817.087601174828));
#164659=CARTESIAN_POINT('Ctrl Pts',(16.1559070823762,-8.04468584505497,
-818.581718821887));
#164660=CARTESIAN_POINT('Ctrl Pts',(15.4104571591017,-9.54175110365538,
-820.075836468945));
#164661=CARTESIAN_POINT('Ctrl Pts',(14.4026149179538,-10.8763499173728,
-821.569954116004));
#164662=CARTESIAN_POINT('Ctrl Pts',(13.3947726768058,-12.2109487310903,
-823.064071763063));
#164663=CARTESIAN_POINT('Ctrl Pts',(12.1588589765331,-13.3376329379985,
-824.558189410121));
#164664=CARTESIAN_POINT('Ctrl Pts',(10.9229452762603,-14.4643171449067,
-826.05230705718));
#164665=CARTESIAN_POINT('Ctrl Pts',(9.50104767561053,-15.3447188656481,
-827.546424704239));
#164666=CARTESIAN_POINT('Ctrl Pts',(8.07915007496071,-16.2251205863895,
-829.040542351298));
#164667=CARTESIAN_POINT('Ctrl Pts',(6.51968959134574,-16.8292587962898,
-830.534659998357));
#164668=CARTESIAN_POINT('Ctrl Pts',(4.96022910773078,-17.4333970061901,
-832.028777645416));
#164669=CARTESIAN_POINT('Ctrl Pts',(3.31631129755346,-17.7406985030951,
-833.522895292475));
#164670=CARTESIAN_POINT('Ctrl Pts',(1.67239348737615,-18.048,-835.017012939534));
#164671=CARTESIAN_POINT('Ctrl Pts',(0.,-18.048,-836.511130586592));
#164672=CARTESIAN_POINT('Ctrl Pts',(-1.67239348737615,-18.048,-838.005248233651));
#164673=CARTESIAN_POINT('Ctrl Pts',(-3.31631129755346,-17.7406985030951,
-839.49936588071));
#164674=CARTESIAN_POINT('Ctrl Pts',(-4.96022910773077,-17.4333970061901,
-840.993483527769));
#164675=CARTESIAN_POINT('Ctrl Pts',(-6.51968959134574,-16.8292587962898,
-842.487601174827));
#164676=CARTESIAN_POINT('Ctrl Pts',(-8.07915007496071,-16.2251205863895,
-843.981718821886));
#164677=CARTESIAN_POINT('Ctrl Pts',(-9.50104767561052,-15.3447188656481,
-845.475836468945));
#164678=CARTESIAN_POINT('Ctrl Pts',(-10.9229452762603,-14.4643171449067,
-846.969954116004));
#164679=CARTESIAN_POINT('Ctrl Pts',(-12.1588589765331,-13.3376329379985,
-848.464071763063));
#164680=CARTESIAN_POINT('Ctrl Pts',(-13.3947726768058,-12.2109487310903,
-849.958189410122));
#164681=CARTESIAN_POINT('Ctrl Pts',(-14.4026149179538,-10.8763499173728,
-851.45230705718));
#164682=CARTESIAN_POINT('Ctrl Pts',(-15.4104571591017,-9.54175110365538,
-852.946424704239));
#164683=CARTESIAN_POINT('Ctrl Pts',(-16.1559070823762,-8.04468584505497,
-854.440542351298));
#164684=CARTESIAN_POINT('Ctrl Pts',(-16.9013570056506,-6.54762058645456,
-855.934659998357));
#164685=CARTESIAN_POINT('Ctrl Pts',(-17.3590292079831,-4.93906964482095,
-857.428777645416));
#164686=CARTESIAN_POINT('Ctrl Pts',(-17.8167014103155,-3.33051870318735,
-858.922895292475));
#164687=CARTESIAN_POINT('Ctrl Pts',(-17.9710104137728,-1.66525935159368,
-860.417012939533));
#164688=CARTESIAN_POINT('Ctrl Pts',(-18.1253194172301,-1.10985572039171E-15,
-861.911130586592));
#164689=CARTESIAN_POINT('Ctrl Pts',(-17.9710104137728,1.66525935159367,
-863.405248233651));
#164690=CARTESIAN_POINT('Ctrl Pts',(-17.8167014103155,3.33051870318735,
-864.89936588071));
#164691=CARTESIAN_POINT('Ctrl Pts',(-17.3590292079831,4.93906964482096,
-866.393483527768));
#164692=CARTESIAN_POINT('Ctrl Pts',(-16.9013570056506,6.54762058645456,
-867.887601174827));
#164693=CARTESIAN_POINT('Ctrl Pts',(-16.1559070823762,8.04468584505497,
-869.381718821886));
#164694=CARTESIAN_POINT('Ctrl Pts',(-15.4104571591017,9.54175110365538,
-870.875836468945));
#164695=CARTESIAN_POINT('Ctrl Pts',(-14.4026149179538,10.8763499173728,
-872.369954116004));
#164696=CARTESIAN_POINT('Ctrl Pts',(-13.3947726768058,12.2109487310903,
-873.864071763063));
#164697=CARTESIAN_POINT('Ctrl Pts',(-12.1588589765331,13.3376329379985,
-875.358189410122));
#164698=CARTESIAN_POINT('Ctrl Pts',(-10.9229452762603,14.4643171449067,
-876.85230705718));
#164699=CARTESIAN_POINT('Ctrl Pts',(-9.50104767561052,15.3447188656481,
-878.346424704239));
#164700=CARTESIAN_POINT('Ctrl Pts',(-8.07915007496071,16.2251205863895,
-879.840542351298));
#164701=CARTESIAN_POINT('Ctrl Pts',(-6.51968959134574,16.8292587962898,
-881.334659998357));
#164702=CARTESIAN_POINT('Ctrl Pts',(-4.96022910773078,17.4333970061901,
-882.828777645416));
#164703=CARTESIAN_POINT('Ctrl Pts',(-3.31631129755346,17.7406985030951,
-884.322895292474));
#164704=CARTESIAN_POINT('Ctrl Pts',(-1.67239348737615,18.048,-885.817012939534));
#164705=CARTESIAN_POINT('Ctrl Pts',(-2.21024254310115E-15,18.048,-887.311130586592));
#164706=CARTESIAN_POINT('Ctrl Pts',(1.67239348737616,18.048,-888.805248233651));
#164707=CARTESIAN_POINT('Ctrl Pts',(3.31631129755346,17.7406985030951,-890.29936588071));
#164708=CARTESIAN_POINT('Ctrl Pts',(4.96022910773077,17.4333970061901,-891.793483527769));
#164709=CARTESIAN_POINT('Ctrl Pts',(6.51968959134575,16.8292587962898,-893.287601174828));
#164710=CARTESIAN_POINT('Ctrl Pts',(8.07915007496071,16.2251205863895,-894.781718821887));
#164711=CARTESIAN_POINT('Ctrl Pts',(9.50104767561053,15.3447188656481,-896.275836468945));
#164712=CARTESIAN_POINT('Ctrl Pts',(10.9229452762603,14.4643171449067,-897.769954116004));
#164713=CARTESIAN_POINT('Ctrl Pts',(12.1588589765331,13.3376329379985,-899.264071763063));
#164714=CARTESIAN_POINT('Ctrl Pts',(13.3947726768058,12.2109487310903,-900.758189410122));
#164715=CARTESIAN_POINT('Ctrl Pts',(14.4026149179538,10.8763499173728,-902.25230705718));
#164716=CARTESIAN_POINT('Ctrl Pts',(15.4104571591017,9.54175110365538,-903.746424704239));
#164717=CARTESIAN_POINT('Ctrl Pts',(16.1559070823762,8.04468584505496,-905.240542351298));
#164718=CARTESIAN_POINT('Ctrl Pts',(16.9013570056506,6.54762058645456,-906.734659998357));
#164719=CARTESIAN_POINT('Ctrl Pts',(17.3590292079831,4.93906964482096,-908.228777645416));
#164720=CARTESIAN_POINT('Ctrl Pts',(17.8167014103155,3.33051870318735,-909.722895292475));
#164721=CARTESIAN_POINT('Ctrl Pts',(17.9710104137728,1.66525935159367,-911.217012939533));
#164722=CARTESIAN_POINT('Ctrl Pts',(18.1253194172301,3.32956716117513E-15,
-912.711130586592));
#164723=CARTESIAN_POINT('Ctrl Pts',(17.9710104137728,-1.66525935159367,
-914.205248233651));
#164724=CARTESIAN_POINT('Ctrl Pts',(17.8167014103155,-3.33051870318736,
-915.69936588071));
#164725=CARTESIAN_POINT('Ctrl Pts',(17.3590292079831,-4.93906964482095,
-917.193483527769));
#164726=CARTESIAN_POINT('Ctrl Pts',(16.9013570056506,-6.54762058645456,
-918.687601174827));
#164727=CARTESIAN_POINT('Ctrl Pts',(16.1559070823762,-8.04468584505497,
-920.181718821887));
#164728=CARTESIAN_POINT('Ctrl Pts',(15.4104571591017,-9.54175110365538,
-921.675836468945));
#164729=CARTESIAN_POINT('Ctrl Pts',(14.4026149179538,-10.8763499173728,
-923.169954116004));
#164730=CARTESIAN_POINT('Ctrl Pts',(13.3947726768058,-12.2109487310903,
-924.664071763063));
#164731=CARTESIAN_POINT('Ctrl Pts',(12.1588589765331,-13.3376329379985,
-926.158189410122));
#164732=CARTESIAN_POINT('Ctrl Pts',(10.9229452762603,-14.4643171449067,
-927.65230705718));
#164733=CARTESIAN_POINT('Ctrl Pts',(9.50104767561053,-15.3447188656481,
-929.146424704239));
#164734=CARTESIAN_POINT('Ctrl Pts',(8.07915007496071,-16.2251205863895,
-930.640542351298));
#164735=CARTESIAN_POINT('Ctrl Pts',(6.51968959134574,-16.8292587962898,
-932.134659998357));
#164736=CARTESIAN_POINT('Ctrl Pts',(4.96022910773078,-17.4333970061901,
-933.628777645416));
#164737=CARTESIAN_POINT('Ctrl Pts',(3.31631129755346,-17.7406985030951,
-935.122895292475));
#164738=CARTESIAN_POINT('Ctrl Pts',(1.67239348737615,-18.048,-936.617012939534));
#164739=CARTESIAN_POINT('Ctrl Pts',(0.,-18.048,-938.111130586592));
#164740=CARTESIAN_POINT('Ctrl Pts',(-1.67239348737615,-18.048,-939.605248233651));
#164741=CARTESIAN_POINT('Ctrl Pts',(-3.31631129755346,-17.7406985030951,
-941.09936588071));
#164742=CARTESIAN_POINT('Ctrl Pts',(-4.96022910773077,-17.4333970061901,
-942.593483527769));
#164743=CARTESIAN_POINT('Ctrl Pts',(-6.51968959134574,-16.8292587962898,
-944.087601174827));
#164744=CARTESIAN_POINT('Ctrl Pts',(-8.07915007496071,-16.2251205863895,
-945.581718821886));
#164745=CARTESIAN_POINT('Ctrl Pts',(-9.50104767561052,-15.3447188656481,
-947.075836468945));
#164746=CARTESIAN_POINT('Ctrl Pts',(-10.9229452762603,-14.4643171449067,
-948.569954116004));
#164747=CARTESIAN_POINT('Ctrl Pts',(-12.1588589765331,-13.3376329379985,
-950.064071763063));
#164748=CARTESIAN_POINT('Ctrl Pts',(-13.3947726768058,-12.2109487310903,
-951.558189410122));
#164749=CARTESIAN_POINT('Ctrl Pts',(-14.4026149179538,-10.8763499173728,
-953.052307057181));
#164750=CARTESIAN_POINT('Ctrl Pts',(-15.4104571591017,-9.54175110365538,
-954.54642470424));
#164751=CARTESIAN_POINT('Ctrl Pts',(-16.1559070823762,-8.04468584505497,
-956.040542351298));
#164752=CARTESIAN_POINT('Ctrl Pts',(-16.9013570056506,-6.54762058645456,
-957.534659998357));
#164753=CARTESIAN_POINT('Ctrl Pts',(-17.3590292079831,-4.93906964482095,
-959.028777645416));
#164754=CARTESIAN_POINT('Ctrl Pts',(-17.8167014103155,-3.33051870318735,
-960.522895292475));
#164755=CARTESIAN_POINT('Ctrl Pts',(-17.9710104137728,-1.66525935159368,
-962.017012939533));
#164756=CARTESIAN_POINT('Ctrl Pts',(-18.1253194172301,-1.10985572039171E-15,
-963.511130586592));
#164757=CARTESIAN_POINT('Ctrl Pts',(-17.9710104137728,1.66525935159367,
-965.005248233651));
#164758=CARTESIAN_POINT('Ctrl Pts',(-17.8167014103155,3.33051870318735,
-966.49936588071));
#164759=CARTESIAN_POINT('Ctrl Pts',(-17.3590292079831,4.93906964482096,
-967.993483527769));
#164760=CARTESIAN_POINT('Ctrl Pts',(-16.9013570056506,6.54762058645456,
-969.487601174828));
#164761=CARTESIAN_POINT('Ctrl Pts',(-16.1559070823762,8.04468584505497,
-970.981718821886));
#164762=CARTESIAN_POINT('Ctrl Pts',(-15.4104571591017,9.54175110365538,
-972.475836468945));
#164763=CARTESIAN_POINT('Ctrl Pts',(-14.4026149179538,10.8763499173728,
-973.969954116004));
#164764=CARTESIAN_POINT('Ctrl Pts',(-13.3947726768058,12.2109487310903,
-975.464071763063));
#164765=CARTESIAN_POINT('Ctrl Pts',(-12.1588589765331,13.3376329379985,
-976.958189410122));
#164766=CARTESIAN_POINT('Ctrl Pts',(-10.9229452762603,14.4643171449067,
-978.452307057181));
#164767=CARTESIAN_POINT('Ctrl Pts',(-9.50104767561052,15.3447188656481,
-979.946424704239));
#164768=CARTESIAN_POINT('Ctrl Pts',(-8.07915007496071,16.2251205863895,
-981.440542351298));
#164769=CARTESIAN_POINT('Ctrl Pts',(-6.51968959134574,16.8292587962898,
-982.934659998357));
#164770=CARTESIAN_POINT('Ctrl Pts',(-4.96022910773078,17.4333970061901,
-984.428777645416));
#164771=CARTESIAN_POINT('Ctrl Pts',(-3.31631129755346,17.7406985030951,
-985.922895292474));
#164772=CARTESIAN_POINT('Ctrl Pts',(-1.67239348737615,18.048,-987.417012939533));
#164773=CARTESIAN_POINT('Ctrl Pts',(-2.21024254310115E-15,18.048,-988.911130586592));
#164774=CARTESIAN_POINT('Ctrl Pts',(1.67239348737616,18.048,-990.405248233651));
#164775=CARTESIAN_POINT('Ctrl Pts',(3.31631129755346,17.7406985030951,-991.89936588071));
#164776=CARTESIAN_POINT('Ctrl Pts',(4.96022910773077,17.4333970061901,-993.393483527769));
#164777=CARTESIAN_POINT('Ctrl Pts',(6.51968959134575,16.8292587962898,-994.887601174828));
#164778=CARTESIAN_POINT('Ctrl Pts',(8.07915007496071,16.2251205863895,-996.381718821887));
#164779=CARTESIAN_POINT('Ctrl Pts',(9.50104767561053,15.3447188656481,-997.875836468945));
#164780=CARTESIAN_POINT('Ctrl Pts',(10.9229452762603,14.4643171449067,-999.369954116004));
#164781=CARTESIAN_POINT('Ctrl Pts',(12.1588589765331,13.3376329379985,-1000.86407176306));
#164782=CARTESIAN_POINT('Ctrl Pts',(13.3947726768058,12.2109487310903,-1002.35818941012));
#164783=CARTESIAN_POINT('Ctrl Pts',(14.4026149179538,10.8763499173728,-1003.85230705718));
#164784=CARTESIAN_POINT('Ctrl Pts',(15.4104571591017,9.54175110365538,-1005.34642470424));
#164785=CARTESIAN_POINT('Ctrl Pts',(16.1559070823762,8.04468584505496,-1006.8405423513));
#164786=CARTESIAN_POINT('Ctrl Pts',(16.9013570056506,6.54762058645456,-1008.33465999836));
#164787=CARTESIAN_POINT('Ctrl Pts',(17.3590292079831,4.93906964482096,-1009.82877764542));
#164788=CARTESIAN_POINT('Ctrl Pts',(17.8167014103155,3.33051870318735,-1011.32289529247));
#164789=CARTESIAN_POINT('Ctrl Pts',(17.9710104137728,1.66525935159367,-1012.81701293953));
#164790=CARTESIAN_POINT('Ctrl Pts',(18.1253194172301,3.32956716117513E-15,
-1014.31113058659));
#164791=CARTESIAN_POINT('Ctrl Pts',(17.9710104137728,-1.66525935159367,
-1015.80524823365));
#164792=CARTESIAN_POINT('Ctrl Pts',(17.8167014103155,-3.33051870318736,
-1017.29936588071));
#164793=CARTESIAN_POINT('Ctrl Pts',(17.3590292079831,-4.93906964482095,
-1018.79348352777));
#164794=CARTESIAN_POINT('Ctrl Pts',(16.9013570056506,-6.54762058645456,
-1020.28760117483));
#164795=CARTESIAN_POINT('Ctrl Pts',(16.1559070823762,-8.04468584505497,
-1021.78171882189));
#164796=CARTESIAN_POINT('Ctrl Pts',(15.4104571591017,-9.54175110365538,
-1023.27583646895));
#164797=CARTESIAN_POINT('Ctrl Pts',(14.4026149179538,-10.8763499173728,
-1024.769954116));
#164798=CARTESIAN_POINT('Ctrl Pts',(13.3947726768058,-12.2109487310903,
-1026.26407176306));
#164799=CARTESIAN_POINT('Ctrl Pts',(12.1588589765331,-13.3376329379985,
-1027.75818941012));
#164800=CARTESIAN_POINT('Ctrl Pts',(10.9229452762603,-14.4643171449067,
-1029.25230705718));
#164801=CARTESIAN_POINT('Ctrl Pts',(9.50104767561053,-15.3447188656481,
-1030.74642470424));
#164802=CARTESIAN_POINT('Ctrl Pts',(8.07915007496071,-16.2251205863895,
-1032.2405423513));
#164803=CARTESIAN_POINT('Ctrl Pts',(6.51968959134574,-16.8292587962898,
-1033.73465999836));
#164804=CARTESIAN_POINT('Ctrl Pts',(4.96022910773078,-17.4333970061901,
-1035.22877764542));
#164805=CARTESIAN_POINT('Ctrl Pts',(3.31631129755346,-17.7406985030951,
-1036.72289529247));
#164806=CARTESIAN_POINT('Ctrl Pts',(1.67239348737615,-18.048,-1038.21701293953));
#164807=CARTESIAN_POINT('Ctrl Pts',(0.,-18.048,-1039.71113058659));
#164808=CARTESIAN_POINT('Ctrl Pts',(-1.67239348737615,-18.048,-1041.20524823365));
#164809=CARTESIAN_POINT('Ctrl Pts',(-3.31631129755346,-17.7406985030951,
-1042.69936588071));
#164810=CARTESIAN_POINT('Ctrl Pts',(-4.96022910773077,-17.4333970061901,
-1044.19348352777));
#164811=CARTESIAN_POINT('Ctrl Pts',(-6.51968959134574,-16.8292587962898,
-1045.68760117483));
#164812=CARTESIAN_POINT('Ctrl Pts',(-8.07915007496071,-16.2251205863895,
-1047.18171882189));
#164813=CARTESIAN_POINT('Ctrl Pts',(-9.50104767561052,-15.3447188656481,
-1048.67583646894));
#164814=CARTESIAN_POINT('Ctrl Pts',(-10.9229452762603,-14.4643171449067,
-1050.169954116));
#164815=CARTESIAN_POINT('Ctrl Pts',(-12.1588589765331,-13.3376329379985,
-1051.66407176306));
#164816=CARTESIAN_POINT('Ctrl Pts',(-13.3947726768058,-12.2109487310903,
-1053.15818941012));
#164817=CARTESIAN_POINT('Ctrl Pts',(-14.4026149179538,-10.8763499173728,
-1054.65230705718));
#164818=CARTESIAN_POINT('Ctrl Pts',(-15.4104571591017,-9.54175110365538,
-1056.14642470424));
#164819=CARTESIAN_POINT('Ctrl Pts',(-16.1559070823762,-8.04468584505497,
-1057.6405423513));
#164820=CARTESIAN_POINT('Ctrl Pts',(-16.9013570056506,-6.54762058645456,
-1059.13465999836));
#164821=CARTESIAN_POINT('Ctrl Pts',(-17.3590292079831,-4.93906964482095,
-1060.62877764542));
#164822=CARTESIAN_POINT('Ctrl Pts',(-17.8167014103155,-3.33051870318735,
-1062.12289529247));
#164823=CARTESIAN_POINT('Ctrl Pts',(-17.9710104137728,-1.66525935159368,
-1063.61701293953));
#164824=CARTESIAN_POINT('Ctrl Pts',(-18.1253194172301,-1.10985572039171E-15,
-1065.11113058659));
#164825=CARTESIAN_POINT('Ctrl Pts',(-17.9710104137728,1.66525935159367,
-1066.60524823365));
#164826=CARTESIAN_POINT('Ctrl Pts',(-17.8167014103155,3.33051870318735,
-1068.09936588071));
#164827=CARTESIAN_POINT('Ctrl Pts',(-17.3590292079831,4.93906964482096,
-1069.59348352777));
#164828=CARTESIAN_POINT('Ctrl Pts',(-16.9013570056506,6.54762058645456,
-1071.08760117483));
#164829=CARTESIAN_POINT('Ctrl Pts',(-16.1559070823762,8.04468584505497,
-1072.58171882189));
#164830=CARTESIAN_POINT('Ctrl Pts',(-15.4104571591017,9.54175110365538,
-1074.07583646895));
#164831=CARTESIAN_POINT('Ctrl Pts',(-14.4026149179538,10.8763499173728,
-1075.569954116));
#164832=CARTESIAN_POINT('Ctrl Pts',(-13.3947726768058,12.2109487310903,
-1077.06407176306));
#164833=CARTESIAN_POINT('Ctrl Pts',(-12.1588589765331,13.3376329379985,
-1078.55818941012));
#164834=CARTESIAN_POINT('Ctrl Pts',(-10.9229452762603,14.4643171449067,
-1080.05230705718));
#164835=CARTESIAN_POINT('Ctrl Pts',(-9.50104767561052,15.3447188656481,
-1081.54642470424));
#164836=CARTESIAN_POINT('Ctrl Pts',(-8.07915007496071,16.2251205863895,
-1083.0405423513));
#164837=CARTESIAN_POINT('Ctrl Pts',(-6.51968959134574,16.8292587962898,
-1084.53465999836));
#164838=CARTESIAN_POINT('Ctrl Pts',(-4.96022910773078,17.4333970061901,
-1086.02877764542));
#164839=CARTESIAN_POINT('Ctrl Pts',(-3.31631129755346,17.7406985030951,
-1087.52289529247));
#164840=CARTESIAN_POINT('Ctrl Pts',(-1.67239348737615,18.048,-1089.01701293953));
#164841=CARTESIAN_POINT('Ctrl Pts',(-2.21024254310115E-15,18.048,-1090.51113058659));
#164842=CARTESIAN_POINT('Ctrl Pts',(1.67239348737616,18.048,-1092.00524823365));
#164843=CARTESIAN_POINT('Ctrl Pts',(3.31631129755346,17.7406985030951,-1093.49936588071));
#164844=CARTESIAN_POINT('Ctrl Pts',(4.96022910773077,17.4333970061901,-1094.99348352777));
#164845=CARTESIAN_POINT('Ctrl Pts',(6.51968959134575,16.8292587962898,-1096.48760117483));
#164846=CARTESIAN_POINT('Ctrl Pts',(8.07915007496071,16.2251205863895,-1097.98171882189));
#164847=CARTESIAN_POINT('Ctrl Pts',(9.50104767561053,15.3447188656481,-1099.47583646895));
#164848=CARTESIAN_POINT('Ctrl Pts',(10.9229452762603,14.4643171449067,-1100.969954116));
#164849=CARTESIAN_POINT('Ctrl Pts',(12.1588589765331,13.3376329379985,-1102.46407176306));
#164850=CARTESIAN_POINT('Ctrl Pts',(13.3947726768058,12.2109487310903,-1103.95818941012));
#164851=CARTESIAN_POINT('Ctrl Pts',(14.4026149179538,10.8763499173728,-1105.45230705718));
#164852=CARTESIAN_POINT('Ctrl Pts',(15.4104571591017,9.54175110365538,-1106.94642470424));
#164853=CARTESIAN_POINT('Ctrl Pts',(16.1559070823762,8.04468584505496,-1108.4405423513));
#164854=CARTESIAN_POINT('Ctrl Pts',(16.9013570056506,6.54762058645456,-1109.93465999836));
#164855=CARTESIAN_POINT('Ctrl Pts',(17.3590292079831,4.93906964482096,-1111.42877764542));
#164856=CARTESIAN_POINT('Ctrl Pts',(17.8167014103155,3.33051870318735,-1112.92289529247));
#164857=CARTESIAN_POINT('Ctrl Pts',(17.9710104137728,1.66525935159367,-1114.41701293953));
#164858=CARTESIAN_POINT('Ctrl Pts',(18.1253194172301,3.32956716117513E-15,
-1115.91113058659));
#164859=CARTESIAN_POINT('Ctrl Pts',(17.9710104137728,-1.66525935159367,
-1117.40524823365));
#164860=CARTESIAN_POINT('Ctrl Pts',(17.8167014103155,-3.33051870318736,
-1118.89936588071));
#164861=CARTESIAN_POINT('Ctrl Pts',(17.3590292079831,-4.93906964482095,
-1120.39348352777));
#164862=CARTESIAN_POINT('Ctrl Pts',(16.9013570056506,-6.54762058645456,
-1121.88760117483));
#164863=CARTESIAN_POINT('Ctrl Pts',(16.1559070823762,-8.04468584505497,
-1123.38171882189));
#164864=CARTESIAN_POINT('Ctrl Pts',(15.4104571591017,-9.54175110365538,
-1124.87583646895));
#164865=CARTESIAN_POINT('Ctrl Pts',(14.4026149179538,-10.8763499173728,
-1126.369954116));
#164866=CARTESIAN_POINT('Ctrl Pts',(13.3947726768058,-12.2109487310903,
-1127.86407176306));
#164867=CARTESIAN_POINT('Ctrl Pts',(12.1588589765331,-13.3376329379985,
-1129.35818941012));
#164868=CARTESIAN_POINT('Ctrl Pts',(10.9229452762603,-14.4643171449067,
-1130.85230705718));
#164869=CARTESIAN_POINT('Ctrl Pts',(9.50104767561053,-15.3447188656481,
-1132.34642470424));
#164870=CARTESIAN_POINT('Ctrl Pts',(8.07915007496071,-16.2251205863895,
-1133.8405423513));
#164871=CARTESIAN_POINT('Ctrl Pts',(6.51968959134574,-16.8292587962898,
-1135.33465999836));
#164872=CARTESIAN_POINT('Ctrl Pts',(4.96022910773078,-17.4333970061901,
-1136.82877764542));
#164873=CARTESIAN_POINT('Ctrl Pts',(3.31631129755346,-17.7406985030951,
-1138.32289529247));
#164874=CARTESIAN_POINT('Ctrl Pts',(1.67239348737615,-18.048,-1139.81701293953));
#164875=CARTESIAN_POINT('Ctrl Pts',(0.,-18.048,-1141.31113058659));
#164876=CARTESIAN_POINT('Ctrl Pts',(-1.67239348737615,-18.048,-1142.80524823365));
#164877=CARTESIAN_POINT('Ctrl Pts',(-3.31631129755346,-17.7406985030951,
-1144.29936588071));
#164878=CARTESIAN_POINT('Ctrl Pts',(-4.96022910773077,-17.4333970061901,
-1145.79348352777));
#164879=CARTESIAN_POINT('Ctrl Pts',(-6.51968959134574,-16.8292587962898,
-1147.28760117483));
#164880=CARTESIAN_POINT('Ctrl Pts',(-8.07915007496071,-16.2251205863895,
-1148.78171882189));
#164881=CARTESIAN_POINT('Ctrl Pts',(-9.50104767561052,-15.3447188656481,
-1150.27583646895));
#164882=CARTESIAN_POINT('Ctrl Pts',(-10.9229452762603,-14.4643171449067,
-1151.769954116));
#164883=CARTESIAN_POINT('Ctrl Pts',(-12.1588589765331,-13.3376329379985,
-1153.26407176306));
#164884=CARTESIAN_POINT('Ctrl Pts',(-13.3947726768058,-12.2109487310903,
-1154.75818941012));
#164885=CARTESIAN_POINT('Ctrl Pts',(-14.4026149179538,-10.8763499173728,
-1156.25230705718));
#164886=CARTESIAN_POINT('Ctrl Pts',(-15.4104571591017,-9.54175110365538,
-1157.74642470424));
#164887=CARTESIAN_POINT('Ctrl Pts',(-16.1559070823762,-8.04468584505497,
-1159.2405423513));
#164888=CARTESIAN_POINT('Ctrl Pts',(-16.9013570056506,-6.54762058645456,
-1160.73465999836));
#164889=CARTESIAN_POINT('Ctrl Pts',(-17.3590292079831,-4.93906964482095,
-1162.22877764542));
#164890=CARTESIAN_POINT('Ctrl Pts',(-17.8167014103155,-3.33051870318735,
-1163.72289529247));
#164891=CARTESIAN_POINT('Ctrl Pts',(-17.9710104137728,-1.66525935159368,
-1165.21701293953));
#164892=CARTESIAN_POINT('Ctrl Pts',(-18.1253194172301,-1.10985572039171E-15,
-1166.71113058659));
#164893=CARTESIAN_POINT('Ctrl Pts',(-17.9710104137728,1.66525935159367,
-1168.20524823365));
#164894=CARTESIAN_POINT('Ctrl Pts',(-17.8167014103155,3.33051870318735,
-1169.69936588071));
#164895=CARTESIAN_POINT('Ctrl Pts',(-17.3590292079831,4.93906964482096,
-1171.19348352777));
#164896=CARTESIAN_POINT('Ctrl Pts',(-16.9013570056506,6.54762058645456,
-1172.68760117483));
#164897=CARTESIAN_POINT('Ctrl Pts',(-16.1559070823762,8.04468584505497,
-1174.18171882189));
#164898=CARTESIAN_POINT('Ctrl Pts',(-15.4104571591017,9.54175110365538,
-1175.67583646895));
#164899=CARTESIAN_POINT('Ctrl Pts',(-14.4026149179538,10.8763499173728,
-1177.169954116));
#164900=CARTESIAN_POINT('Ctrl Pts',(-13.3947726768058,12.2109487310903,
-1178.66407176306));
#164901=CARTESIAN_POINT('Ctrl Pts',(-12.1588589765331,13.3376329379985,
-1180.15818941012));
#164902=CARTESIAN_POINT('Ctrl Pts',(-10.9229452762603,14.4643171449067,
-1181.65230705718));
#164903=CARTESIAN_POINT('Ctrl Pts',(-9.50104767561052,15.3447188656481,
-1183.14642470424));
#164904=CARTESIAN_POINT('Ctrl Pts',(-8.07915007496071,16.2251205863895,
-1184.6405423513));
#164905=CARTESIAN_POINT('Ctrl Pts',(-6.51968959134574,16.8292587962898,
-1186.13465999836));
#164906=CARTESIAN_POINT('Ctrl Pts',(-4.96022910773078,17.4333970061901,
-1187.62877764542));
#164907=CARTESIAN_POINT('Ctrl Pts',(-3.31631129755346,17.7406985030951,
-1189.12289529247));
#164908=CARTESIAN_POINT('Ctrl Pts',(-1.67239348737615,18.048,-1190.61701293953));
#164909=CARTESIAN_POINT('Ctrl Pts',(-2.21024254310115E-15,18.048,-1192.11113058659));
#164910=CARTESIAN_POINT('Ctrl Pts',(1.67239348737616,18.048,-1193.60524823365));
#164911=CARTESIAN_POINT('Ctrl Pts',(3.31631129755346,17.7406985030951,-1195.09936588071));
#164912=CARTESIAN_POINT('Ctrl Pts',(4.96022910773077,17.4333970061901,-1196.59348352777));
#164913=CARTESIAN_POINT('Ctrl Pts',(6.51968959134575,16.8292587962898,-1198.08760117483));
#164914=CARTESIAN_POINT('Ctrl Pts',(8.07915007496071,16.2251205863895,-1199.58171882189));
#164915=CARTESIAN_POINT('Ctrl Pts',(9.50104767561053,15.3447188656481,-1201.07583646894));
#164916=CARTESIAN_POINT('Ctrl Pts',(10.9229452762603,14.4643171449067,-1202.569954116));
#164917=CARTESIAN_POINT('Ctrl Pts',(12.1588589765331,13.3376329379985,-1204.06407176306));
#164918=CARTESIAN_POINT('Ctrl Pts',(13.3947726768058,12.2109487310903,-1205.55818941012));
#164919=CARTESIAN_POINT('Ctrl Pts',(14.4026149179538,10.8763499173728,-1207.05230705718));
#164920=CARTESIAN_POINT('Ctrl Pts',(15.4104571591017,9.54175110365538,-1208.54642470424));
#164921=CARTESIAN_POINT('Ctrl Pts',(16.1559070823762,8.04468584505496,-1210.0405423513));
#164922=CARTESIAN_POINT('Ctrl Pts',(16.9013570056506,6.54762058645456,-1211.53465999836));
#164923=CARTESIAN_POINT('Ctrl Pts',(17.3590292079831,4.93906964482096,-1213.02877764542));
#164924=CARTESIAN_POINT('Ctrl Pts',(17.8167014103155,3.33051870318735,-1214.52289529247));
#164925=CARTESIAN_POINT('Ctrl Pts',(17.9710104137728,1.66525935159367,-1216.01701293953));
#164926=CARTESIAN_POINT('Ctrl Pts',(18.1253194172301,3.32956716117513E-15,
-1217.51113058659));
#164927=CARTESIAN_POINT('Ctrl Pts',(17.9710104137728,-1.66525935159367,
-1219.00524823365));
#164928=CARTESIAN_POINT('Ctrl Pts',(17.8167014103155,-3.33051870318736,
-1220.49936588071));
#164929=CARTESIAN_POINT('Ctrl Pts',(17.3590292079831,-4.93906964482095,
-1221.99348352777));
#164930=CARTESIAN_POINT('Ctrl Pts',(16.9013570056506,-6.54762058645456,
-1223.48760117483));
#164931=CARTESIAN_POINT('Ctrl Pts',(16.1559070823762,-8.04468584505497,
-1224.98171882189));
#164932=CARTESIAN_POINT('Ctrl Pts',(15.4104571591017,-9.54175110365538,
-1226.47583646895));
#164933=CARTESIAN_POINT('Ctrl Pts',(14.4026149179538,-10.8763499173728,
-1227.969954116));
#164934=CARTESIAN_POINT('Ctrl Pts',(13.3947726768058,-12.2109487310903,
-1229.46407176306));
#164935=CARTESIAN_POINT('Ctrl Pts',(12.1588589765331,-13.3376329379985,
-1230.95818941012));
#164936=CARTESIAN_POINT('Ctrl Pts',(10.9229452762603,-14.4643171449067,
-1232.45230705718));
#164937=CARTESIAN_POINT('Ctrl Pts',(9.50104767561053,-15.3447188656481,
-1233.94642470424));
#164938=CARTESIAN_POINT('Ctrl Pts',(8.07915007496071,-16.2251205863895,
-1235.4405423513));
#164939=CARTESIAN_POINT('Ctrl Pts',(6.51968959134574,-16.8292587962898,
-1236.93465999836));
#164940=CARTESIAN_POINT('Ctrl Pts',(4.96022910773078,-17.4333970061901,
-1238.42877764542));
#164941=CARTESIAN_POINT('Ctrl Pts',(3.31631129755346,-17.7406985030951,
-1239.92289529247));
#164942=CARTESIAN_POINT('Ctrl Pts',(1.67239348737615,-18.048,-1241.41701293953));
#164943=CARTESIAN_POINT('Ctrl Pts',(0.,-18.048,-1242.91113058659));
#164944=CARTESIAN_POINT('Ctrl Pts',(-1.67239348737615,-18.048,-1244.40524823365));
#164945=CARTESIAN_POINT('Ctrl Pts',(-3.31631129755346,-17.7406985030951,
-1245.89936588071));
#164946=CARTESIAN_POINT('Ctrl Pts',(-4.96022910773077,-17.4333970061901,
-1247.39348352777));
#164947=CARTESIAN_POINT('Ctrl Pts',(-6.51968959134574,-16.8292587962898,
-1248.88760117483));
#164948=CARTESIAN_POINT('Ctrl Pts',(-8.07915007496071,-16.2251205863895,
-1250.38171882189));
#164949=CARTESIAN_POINT('Ctrl Pts',(-9.50104767561052,-15.3447188656481,
-1251.87583646895));
#164950=CARTESIAN_POINT('Ctrl Pts',(-10.9229452762603,-14.4643171449067,
-1253.369954116));
#164951=CARTESIAN_POINT('Ctrl Pts',(-12.1588589765331,-13.3376329379985,
-1254.86407176306));
#164952=CARTESIAN_POINT('Ctrl Pts',(-13.3947726768058,-12.2109487310903,
-1256.35818941012));
#164953=CARTESIAN_POINT('Ctrl Pts',(-14.4026149179538,-10.8763499173728,
-1257.85230705718));
#164954=CARTESIAN_POINT('Ctrl Pts',(-15.4104571591017,-9.54175110365538,
-1259.34642470424));
#164955=CARTESIAN_POINT('Ctrl Pts',(-16.1559070823762,-8.04468584505497,
-1260.8405423513));
#164956=CARTESIAN_POINT('Ctrl Pts',(-16.9013570056506,-6.54762058645456,
-1262.33465999836));
#164957=CARTESIAN_POINT('Ctrl Pts',(-17.3590292079831,-4.93906964482095,
-1263.82877764542));
#164958=CARTESIAN_POINT('Ctrl Pts',(-17.8167014103155,-3.33051870318735,
-1265.32289529247));
#164959=CARTESIAN_POINT('Ctrl Pts',(-17.9710104137728,-1.66525935159368,
-1266.81701293953));
#164960=CARTESIAN_POINT('Ctrl Pts',(-18.1253194172301,-1.10985572039171E-15,
-1268.31113058659));
#164961=CARTESIAN_POINT('Ctrl Pts',(-17.9710104137728,1.66525935159367,
-1269.80524823365));
#164962=CARTESIAN_POINT('Ctrl Pts',(-17.8167014103155,3.33051870318735,
-1271.29936588071));
#164963=CARTESIAN_POINT('Ctrl Pts',(-17.3590292079831,4.93906964482096,
-1272.79348352777));
#164964=CARTESIAN_POINT('Ctrl Pts',(-16.9013570056506,6.54762058645456,
-1274.28760117483));
#164965=CARTESIAN_POINT('Ctrl Pts',(-16.1559070823762,8.04468584505497,
-1275.78171882189));
#164966=CARTESIAN_POINT('Ctrl Pts',(-15.4104571591017,9.54175110365538,
-1277.27583646895));
#164967=CARTESIAN_POINT('Ctrl Pts',(-14.4026149179538,10.8763499173728,
-1278.769954116));
#164968=CARTESIAN_POINT('Ctrl Pts',(-13.3947726768058,12.2109487310903,
-1280.26407176306));
#164969=CARTESIAN_POINT('Ctrl Pts',(-12.1588589765331,13.3376329379985,
-1281.75818941012));
#164970=CARTESIAN_POINT('Ctrl Pts',(-10.9229452762603,14.4643171449067,
-1283.25230705718));
#164971=CARTESIAN_POINT('Ctrl Pts',(-9.50104767561052,15.3447188656481,
-1284.74642470424));
#164972=CARTESIAN_POINT('Ctrl Pts',(-8.07915007496071,16.2251205863895,
-1286.2405423513));
#164973=CARTESIAN_POINT('Ctrl Pts',(-6.51968959134574,16.8292587962898,
-1287.73465999836));
#164974=CARTESIAN_POINT('Ctrl Pts',(-4.96022910773078,17.4333970061901,
-1289.22877764542));
#164975=CARTESIAN_POINT('Ctrl Pts',(-3.31631129755346,17.7406985030951,
-1290.72289529247));
#164976=CARTESIAN_POINT('Ctrl Pts',(-1.67239348737615,18.048,-1292.21701293953));
#164977=CARTESIAN_POINT('Ctrl Pts',(-2.21024254310115E-15,18.048,-1293.71113058659));
#164978=CARTESIAN_POINT('Ctrl Pts',(1.67239348737616,18.048,-1295.20524823365));
#164979=CARTESIAN_POINT('Ctrl Pts',(3.31631129755346,17.7406985030951,-1296.69936588071));
#164980=CARTESIAN_POINT('Ctrl Pts',(4.96022910773077,17.4333970061901,-1298.19348352777));
#164981=CARTESIAN_POINT('Ctrl Pts',(6.51968959134575,16.8292587962898,-1299.68760117483));
#164982=CARTESIAN_POINT('Ctrl Pts',(8.07915007496071,16.2251205863895,-1301.18171882189));
#164983=CARTESIAN_POINT('Ctrl Pts',(9.50104767561053,15.3447188656481,-1302.67583646895));
#164984=CARTESIAN_POINT('Ctrl Pts',(10.9229452762603,14.4643171449067,-1304.169954116));
#164985=CARTESIAN_POINT('Ctrl Pts',(12.1588589765331,13.3376329379985,-1305.66407176306));
#164986=CARTESIAN_POINT('Ctrl Pts',(13.3947726768058,12.2109487310903,-1307.15818941012));
#164987=CARTESIAN_POINT('Ctrl Pts',(14.4026149179538,10.8763499173728,-1308.65230705718));
#164988=CARTESIAN_POINT('Ctrl Pts',(15.4104571591017,9.54175110365538,-1310.14642470424));
#164989=CARTESIAN_POINT('Ctrl Pts',(16.1559070823762,8.04468584505496,-1311.6405423513));
#164990=CARTESIAN_POINT('Ctrl Pts',(16.9013570056506,6.54762058645456,-1313.13465999836));
#164991=CARTESIAN_POINT('Ctrl Pts',(17.3590292079831,4.93906964482096,-1314.62877764542));
#164992=CARTESIAN_POINT('Ctrl Pts',(17.8167014103155,3.33051870318735,-1316.12289529247));
#164993=CARTESIAN_POINT('Ctrl Pts',(17.9710104137728,1.66525935159367,-1317.61701293953));
#164994=CARTESIAN_POINT('Ctrl Pts',(18.1253194172301,3.32956716117513E-15,
-1319.11113058659));
#164995=CARTESIAN_POINT('Ctrl Pts',(17.9710104137728,-1.66525935159367,
-1320.60524823365));
#164996=CARTESIAN_POINT('Ctrl Pts',(17.8167014103155,-3.33051870318736,
-1322.09936588071));
#164997=CARTESIAN_POINT('Ctrl Pts',(17.3590292079831,-4.93906964482095,
-1323.59348352777));
#164998=CARTESIAN_POINT('Ctrl Pts',(16.9013570056506,-6.54762058645456,
-1325.08760117483));
#164999=CARTESIAN_POINT('Ctrl Pts',(16.1559070823762,-8.04468584505497,
-1326.58171882189));
#165000=CARTESIAN_POINT('Ctrl Pts',(15.4104571591017,-9.54175110365538,
-1328.07583646895));
#165001=CARTESIAN_POINT('Ctrl Pts',(14.4026149179538,-10.8763499173728,
-1329.569954116));
#165002=CARTESIAN_POINT('Ctrl Pts',(13.3947726768058,-12.2109487310903,
-1331.06407176306));
#165003=CARTESIAN_POINT('Ctrl Pts',(12.1588589765331,-13.3376329379985,
-1332.55818941012));
#165004=CARTESIAN_POINT('Ctrl Pts',(10.9229452762603,-14.4643171449067,
-1334.05230705718));
#165005=CARTESIAN_POINT('Ctrl Pts',(9.50104767561053,-15.3447188656481,
-1335.54642470424));
#165006=CARTESIAN_POINT('Ctrl Pts',(8.07915007496071,-16.2251205863895,
-1337.0405423513));
#165007=CARTESIAN_POINT('Ctrl Pts',(6.51968959134574,-16.8292587962898,
-1338.53465999836));
#165008=CARTESIAN_POINT('Ctrl Pts',(4.96022910773078,-17.4333970061901,
-1340.02877764542));
#165009=CARTESIAN_POINT('Ctrl Pts',(3.31631129755346,-17.7406985030951,
-1341.52289529247));
#165010=CARTESIAN_POINT('Ctrl Pts',(1.67239348737615,-18.048,-1343.01701293953));
#165011=CARTESIAN_POINT('Ctrl Pts',(0.,-18.048,-1344.51113058659));
#165012=CARTESIAN_POINT('Ctrl Pts',(-1.67239348737615,-18.048,-1346.00524823365));
#165013=CARTESIAN_POINT('Ctrl Pts',(-3.31631129755346,-17.7406985030951,
-1347.49936588071));
#165014=CARTESIAN_POINT('Ctrl Pts',(-4.96022910773077,-17.4333970061901,
-1348.99348352777));
#165015=CARTESIAN_POINT('Ctrl Pts',(-6.51968959134574,-16.8292587962898,
-1350.48760117483));
#165016=CARTESIAN_POINT('Ctrl Pts',(-8.07915007496071,-16.2251205863895,
-1351.98171882189));
#165017=CARTESIAN_POINT('Ctrl Pts',(-9.50104767561052,-15.3447188656481,
-1353.47583646895));
#165018=CARTESIAN_POINT('Ctrl Pts',(-10.9229452762603,-14.4643171449067,
-1354.969954116));
#165019=CARTESIAN_POINT('Ctrl Pts',(-12.1588589765331,-13.3376329379985,
-1356.46407176306));
#165020=CARTESIAN_POINT('Ctrl Pts',(-13.3947726768058,-12.2109487310903,
-1357.95818941012));
#165021=CARTESIAN_POINT('Ctrl Pts',(-14.4026149179538,-10.8763499173728,
-1359.45230705718));
#165022=CARTESIAN_POINT('Ctrl Pts',(-15.4104571591017,-9.54175110365538,
-1360.94642470424));
#165023=CARTESIAN_POINT('Ctrl Pts',(-16.1559070823762,-8.04468584505497,
-1362.4405423513));
#165024=CARTESIAN_POINT('Ctrl Pts',(-16.9013570056506,-6.54762058645456,
-1363.93465999836));
#165025=CARTESIAN_POINT('Ctrl Pts',(-17.3590292079831,-4.93906964482095,
-1365.42877764542));
#165026=CARTESIAN_POINT('Ctrl Pts',(-17.8167014103155,-3.33051870318735,
-1366.92289529248));
#165027=CARTESIAN_POINT('Ctrl Pts',(-17.9710104137728,-1.66525935159368,
-1368.41701293953));
#165028=CARTESIAN_POINT('Ctrl Pts',(-18.1253194172301,-1.10985572039171E-15,
-1369.91113058659));
#165029=CARTESIAN_POINT('Ctrl Pts',(-17.9710104137728,1.66525935159367,
-1371.40524823365));
#165030=CARTESIAN_POINT('Ctrl Pts',(-17.8167014103155,3.33051870318735,
-1372.89936588071));
#165031=CARTESIAN_POINT('Ctrl Pts',(-17.3590292079831,4.93906964482096,
-1374.39348352777));
#165032=CARTESIAN_POINT('Ctrl Pts',(-16.9013570056506,6.54762058645456,
-1375.88760117483));
#165033=CARTESIAN_POINT('Ctrl Pts',(-16.1559070823762,8.04468584505497,
-1377.38171882189));
#165034=CARTESIAN_POINT('Ctrl Pts',(-15.4104571591017,9.54175110365538,
-1378.87583646895));
#165035=CARTESIAN_POINT('Ctrl Pts',(-14.4026149179538,10.8763499173728,
-1380.369954116));
#165036=CARTESIAN_POINT('Ctrl Pts',(-13.3947726768058,12.2109487310903,
-1381.86407176306));
#165037=CARTESIAN_POINT('Ctrl Pts',(-12.1588589765331,13.3376329379985,
-1383.35818941012));
#165038=CARTESIAN_POINT('Ctrl Pts',(-10.9229452762603,14.4643171449067,
-1384.85230705718));
#165039=CARTESIAN_POINT('Ctrl Pts',(-9.50104767561052,15.3447188656481,
-1386.34642470424));
#165040=CARTESIAN_POINT('Ctrl Pts',(-8.07915007496071,16.2251205863895,
-1387.8405423513));
#165041=CARTESIAN_POINT('Ctrl Pts',(-6.51968959134574,16.8292587962898,
-1389.33465999836));
#165042=CARTESIAN_POINT('Ctrl Pts',(-4.96022910773078,17.4333970061901,
-1390.82877764542));
#165043=CARTESIAN_POINT('Ctrl Pts',(-3.31631129755346,17.7406985030951,
-1392.32289529247));
#165044=CARTESIAN_POINT('Ctrl Pts',(-1.67239348737615,18.048,-1393.81701293953));
#165045=CARTESIAN_POINT('Ctrl Pts',(-2.21024254310115E-15,18.048,-1395.31113058659));
#165046=CARTESIAN_POINT('Ctrl Pts',(1.67239348737616,18.048,-1396.80524823365));
#165047=CARTESIAN_POINT('Ctrl Pts',(3.31631129755346,17.7406985030951,-1398.29936588071));
#165048=CARTESIAN_POINT('Ctrl Pts',(4.96022910773077,17.4333970061901,-1399.79348352777));
#165049=CARTESIAN_POINT('Ctrl Pts',(6.51968959134575,16.8292587962898,-1401.28760117483));
#165050=CARTESIAN_POINT('Ctrl Pts',(8.07915007496071,16.2251205863895,-1402.78171882189));
#165051=CARTESIAN_POINT('Ctrl Pts',(9.50104767561053,15.3447188656481,-1404.27583646895));
#165052=CARTESIAN_POINT('Ctrl Pts',(10.9229452762603,14.4643171449067,-1405.769954116));
#165053=CARTESIAN_POINT('Ctrl Pts',(12.1588589765331,13.3376329379985,-1407.26407176306));
#165054=CARTESIAN_POINT('Ctrl Pts',(13.3947726768058,12.2109487310903,-1408.75818941012));
#165055=CARTESIAN_POINT('Ctrl Pts',(14.4026149179538,10.8763499173728,-1410.25230705718));
#165056=CARTESIAN_POINT('Ctrl Pts',(15.4104571591017,9.54175110365538,-1411.74642470424));
#165057=CARTESIAN_POINT('Ctrl Pts',(16.1559070823762,8.04468584505496,-1413.2405423513));
#165058=CARTESIAN_POINT('Ctrl Pts',(16.9013570056506,6.54762058645456,-1414.73465999836));
#165059=CARTESIAN_POINT('Ctrl Pts',(17.3590292079831,4.93906964482096,-1416.22877764542));
#165060=CARTESIAN_POINT('Ctrl Pts',(17.8167014103155,3.33051870318735,-1417.72289529247));
#165061=CARTESIAN_POINT('Ctrl Pts',(17.9710104137728,1.66525935159367,-1419.21701293953));
#165062=CARTESIAN_POINT('Ctrl Pts',(18.1253194172301,3.32956716117513E-15,
-1420.71113058659));
#165063=CARTESIAN_POINT('Ctrl Pts',(17.9710104137728,-1.66525935159367,
-1422.20524823365));
#165064=CARTESIAN_POINT('Ctrl Pts',(17.8167014103155,-3.33051870318736,
-1423.69936588071));
#165065=CARTESIAN_POINT('Ctrl Pts',(17.3590292079831,-4.93906964482095,
-1425.19348352777));
#165066=CARTESIAN_POINT('Ctrl Pts',(16.9013570056506,-6.54762058645456,
-1426.68760117483));
#165067=CARTESIAN_POINT('Ctrl Pts',(16.1559070823762,-8.04468584505497,
-1428.18171882189));
#165068=CARTESIAN_POINT('Ctrl Pts',(15.4104571591017,-9.54175110365538,
-1429.67583646895));
#165069=CARTESIAN_POINT('Ctrl Pts',(14.4026149179538,-10.8763499173728,
-1431.169954116));
#165070=CARTESIAN_POINT('Ctrl Pts',(13.3947726768058,-12.2109487310903,
-1432.66407176306));
#165071=CARTESIAN_POINT('Ctrl Pts',(12.1588589765331,-13.3376329379985,
-1434.15818941012));
#165072=CARTESIAN_POINT('Ctrl Pts',(10.9229452762603,-14.4643171449067,
-1435.65230705718));
#165073=CARTESIAN_POINT('Ctrl Pts',(9.50104767561053,-15.3447188656481,
-1437.14642470424));
#165074=CARTESIAN_POINT('Ctrl Pts',(8.07915007496071,-16.2251205863895,
-1438.6405423513));
#165075=CARTESIAN_POINT('Ctrl Pts',(6.51968959134574,-16.8292587962898,
-1440.13465999836));
#165076=CARTESIAN_POINT('Ctrl Pts',(4.96022910773078,-17.4333970061901,
-1441.62877764542));
#165077=CARTESIAN_POINT('Ctrl Pts',(3.31631129755346,-17.7406985030951,
-1443.12289529247));
#165078=CARTESIAN_POINT('Ctrl Pts',(1.67239348737615,-18.048,-1444.61701293953));
#165079=CARTESIAN_POINT('Ctrl Pts',(0.,-18.048,-1446.11113058659));
#165080=CARTESIAN_POINT('Ctrl Pts',(-1.67239348737615,-18.048,-1447.60524823365));
#165081=CARTESIAN_POINT('Ctrl Pts',(-3.31631129755346,-17.7406985030951,
-1449.09936588071));
#165082=CARTESIAN_POINT('Ctrl Pts',(-4.96022910773077,-17.4333970061901,
-1450.59348352777));
#165083=CARTESIAN_POINT('Ctrl Pts',(-6.51968959134574,-16.8292587962898,
-1452.08760117483));
#165084=CARTESIAN_POINT('Ctrl Pts',(-8.07915007496071,-16.2251205863895,
-1453.58171882189));
#165085=CARTESIAN_POINT('Ctrl Pts',(-9.50104767561052,-15.3447188656481,
-1455.07583646895));
#165086=CARTESIAN_POINT('Ctrl Pts',(-10.9229452762603,-14.4643171449067,
-1456.569954116));
#165087=CARTESIAN_POINT('Ctrl Pts',(-12.1588589765331,-13.3376329379985,
-1458.06407176306));
#165088=CARTESIAN_POINT('Ctrl Pts',(-13.3947726768058,-12.2109487310903,
-1459.55818941012));
#165089=CARTESIAN_POINT('Ctrl Pts',(-14.4026149179538,-10.8763499173728,
-1461.05230705718));
#165090=CARTESIAN_POINT('Ctrl Pts',(-15.4104571591017,-9.54175110365538,
-1462.54642470424));
#165091=CARTESIAN_POINT('Ctrl Pts',(-16.1559070823762,-8.04468584505497,
-1464.0405423513));
#165092=CARTESIAN_POINT('Ctrl Pts',(-16.9013570056506,-6.54762058645456,
-1465.53465999836));
#165093=CARTESIAN_POINT('Ctrl Pts',(-17.3590292079831,-4.93906964482095,
-1467.02877764542));
#165094=CARTESIAN_POINT('Ctrl Pts',(-17.8167014103155,-3.33051870318735,
-1468.52289529247));
#165095=CARTESIAN_POINT('Ctrl Pts',(-17.9710104137728,-1.66525935159368,
-1470.01701293953));
#165096=CARTESIAN_POINT('Ctrl Pts',(-18.1253194172301,-1.10985572039171E-15,
-1471.51113058659));
#165097=CARTESIAN_POINT('Ctrl Pts',(-17.9710104137728,1.66525935159367,
-1473.00524823365));
#165098=CARTESIAN_POINT('Ctrl Pts',(-17.8167014103155,3.33051870318735,
-1474.49936588071));
#165099=CARTESIAN_POINT('Ctrl Pts',(-17.3590292079831,4.93906964482096,
-1475.99348352777));
#165100=CARTESIAN_POINT('Ctrl Pts',(-16.9013570056506,6.54762058645456,
-1477.48760117483));
#165101=CARTESIAN_POINT('Ctrl Pts',(-16.1559070823762,8.04468584505497,
-1478.98171882189));
#165102=CARTESIAN_POINT('Ctrl Pts',(-15.4104571591017,9.54175110365538,
-1480.47583646895));
#165103=CARTESIAN_POINT('Ctrl Pts',(-14.4026149179538,10.8763499173728,
-1481.969954116));
#165104=CARTESIAN_POINT('Ctrl Pts',(-13.3947726768058,12.2109487310903,
-1483.46407176306));
#165105=CARTESIAN_POINT('Ctrl Pts',(-12.1588589765331,13.3376329379985,
-1484.95818941012));
#165106=CARTESIAN_POINT('Ctrl Pts',(-10.9229452762603,14.4643171449067,
-1486.45230705718));
#165107=CARTESIAN_POINT('Ctrl Pts',(-9.50104767561052,15.3447188656481,
-1487.94642470424));
#165108=CARTESIAN_POINT('Ctrl Pts',(-8.07915007496071,16.2251205863895,
-1489.4405423513));
#165109=CARTESIAN_POINT('Ctrl Pts',(-6.51968959134574,16.8292587962898,
-1490.93465999836));
#165110=CARTESIAN_POINT('Ctrl Pts',(-4.96022910773078,17.4333970061901,
-1492.42877764542));
#165111=CARTESIAN_POINT('Ctrl Pts',(-3.31631129755346,17.7406985030951,
-1493.92289529247));
#165112=CARTESIAN_POINT('Ctrl Pts',(-1.67239348737615,18.048,-1495.41701293953));
#165113=CARTESIAN_POINT('Ctrl Pts',(-2.21024254310115E-15,18.048,-1496.91113058659));
#165114=CARTESIAN_POINT('Ctrl Pts',(1.67239348737616,18.048,-1498.40524823365));
#165115=CARTESIAN_POINT('Ctrl Pts',(3.31631129755346,17.7406985030951,-1499.89936588071));
#165116=CARTESIAN_POINT('Ctrl Pts',(4.96022910773077,17.4333970061901,-1501.39348352777));
#165117=CARTESIAN_POINT('Ctrl Pts',(6.51968959134575,16.8292587962898,-1502.88760117483));
#165118=CARTESIAN_POINT('Ctrl Pts',(7.54128438222173,16.4334908658498,-1503.86639019913));
#165119=CARTESIAN_POINT('Ctrl Pts',(8.50750525179015,15.9170555816949,-1504.84896316329));
#165120=CARTESIAN_POINT('Ctrl Pts',(23.3054664377218,8.00769496792138,-1519.89736156162));
#165121=CARTESIAN_POINT('Ctrl Pts',(38.1034276236535,0.0983343541478931,
-1534.94575995995));
#165122=CARTESIAN_POINT('Ctrl Pts',(0.,-18.048,1500.1875));
#165123=CARTESIAN_POINT('Ctrl Pts',(-1.67239348737615,-18.048,1498.69338235294));
#165124=CARTESIAN_POINT('Ctrl Pts',(-3.31631129755346,-17.7406985030951,
1497.19926470588));
#165125=CARTESIAN_POINT('Ctrl Pts',(-4.96022910773077,-17.4333970061901,
1495.70514705882));
#165126=CARTESIAN_POINT('Ctrl Pts',(-6.51968959134574,-16.8292587962898,
1494.21102941176));
#165127=CARTESIAN_POINT('Ctrl Pts',(-8.07915007496071,-16.2251205863895,
1492.71691176471));
#165128=CARTESIAN_POINT('Ctrl Pts',(-9.50104767561052,-15.3447188656481,
1491.22279411765));
#165129=CARTESIAN_POINT('Ctrl Pts',(-10.9229452762603,-14.4643171449067,
1489.72867647059));
#165130=CARTESIAN_POINT('Ctrl Pts',(-12.1588589765331,-13.3376329379985,
1488.23455882353));
#165131=CARTESIAN_POINT('Ctrl Pts',(-13.3947726768058,-12.2109487310903,
1486.74044117647));
#165132=CARTESIAN_POINT('Ctrl Pts',(-14.4026149179538,-10.8763499173728,
1485.24632352941));
#165133=CARTESIAN_POINT('Ctrl Pts',(-15.4104571591017,-9.54175110365538,
1483.75220588235));
#165134=CARTESIAN_POINT('Ctrl Pts',(-16.1559070823762,-8.04468584505497,
1482.25808823529));
#165135=CARTESIAN_POINT('Ctrl Pts',(-16.9013570056506,-6.54762058645456,
1480.76397058824));
#165136=CARTESIAN_POINT('Ctrl Pts',(-17.3590292079831,-4.93906964482095,
1479.26985294118));
#165137=CARTESIAN_POINT('Ctrl Pts',(-17.8167014103155,-3.33051870318735,
1477.77573529412));
#165138=CARTESIAN_POINT('Ctrl Pts',(-17.9710104137728,-1.66525935159368,
1476.28161764706));
#165139=CARTESIAN_POINT('Ctrl Pts',(-18.1253194172301,-1.10985572039171E-15,
1474.7875));
#165140=CARTESIAN_POINT('Ctrl Pts',(-17.9710104137728,1.66525935159367,
1473.29338235294));
#165141=CARTESIAN_POINT('Ctrl Pts',(-17.8167014103155,3.33051870318735,
1471.79926470588));
#165142=CARTESIAN_POINT('Ctrl Pts',(-17.3590292079831,4.93906964482096,
1470.30514705882));
#165143=CARTESIAN_POINT('Ctrl Pts',(-16.9013570056506,6.54762058645456,
1468.81102941177));
#165144=CARTESIAN_POINT('Ctrl Pts',(-16.1559070823762,8.04468584505497,
1467.31691176471));
#165145=CARTESIAN_POINT('Ctrl Pts',(-15.4104571591017,9.54175110365538,
1465.82279411765));
#165146=CARTESIAN_POINT('Ctrl Pts',(-14.4026149179538,10.8763499173728,
1464.32867647059));
#165147=CARTESIAN_POINT('Ctrl Pts',(-13.3947726768058,12.2109487310903,
1462.83455882353));
#165148=CARTESIAN_POINT('Ctrl Pts',(-12.1588589765331,13.3376329379985,
1461.34044117647));
#165149=CARTESIAN_POINT('Ctrl Pts',(-10.9229452762603,14.4643171449067,
1459.84632352941));
#165150=CARTESIAN_POINT('Ctrl Pts',(-9.50104767561052,15.3447188656481,
1458.35220588235));
#165151=CARTESIAN_POINT('Ctrl Pts',(-8.07915007496071,16.2251205863895,
1456.85808823529));
#165152=CARTESIAN_POINT('Ctrl Pts',(-6.51968959134574,16.8292587962898,
1455.36397058824));
#165153=CARTESIAN_POINT('Ctrl Pts',(-4.96022910773078,17.4333970061901,
1453.86985294118));
#165154=CARTESIAN_POINT('Ctrl Pts',(-3.31631129755346,17.7406985030951,
1452.37573529412));
#165155=CARTESIAN_POINT('Ctrl Pts',(-1.67239348737615,18.048,1450.88161764706));
#165156=CARTESIAN_POINT('Ctrl Pts',(-2.21024254310115E-15,18.048,1449.3875));
#165157=CARTESIAN_POINT('Ctrl Pts',(1.67239348737616,18.048,1447.89338235294));
#165158=CARTESIAN_POINT('Ctrl Pts',(3.31631129755346,17.7406985030951,1446.39926470588));
#165159=CARTESIAN_POINT('Ctrl Pts',(4.96022910773077,17.4333970061901,1444.90514705882));
#165160=CARTESIAN_POINT('Ctrl Pts',(6.51968959134575,16.8292587962898,1443.41102941176));
#165161=CARTESIAN_POINT('Ctrl Pts',(8.07915007496071,16.2251205863895,1441.91691176471));
#165162=CARTESIAN_POINT('Ctrl Pts',(9.50104767561053,15.3447188656481,1440.42279411765));
#165163=CARTESIAN_POINT('Ctrl Pts',(10.9229452762603,14.4643171449067,1438.92867647059));
#165164=CARTESIAN_POINT('Ctrl Pts',(12.1588589765331,13.3376329379985,1437.43455882353));
#165165=CARTESIAN_POINT('Ctrl Pts',(13.3947726768058,12.2109487310903,1435.94044117647));
#165166=CARTESIAN_POINT('Ctrl Pts',(14.4026149179538,10.8763499173728,1434.44632352941));
#165167=CARTESIAN_POINT('Ctrl Pts',(15.4104571591017,9.54175110365538,1432.95220588235));
#165168=CARTESIAN_POINT('Ctrl Pts',(16.1559070823762,8.04468584505496,1431.45808823529));
#165169=CARTESIAN_POINT('Ctrl Pts',(16.9013570056506,6.54762058645456,1429.96397058824));
#165170=CARTESIAN_POINT('Ctrl Pts',(17.3590292079831,4.93906964482096,1428.46985294118));
#165171=CARTESIAN_POINT('Ctrl Pts',(17.8167014103155,3.33051870318735,1426.97573529412));
#165172=CARTESIAN_POINT('Ctrl Pts',(17.9710104137728,1.66525935159367,1425.48161764706));
#165173=CARTESIAN_POINT('Ctrl Pts',(18.1253194172301,3.32956716117513E-15,
1423.9875));
#165174=CARTESIAN_POINT('Ctrl Pts',(17.9710104137728,-1.66525935159367,
1422.49338235294));
#165175=CARTESIAN_POINT('Ctrl Pts',(17.8167014103155,-3.33051870318736,
1420.99926470588));
#165176=CARTESIAN_POINT('Ctrl Pts',(17.3590292079831,-4.93906964482095,
1419.50514705882));
#165177=CARTESIAN_POINT('Ctrl Pts',(16.9013570056506,-6.54762058645456,
1418.01102941176));
#165178=CARTESIAN_POINT('Ctrl Pts',(16.1559070823762,-8.04468584505497,
1416.51691176471));
#165179=CARTESIAN_POINT('Ctrl Pts',(15.4104571591017,-9.54175110365538,
1415.02279411765));
#165180=CARTESIAN_POINT('Ctrl Pts',(14.4026149179538,-10.8763499173728,
1413.52867647059));
#165181=CARTESIAN_POINT('Ctrl Pts',(13.3947726768058,-12.2109487310903,
1412.03455882353));
#165182=CARTESIAN_POINT('Ctrl Pts',(12.1588589765331,-13.3376329379985,
1410.54044117647));
#165183=CARTESIAN_POINT('Ctrl Pts',(10.9229452762603,-14.4643171449067,
1409.04632352941));
#165184=CARTESIAN_POINT('Ctrl Pts',(9.50104767561053,-15.3447188656481,
1407.55220588235));
#165185=CARTESIAN_POINT('Ctrl Pts',(8.07915007496071,-16.2251205863895,
1406.05808823529));
#165186=CARTESIAN_POINT('Ctrl Pts',(6.51968959134574,-16.8292587962898,
1404.56397058824));
#165187=CARTESIAN_POINT('Ctrl Pts',(4.96022910773078,-17.4333970061901,
1403.06985294118));
#165188=CARTESIAN_POINT('Ctrl Pts',(3.31631129755346,-17.7406985030951,
1401.57573529412));
#165189=CARTESIAN_POINT('Ctrl Pts',(1.67239348737615,-18.048,1400.08161764706));
#165190=CARTESIAN_POINT('Ctrl Pts',(0.,-18.048,1398.5875));
#165191=CARTESIAN_POINT('Ctrl Pts',(-1.67239348737615,-18.048,1397.09338235294));
#165192=CARTESIAN_POINT('Ctrl Pts',(-3.31631129755346,-17.7406985030951,
1395.59926470588));
#165193=CARTESIAN_POINT('Ctrl Pts',(-4.96022910773077,-17.4333970061901,
1394.10514705882));
#165194=CARTESIAN_POINT('Ctrl Pts',(-6.51968959134574,-16.8292587962898,
1392.61102941176));
#165195=CARTESIAN_POINT('Ctrl Pts',(-8.07915007496071,-16.2251205863895,
1391.11691176471));
#165196=CARTESIAN_POINT('Ctrl Pts',(-9.50104767561052,-15.3447188656481,
1389.62279411765));
#165197=CARTESIAN_POINT('Ctrl Pts',(-10.9229452762603,-14.4643171449067,
1388.12867647059));
#165198=CARTESIAN_POINT('Ctrl Pts',(-12.1588589765331,-13.3376329379985,
1386.63455882353));
#165199=CARTESIAN_POINT('Ctrl Pts',(-13.3947726768058,-12.2109487310903,
1385.14044117647));
#165200=CARTESIAN_POINT('Ctrl Pts',(-14.4026149179538,-10.8763499173728,
1383.64632352941));
#165201=CARTESIAN_POINT('Ctrl Pts',(-15.4104571591017,-9.54175110365538,
1382.15220588235));
#165202=CARTESIAN_POINT('Ctrl Pts',(-16.1559070823762,-8.04468584505497,
1380.65808823529));
#165203=CARTESIAN_POINT('Ctrl Pts',(-16.9013570056506,-6.54762058645456,
1379.16397058824));
#165204=CARTESIAN_POINT('Ctrl Pts',(-17.3590292079831,-4.93906964482095,
1377.66985294118));
#165205=CARTESIAN_POINT('Ctrl Pts',(-17.8167014103155,-3.33051870318735,
1376.17573529412));
#165206=CARTESIAN_POINT('Ctrl Pts',(-17.9710104137728,-1.66525935159368,
1374.68161764706));
#165207=CARTESIAN_POINT('Ctrl Pts',(-18.1253194172301,-1.10985572039171E-15,
1373.1875));
#165208=CARTESIAN_POINT('Ctrl Pts',(-17.9710104137728,1.66525935159367,
1371.69338235294));
#165209=CARTESIAN_POINT('Ctrl Pts',(-17.8167014103155,3.33051870318735,
1370.19926470588));
#165210=CARTESIAN_POINT('Ctrl Pts',(-17.3590292079831,4.93906964482096,
1368.70514705882));
#165211=CARTESIAN_POINT('Ctrl Pts',(-16.9013570056506,6.54762058645456,
1367.21102941176));
#165212=CARTESIAN_POINT('Ctrl Pts',(-16.1559070823762,8.04468584505497,
1365.71691176471));
#165213=CARTESIAN_POINT('Ctrl Pts',(-15.4104571591017,9.54175110365538,
1364.22279411765));
#165214=CARTESIAN_POINT('Ctrl Pts',(-14.4026149179538,10.8763499173728,
1362.72867647059));
#165215=CARTESIAN_POINT('Ctrl Pts',(-13.3947726768058,12.2109487310903,
1361.23455882353));
#165216=CARTESIAN_POINT('Ctrl Pts',(-12.1588589765331,13.3376329379985,
1359.74044117647));
#165217=CARTESIAN_POINT('Ctrl Pts',(-10.9229452762603,14.4643171449067,
1358.24632352941));
#165218=CARTESIAN_POINT('Ctrl Pts',(-9.50104767561052,15.3447188656481,
1356.75220588235));
#165219=CARTESIAN_POINT('Ctrl Pts',(-8.07915007496071,16.2251205863895,
1355.25808823529));
#165220=CARTESIAN_POINT('Ctrl Pts',(-6.51968959134574,16.8292587962898,
1353.76397058824));
#165221=CARTESIAN_POINT('Ctrl Pts',(-4.96022910773078,17.4333970061901,
1352.26985294118));
#165222=CARTESIAN_POINT('Ctrl Pts',(-3.31631129755346,17.7406985030951,
1350.77573529412));
#165223=CARTESIAN_POINT('Ctrl Pts',(-1.67239348737615,18.048,1349.28161764706));
#165224=CARTESIAN_POINT('Ctrl Pts',(-2.21024254310115E-15,18.048,1347.7875));
#165225=CARTESIAN_POINT('Ctrl Pts',(1.67239348737616,18.048,1346.29338235294));
#165226=CARTESIAN_POINT('Ctrl Pts',(3.31631129755346,17.7406985030951,1344.79926470588));
#165227=CARTESIAN_POINT('Ctrl Pts',(4.96022910773077,17.4333970061901,1343.30514705882));
#165228=CARTESIAN_POINT('Ctrl Pts',(6.51968959134575,16.8292587962898,1341.81102941176));
#165229=CARTESIAN_POINT('Ctrl Pts',(8.07915007496071,16.2251205863895,1340.31691176471));
#165230=CARTESIAN_POINT('Ctrl Pts',(9.50104767561053,15.3447188656481,1338.82279411765));
#165231=CARTESIAN_POINT('Ctrl Pts',(10.9229452762603,14.4643171449067,1337.32867647059));
#165232=CARTESIAN_POINT('Ctrl Pts',(12.1588589765331,13.3376329379985,1335.83455882353));
#165233=CARTESIAN_POINT('Ctrl Pts',(13.3947726768058,12.2109487310903,1334.34044117647));
#165234=CARTESIAN_POINT('Ctrl Pts',(14.4026149179538,10.8763499173728,1332.84632352941));
#165235=CARTESIAN_POINT('Ctrl Pts',(15.4104571591017,9.54175110365538,1331.35220588235));
#165236=CARTESIAN_POINT('Ctrl Pts',(16.1559070823762,8.04468584505496,1329.85808823529));
#165237=CARTESIAN_POINT('Ctrl Pts',(16.9013570056506,6.54762058645456,1328.36397058824));
#165238=CARTESIAN_POINT('Ctrl Pts',(17.3590292079831,4.93906964482096,1326.86985294118));
#165239=CARTESIAN_POINT('Ctrl Pts',(17.8167014103155,3.33051870318735,1325.37573529412));
#165240=CARTESIAN_POINT('Ctrl Pts',(17.9710104137728,1.66525935159367,1323.88161764706));
#165241=CARTESIAN_POINT('Ctrl Pts',(18.1253194172301,3.32956716117513E-15,
1322.3875));
#165242=CARTESIAN_POINT('Ctrl Pts',(17.9710104137728,-1.66525935159367,
1320.89338235294));
#165243=CARTESIAN_POINT('Ctrl Pts',(17.8167014103155,-3.33051870318736,
1319.39926470588));
#165244=CARTESIAN_POINT('Ctrl Pts',(17.3590292079831,-4.93906964482095,
1317.90514705882));
#165245=CARTESIAN_POINT('Ctrl Pts',(16.9013570056506,-6.54762058645456,
1316.41102941176));
#165246=CARTESIAN_POINT('Ctrl Pts',(16.1559070823762,-8.04468584505497,
1314.91691176471));
#165247=CARTESIAN_POINT('Ctrl Pts',(15.4104571591017,-9.54175110365538,
1313.42279411765));
#165248=CARTESIAN_POINT('Ctrl Pts',(14.4026149179538,-10.8763499173728,
1311.92867647059));
#165249=CARTESIAN_POINT('Ctrl Pts',(13.3947726768058,-12.2109487310903,
1310.43455882353));
#165250=CARTESIAN_POINT('Ctrl Pts',(12.1588589765331,-13.3376329379985,
1308.94044117647));
#165251=CARTESIAN_POINT('Ctrl Pts',(10.9229452762603,-14.4643171449067,
1307.44632352941));
#165252=CARTESIAN_POINT('Ctrl Pts',(9.50104767561053,-15.3447188656481,
1305.95220588235));
#165253=CARTESIAN_POINT('Ctrl Pts',(8.07915007496071,-16.2251205863895,
1304.45808823529));
#165254=CARTESIAN_POINT('Ctrl Pts',(6.51968959134574,-16.8292587962898,
1302.96397058824));
#165255=CARTESIAN_POINT('Ctrl Pts',(4.96022910773078,-17.4333970061901,
1301.46985294118));
#165256=CARTESIAN_POINT('Ctrl Pts',(3.31631129755346,-17.7406985030951,
1299.97573529412));
#165257=CARTESIAN_POINT('Ctrl Pts',(1.67239348737615,-18.048,1298.48161764706));
#165258=CARTESIAN_POINT('Ctrl Pts',(0.,-18.048,1296.9875));
#165259=CARTESIAN_POINT('Ctrl Pts',(-1.67239348737615,-18.048,1295.49338235294));
#165260=CARTESIAN_POINT('Ctrl Pts',(-3.31631129755346,-17.7406985030951,
1293.99926470588));
#165261=CARTESIAN_POINT('Ctrl Pts',(-4.96022910773077,-17.4333970061901,
1292.50514705882));
#165262=CARTESIAN_POINT('Ctrl Pts',(-6.51968959134574,-16.8292587962898,
1291.01102941176));
#165263=CARTESIAN_POINT('Ctrl Pts',(-8.07915007496071,-16.2251205863895,
1289.51691176471));
#165264=CARTESIAN_POINT('Ctrl Pts',(-9.50104767561052,-15.3447188656481,
1288.02279411765));
#165265=CARTESIAN_POINT('Ctrl Pts',(-10.9229452762603,-14.4643171449067,
1286.52867647059));
#165266=CARTESIAN_POINT('Ctrl Pts',(-12.1588589765331,-13.3376329379985,
1285.03455882353));
#165267=CARTESIAN_POINT('Ctrl Pts',(-13.3947726768058,-12.2109487310903,
1283.54044117647));
#165268=CARTESIAN_POINT('Ctrl Pts',(-14.4026149179538,-10.8763499173728,
1282.04632352941));
#165269=CARTESIAN_POINT('Ctrl Pts',(-15.4104571591017,-9.54175110365538,
1280.55220588235));
#165270=CARTESIAN_POINT('Ctrl Pts',(-16.1559070823762,-8.04468584505497,
1279.05808823529));
#165271=CARTESIAN_POINT('Ctrl Pts',(-16.9013570056506,-6.54762058645456,
1277.56397058824));
#165272=CARTESIAN_POINT('Ctrl Pts',(-17.3590292079831,-4.93906964482095,
1276.06985294118));
#165273=CARTESIAN_POINT('Ctrl Pts',(-17.8167014103155,-3.33051870318735,
1274.57573529412));
#165274=CARTESIAN_POINT('Ctrl Pts',(-17.9710104137728,-1.66525935159368,
1273.08161764706));
#165275=CARTESIAN_POINT('Ctrl Pts',(-18.1253194172301,-1.10985572039171E-15,
1271.5875));
#165276=CARTESIAN_POINT('Ctrl Pts',(-17.9710104137728,1.66525935159367,
1270.09338235294));
#165277=CARTESIAN_POINT('Ctrl Pts',(-17.8167014103155,3.33051870318735,
1268.59926470588));
#165278=CARTESIAN_POINT('Ctrl Pts',(-17.3590292079831,4.93906964482096,
1267.10514705882));
#165279=CARTESIAN_POINT('Ctrl Pts',(-16.9013570056506,6.54762058645456,
1265.61102941176));
#165280=CARTESIAN_POINT('Ctrl Pts',(-16.1559070823762,8.04468584505497,
1264.11691176471));
#165281=CARTESIAN_POINT('Ctrl Pts',(-15.4104571591017,9.54175110365538,
1262.62279411765));
#165282=CARTESIAN_POINT('Ctrl Pts',(-14.4026149179538,10.8763499173728,
1261.12867647059));
#165283=CARTESIAN_POINT('Ctrl Pts',(-13.3947726768058,12.2109487310903,
1259.63455882353));
#165284=CARTESIAN_POINT('Ctrl Pts',(-12.1588589765331,13.3376329379985,
1258.14044117647));
#165285=CARTESIAN_POINT('Ctrl Pts',(-10.9229452762603,14.4643171449067,
1256.64632352941));
#165286=CARTESIAN_POINT('Ctrl Pts',(-9.50104767561052,15.3447188656481,
1255.15220588235));
#165287=CARTESIAN_POINT('Ctrl Pts',(-8.07915007496071,16.2251205863895,
1253.65808823529));
#165288=CARTESIAN_POINT('Ctrl Pts',(-6.51968959134574,16.8292587962898,
1252.16397058824));
#165289=CARTESIAN_POINT('Ctrl Pts',(-4.96022910773078,17.4333970061901,
1250.66985294118));
#165290=CARTESIAN_POINT('Ctrl Pts',(-3.31631129755346,17.7406985030951,
1249.17573529412));
#165291=CARTESIAN_POINT('Ctrl Pts',(-1.67239348737615,18.048,1247.68161764706));
#165292=CARTESIAN_POINT('Ctrl Pts',(-2.21024254310115E-15,18.048,1246.1875));
#165293=CARTESIAN_POINT('Ctrl Pts',(1.67239348737616,18.048,1244.69338235294));
#165294=CARTESIAN_POINT('Ctrl Pts',(3.31631129755346,17.7406985030951,1243.19926470588));
#165295=CARTESIAN_POINT('Ctrl Pts',(4.96022910773077,17.4333970061901,1241.70514705882));
#165296=CARTESIAN_POINT('Ctrl Pts',(6.51968959134575,16.8292587962898,1240.21102941176));
#165297=CARTESIAN_POINT('Ctrl Pts',(8.07915007496071,16.2251205863895,1238.71691176471));
#165298=CARTESIAN_POINT('Ctrl Pts',(9.50104767561053,15.3447188656481,1237.22279411765));
#165299=CARTESIAN_POINT('Ctrl Pts',(10.9229452762603,14.4643171449067,1235.72867647059));
#165300=CARTESIAN_POINT('Ctrl Pts',(12.1588589765331,13.3376329379985,1234.23455882353));
#165301=CARTESIAN_POINT('Ctrl Pts',(13.3947726768058,12.2109487310903,1232.74044117647));
#165302=CARTESIAN_POINT('Ctrl Pts',(14.4026149179538,10.8763499173728,1231.24632352941));
#165303=CARTESIAN_POINT('Ctrl Pts',(15.4104571591017,9.54175110365538,1229.75220588235));
#165304=CARTESIAN_POINT('Ctrl Pts',(16.1559070823762,8.04468584505496,1228.25808823529));
#165305=CARTESIAN_POINT('Ctrl Pts',(16.9013570056506,6.54762058645456,1226.76397058824));
#165306=CARTESIAN_POINT('Ctrl Pts',(17.3590292079831,4.93906964482096,1225.26985294118));
#165307=CARTESIAN_POINT('Ctrl Pts',(17.8167014103155,3.33051870318735,1223.77573529412));
#165308=CARTESIAN_POINT('Ctrl Pts',(17.9710104137728,1.66525935159367,1222.28161764706));
#165309=CARTESIAN_POINT('Ctrl Pts',(18.1253194172301,3.32956716117513E-15,
1220.7875));
#165310=CARTESIAN_POINT('Ctrl Pts',(17.9710104137728,-1.66525935159367,
1219.29338235294));
#165311=CARTESIAN_POINT('Ctrl Pts',(17.8167014103155,-3.33051870318736,
1217.79926470588));
#165312=CARTESIAN_POINT('Ctrl Pts',(17.3590292079831,-4.93906964482095,
1216.30514705882));
#165313=CARTESIAN_POINT('Ctrl Pts',(16.9013570056506,-6.54762058645456,
1214.81102941176));
#165314=CARTESIAN_POINT('Ctrl Pts',(16.1559070823762,-8.04468584505497,
1213.31691176471));
#165315=CARTESIAN_POINT('Ctrl Pts',(15.4104571591017,-9.54175110365538,
1211.82279411765));
#165316=CARTESIAN_POINT('Ctrl Pts',(14.4026149179538,-10.8763499173728,
1210.32867647059));
#165317=CARTESIAN_POINT('Ctrl Pts',(13.3947726768058,-12.2109487310903,
1208.83455882353));
#165318=CARTESIAN_POINT('Ctrl Pts',(12.1588589765331,-13.3376329379985,
1207.34044117647));
#165319=CARTESIAN_POINT('Ctrl Pts',(10.9229452762603,-14.4643171449067,
1205.84632352941));
#165320=CARTESIAN_POINT('Ctrl Pts',(9.50104767561053,-15.3447188656481,
1204.35220588235));
#165321=CARTESIAN_POINT('Ctrl Pts',(8.07915007496071,-16.2251205863895,
1202.85808823529));
#165322=CARTESIAN_POINT('Ctrl Pts',(6.51968959134574,-16.8292587962898,
1201.36397058824));
#165323=CARTESIAN_POINT('Ctrl Pts',(4.96022910773078,-17.4333970061901,
1199.86985294118));
#165324=CARTESIAN_POINT('Ctrl Pts',(3.31631129755346,-17.7406985030951,
1198.37573529412));
#165325=CARTESIAN_POINT('Ctrl Pts',(1.67239348737615,-18.048,1196.88161764706));
#165326=CARTESIAN_POINT('Ctrl Pts',(0.,-18.048,1195.3875));
#165327=CARTESIAN_POINT('Ctrl Pts',(-1.67239348737615,-18.048,1193.89338235294));
#165328=CARTESIAN_POINT('Ctrl Pts',(-3.31631129755346,-17.7406985030951,
1192.39926470588));
#165329=CARTESIAN_POINT('Ctrl Pts',(-4.96022910773077,-17.4333970061901,
1190.90514705882));
#165330=CARTESIAN_POINT('Ctrl Pts',(-6.51968959134574,-16.8292587962898,
1189.41102941176));
#165331=CARTESIAN_POINT('Ctrl Pts',(-8.07915007496071,-16.2251205863895,
1187.91691176471));
#165332=CARTESIAN_POINT('Ctrl Pts',(-9.50104767561052,-15.3447188656481,
1186.42279411765));
#165333=CARTESIAN_POINT('Ctrl Pts',(-10.9229452762603,-14.4643171449067,
1184.92867647059));
#165334=CARTESIAN_POINT('Ctrl Pts',(-12.1588589765331,-13.3376329379985,
1183.43455882353));
#165335=CARTESIAN_POINT('Ctrl Pts',(-13.3947726768058,-12.2109487310903,
1181.94044117647));
#165336=CARTESIAN_POINT('Ctrl Pts',(-14.4026149179538,-10.8763499173728,
1180.44632352941));
#165337=CARTESIAN_POINT('Ctrl Pts',(-15.4104571591017,-9.54175110365538,
1178.95220588235));
#165338=CARTESIAN_POINT('Ctrl Pts',(-16.1559070823762,-8.04468584505497,
1177.45808823529));
#165339=CARTESIAN_POINT('Ctrl Pts',(-16.9013570056506,-6.54762058645456,
1175.96397058824));
#165340=CARTESIAN_POINT('Ctrl Pts',(-17.3590292079831,-4.93906964482095,
1174.46985294118));
#165341=CARTESIAN_POINT('Ctrl Pts',(-17.8167014103155,-3.33051870318735,
1172.97573529412));
#165342=CARTESIAN_POINT('Ctrl Pts',(-17.9710104137728,-1.66525935159368,
1171.48161764706));
#165343=CARTESIAN_POINT('Ctrl Pts',(-18.1253194172301,-1.10985572039171E-15,
1169.9875));
#165344=CARTESIAN_POINT('Ctrl Pts',(-17.9710104137728,1.66525935159367,
1168.49338235294));
#165345=CARTESIAN_POINT('Ctrl Pts',(-17.8167014103155,3.33051870318735,
1166.99926470588));
#165346=CARTESIAN_POINT('Ctrl Pts',(-17.3590292079831,4.93906964482096,
1165.50514705882));
#165347=CARTESIAN_POINT('Ctrl Pts',(-16.9013570056506,6.54762058645456,
1164.01102941176));
#165348=CARTESIAN_POINT('Ctrl Pts',(-16.1559070823762,8.04468584505497,
1162.51691176471));
#165349=CARTESIAN_POINT('Ctrl Pts',(-15.4104571591017,9.54175110365538,
1161.02279411765));
#165350=CARTESIAN_POINT('Ctrl Pts',(-14.4026149179538,10.8763499173728,
1159.52867647059));
#165351=CARTESIAN_POINT('Ctrl Pts',(-13.3947726768058,12.2109487310903,
1158.03455882353));
#165352=CARTESIAN_POINT('Ctrl Pts',(-12.1588589765331,13.3376329379985,
1156.54044117647));
#165353=CARTESIAN_POINT('Ctrl Pts',(-10.9229452762603,14.4643171449067,
1155.04632352941));
#165354=CARTESIAN_POINT('Ctrl Pts',(-9.50104767561052,15.3447188656481,
1153.55220588235));
#165355=CARTESIAN_POINT('Ctrl Pts',(-8.07915007496071,16.2251205863895,
1152.05808823529));
#165356=CARTESIAN_POINT('Ctrl Pts',(-6.51968959134574,16.8292587962898,
1150.56397058824));
#165357=CARTESIAN_POINT('Ctrl Pts',(-4.96022910773078,17.4333970061901,
1149.06985294118));
#165358=CARTESIAN_POINT('Ctrl Pts',(-3.31631129755346,17.7406985030951,
1147.57573529412));
#165359=CARTESIAN_POINT('Ctrl Pts',(-1.67239348737615,18.048,1146.08161764706));
#165360=CARTESIAN_POINT('Ctrl Pts',(-2.21024254310115E-15,18.048,1144.5875));
#165361=CARTESIAN_POINT('Ctrl Pts',(1.67239348737616,18.048,1143.09338235294));
#165362=CARTESIAN_POINT('Ctrl Pts',(3.31631129755346,17.7406985030951,1141.59926470588));
#165363=CARTESIAN_POINT('Ctrl Pts',(4.96022910773077,17.4333970061901,1140.10514705882));
#165364=CARTESIAN_POINT('Ctrl Pts',(6.51968959134575,16.8292587962898,1138.61102941176));
#165365=CARTESIAN_POINT('Ctrl Pts',(8.07915007496071,16.2251205863895,1137.11691176471));
#165366=CARTESIAN_POINT('Ctrl Pts',(9.50104767561053,15.3447188656481,1135.62279411765));
#165367=CARTESIAN_POINT('Ctrl Pts',(10.9229452762603,14.4643171449067,1134.12867647059));
#165368=CARTESIAN_POINT('Ctrl Pts',(12.1588589765331,13.3376329379985,1132.63455882353));
#165369=CARTESIAN_POINT('Ctrl Pts',(13.3947726768058,12.2109487310903,1131.14044117647));
#165370=CARTESIAN_POINT('Ctrl Pts',(14.4026149179538,10.8763499173728,1129.64632352941));
#165371=CARTESIAN_POINT('Ctrl Pts',(15.4104571591017,9.54175110365538,1128.15220588235));
#165372=CARTESIAN_POINT('Ctrl Pts',(16.1559070823762,8.04468584505496,1126.65808823529));
#165373=CARTESIAN_POINT('Ctrl Pts',(16.9013570056506,6.54762058645456,1125.16397058824));
#165374=CARTESIAN_POINT('Ctrl Pts',(17.3590292079831,4.93906964482096,1123.66985294118));
#165375=CARTESIAN_POINT('Ctrl Pts',(17.8167014103155,3.33051870318735,1122.17573529412));
#165376=CARTESIAN_POINT('Ctrl Pts',(17.9710104137728,1.66525935159367,1120.68161764706));
#165377=CARTESIAN_POINT('Ctrl Pts',(18.1253194172301,3.32956716117513E-15,
1119.1875));
#165378=CARTESIAN_POINT('Ctrl Pts',(17.9710104137728,-1.66525935159367,
1117.69338235294));
#165379=CARTESIAN_POINT('Ctrl Pts',(17.8167014103155,-3.33051870318736,
1116.19926470588));
#165380=CARTESIAN_POINT('Ctrl Pts',(17.3590292079831,-4.93906964482095,
1114.70514705882));
#165381=CARTESIAN_POINT('Ctrl Pts',(16.9013570056506,-6.54762058645456,
1113.21102941176));
#165382=CARTESIAN_POINT('Ctrl Pts',(16.1559070823762,-8.04468584505497,
1111.71691176471));
#165383=CARTESIAN_POINT('Ctrl Pts',(15.4104571591017,-9.54175110365538,
1110.22279411765));
#165384=CARTESIAN_POINT('Ctrl Pts',(14.4026149179538,-10.8763499173728,
1108.72867647059));
#165385=CARTESIAN_POINT('Ctrl Pts',(13.3947726768058,-12.2109487310903,
1107.23455882353));
#165386=CARTESIAN_POINT('Ctrl Pts',(12.1588589765331,-13.3376329379985,
1105.74044117647));
#165387=CARTESIAN_POINT('Ctrl Pts',(10.9229452762603,-14.4643171449067,
1104.24632352941));
#165388=CARTESIAN_POINT('Ctrl Pts',(9.50104767561053,-15.3447188656481,
1102.75220588235));
#165389=CARTESIAN_POINT('Ctrl Pts',(8.07915007496071,-16.2251205863895,
1101.25808823529));
#165390=CARTESIAN_POINT('Ctrl Pts',(6.51968959134574,-16.8292587962898,
1099.76397058824));
#165391=CARTESIAN_POINT('Ctrl Pts',(4.96022910773078,-17.4333970061901,
1098.26985294118));
#165392=CARTESIAN_POINT('Ctrl Pts',(3.31631129755346,-17.7406985030951,
1096.77573529412));
#165393=CARTESIAN_POINT('Ctrl Pts',(1.67239348737615,-18.048,1095.28161764706));
#165394=CARTESIAN_POINT('Ctrl Pts',(0.,-18.048,1093.7875));
#165395=CARTESIAN_POINT('Ctrl Pts',(-1.67239348737615,-18.048,1092.29338235294));
#165396=CARTESIAN_POINT('Ctrl Pts',(-3.31631129755346,-17.7406985030951,
1090.79926470588));
#165397=CARTESIAN_POINT('Ctrl Pts',(-4.96022910773077,-17.4333970061901,
1089.30514705882));
#165398=CARTESIAN_POINT('Ctrl Pts',(-6.51968959134574,-16.8292587962898,
1087.81102941176));
#165399=CARTESIAN_POINT('Ctrl Pts',(-8.07915007496071,-16.2251205863895,
1086.31691176471));
#165400=CARTESIAN_POINT('Ctrl Pts',(-9.50104767561052,-15.3447188656481,
1084.82279411765));
#165401=CARTESIAN_POINT('Ctrl Pts',(-10.9229452762603,-14.4643171449067,
1083.32867647059));
#165402=CARTESIAN_POINT('Ctrl Pts',(-12.1588589765331,-13.3376329379985,
1081.83455882353));
#165403=CARTESIAN_POINT('Ctrl Pts',(-13.3947726768058,-12.2109487310903,
1080.34044117647));
#165404=CARTESIAN_POINT('Ctrl Pts',(-14.4026149179538,-10.8763499173728,
1078.84632352941));
#165405=CARTESIAN_POINT('Ctrl Pts',(-15.4104571591017,-9.54175110365538,
1077.35220588235));
#165406=CARTESIAN_POINT('Ctrl Pts',(-16.1559070823762,-8.04468584505497,
1075.85808823529));
#165407=CARTESIAN_POINT('Ctrl Pts',(-16.9013570056506,-6.54762058645456,
1074.36397058824));
#165408=CARTESIAN_POINT('Ctrl Pts',(-17.3590292079831,-4.93906964482095,
1072.86985294118));
#165409=CARTESIAN_POINT('Ctrl Pts',(-17.8167014103155,-3.33051870318735,
1071.37573529412));
#165410=CARTESIAN_POINT('Ctrl Pts',(-17.9710104137728,-1.66525935159368,
1069.88161764706));
#165411=CARTESIAN_POINT('Ctrl Pts',(-18.1253194172301,-1.10985572039171E-15,
1068.3875));
#165412=CARTESIAN_POINT('Ctrl Pts',(-17.9710104137728,1.66525935159367,
1066.89338235294));
#165413=CARTESIAN_POINT('Ctrl Pts',(-17.8167014103155,3.33051870318735,
1065.39926470588));
#165414=CARTESIAN_POINT('Ctrl Pts',(-17.3590292079831,4.93906964482096,
1063.90514705882));
#165415=CARTESIAN_POINT('Ctrl Pts',(-16.9013570056506,6.54762058645456,
1062.41102941176));
#165416=CARTESIAN_POINT('Ctrl Pts',(-16.1559070823762,8.04468584505497,
1060.91691176471));
#165417=CARTESIAN_POINT('Ctrl Pts',(-15.4104571591017,9.54175110365538,
1059.42279411765));
#165418=CARTESIAN_POINT('Ctrl Pts',(-14.4026149179538,10.8763499173728,
1057.92867647059));
#165419=CARTESIAN_POINT('Ctrl Pts',(-13.3947726768058,12.2109487310903,
1056.43455882353));
#165420=CARTESIAN_POINT('Ctrl Pts',(-12.1588589765331,13.3376329379985,
1054.94044117647));
#165421=CARTESIAN_POINT('Ctrl Pts',(-10.9229452762603,14.4643171449067,
1053.44632352941));
#165422=CARTESIAN_POINT('Ctrl Pts',(-9.50104767561052,15.3447188656481,
1051.95220588235));
#165423=CARTESIAN_POINT('Ctrl Pts',(-8.07915007496071,16.2251205863895,
1050.45808823529));
#165424=CARTESIAN_POINT('Ctrl Pts',(-6.51968959134574,16.8292587962898,
1048.96397058824));
#165425=CARTESIAN_POINT('Ctrl Pts',(-4.96022910773078,17.4333970061901,
1047.46985294118));
#165426=CARTESIAN_POINT('Ctrl Pts',(-3.31631129755346,17.7406985030951,
1045.97573529412));
#165427=CARTESIAN_POINT('Ctrl Pts',(-1.67239348737615,18.048,1044.48161764706));
#165428=CARTESIAN_POINT('Ctrl Pts',(-2.21024254310115E-15,18.048,1042.9875));
#165429=CARTESIAN_POINT('Ctrl Pts',(1.67239348737616,18.048,1041.49338235294));
#165430=CARTESIAN_POINT('Ctrl Pts',(3.31631129755346,17.7406985030951,1039.99926470588));
#165431=CARTESIAN_POINT('Ctrl Pts',(4.96022910773077,17.4333970061901,1038.50514705882));
#165432=CARTESIAN_POINT('Ctrl Pts',(6.51968959134575,16.8292587962898,1037.01102941176));
#165433=CARTESIAN_POINT('Ctrl Pts',(8.07915007496071,16.2251205863895,1035.51691176471));
#165434=CARTESIAN_POINT('Ctrl Pts',(9.50104767561053,15.3447188656481,1034.02279411765));
#165435=CARTESIAN_POINT('Ctrl Pts',(10.9229452762603,14.4643171449067,1032.52867647059));
#165436=CARTESIAN_POINT('Ctrl Pts',(12.1588589765331,13.3376329379985,1031.03455882353));
#165437=CARTESIAN_POINT('Ctrl Pts',(13.3947726768058,12.2109487310903,1029.54044117647));
#165438=CARTESIAN_POINT('Ctrl Pts',(14.4026149179538,10.8763499173728,1028.04632352941));
#165439=CARTESIAN_POINT('Ctrl Pts',(15.4104571591017,9.54175110365538,1026.55220588235));
#165440=CARTESIAN_POINT('Ctrl Pts',(16.1559070823762,8.04468584505496,1025.05808823529));
#165441=CARTESIAN_POINT('Ctrl Pts',(16.9013570056506,6.54762058645456,1023.56397058824));
#165442=CARTESIAN_POINT('Ctrl Pts',(17.3590292079831,4.93906964482096,1022.06985294118));
#165443=CARTESIAN_POINT('Ctrl Pts',(17.8167014103155,3.33051870318735,1020.57573529412));
#165444=CARTESIAN_POINT('Ctrl Pts',(17.9710104137728,1.66525935159367,1019.08161764706));
#165445=CARTESIAN_POINT('Ctrl Pts',(18.1253194172301,3.32956716117513E-15,
1017.5875));
#165446=CARTESIAN_POINT('Ctrl Pts',(17.9710104137728,-1.66525935159367,
1016.09338235294));
#165447=CARTESIAN_POINT('Ctrl Pts',(17.8167014103155,-3.33051870318736,
1014.59926470588));
#165448=CARTESIAN_POINT('Ctrl Pts',(17.3590292079831,-4.93906964482095,
1013.10514705882));
#165449=CARTESIAN_POINT('Ctrl Pts',(16.9013570056506,-6.54762058645456,
1011.61102941176));
#165450=CARTESIAN_POINT('Ctrl Pts',(16.1559070823762,-8.04468584505497,
1010.11691176471));
#165451=CARTESIAN_POINT('Ctrl Pts',(15.4104571591017,-9.54175110365538,
1008.62279411765));
#165452=CARTESIAN_POINT('Ctrl Pts',(14.4026149179538,-10.8763499173728,
1007.12867647059));
#165453=CARTESIAN_POINT('Ctrl Pts',(13.3947726768058,-12.2109487310903,
1005.63455882353));
#165454=CARTESIAN_POINT('Ctrl Pts',(12.1588589765331,-13.3376329379985,
1004.14044117647));
#165455=CARTESIAN_POINT('Ctrl Pts',(10.9229452762603,-14.4643171449067,
1002.64632352941));
#165456=CARTESIAN_POINT('Ctrl Pts',(9.50104767561053,-15.3447188656481,
1001.15220588235));
#165457=CARTESIAN_POINT('Ctrl Pts',(8.07915007496071,-16.2251205863895,
999.658088235294));
#165458=CARTESIAN_POINT('Ctrl Pts',(6.51968959134574,-16.8292587962898,
998.163970588235));
#165459=CARTESIAN_POINT('Ctrl Pts',(4.96022910773078,-17.4333970061901,
996.669852941177));
#165460=CARTESIAN_POINT('Ctrl Pts',(3.31631129755346,-17.7406985030951,
995.175735294118));
#165461=CARTESIAN_POINT('Ctrl Pts',(1.67239348737615,-18.048,993.681617647059));
#165462=CARTESIAN_POINT('Ctrl Pts',(0.,-18.048,992.1875));
#165463=CARTESIAN_POINT('Ctrl Pts',(-1.67239348737615,-18.048,990.693382352941));
#165464=CARTESIAN_POINT('Ctrl Pts',(-3.31631129755346,-17.7406985030951,
989.199264705882));
#165465=CARTESIAN_POINT('Ctrl Pts',(-4.96022910773077,-17.4333970061901,
987.705147058824));
#165466=CARTESIAN_POINT('Ctrl Pts',(-6.51968959134574,-16.8292587962898,
986.211029411765));
#165467=CARTESIAN_POINT('Ctrl Pts',(-8.07915007496071,-16.2251205863895,
984.716911764706));
#165468=CARTESIAN_POINT('Ctrl Pts',(-9.50104767561052,-15.3447188656481,
983.222794117647));
#165469=CARTESIAN_POINT('Ctrl Pts',(-10.9229452762603,-14.4643171449067,
981.728676470589));
#165470=CARTESIAN_POINT('Ctrl Pts',(-12.1588589765331,-13.3376329379985,
980.234558823529));
#165471=CARTESIAN_POINT('Ctrl Pts',(-13.3947726768058,-12.2109487310903,
978.740441176471));
#165472=CARTESIAN_POINT('Ctrl Pts',(-14.4026149179538,-10.8763499173728,
977.246323529412));
#165473=CARTESIAN_POINT('Ctrl Pts',(-15.4104571591017,-9.54175110365538,
975.752205882353));
#165474=CARTESIAN_POINT('Ctrl Pts',(-16.1559070823762,-8.04468584505497,
974.258088235294));
#165475=CARTESIAN_POINT('Ctrl Pts',(-16.9013570056506,-6.54762058645456,
972.763970588235));
#165476=CARTESIAN_POINT('Ctrl Pts',(-17.3590292079831,-4.93906964482095,
971.269852941177));
#165477=CARTESIAN_POINT('Ctrl Pts',(-17.8167014103155,-3.33051870318735,
969.775735294118));
#165478=CARTESIAN_POINT('Ctrl Pts',(-17.9710104137728,-1.66525935159368,
968.281617647059));
#165479=CARTESIAN_POINT('Ctrl Pts',(-18.1253194172301,-1.10985572039171E-15,
966.7875));
#165480=CARTESIAN_POINT('Ctrl Pts',(-17.9710104137728,1.66525935159367,
965.293382352941));
#165481=CARTESIAN_POINT('Ctrl Pts',(-17.8167014103155,3.33051870318735,
963.799264705882));
#165482=CARTESIAN_POINT('Ctrl Pts',(-17.3590292079831,4.93906964482096,
962.305147058824));
#165483=CARTESIAN_POINT('Ctrl Pts',(-16.9013570056506,6.54762058645456,
960.811029411765));
#165484=CARTESIAN_POINT('Ctrl Pts',(-16.1559070823762,8.04468584505497,
959.316911764706));
#165485=CARTESIAN_POINT('Ctrl Pts',(-15.4104571591017,9.54175110365538,
957.822794117647));
#165486=CARTESIAN_POINT('Ctrl Pts',(-14.4026149179538,10.8763499173728,
956.328676470588));
#165487=CARTESIAN_POINT('Ctrl Pts',(-13.3947726768058,12.2109487310903,
954.834558823529));
#165488=CARTESIAN_POINT('Ctrl Pts',(-12.1588589765331,13.3376329379985,
953.340441176471));
#165489=CARTESIAN_POINT('Ctrl Pts',(-10.9229452762603,14.4643171449067,
951.846323529412));
#165490=CARTESIAN_POINT('Ctrl Pts',(-9.50104767561052,15.3447188656481,
950.352205882353));
#165491=CARTESIAN_POINT('Ctrl Pts',(-8.07915007496071,16.2251205863895,
948.858088235294));
#165492=CARTESIAN_POINT('Ctrl Pts',(-6.51968959134574,16.8292587962898,
947.363970588235));
#165493=CARTESIAN_POINT('Ctrl Pts',(-4.96022910773078,17.4333970061901,
945.869852941177));
#165494=CARTESIAN_POINT('Ctrl Pts',(-3.31631129755346,17.7406985030951,
944.375735294118));
#165495=CARTESIAN_POINT('Ctrl Pts',(-1.67239348737615,18.048,942.881617647059));
#165496=CARTESIAN_POINT('Ctrl Pts',(-2.21024254310115E-15,18.048,941.3875));
#165497=CARTESIAN_POINT('Ctrl Pts',(1.67239348737616,18.048,939.893382352941));
#165498=CARTESIAN_POINT('Ctrl Pts',(3.31631129755346,17.7406985030951,938.399264705882));
#165499=CARTESIAN_POINT('Ctrl Pts',(4.96022910773077,17.4333970061901,936.905147058824));
#165500=CARTESIAN_POINT('Ctrl Pts',(6.51968959134575,16.8292587962898,935.411029411765));
#165501=CARTESIAN_POINT('Ctrl Pts',(8.07915007496071,16.2251205863895,933.916911764706));
#165502=CARTESIAN_POINT('Ctrl Pts',(9.50104767561053,15.3447188656481,932.422794117647));
#165503=CARTESIAN_POINT('Ctrl Pts',(10.9229452762603,14.4643171449067,930.928676470588));
#165504=CARTESIAN_POINT('Ctrl Pts',(12.1588589765331,13.3376329379985,929.43455882353));
#165505=CARTESIAN_POINT('Ctrl Pts',(13.3947726768058,12.2109487310903,927.94044117647));
#165506=CARTESIAN_POINT('Ctrl Pts',(14.4026149179538,10.8763499173728,926.446323529412));
#165507=CARTESIAN_POINT('Ctrl Pts',(15.4104571591017,9.54175110365538,924.952205882353));
#165508=CARTESIAN_POINT('Ctrl Pts',(16.1559070823762,8.04468584505496,923.458088235294));
#165509=CARTESIAN_POINT('Ctrl Pts',(16.9013570056506,6.54762058645456,921.963970588235));
#165510=CARTESIAN_POINT('Ctrl Pts',(17.3590292079831,4.93906964482096,920.469852941176));
#165511=CARTESIAN_POINT('Ctrl Pts',(17.8167014103155,3.33051870318735,918.975735294118));
#165512=CARTESIAN_POINT('Ctrl Pts',(17.9710104137728,1.66525935159367,917.481617647059));
#165513=CARTESIAN_POINT('Ctrl Pts',(18.1253194172301,3.32956716117513E-15,
915.9875));
#165514=CARTESIAN_POINT('Ctrl Pts',(17.9710104137728,-1.66525935159367,
914.493382352941));
#165515=CARTESIAN_POINT('Ctrl Pts',(17.8167014103155,-3.33051870318736,
912.999264705882));
#165516=CARTESIAN_POINT('Ctrl Pts',(17.3590292079831,-4.93906964482095,
911.505147058824));
#165517=CARTESIAN_POINT('Ctrl Pts',(16.9013570056506,-6.54762058645456,
910.011029411765));
#165518=CARTESIAN_POINT('Ctrl Pts',(16.1559070823762,-8.04468584505497,
908.516911764706));
#165519=CARTESIAN_POINT('Ctrl Pts',(15.4104571591017,-9.54175110365538,
907.022794117647));
#165520=CARTESIAN_POINT('Ctrl Pts',(14.4026149179538,-10.8763499173728,
905.528676470588));
#165521=CARTESIAN_POINT('Ctrl Pts',(13.3947726768058,-12.2109487310903,
904.034558823529));
#165522=CARTESIAN_POINT('Ctrl Pts',(12.1588589765331,-13.3376329379985,
902.540441176471));
#165523=CARTESIAN_POINT('Ctrl Pts',(10.9229452762603,-14.4643171449067,
901.046323529412));
#165524=CARTESIAN_POINT('Ctrl Pts',(9.50104767561053,-15.3447188656481,
899.552205882353));
#165525=CARTESIAN_POINT('Ctrl Pts',(8.07915007496071,-16.2251205863895,
898.058088235294));
#165526=CARTESIAN_POINT('Ctrl Pts',(6.51968959134574,-16.8292587962898,
896.563970588235));
#165527=CARTESIAN_POINT('Ctrl Pts',(4.96022910773078,-17.4333970061901,
895.069852941177));
#165528=CARTESIAN_POINT('Ctrl Pts',(3.31631129755346,-17.7406985030951,
893.575735294118));
#165529=CARTESIAN_POINT('Ctrl Pts',(1.67239348737615,-18.048,892.081617647059));
#165530=CARTESIAN_POINT('Ctrl Pts',(0.,-18.048,890.5875));
#165531=CARTESIAN_POINT('Ctrl Pts',(-1.67239348737615,-18.048,889.093382352941));
#165532=CARTESIAN_POINT('Ctrl Pts',(-3.31631129755346,-17.7406985030951,
887.599264705882));
#165533=CARTESIAN_POINT('Ctrl Pts',(-4.96022910773077,-17.4333970061901,
886.105147058824));
#165534=CARTESIAN_POINT('Ctrl Pts',(-6.51968959134574,-16.8292587962898,
884.611029411765));
#165535=CARTESIAN_POINT('Ctrl Pts',(-8.07915007496071,-16.2251205863895,
883.116911764706));
#165536=CARTESIAN_POINT('Ctrl Pts',(-9.50104767561052,-15.3447188656481,
881.622794117647));
#165537=CARTESIAN_POINT('Ctrl Pts',(-10.9229452762603,-14.4643171449067,
880.128676470588));
#165538=CARTESIAN_POINT('Ctrl Pts',(-12.1588589765331,-13.3376329379985,
878.634558823529));
#165539=CARTESIAN_POINT('Ctrl Pts',(-13.3947726768058,-12.2109487310903,
877.140441176471));
#165540=CARTESIAN_POINT('Ctrl Pts',(-14.4026149179538,-10.8763499173728,
875.646323529412));
#165541=CARTESIAN_POINT('Ctrl Pts',(-15.4104571591017,-9.54175110365538,
874.152205882353));
#165542=CARTESIAN_POINT('Ctrl Pts',(-16.1559070823762,-8.04468584505497,
872.658088235294));
#165543=CARTESIAN_POINT('Ctrl Pts',(-16.9013570056506,-6.54762058645456,
871.163970588236));
#165544=CARTESIAN_POINT('Ctrl Pts',(-17.3590292079831,-4.93906964482095,
869.669852941176));
#165545=CARTESIAN_POINT('Ctrl Pts',(-17.8167014103155,-3.33051870318735,
868.175735294118));
#165546=CARTESIAN_POINT('Ctrl Pts',(-17.9710104137728,-1.66525935159368,
866.681617647059));
#165547=CARTESIAN_POINT('Ctrl Pts',(-18.1253194172301,-1.10985572039171E-15,
865.1875));
#165548=CARTESIAN_POINT('Ctrl Pts',(-17.9710104137728,1.66525935159367,
863.693382352941));
#165549=CARTESIAN_POINT('Ctrl Pts',(-17.8167014103155,3.33051870318735,
862.199264705883));
#165550=CARTESIAN_POINT('Ctrl Pts',(-17.3590292079831,4.93906964482096,
860.705147058824));
#165551=CARTESIAN_POINT('Ctrl Pts',(-16.9013570056506,6.54762058645456,
859.211029411765));
#165552=CARTESIAN_POINT('Ctrl Pts',(-16.1559070823762,8.04468584505497,
857.716911764706));
#165553=CARTESIAN_POINT('Ctrl Pts',(-15.4104571591017,9.54175110365538,
856.222794117647));
#165554=CARTESIAN_POINT('Ctrl Pts',(-14.4026149179538,10.8763499173728,
854.728676470588));
#165555=CARTESIAN_POINT('Ctrl Pts',(-13.3947726768058,12.2109487310903,
853.234558823529));
#165556=CARTESIAN_POINT('Ctrl Pts',(-12.1588589765331,13.3376329379985,
851.740441176471));
#165557=CARTESIAN_POINT('Ctrl Pts',(-10.9229452762603,14.4643171449067,
850.246323529412));
#165558=CARTESIAN_POINT('Ctrl Pts',(-9.50104767561052,15.3447188656481,
848.752205882353));
#165559=CARTESIAN_POINT('Ctrl Pts',(-8.07915007496071,16.2251205863895,
847.258088235294));
#165560=CARTESIAN_POINT('Ctrl Pts',(-6.51968959134574,16.8292587962898,
845.763970588235));
#165561=CARTESIAN_POINT('Ctrl Pts',(-4.96022910773078,17.4333970061901,
844.269852941177));
#165562=CARTESIAN_POINT('Ctrl Pts',(-3.31631129755346,17.7406985030951,
842.775735294118));
#165563=CARTESIAN_POINT('Ctrl Pts',(-1.67239348737615,18.048,841.281617647059));
#165564=CARTESIAN_POINT('Ctrl Pts',(-2.21024254310115E-15,18.048,839.7875));
#165565=CARTESIAN_POINT('Ctrl Pts',(1.67239348737616,18.048,838.293382352941));
#165566=CARTESIAN_POINT('Ctrl Pts',(3.31631129755346,17.7406985030951,836.799264705882));
#165567=CARTESIAN_POINT('Ctrl Pts',(4.96022910773077,17.4333970061901,835.305147058824));
#165568=CARTESIAN_POINT('Ctrl Pts',(6.51968959134575,16.8292587962898,833.811029411765));
#165569=CARTESIAN_POINT('Ctrl Pts',(8.07915007496071,16.2251205863895,832.316911764706));
#165570=CARTESIAN_POINT('Ctrl Pts',(9.50104767561053,15.3447188656481,830.822794117647));
#165571=CARTESIAN_POINT('Ctrl Pts',(10.9229452762603,14.4643171449067,829.328676470588));
#165572=CARTESIAN_POINT('Ctrl Pts',(12.1588589765331,13.3376329379985,827.834558823529));
#165573=CARTESIAN_POINT('Ctrl Pts',(13.3947726768058,12.2109487310903,826.340441176471));
#165574=CARTESIAN_POINT('Ctrl Pts',(14.4026149179538,10.8763499173728,824.846323529412));
#165575=CARTESIAN_POINT('Ctrl Pts',(15.4104571591017,9.54175110365538,823.352205882353));
#165576=CARTESIAN_POINT('Ctrl Pts',(16.1559070823762,8.04468584505496,821.858088235294));
#165577=CARTESIAN_POINT('Ctrl Pts',(16.9013570056506,6.54762058645456,820.363970588236));
#165578=CARTESIAN_POINT('Ctrl Pts',(17.3590292079831,4.93906964482096,818.869852941177));
#165579=CARTESIAN_POINT('Ctrl Pts',(17.8167014103155,3.33051870318735,817.375735294118));
#165580=CARTESIAN_POINT('Ctrl Pts',(17.9710104137728,1.66525935159367,815.881617647059));
#165581=CARTESIAN_POINT('Ctrl Pts',(18.1253194172301,3.32956716117513E-15,
814.3875));
#165582=CARTESIAN_POINT('Ctrl Pts',(17.9710104137728,-1.66525935159367,
812.893382352941));
#165583=CARTESIAN_POINT('Ctrl Pts',(17.8167014103155,-3.33051870318736,
811.399264705883));
#165584=CARTESIAN_POINT('Ctrl Pts',(17.3590292079831,-4.93906964482095,
809.905147058824));
#165585=CARTESIAN_POINT('Ctrl Pts',(16.9013570056506,-6.54762058645456,
808.411029411765));
#165586=CARTESIAN_POINT('Ctrl Pts',(16.1559070823762,-8.04468584505497,
806.916911764706));
#165587=CARTESIAN_POINT('Ctrl Pts',(15.4104571591017,-9.54175110365538,
805.422794117647));
#165588=CARTESIAN_POINT('Ctrl Pts',(14.4026149179538,-10.8763499173728,
803.928676470588));
#165589=CARTESIAN_POINT('Ctrl Pts',(13.3947726768058,-12.2109487310903,
802.434558823529));
#165590=CARTESIAN_POINT('Ctrl Pts',(12.1588589765331,-13.3376329379985,
800.940441176471));
#165591=CARTESIAN_POINT('Ctrl Pts',(10.9229452762603,-14.4643171449067,
799.446323529412));
#165592=CARTESIAN_POINT('Ctrl Pts',(9.50104767561053,-15.3447188656481,
797.952205882353));
#165593=CARTESIAN_POINT('Ctrl Pts',(8.07915007496071,-16.2251205863895,
796.458088235294));
#165594=CARTESIAN_POINT('Ctrl Pts',(6.51968959134574,-16.8292587962898,
794.963970588235));
#165595=CARTESIAN_POINT('Ctrl Pts',(4.96022910773078,-17.4333970061901,
793.469852941176));
#165596=CARTESIAN_POINT('Ctrl Pts',(3.31631129755346,-17.7406985030951,
791.975735294118));
#165597=CARTESIAN_POINT('Ctrl Pts',(1.67239348737615,-18.048,790.481617647059));
#165598=CARTESIAN_POINT('Ctrl Pts',(0.,-18.048,788.9875));
#165599=CARTESIAN_POINT('Ctrl Pts',(-1.67239348737615,-18.048,787.493382352941));
#165600=CARTESIAN_POINT('Ctrl Pts',(-3.31631129755346,-17.7406985030951,
785.999264705882));
#165601=CARTESIAN_POINT('Ctrl Pts',(-4.96022910773077,-17.4333970061901,
784.505147058824));
#165602=CARTESIAN_POINT('Ctrl Pts',(-6.51968959134574,-16.8292587962898,
783.011029411765));
#165603=CARTESIAN_POINT('Ctrl Pts',(-8.07915007496071,-16.2251205863895,
781.516911764706));
#165604=CARTESIAN_POINT('Ctrl Pts',(-9.50104767561052,-15.3447188656481,
780.022794117647));
#165605=CARTESIAN_POINT('Ctrl Pts',(-10.9229452762603,-14.4643171449067,
778.528676470588));
#165606=CARTESIAN_POINT('Ctrl Pts',(-12.1588589765331,-13.3376329379985,
777.03455882353));
#165607=CARTESIAN_POINT('Ctrl Pts',(-13.3947726768058,-12.2109487310903,
775.540441176471));
#165608=CARTESIAN_POINT('Ctrl Pts',(-14.4026149179538,-10.8763499173728,
774.046323529412));
#165609=CARTESIAN_POINT('Ctrl Pts',(-15.4104571591017,-9.54175110365538,
772.552205882353));
#165610=CARTESIAN_POINT('Ctrl Pts',(-16.1559070823762,-8.04468584505497,
771.058088235294));
#165611=CARTESIAN_POINT('Ctrl Pts',(-16.9013570056506,-6.54762058645456,
769.563970588235));
#165612=CARTESIAN_POINT('Ctrl Pts',(-17.3590292079831,-4.93906964482095,
768.069852941177));
#165613=CARTESIAN_POINT('Ctrl Pts',(-17.8167014103155,-3.33051870318735,
766.575735294118));
#165614=CARTESIAN_POINT('Ctrl Pts',(-17.9710104137728,-1.66525935159368,
765.081617647059));
#165615=CARTESIAN_POINT('Ctrl Pts',(-18.1253194172301,-1.10985572039171E-15,
763.5875));
#165616=CARTESIAN_POINT('Ctrl Pts',(-17.9710104137728,1.66525935159367,
762.093382352941));
#165617=CARTESIAN_POINT('Ctrl Pts',(-17.8167014103155,3.33051870318735,
760.599264705883));
#165618=CARTESIAN_POINT('Ctrl Pts',(-17.3590292079831,4.93906964482096,
759.105147058824));
#165619=CARTESIAN_POINT('Ctrl Pts',(-16.9013570056506,6.54762058645456,
757.611029411765));
#165620=CARTESIAN_POINT('Ctrl Pts',(-16.1559070823762,8.04468584505497,
756.116911764706));
#165621=CARTESIAN_POINT('Ctrl Pts',(-15.4104571591017,9.54175110365538,
754.622794117647));
#165622=CARTESIAN_POINT('Ctrl Pts',(-14.4026149179538,10.8763499173728,
753.128676470588));
#165623=CARTESIAN_POINT('Ctrl Pts',(-13.3947726768058,12.2109487310903,
751.634558823529));
#165624=CARTESIAN_POINT('Ctrl Pts',(-12.1588589765331,13.3376329379985,
750.140441176471));
#165625=CARTESIAN_POINT('Ctrl Pts',(-10.9229452762603,14.4643171449067,
748.646323529412));
#165626=CARTESIAN_POINT('Ctrl Pts',(-9.50104767561052,15.3447188656481,
747.152205882353));
#165627=CARTESIAN_POINT('Ctrl Pts',(-8.07915007496071,16.2251205863895,
745.658088235294));
#165628=CARTESIAN_POINT('Ctrl Pts',(-6.51968959134574,16.8292587962898,
744.163970588235));
#165629=CARTESIAN_POINT('Ctrl Pts',(-4.96022910773078,17.4333970061901,
742.669852941176));
#165630=CARTESIAN_POINT('Ctrl Pts',(-3.31631129755346,17.7406985030951,
741.175735294118));
#165631=CARTESIAN_POINT('Ctrl Pts',(-1.67239348737615,18.048,739.681617647059));
#165632=CARTESIAN_POINT('Ctrl Pts',(-2.21024254310115E-15,18.048,738.1875));
#165633=CARTESIAN_POINT('Ctrl Pts',(1.67239348737616,18.048,736.693382352941));
#165634=CARTESIAN_POINT('Ctrl Pts',(3.31631129755346,17.7406985030951,735.199264705882));
#165635=CARTESIAN_POINT('Ctrl Pts',(4.96022910773077,17.4333970061901,733.705147058824));
#165636=CARTESIAN_POINT('Ctrl Pts',(6.51968959134575,16.8292587962898,732.211029411765));
#165637=CARTESIAN_POINT('Ctrl Pts',(8.07915007496071,16.2251205863895,730.716911764706));
#165638=CARTESIAN_POINT('Ctrl Pts',(9.50104767561053,15.3447188656481,729.222794117647));
#165639=CARTESIAN_POINT('Ctrl Pts',(10.9229452762603,14.4643171449067,727.728676470588));
#165640=CARTESIAN_POINT('Ctrl Pts',(12.1588589765331,13.3376329379985,726.234558823529));
#165641=CARTESIAN_POINT('Ctrl Pts',(13.3947726768058,12.2109487310903,724.740441176471));
#165642=CARTESIAN_POINT('Ctrl Pts',(14.4026149179538,10.8763499173728,723.246323529412));
#165643=CARTESIAN_POINT('Ctrl Pts',(15.4104571591017,9.54175110365538,721.752205882353));
#165644=CARTESIAN_POINT('Ctrl Pts',(16.1559070823762,8.04468584505496,720.258088235294));
#165645=CARTESIAN_POINT('Ctrl Pts',(16.9013570056506,6.54762058645456,718.763970588235));
#165646=CARTESIAN_POINT('Ctrl Pts',(17.3590292079831,4.93906964482096,717.269852941177));
#165647=CARTESIAN_POINT('Ctrl Pts',(17.8167014103155,3.33051870318735,715.775735294118));
#165648=CARTESIAN_POINT('Ctrl Pts',(17.9710104137728,1.66525935159367,714.281617647059));
#165649=CARTESIAN_POINT('Ctrl Pts',(18.1253194172301,3.32956716117513E-15,
712.7875));
#165650=CARTESIAN_POINT('Ctrl Pts',(17.9710104137728,-1.66525935159367,
711.293382352941));
#165651=CARTESIAN_POINT('Ctrl Pts',(17.8167014103155,-3.33051870318736,
709.799264705883));
#165652=CARTESIAN_POINT('Ctrl Pts',(17.3590292079831,-4.93906964482095,
708.305147058824));
#165653=CARTESIAN_POINT('Ctrl Pts',(16.9013570056506,-6.54762058645456,
706.811029411765));
#165654=CARTESIAN_POINT('Ctrl Pts',(16.1559070823762,-8.04468584505497,
705.316911764706));
#165655=CARTESIAN_POINT('Ctrl Pts',(15.4104571591017,-9.54175110365538,
703.822794117647));
#165656=CARTESIAN_POINT('Ctrl Pts',(14.4026149179538,-10.8763499173728,
702.328676470588));
#165657=CARTESIAN_POINT('Ctrl Pts',(13.3947726768058,-12.2109487310903,
700.83455882353));
#165658=CARTESIAN_POINT('Ctrl Pts',(12.1588589765331,-13.3376329379985,
699.340441176471));
#165659=CARTESIAN_POINT('Ctrl Pts',(10.9229452762603,-14.4643171449067,
697.846323529412));
#165660=CARTESIAN_POINT('Ctrl Pts',(9.50104767561053,-15.3447188656481,
696.352205882353));
#165661=CARTESIAN_POINT('Ctrl Pts',(8.07915007496071,-16.2251205863895,
694.858088235294));
#165662=CARTESIAN_POINT('Ctrl Pts',(6.51968959134574,-16.8292587962898,
693.363970588235));
#165663=CARTESIAN_POINT('Ctrl Pts',(4.96022910773078,-17.4333970061901,
691.869852941177));
#165664=CARTESIAN_POINT('Ctrl Pts',(3.31631129755346,-17.7406985030951,
690.375735294118));
#165665=CARTESIAN_POINT('Ctrl Pts',(1.67239348737615,-18.048,688.881617647059));
#165666=CARTESIAN_POINT('Ctrl Pts',(0.,-18.048,687.3875));
#165667=CARTESIAN_POINT('Ctrl Pts',(-1.67239348737615,-18.048,685.893382352941));
#165668=CARTESIAN_POINT('Ctrl Pts',(-3.31631129755346,-17.7406985030951,
684.399264705883));
#165669=CARTESIAN_POINT('Ctrl Pts',(-4.96022910773077,-17.4333970061901,
682.905147058824));
#165670=CARTESIAN_POINT('Ctrl Pts',(-6.51968959134574,-16.8292587962898,
681.411029411765));
#165671=CARTESIAN_POINT('Ctrl Pts',(-8.07915007496071,-16.2251205863895,
679.916911764706));
#165672=CARTESIAN_POINT('Ctrl Pts',(-9.50104767561052,-15.3447188656481,
678.422794117647));
#165673=CARTESIAN_POINT('Ctrl Pts',(-10.9229452762603,-14.4643171449067,
676.928676470588));
#165674=CARTESIAN_POINT('Ctrl Pts',(-12.1588589765331,-13.3376329379985,
675.434558823529));
#165675=CARTESIAN_POINT('Ctrl Pts',(-13.3947726768058,-12.2109487310903,
673.940441176471));
#165676=CARTESIAN_POINT('Ctrl Pts',(-14.4026149179538,-10.8763499173728,
672.446323529412));
#165677=CARTESIAN_POINT('Ctrl Pts',(-15.4104571591017,-9.54175110365538,
670.952205882353));
#165678=CARTESIAN_POINT('Ctrl Pts',(-16.1559070823762,-8.04468584505497,
669.458088235294));
#165679=CARTESIAN_POINT('Ctrl Pts',(-16.9013570056506,-6.54762058645456,
667.963970588235));
#165680=CARTESIAN_POINT('Ctrl Pts',(-17.3590292079831,-4.93906964482095,
666.469852941176));
#165681=CARTESIAN_POINT('Ctrl Pts',(-17.8167014103155,-3.33051870318735,
664.975735294118));
#165682=CARTESIAN_POINT('Ctrl Pts',(-17.9710104137728,-1.66525935159368,
663.481617647059));
#165683=CARTESIAN_POINT('Ctrl Pts',(-18.1253194172301,-1.10985572039171E-15,
661.9875));
#165684=CARTESIAN_POINT('Ctrl Pts',(-17.9710104137728,1.66525935159367,
660.493382352941));
#165685=CARTESIAN_POINT('Ctrl Pts',(-17.8167014103155,3.33051870318735,
658.999264705882));
#165686=CARTESIAN_POINT('Ctrl Pts',(-17.3590292079831,4.93906964482096,
657.505147058824));
#165687=CARTESIAN_POINT('Ctrl Pts',(-16.9013570056506,6.54762058645456,
656.011029411765));
#165688=CARTESIAN_POINT('Ctrl Pts',(-16.1559070823762,8.04468584505497,
654.516911764706));
#165689=CARTESIAN_POINT('Ctrl Pts',(-15.4104571591017,9.54175110365538,
653.022794117647));
#165690=CARTESIAN_POINT('Ctrl Pts',(-14.4026149179538,10.8763499173728,
651.528676470588));
#165691=CARTESIAN_POINT('Ctrl Pts',(-13.3947726768058,12.2109487310903,
650.03455882353));
#165692=CARTESIAN_POINT('Ctrl Pts',(-12.1588589765331,13.3376329379985,
648.540441176471));
#165693=CARTESIAN_POINT('Ctrl Pts',(-10.9229452762603,14.4643171449067,
647.046323529412));
#165694=CARTESIAN_POINT('Ctrl Pts',(-9.50104767561052,15.3447188656481,
645.552205882353));
#165695=CARTESIAN_POINT('Ctrl Pts',(-8.07915007496071,16.2251205863895,
644.058088235294));
#165696=CARTESIAN_POINT('Ctrl Pts',(-6.51968959134574,16.8292587962898,
642.563970588235));
#165697=CARTESIAN_POINT('Ctrl Pts',(-4.96022910773078,17.4333970061901,
641.069852941176));
#165698=CARTESIAN_POINT('Ctrl Pts',(-3.31631129755346,17.7406985030951,
639.575735294118));
#165699=CARTESIAN_POINT('Ctrl Pts',(-1.67239348737615,18.048,638.081617647059));
#165700=CARTESIAN_POINT('Ctrl Pts',(-2.21024254310115E-15,18.048,636.5875));
#165701=CARTESIAN_POINT('Ctrl Pts',(1.67239348737616,18.048,635.093382352941));
#165702=CARTESIAN_POINT('Ctrl Pts',(3.31631129755346,17.7406985030951,633.599264705882));
#165703=CARTESIAN_POINT('Ctrl Pts',(4.96022910773077,17.4333970061901,632.105147058824));
#165704=CARTESIAN_POINT('Ctrl Pts',(6.51968959134575,16.8292587962898,630.611029411765));
#165705=CARTESIAN_POINT('Ctrl Pts',(8.07915007496071,16.2251205863895,629.116911764706));
#165706=CARTESIAN_POINT('Ctrl Pts',(9.50104767561053,15.3447188656481,627.622794117647));
#165707=CARTESIAN_POINT('Ctrl Pts',(10.9229452762603,14.4643171449067,626.128676470588));
#165708=CARTESIAN_POINT('Ctrl Pts',(12.1588589765331,13.3376329379985,624.634558823529));
#165709=CARTESIAN_POINT('Ctrl Pts',(13.3947726768058,12.2109487310903,623.140441176471));
#165710=CARTESIAN_POINT('Ctrl Pts',(14.4026149179538,10.8763499173728,621.646323529412));
#165711=CARTESIAN_POINT('Ctrl Pts',(15.4104571591017,9.54175110365538,620.152205882353));
#165712=CARTESIAN_POINT('Ctrl Pts',(16.1559070823762,8.04468584505496,618.658088235294));
#165713=CARTESIAN_POINT('Ctrl Pts',(16.9013570056506,6.54762058645456,617.163970588235));
#165714=CARTESIAN_POINT('Ctrl Pts',(17.3590292079831,4.93906964482096,615.669852941176));
#165715=CARTESIAN_POINT('Ctrl Pts',(17.8167014103155,3.33051870318735,614.175735294118));
#165716=CARTESIAN_POINT('Ctrl Pts',(17.9710104137728,1.66525935159367,612.681617647059));
#165717=CARTESIAN_POINT('Ctrl Pts',(18.1253194172301,3.32956716117513E-15,
611.1875));
#165718=CARTESIAN_POINT('Ctrl Pts',(17.9710104137728,-1.66525935159367,
609.693382352941));
#165719=CARTESIAN_POINT('Ctrl Pts',(17.8167014103155,-3.33051870318736,
608.199264705882));
#165720=CARTESIAN_POINT('Ctrl Pts',(17.3590292079831,-4.93906964482095,
606.705147058824));
#165721=CARTESIAN_POINT('Ctrl Pts',(16.9013570056506,-6.54762058645456,
605.211029411765));
#165722=CARTESIAN_POINT('Ctrl Pts',(16.1559070823762,-8.04468584505497,
603.716911764706));
#165723=CARTESIAN_POINT('Ctrl Pts',(15.4104571591017,-9.54175110365538,
602.222794117647));
#165724=CARTESIAN_POINT('Ctrl Pts',(14.4026149179538,-10.8763499173728,
600.728676470588));
#165725=CARTESIAN_POINT('Ctrl Pts',(13.3947726768058,-12.2109487310903,
599.23455882353));
#165726=CARTESIAN_POINT('Ctrl Pts',(12.1588589765331,-13.3376329379985,
597.740441176471));
#165727=CARTESIAN_POINT('Ctrl Pts',(10.9229452762603,-14.4643171449067,
596.246323529412));
#165728=CARTESIAN_POINT('Ctrl Pts',(9.50104767561053,-15.3447188656481,
594.752205882353));
#165729=CARTESIAN_POINT('Ctrl Pts',(8.07915007496071,-16.2251205863895,
593.258088235294));
#165730=CARTESIAN_POINT('Ctrl Pts',(6.51968959134574,-16.8292587962898,
591.763970588235));
#165731=CARTESIAN_POINT('Ctrl Pts',(4.96022910773078,-17.4333970061901,
590.269852941177));
#165732=CARTESIAN_POINT('Ctrl Pts',(3.31631129755346,-17.7406985030951,
588.775735294118));
#165733=CARTESIAN_POINT('Ctrl Pts',(1.67239348737615,-18.048,587.281617647059));
#165734=CARTESIAN_POINT('Ctrl Pts',(0.,-18.048,585.7875));
#165735=CARTESIAN_POINT('Ctrl Pts',(-1.67239348737615,-18.048,584.293382352941));
#165736=CARTESIAN_POINT('Ctrl Pts',(-3.31631129755346,-17.7406985030951,
582.799264705882));
#165737=CARTESIAN_POINT('Ctrl Pts',(-4.96022910773077,-17.4333970061901,
581.305147058824));
#165738=CARTESIAN_POINT('Ctrl Pts',(-6.51968959134574,-16.8292587962898,
579.811029411765));
#165739=CARTESIAN_POINT('Ctrl Pts',(-8.07915007496071,-16.2251205863895,
578.316911764706));
#165740=CARTESIAN_POINT('Ctrl Pts',(-9.50104767561052,-15.3447188656481,
576.822794117647));
#165741=CARTESIAN_POINT('Ctrl Pts',(-10.9229452762603,-14.4643171449067,
575.328676470588));
#165742=CARTESIAN_POINT('Ctrl Pts',(-12.1588589765331,-13.3376329379985,
573.834558823529));
#165743=CARTESIAN_POINT('Ctrl Pts',(-13.3947726768058,-12.2109487310903,
572.340441176471));
#165744=CARTESIAN_POINT('Ctrl Pts',(-14.4026149179538,-10.8763499173728,
570.846323529412));
#165745=CARTESIAN_POINT('Ctrl Pts',(-15.4104571591017,-9.54175110365538,
569.352205882353));
#165746=CARTESIAN_POINT('Ctrl Pts',(-16.1559070823762,-8.04468584505497,
567.858088235294));
#165747=CARTESIAN_POINT('Ctrl Pts',(-16.9013570056506,-6.54762058645456,
566.363970588235));
#165748=CARTESIAN_POINT('Ctrl Pts',(-17.3590292079831,-4.93906964482095,
564.869852941177));
#165749=CARTESIAN_POINT('Ctrl Pts',(-17.8167014103155,-3.33051870318735,
563.375735294118));
#165750=CARTESIAN_POINT('Ctrl Pts',(-17.9710104137728,-1.66525935159368,
561.881617647059));
#165751=CARTESIAN_POINT('Ctrl Pts',(-18.1253194172301,-1.10985572039171E-15,
560.3875));
#165752=CARTESIAN_POINT('Ctrl Pts',(-17.9710104137728,1.66525935159367,
558.893382352941));
#165753=CARTESIAN_POINT('Ctrl Pts',(-17.8167014103155,3.33051870318735,
557.399264705882));
#165754=CARTESIAN_POINT('Ctrl Pts',(-17.3590292079831,4.93906964482096,
555.905147058824));
#165755=CARTESIAN_POINT('Ctrl Pts',(-16.9013570056506,6.54762058645456,
554.411029411765));
#165756=CARTESIAN_POINT('Ctrl Pts',(-16.1559070823762,8.04468584505497,
552.916911764706));
#165757=CARTESIAN_POINT('Ctrl Pts',(-15.4104571591017,9.54175110365538,
551.422794117647));
#165758=CARTESIAN_POINT('Ctrl Pts',(-14.4026149179538,10.8763499173728,
549.928676470588));
#165759=CARTESIAN_POINT('Ctrl Pts',(-13.3947726768058,12.2109487310903,
548.43455882353));
#165760=CARTESIAN_POINT('Ctrl Pts',(-12.1588589765331,13.3376329379985,
546.940441176471));
#165761=CARTESIAN_POINT('Ctrl Pts',(-10.9229452762603,14.4643171449067,
545.446323529412));
#165762=CARTESIAN_POINT('Ctrl Pts',(-9.50104767561052,15.3447188656481,
543.952205882353));
#165763=CARTESIAN_POINT('Ctrl Pts',(-8.07915007496071,16.2251205863895,
542.458088235294));
#165764=CARTESIAN_POINT('Ctrl Pts',(-6.51968959134574,16.8292587962898,
540.963970588235));
#165765=CARTESIAN_POINT('Ctrl Pts',(-4.96022910773078,17.4333970061901,
539.469852941177));
#165766=CARTESIAN_POINT('Ctrl Pts',(-3.31631129755346,17.7406985030951,
537.975735294118));
#165767=CARTESIAN_POINT('Ctrl Pts',(-1.67239348737615,18.048,536.481617647059));
#165768=CARTESIAN_POINT('Ctrl Pts',(-2.21024254310115E-15,18.048,534.9875));
#165769=CARTESIAN_POINT('Ctrl Pts',(1.67239348737616,18.048,533.493382352941));
#165770=CARTESIAN_POINT('Ctrl Pts',(3.31631129755346,17.7406985030951,531.999264705882));
#165771=CARTESIAN_POINT('Ctrl Pts',(4.96022910773077,17.4333970061901,530.505147058824));
#165772=CARTESIAN_POINT('Ctrl Pts',(6.51968959134575,16.8292587962898,529.011029411765));
#165773=CARTESIAN_POINT('Ctrl Pts',(8.07915007496071,16.2251205863895,527.516911764706));
#165774=CARTESIAN_POINT('Ctrl Pts',(9.50104767561053,15.3447188656481,526.022794117647));
#165775=CARTESIAN_POINT('Ctrl Pts',(10.9229452762603,14.4643171449067,524.528676470588));
#165776=CARTESIAN_POINT('Ctrl Pts',(12.1588589765331,13.3376329379985,523.03455882353));
#165777=CARTESIAN_POINT('Ctrl Pts',(13.3947726768058,12.2109487310903,521.540441176471));
#165778=CARTESIAN_POINT('Ctrl Pts',(14.4026149179538,10.8763499173728,520.046323529412));
#165779=CARTESIAN_POINT('Ctrl Pts',(15.4104571591017,9.54175110365538,518.552205882353));
#165780=CARTESIAN_POINT('Ctrl Pts',(16.1559070823762,8.04468584505496,517.058088235294));
#165781=CARTESIAN_POINT('Ctrl Pts',(16.9013570056506,6.54762058645456,515.563970588235));
#165782=CARTESIAN_POINT('Ctrl Pts',(17.3590292079831,4.93906964482096,514.069852941176));
#165783=CARTESIAN_POINT('Ctrl Pts',(17.8167014103155,3.33051870318735,512.575735294118));
#165784=CARTESIAN_POINT('Ctrl Pts',(17.9710104137728,1.66525935159367,511.081617647059));
#165785=CARTESIAN_POINT('Ctrl Pts',(18.1253194172301,3.32956716117513E-15,
509.5875));
#165786=CARTESIAN_POINT('Ctrl Pts',(17.9710104137728,-1.66525935159367,
508.093382352941));
#165787=CARTESIAN_POINT('Ctrl Pts',(17.8167014103155,-3.33051870318736,
506.599264705882));
#165788=CARTESIAN_POINT('Ctrl Pts',(17.3590292079831,-4.93906964482095,
505.105147058824));
#165789=CARTESIAN_POINT('Ctrl Pts',(16.9013570056506,-6.54762058645456,
503.611029411765));
#165790=CARTESIAN_POINT('Ctrl Pts',(16.1559070823762,-8.04468584505497,
502.116911764706));
#165791=CARTESIAN_POINT('Ctrl Pts',(15.4104571591017,-9.54175110365538,
500.622794117647));
#165792=CARTESIAN_POINT('Ctrl Pts',(14.4026149179538,-10.8763499173728,
499.128676470588));
#165793=CARTESIAN_POINT('Ctrl Pts',(13.3947726768058,-12.2109487310903,
497.63455882353));
#165794=CARTESIAN_POINT('Ctrl Pts',(12.1588589765331,-13.3376329379985,
496.140441176471));
#165795=CARTESIAN_POINT('Ctrl Pts',(10.9229452762603,-14.4643171449067,
494.646323529412));
#165796=CARTESIAN_POINT('Ctrl Pts',(9.50104767561053,-15.3447188656481,
493.152205882353));
#165797=CARTESIAN_POINT('Ctrl Pts',(8.07915007496071,-16.2251205863895,
491.658088235294));
#165798=CARTESIAN_POINT('Ctrl Pts',(6.51968959134574,-16.8292587962898,
490.163970588235));
#165799=CARTESIAN_POINT('Ctrl Pts',(4.96022910773078,-17.4333970061901,
488.669852941177));
#165800=CARTESIAN_POINT('Ctrl Pts',(3.31631129755346,-17.7406985030951,
487.175735294118));
#165801=CARTESIAN_POINT('Ctrl Pts',(1.67239348737615,-18.048,485.681617647059));
#165802=CARTESIAN_POINT('Ctrl Pts',(0.,-18.048,484.1875));
#165803=CARTESIAN_POINT('Ctrl Pts',(-1.67239348737615,-18.048,482.693382352941));
#165804=CARTESIAN_POINT('Ctrl Pts',(-3.31631129755346,-17.7406985030951,
481.199264705882));
#165805=CARTESIAN_POINT('Ctrl Pts',(-4.96022910773077,-17.4333970061901,
479.705147058824));
#165806=CARTESIAN_POINT('Ctrl Pts',(-6.51968959134574,-16.8292587962898,
478.211029411765));
#165807=CARTESIAN_POINT('Ctrl Pts',(-8.07915007496071,-16.2251205863895,
476.716911764706));
#165808=CARTESIAN_POINT('Ctrl Pts',(-9.50104767561052,-15.3447188656481,
475.222794117647));
#165809=CARTESIAN_POINT('Ctrl Pts',(-10.9229452762603,-14.4643171449067,
473.728676470588));
#165810=CARTESIAN_POINT('Ctrl Pts',(-12.1588589765331,-13.3376329379985,
472.234558823529));
#165811=CARTESIAN_POINT('Ctrl Pts',(-13.3947726768058,-12.2109487310903,
470.740441176471));
#165812=CARTESIAN_POINT('Ctrl Pts',(-14.4026149179538,-10.8763499173728,
469.246323529412));
#165813=CARTESIAN_POINT('Ctrl Pts',(-15.4104571591017,-9.54175110365538,
467.752205882353));
#165814=CARTESIAN_POINT('Ctrl Pts',(-16.1559070823762,-8.04468584505497,
466.258088235294));
#165815=CARTESIAN_POINT('Ctrl Pts',(-16.9013570056506,-6.54762058645456,
464.763970588236));
#165816=CARTESIAN_POINT('Ctrl Pts',(-17.3590292079831,-4.93906964482095,
463.269852941177));
#165817=CARTESIAN_POINT('Ctrl Pts',(-17.8167014103155,-3.33051870318735,
461.775735294118));
#165818=CARTESIAN_POINT('Ctrl Pts',(-17.9710104137728,-1.66525935159368,
460.281617647059));
#165819=CARTESIAN_POINT('Ctrl Pts',(-18.1253194172301,-1.10985572039171E-15,
458.7875));
#165820=CARTESIAN_POINT('Ctrl Pts',(-17.9710104137728,1.66525935159367,
457.293382352941));
#165821=CARTESIAN_POINT('Ctrl Pts',(-17.8167014103155,3.33051870318735,
455.799264705882));
#165822=CARTESIAN_POINT('Ctrl Pts',(-17.3590292079831,4.93906964482096,
454.305147058824));
#165823=CARTESIAN_POINT('Ctrl Pts',(-16.9013570056506,6.54762058645456,
452.811029411765));
#165824=CARTESIAN_POINT('Ctrl Pts',(-16.1559070823762,8.04468584505497,
451.316911764706));
#165825=CARTESIAN_POINT('Ctrl Pts',(-15.4104571591017,9.54175110365538,
449.822794117647));
#165826=CARTESIAN_POINT('Ctrl Pts',(-14.4026149179538,10.8763499173728,
448.328676470588));
#165827=CARTESIAN_POINT('Ctrl Pts',(-13.3947726768058,12.2109487310903,
446.83455882353));
#165828=CARTESIAN_POINT('Ctrl Pts',(-12.1588589765331,13.3376329379985,
445.340441176471));
#165829=CARTESIAN_POINT('Ctrl Pts',(-10.9229452762603,14.4643171449067,
443.846323529412));
#165830=CARTESIAN_POINT('Ctrl Pts',(-9.50104767561052,15.3447188656481,
442.352205882353));
#165831=CARTESIAN_POINT('Ctrl Pts',(-8.07915007496071,16.2251205863895,
440.858088235294));
#165832=CARTESIAN_POINT('Ctrl Pts',(-6.51968959134574,16.8292587962898,
439.363970588235));
#165833=CARTESIAN_POINT('Ctrl Pts',(-4.96022910773078,17.4333970061901,
437.869852941176));
#165834=CARTESIAN_POINT('Ctrl Pts',(-3.31631129755346,17.7406985030951,
436.375735294118));
#165835=CARTESIAN_POINT('Ctrl Pts',(-1.67239348737615,18.048,434.881617647059));
#165836=CARTESIAN_POINT('Ctrl Pts',(-2.21024254310115E-15,18.048,433.3875));
#165837=CARTESIAN_POINT('Ctrl Pts',(1.67239348737616,18.048,431.893382352941));
#165838=CARTESIAN_POINT('Ctrl Pts',(3.31631129755346,17.7406985030951,430.399264705882));
#165839=CARTESIAN_POINT('Ctrl Pts',(4.96022910773077,17.4333970061901,428.905147058824));
#165840=CARTESIAN_POINT('Ctrl Pts',(6.51968959134575,16.8292587962898,427.411029411765));
#165841=CARTESIAN_POINT('Ctrl Pts',(8.07915007496071,16.2251205863895,425.916911764706));
#165842=CARTESIAN_POINT('Ctrl Pts',(9.50104767561053,15.3447188656481,424.422794117647));
#165843=CARTESIAN_POINT('Ctrl Pts',(10.9229452762603,14.4643171449067,422.928676470588));
#165844=CARTESIAN_POINT('Ctrl Pts',(12.1588589765331,13.3376329379985,421.43455882353));
#165845=CARTESIAN_POINT('Ctrl Pts',(13.3947726768058,12.2109487310903,419.940441176471));
#165846=CARTESIAN_POINT('Ctrl Pts',(14.4026149179538,10.8763499173728,418.446323529412));
#165847=CARTESIAN_POINT('Ctrl Pts',(15.4104571591017,9.54175110365538,416.952205882353));
#165848=CARTESIAN_POINT('Ctrl Pts',(16.1559070823762,8.04468584505496,415.458088235294));
#165849=CARTESIAN_POINT('Ctrl Pts',(16.9013570056506,6.54762058645456,413.963970588235));
#165850=CARTESIAN_POINT('Ctrl Pts',(17.3590292079831,4.93906964482096,412.469852941177));
#165851=CARTESIAN_POINT('Ctrl Pts',(17.8167014103155,3.33051870318735,410.975735294118));
#165852=CARTESIAN_POINT('Ctrl Pts',(17.9710104137728,1.66525935159367,409.481617647059));
#165853=CARTESIAN_POINT('Ctrl Pts',(18.1253194172301,3.32956716117513E-15,
407.9875));
#165854=CARTESIAN_POINT('Ctrl Pts',(17.9710104137728,-1.66525935159367,
406.493382352941));
#165855=CARTESIAN_POINT('Ctrl Pts',(17.8167014103155,-3.33051870318736,
404.999264705882));
#165856=CARTESIAN_POINT('Ctrl Pts',(17.3590292079831,-4.93906964482095,
403.505147058824));
#165857=CARTESIAN_POINT('Ctrl Pts',(16.9013570056506,-6.54762058645456,
402.011029411765));
#165858=CARTESIAN_POINT('Ctrl Pts',(16.1559070823762,-8.04468584505497,
400.516911764706));
#165859=CARTESIAN_POINT('Ctrl Pts',(15.4104571591017,-9.54175110365538,
399.022794117647));
#165860=CARTESIAN_POINT('Ctrl Pts',(14.4026149179538,-10.8763499173728,
397.528676470588));
#165861=CARTESIAN_POINT('Ctrl Pts',(13.3947726768058,-12.2109487310903,
396.034558823529));
#165862=CARTESIAN_POINT('Ctrl Pts',(12.1588589765331,-13.3376329379985,
394.540441176471));
#165863=CARTESIAN_POINT('Ctrl Pts',(10.9229452762603,-14.4643171449067,
393.046323529412));
#165864=CARTESIAN_POINT('Ctrl Pts',(9.50104767561053,-15.3447188656481,
391.552205882353));
#165865=CARTESIAN_POINT('Ctrl Pts',(8.07915007496071,-16.2251205863895,
390.058088235294));
#165866=CARTESIAN_POINT('Ctrl Pts',(6.51968959134574,-16.8292587962898,
388.563970588235));
#165867=CARTESIAN_POINT('Ctrl Pts',(4.96022910773078,-17.4333970061901,
387.069852941177));
#165868=CARTESIAN_POINT('Ctrl Pts',(3.31631129755346,-17.7406985030951,
385.575735294118));
#165869=CARTESIAN_POINT('Ctrl Pts',(1.67239348737615,-18.048,384.081617647059));
#165870=CARTESIAN_POINT('Ctrl Pts',(0.,-18.048,382.5875));
#165871=CARTESIAN_POINT('Ctrl Pts',(-1.67239348737615,-18.048,381.093382352941));
#165872=CARTESIAN_POINT('Ctrl Pts',(-3.31631129755346,-17.7406985030951,
379.599264705882));
#165873=CARTESIAN_POINT('Ctrl Pts',(-4.96022910773077,-17.4333970061901,
378.105147058823));
#165874=CARTESIAN_POINT('Ctrl Pts',(-6.51968959134574,-16.8292587962898,
376.611029411765));
#165875=CARTESIAN_POINT('Ctrl Pts',(-8.07915007496071,-16.2251205863895,
375.116911764706));
#165876=CARTESIAN_POINT('Ctrl Pts',(-9.50104767561052,-15.3447188656481,
373.622794117647));
#165877=CARTESIAN_POINT('Ctrl Pts',(-10.9229452762603,-14.4643171449067,
372.128676470588));
#165878=CARTESIAN_POINT('Ctrl Pts',(-12.1588589765331,-13.3376329379985,
370.634558823529));
#165879=CARTESIAN_POINT('Ctrl Pts',(-13.3947726768058,-12.2109487310903,
369.140441176471));
#165880=CARTESIAN_POINT('Ctrl Pts',(-14.4026149179538,-10.8763499173728,
367.646323529412));
#165881=CARTESIAN_POINT('Ctrl Pts',(-15.4104571591017,-9.54175110365538,
366.152205882353));
#165882=CARTESIAN_POINT('Ctrl Pts',(-16.1559070823762,-8.04468584505497,
364.658088235294));
#165883=CARTESIAN_POINT('Ctrl Pts',(-16.9013570056506,-6.54762058645456,
363.163970588235));
#165884=CARTESIAN_POINT('Ctrl Pts',(-17.3590292079831,-4.93906964482095,
361.669852941177));
#165885=CARTESIAN_POINT('Ctrl Pts',(-17.8167014103155,-3.33051870318735,
360.175735294118));
#165886=CARTESIAN_POINT('Ctrl Pts',(-17.9710104137728,-1.66525935159368,
358.681617647059));
#165887=CARTESIAN_POINT('Ctrl Pts',(-18.1253194172301,-1.10985572039171E-15,
357.1875));
#165888=CARTESIAN_POINT('Ctrl Pts',(-17.9710104137728,1.66525935159367,
355.693382352941));
#165889=CARTESIAN_POINT('Ctrl Pts',(-17.8167014103155,3.33051870318735,
354.199264705883));
#165890=CARTESIAN_POINT('Ctrl Pts',(-17.3590292079831,4.93906964482096,
352.705147058824));
#165891=CARTESIAN_POINT('Ctrl Pts',(-16.9013570056506,6.54762058645456,
351.211029411765));
#165892=CARTESIAN_POINT('Ctrl Pts',(-16.1559070823762,8.04468584505497,
349.716911764706));
#165893=CARTESIAN_POINT('Ctrl Pts',(-15.4104571591017,9.54175110365538,
348.222794117647));
#165894=CARTESIAN_POINT('Ctrl Pts',(-14.4026149179538,10.8763499173728,
346.728676470588));
#165895=CARTESIAN_POINT('Ctrl Pts',(-13.3947726768058,12.2109487310903,
345.234558823529));
#165896=CARTESIAN_POINT('Ctrl Pts',(-12.1588589765331,13.3376329379985,
343.740441176471));
#165897=CARTESIAN_POINT('Ctrl Pts',(-10.9229452762603,14.4643171449067,
342.246323529412));
#165898=CARTESIAN_POINT('Ctrl Pts',(-9.50104767561052,15.3447188656481,
340.752205882353));
#165899=CARTESIAN_POINT('Ctrl Pts',(-8.07915007496071,16.2251205863895,
339.258088235294));
#165900=CARTESIAN_POINT('Ctrl Pts',(-6.51968959134574,16.8292587962898,
337.763970588235));
#165901=CARTESIAN_POINT('Ctrl Pts',(-4.96022910773078,17.4333970061901,
336.269852941177));
#165902=CARTESIAN_POINT('Ctrl Pts',(-3.31631129755346,17.7406985030951,
334.775735294118));
#165903=CARTESIAN_POINT('Ctrl Pts',(-1.67239348737615,18.048,333.281617647059));
#165904=CARTESIAN_POINT('Ctrl Pts',(-2.21024254310115E-15,18.048,331.7875));
#165905=CARTESIAN_POINT('Ctrl Pts',(1.67239348737616,18.048,330.293382352941));
#165906=CARTESIAN_POINT('Ctrl Pts',(3.31631129755346,17.7406985030951,328.799264705882));
#165907=CARTESIAN_POINT('Ctrl Pts',(4.96022910773077,17.4333970061901,327.305147058824));
#165908=CARTESIAN_POINT('Ctrl Pts',(6.51968959134575,16.8292587962898,325.811029411765));
#165909=CARTESIAN_POINT('Ctrl Pts',(8.07915007496071,16.2251205863895,324.316911764706));
#165910=CARTESIAN_POINT('Ctrl Pts',(9.50104767561053,15.3447188656481,322.822794117647));
#165911=CARTESIAN_POINT('Ctrl Pts',(10.9229452762603,14.4643171449067,321.328676470588));
#165912=CARTESIAN_POINT('Ctrl Pts',(12.1588589765331,13.3376329379985,319.834558823529));
#165913=CARTESIAN_POINT('Ctrl Pts',(13.3947726768058,12.2109487310903,318.340441176471));
#165914=CARTESIAN_POINT('Ctrl Pts',(14.4026149179538,10.8763499173728,316.846323529412));
#165915=CARTESIAN_POINT('Ctrl Pts',(15.4104571591017,9.54175110365538,315.352205882353));
#165916=CARTESIAN_POINT('Ctrl Pts',(16.1559070823762,8.04468584505496,313.858088235294));
#165917=CARTESIAN_POINT('Ctrl Pts',(16.9013570056506,6.54762058645456,312.363970588235));
#165918=CARTESIAN_POINT('Ctrl Pts',(17.3590292079831,4.93906964482096,310.869852941176));
#165919=CARTESIAN_POINT('Ctrl Pts',(17.8167014103155,3.33051870318735,309.375735294118));
#165920=CARTESIAN_POINT('Ctrl Pts',(17.9710104137728,1.66525935159367,307.881617647059));
#165921=CARTESIAN_POINT('Ctrl Pts',(18.1253194172301,3.32956716117513E-15,
306.3875));
#165922=CARTESIAN_POINT('Ctrl Pts',(17.9710104137728,-1.66525935159367,
304.893382352941));
#165923=CARTESIAN_POINT('Ctrl Pts',(17.8167014103155,-3.33051870318736,
303.399264705882));
#165924=CARTESIAN_POINT('Ctrl Pts',(17.3590292079831,-4.93906964482095,
301.905147058824));
#165925=CARTESIAN_POINT('Ctrl Pts',(16.9013570056506,-6.54762058645456,
300.411029411765));
#165926=CARTESIAN_POINT('Ctrl Pts',(16.1559070823762,-8.04468584505497,
298.916911764706));
#165927=CARTESIAN_POINT('Ctrl Pts',(15.4104571591017,-9.54175110365538,
297.422794117647));
#165928=CARTESIAN_POINT('Ctrl Pts',(14.4026149179538,-10.8763499173728,
295.928676470588));
#165929=CARTESIAN_POINT('Ctrl Pts',(13.3947726768058,-12.2109487310903,
294.43455882353));
#165930=CARTESIAN_POINT('Ctrl Pts',(12.1588589765331,-13.3376329379985,
292.940441176471));
#165931=CARTESIAN_POINT('Ctrl Pts',(10.9229452762603,-14.4643171449067,
291.446323529412));
#165932=CARTESIAN_POINT('Ctrl Pts',(9.50104767561053,-15.3447188656481,
289.952205882353));
#165933=CARTESIAN_POINT('Ctrl Pts',(8.07915007496071,-16.2251205863895,
288.458088235294));
#165934=CARTESIAN_POINT('Ctrl Pts',(6.51968959134574,-16.8292587962898,
286.963970588235));
#165935=CARTESIAN_POINT('Ctrl Pts',(4.96022910773078,-17.4333970061901,
285.469852941177));
#165936=CARTESIAN_POINT('Ctrl Pts',(3.31631129755346,-17.7406985030951,
283.975735294118));
#165937=CARTESIAN_POINT('Ctrl Pts',(1.67239348737615,-18.048,282.481617647059));
#165938=CARTESIAN_POINT('Ctrl Pts',(0.,-18.048,280.9875));
#165939=CARTESIAN_POINT('Ctrl Pts',(-1.67239348737615,-18.048,279.493382352941));
#165940=CARTESIAN_POINT('Ctrl Pts',(-3.31631129755346,-17.7406985030951,
277.999264705882));
#165941=CARTESIAN_POINT('Ctrl Pts',(-4.96022910773077,-17.4333970061901,
276.505147058824));
#165942=CARTESIAN_POINT('Ctrl Pts',(-6.51968959134574,-16.8292587962898,
275.011029411765));
#165943=CARTESIAN_POINT('Ctrl Pts',(-8.07915007496071,-16.2251205863895,
273.516911764706));
#165944=CARTESIAN_POINT('Ctrl Pts',(-9.50104767561052,-15.3447188656481,
272.022794117647));
#165945=CARTESIAN_POINT('Ctrl Pts',(-10.9229452762603,-14.4643171449067,
270.528676470588));
#165946=CARTESIAN_POINT('Ctrl Pts',(-12.1588589765331,-13.3376329379985,
269.034558823529));
#165947=CARTESIAN_POINT('Ctrl Pts',(-13.3947726768058,-12.2109487310903,
267.540441176471));
#165948=CARTESIAN_POINT('Ctrl Pts',(-14.4026149179538,-10.8763499173728,
266.046323529412));
#165949=CARTESIAN_POINT('Ctrl Pts',(-15.4104571591017,-9.54175110365538,
264.552205882353));
#165950=CARTESIAN_POINT('Ctrl Pts',(-16.1559070823762,-8.04468584505497,
263.058088235294));
#165951=CARTESIAN_POINT('Ctrl Pts',(-16.9013570056506,-6.54762058645456,
261.563970588235));
#165952=CARTESIAN_POINT('Ctrl Pts',(-17.3590292079831,-4.93906964482095,
260.069852941176));
#165953=CARTESIAN_POINT('Ctrl Pts',(-17.8167014103155,-3.33051870318735,
258.575735294118));
#165954=CARTESIAN_POINT('Ctrl Pts',(-17.9710104137728,-1.66525935159368,
257.081617647059));
#165955=CARTESIAN_POINT('Ctrl Pts',(-18.1253194172301,-1.10985572039171E-15,
255.5875));
#165956=CARTESIAN_POINT('Ctrl Pts',(-17.9710104137728,1.66525935159367,
254.093382352941));
#165957=CARTESIAN_POINT('Ctrl Pts',(-17.8167014103155,3.33051870318735,
252.599264705882));
#165958=CARTESIAN_POINT('Ctrl Pts',(-17.3590292079831,4.93906964482096,
251.105147058823));
#165959=CARTESIAN_POINT('Ctrl Pts',(-16.9013570056506,6.54762058645456,
249.611029411765));
#165960=CARTESIAN_POINT('Ctrl Pts',(-16.1559070823762,8.04468584505497,
248.116911764706));
#165961=CARTESIAN_POINT('Ctrl Pts',(-15.4104571591017,9.54175110365538,
246.622794117647));
#165962=CARTESIAN_POINT('Ctrl Pts',(-14.4026149179538,10.8763499173728,
245.128676470588));
#165963=CARTESIAN_POINT('Ctrl Pts',(-13.3947726768058,12.2109487310903,
243.634558823529));
#165964=CARTESIAN_POINT('Ctrl Pts',(-12.1588589765331,13.3376329379985,
242.140441176471));
#165965=CARTESIAN_POINT('Ctrl Pts',(-10.9229452762603,14.4643171449067,
240.646323529412));
#165966=CARTESIAN_POINT('Ctrl Pts',(-9.50104767561052,15.3447188656481,
239.152205882353));
#165967=CARTESIAN_POINT('Ctrl Pts',(-8.07915007496071,16.2251205863895,
237.658088235294));
#165968=CARTESIAN_POINT('Ctrl Pts',(-6.51968959134574,16.8292587962898,
236.163970588235));
#165969=CARTESIAN_POINT('Ctrl Pts',(-4.96022910773078,17.4333970061901,
234.669852941177));
#165970=CARTESIAN_POINT('Ctrl Pts',(-3.31631129755346,17.7406985030951,
233.175735294118));
#165971=CARTESIAN_POINT('Ctrl Pts',(-1.67239348737615,18.048,231.681617647059));
#165972=CARTESIAN_POINT('Ctrl Pts',(-2.21024254310115E-15,18.048,230.1875));
#165973=CARTESIAN_POINT('Ctrl Pts',(1.67239348737616,18.048,228.693382352941));
#165974=CARTESIAN_POINT('Ctrl Pts',(3.31631129755346,17.7406985030951,227.199264705882));
#165975=CARTESIAN_POINT('Ctrl Pts',(4.96022910773077,17.4333970061901,225.705147058824));
#165976=CARTESIAN_POINT('Ctrl Pts',(6.51968959134575,16.8292587962898,224.211029411765));
#165977=CARTESIAN_POINT('Ctrl Pts',(8.07915007496071,16.2251205863895,222.716911764706));
#165978=CARTESIAN_POINT('Ctrl Pts',(9.50104767561053,15.3447188656481,221.222794117647));
#165979=CARTESIAN_POINT('Ctrl Pts',(10.9229452762603,14.4643171449067,219.728676470588));
#165980=CARTESIAN_POINT('Ctrl Pts',(12.1588589765331,13.3376329379985,218.234558823529));
#165981=CARTESIAN_POINT('Ctrl Pts',(13.3947726768058,12.2109487310903,216.740441176471));
#165982=CARTESIAN_POINT('Ctrl Pts',(14.4026149179538,10.8763499173728,215.246323529412));
#165983=CARTESIAN_POINT('Ctrl Pts',(15.4104571591017,9.54175110365538,213.752205882353));
#165984=CARTESIAN_POINT('Ctrl Pts',(16.1559070823762,8.04468584505496,212.258088235294));
#165985=CARTESIAN_POINT('Ctrl Pts',(16.9013570056506,6.54762058645456,210.763970588235));
#165986=CARTESIAN_POINT('Ctrl Pts',(17.3590292079831,4.93906964482096,209.269852941177));
#165987=CARTESIAN_POINT('Ctrl Pts',(17.8167014103155,3.33051870318735,207.775735294118));
#165988=CARTESIAN_POINT('Ctrl Pts',(17.9710104137728,1.66525935159367,206.281617647059));
#165989=CARTESIAN_POINT('Ctrl Pts',(18.1253194172301,3.32956716117513E-15,
204.7875));
#165990=CARTESIAN_POINT('Ctrl Pts',(17.9710104137728,-1.66525935159367,
203.293382352941));
#165991=CARTESIAN_POINT('Ctrl Pts',(17.8167014103155,-3.33051870318736,
201.799264705882));
#165992=CARTESIAN_POINT('Ctrl Pts',(17.3590292079831,-4.93906964482095,
200.305147058824));
#165993=CARTESIAN_POINT('Ctrl Pts',(16.9013570056506,-6.54762058645456,
198.811029411765));
#165994=CARTESIAN_POINT('Ctrl Pts',(16.1559070823762,-8.04468584505497,
197.316911764706));
#165995=CARTESIAN_POINT('Ctrl Pts',(15.4104571591017,-9.54175110365538,
195.822794117647));
#165996=CARTESIAN_POINT('Ctrl Pts',(14.4026149179538,-10.8763499173728,
194.328676470588));
#165997=CARTESIAN_POINT('Ctrl Pts',(13.3947726768058,-12.2109487310903,
192.834558823529));
#165998=CARTESIAN_POINT('Ctrl Pts',(12.1588589765331,-13.3376329379985,
191.340441176471));
#165999=CARTESIAN_POINT('Ctrl Pts',(10.9229452762603,-14.4643171449067,
189.846323529412));
#166000=CARTESIAN_POINT('Ctrl Pts',(9.50104767561053,-15.3447188656481,
188.352205882353));
#166001=CARTESIAN_POINT('Ctrl Pts',(8.07915007496071,-16.2251205863895,
186.858088235294));
#166002=CARTESIAN_POINT('Ctrl Pts',(6.51968959134574,-16.8292587962898,
185.363970588235));
#166003=CARTESIAN_POINT('Ctrl Pts',(4.96022910773078,-17.4333970061901,
183.869852941176));
#166004=CARTESIAN_POINT('Ctrl Pts',(3.31631129755346,-17.7406985030951,
182.375735294118));
#166005=CARTESIAN_POINT('Ctrl Pts',(1.67239348737615,-18.048,180.881617647059));
#166006=CARTESIAN_POINT('Ctrl Pts',(0.,-18.048,179.3875));
#166007=CARTESIAN_POINT('Ctrl Pts',(-1.67239348737615,-18.048,177.893382352941));
#166008=CARTESIAN_POINT('Ctrl Pts',(-3.31631129755346,-17.7406985030951,
176.399264705882));
#166009=CARTESIAN_POINT('Ctrl Pts',(-4.96022910773077,-17.4333970061901,
174.905147058824));
#166010=CARTESIAN_POINT('Ctrl Pts',(-6.51968959134574,-16.8292587962898,
173.411029411765));
#166011=CARTESIAN_POINT('Ctrl Pts',(-8.07915007496071,-16.2251205863895,
171.916911764706));
#166012=CARTESIAN_POINT('Ctrl Pts',(-9.50104767561052,-15.3447188656481,
170.422794117647));
#166013=CARTESIAN_POINT('Ctrl Pts',(-10.9229452762603,-14.4643171449067,
168.928676470588));
#166014=CARTESIAN_POINT('Ctrl Pts',(-12.1588589765331,-13.3376329379985,
167.43455882353));
#166015=CARTESIAN_POINT('Ctrl Pts',(-13.3947726768058,-12.2109487310903,
165.940441176471));
#166016=CARTESIAN_POINT('Ctrl Pts',(-14.4026149179538,-10.8763499173728,
164.446323529412));
#166017=CARTESIAN_POINT('Ctrl Pts',(-15.4104571591017,-9.54175110365538,
162.952205882353));
#166018=CARTESIAN_POINT('Ctrl Pts',(-16.1559070823762,-8.04468584505497,
161.458088235294));
#166019=CARTESIAN_POINT('Ctrl Pts',(-16.9013570056506,-6.54762058645456,
159.963970588235));
#166020=CARTESIAN_POINT('Ctrl Pts',(-17.3590292079831,-4.93906964482095,
158.469852941177));
#166021=CARTESIAN_POINT('Ctrl Pts',(-17.8167014103155,-3.33051870318735,
156.975735294118));
#166022=CARTESIAN_POINT('Ctrl Pts',(-17.9710104137728,-1.66525935159368,
155.481617647059));
#166023=CARTESIAN_POINT('Ctrl Pts',(-18.1253194172301,-1.10985572039171E-15,
153.9875));
#166024=CARTESIAN_POINT('Ctrl Pts',(-17.9710104137728,1.66525935159367,
152.493382352941));
#166025=CARTESIAN_POINT('Ctrl Pts',(-17.8167014103155,3.33051870318735,
150.999264705882));
#166026=CARTESIAN_POINT('Ctrl Pts',(-17.3590292079831,4.93906964482096,
149.505147058824));
#166027=CARTESIAN_POINT('Ctrl Pts',(-16.9013570056506,6.54762058645456,
148.011029411765));
#166028=CARTESIAN_POINT('Ctrl Pts',(-16.1559070823762,8.04468584505497,
146.516911764706));
#166029=CARTESIAN_POINT('Ctrl Pts',(-15.4104571591017,9.54175110365538,
145.022794117647));
#166030=CARTESIAN_POINT('Ctrl Pts',(-14.4026149179538,10.8763499173728,
143.528676470588));
#166031=CARTESIAN_POINT('Ctrl Pts',(-13.3947726768058,12.2109487310903,
142.034558823529));
#166032=CARTESIAN_POINT('Ctrl Pts',(-12.1588589765331,13.3376329379985,
140.540441176471));
#166033=CARTESIAN_POINT('Ctrl Pts',(-10.9229452762603,14.4643171449067,
139.046323529412));
#166034=CARTESIAN_POINT('Ctrl Pts',(-9.50104767561052,15.3447188656481,
137.552205882353));
#166035=CARTESIAN_POINT('Ctrl Pts',(-8.07915007496071,16.2251205863895,
136.058088235294));
#166036=CARTESIAN_POINT('Ctrl Pts',(-6.51968959134574,16.8292587962898,
134.563970588235));
#166037=CARTESIAN_POINT('Ctrl Pts',(-4.96022910773078,17.4333970061901,
133.069852941176));
#166038=CARTESIAN_POINT('Ctrl Pts',(-3.31631129755346,17.7406985030951,
131.575735294118));
#166039=CARTESIAN_POINT('Ctrl Pts',(-1.67239348737615,18.048,130.081617647059));
#166040=CARTESIAN_POINT('Ctrl Pts',(-2.21024254310115E-15,18.048,128.5875));
#166041=CARTESIAN_POINT('Ctrl Pts',(1.67239348737616,18.048,127.093382352941));
#166042=CARTESIAN_POINT('Ctrl Pts',(3.31631129755346,17.7406985030951,125.599264705882));
#166043=CARTESIAN_POINT('Ctrl Pts',(4.96022910773077,17.4333970061901,124.105147058824));
#166044=CARTESIAN_POINT('Ctrl Pts',(6.51968959134575,16.8292587962898,122.611029411765));
#166045=CARTESIAN_POINT('Ctrl Pts',(8.07915007496071,16.2251205863895,121.116911764706));
#166046=CARTESIAN_POINT('Ctrl Pts',(9.50104767561053,15.3447188656481,119.622794117647));
#166047=CARTESIAN_POINT('Ctrl Pts',(10.9229452762603,14.4643171449067,118.128676470588));
#166048=CARTESIAN_POINT('Ctrl Pts',(12.1588589765331,13.3376329379985,116.634558823529));
#166049=CARTESIAN_POINT('Ctrl Pts',(13.3947726768058,12.2109487310903,115.140441176471));
#166050=CARTESIAN_POINT('Ctrl Pts',(14.4026149179538,10.8763499173728,113.646323529412));
#166051=CARTESIAN_POINT('Ctrl Pts',(15.4104571591017,9.54175110365538,112.152205882353));
#166052=CARTESIAN_POINT('Ctrl Pts',(16.1559070823762,8.04468584505496,110.658088235294));
#166053=CARTESIAN_POINT('Ctrl Pts',(16.9013570056506,6.54762058645456,109.163970588235));
#166054=CARTESIAN_POINT('Ctrl Pts',(17.3590292079831,4.93906964482096,107.669852941177));
#166055=CARTESIAN_POINT('Ctrl Pts',(17.8167014103155,3.33051870318735,106.175735294118));
#166056=CARTESIAN_POINT('Ctrl Pts',(17.9710104137728,1.66525935159367,104.681617647059));
#166057=CARTESIAN_POINT('Ctrl Pts',(18.1253194172301,3.32956716117513E-15,
103.1875));
#166058=CARTESIAN_POINT('Ctrl Pts',(17.9710104137728,-1.66525935159367,
101.693382352941));
#166059=CARTESIAN_POINT('Ctrl Pts',(17.8167014103155,-3.33051870318736,
100.199264705882));
#166060=CARTESIAN_POINT('Ctrl Pts',(17.3590292079831,-4.93906964482095,
98.7051470588236));
#166061=CARTESIAN_POINT('Ctrl Pts',(16.9013570056506,-6.54762058645456,
97.2110294117647));
#166062=CARTESIAN_POINT('Ctrl Pts',(16.1559070823762,-8.04468584505497,
95.7169117647059));
#166063=CARTESIAN_POINT('Ctrl Pts',(15.4104571591017,-9.54175110365538,
94.222794117647));
#166064=CARTESIAN_POINT('Ctrl Pts',(14.4026149179538,-10.8763499173728,
92.7286764705884));
#166065=CARTESIAN_POINT('Ctrl Pts',(13.3947726768058,-12.2109487310903,
91.2345588235295));
#166066=CARTESIAN_POINT('Ctrl Pts',(12.1588589765331,-13.3376329379985,
89.7404411764706));
#166067=CARTESIAN_POINT('Ctrl Pts',(10.9229452762603,-14.4643171449067,
88.2463235294117));
#166068=CARTESIAN_POINT('Ctrl Pts',(9.50104767561053,-15.3447188656481,
86.7522058823529));
#166069=CARTESIAN_POINT('Ctrl Pts',(8.07915007496071,-16.2251205863895,
85.2580882352942));
#166070=CARTESIAN_POINT('Ctrl Pts',(6.51968959134574,-16.8292587962898,
83.7639705882354));
#166071=CARTESIAN_POINT('Ctrl Pts',(4.96022910773078,-17.4333970061901,
82.2698529411765));
#166072=CARTESIAN_POINT('Ctrl Pts',(3.31631129755346,-17.7406985030951,
80.7757352941176));
#166073=CARTESIAN_POINT('Ctrl Pts',(1.67239348737615,-18.048,79.2816176470588));
#166074=CARTESIAN_POINT('Ctrl Pts',(0.,-18.048,77.7875000000001));
#166075=CARTESIAN_POINT('Ctrl Pts',(-1.67239348737615,-18.048,76.2933823529413));
#166076=CARTESIAN_POINT('Ctrl Pts',(-3.31631129755346,-17.7406985030951,
74.7992647058824));
#166077=CARTESIAN_POINT('Ctrl Pts',(-4.96022910773077,-17.4333970061901,
73.3051470588235));
#166078=CARTESIAN_POINT('Ctrl Pts',(-6.51968959134574,-16.8292587962898,
71.8110294117647));
#166079=CARTESIAN_POINT('Ctrl Pts',(-8.07915007496071,-16.2251205863895,
70.316911764706));
#166080=CARTESIAN_POINT('Ctrl Pts',(-9.50104767561052,-15.3447188656481,
68.8227941176471));
#166081=CARTESIAN_POINT('Ctrl Pts',(-10.9229452762603,-14.4643171449067,
67.3286764705883));
#166082=CARTESIAN_POINT('Ctrl Pts',(-12.1588589765331,-13.3376329379985,
65.8345588235294));
#166083=CARTESIAN_POINT('Ctrl Pts',(-13.3947726768058,-12.2109487310903,
64.3404411764705));
#166084=CARTESIAN_POINT('Ctrl Pts',(-14.4026149179538,-10.8763499173728,
62.8463235294119));
#166085=CARTESIAN_POINT('Ctrl Pts',(-15.4104571591017,-9.54175110365538,
61.352205882353));
#166086=CARTESIAN_POINT('Ctrl Pts',(-16.1559070823762,-8.04468584505497,
59.8580882352941));
#166087=CARTESIAN_POINT('Ctrl Pts',(-16.9013570056506,-6.54762058645456,
58.3639705882353));
#166088=CARTESIAN_POINT('Ctrl Pts',(-17.3590292079831,-4.93906964482095,
56.8698529411764));
#166089=CARTESIAN_POINT('Ctrl Pts',(-17.8167014103155,-3.33051870318735,
55.3757352941178));
#166090=CARTESIAN_POINT('Ctrl Pts',(-17.9710104137728,-1.66525935159368,
53.8816176470589));
#166091=CARTESIAN_POINT('Ctrl Pts',(-18.1253194172301,-1.10985572039171E-15,
52.3875));
#166092=CARTESIAN_POINT('Ctrl Pts',(-17.9710104137728,1.66525935159367,
50.8933823529412));
#166093=CARTESIAN_POINT('Ctrl Pts',(-17.8167014103155,3.33051870318735,
49.3992647058823));
#166094=CARTESIAN_POINT('Ctrl Pts',(-17.3590292079831,4.93906964482096,
47.9051470588237));
#166095=CARTESIAN_POINT('Ctrl Pts',(-16.9013570056506,6.54762058645456,
46.4110294117648));
#166096=CARTESIAN_POINT('Ctrl Pts',(-16.1559070823762,8.04468584505497,
44.9169117647059));
#166097=CARTESIAN_POINT('Ctrl Pts',(-15.4104571591017,9.54175110365538,
43.422794117647));
#166098=CARTESIAN_POINT('Ctrl Pts',(-14.4026149179538,10.8763499173728,
41.9286764705882));
#166099=CARTESIAN_POINT('Ctrl Pts',(-13.3947726768058,12.2109487310903,
40.4345588235295));
#166100=CARTESIAN_POINT('Ctrl Pts',(-12.1588589765331,13.3376329379985,
38.9404411764707));
#166101=CARTESIAN_POINT('Ctrl Pts',(-10.9229452762603,14.4643171449067,
37.4463235294118));
#166102=CARTESIAN_POINT('Ctrl Pts',(-9.50104767561052,15.3447188656481,
35.9522058823529));
#166103=CARTESIAN_POINT('Ctrl Pts',(-8.07915007496071,16.2251205863895,
34.4580882352941));
#166104=CARTESIAN_POINT('Ctrl Pts',(-6.51968959134574,16.8292587962898,
32.9639705882354));
#166105=CARTESIAN_POINT('Ctrl Pts',(-4.96022910773078,17.4333970061901,
31.4698529411765));
#166106=CARTESIAN_POINT('Ctrl Pts',(-3.31631129755346,17.7406985030951,
29.9757352941177));
#166107=CARTESIAN_POINT('Ctrl Pts',(-1.67239348737615,18.048,28.4816176470588));
#166108=CARTESIAN_POINT('Ctrl Pts',(-2.21024254310115E-15,18.048,26.9874999999999));
#166109=CARTESIAN_POINT('Ctrl Pts',(1.67239348737616,18.048,25.4933823529413));
#166110=CARTESIAN_POINT('Ctrl Pts',(3.31631129755346,17.7406985030951,23.9992647058824));
#166111=CARTESIAN_POINT('Ctrl Pts',(4.96022910773077,17.4333970061901,22.5051470588236));
#166112=CARTESIAN_POINT('Ctrl Pts',(6.51968959134575,16.8292587962898,21.0110294117647));
#166113=CARTESIAN_POINT('Ctrl Pts',(8.07915007496071,16.2251205863895,19.5169117647058));
#166114=CARTESIAN_POINT('Ctrl Pts',(9.50104767561053,15.3447188656481,18.0227941176472));
#166115=CARTESIAN_POINT('Ctrl Pts',(10.9229452762603,14.4643171449067,16.5286764705883));
#166116=CARTESIAN_POINT('Ctrl Pts',(12.1588589765331,13.3376329379985,15.0345588235294));
#166117=CARTESIAN_POINT('Ctrl Pts',(13.3947726768058,12.2109487310903,13.5404411764706));
#166118=CARTESIAN_POINT('Ctrl Pts',(14.4026149179538,10.8763499173728,12.0463235294117));
#166119=CARTESIAN_POINT('Ctrl Pts',(15.4104571591017,9.54175110365538,10.5522058823531));
#166120=CARTESIAN_POINT('Ctrl Pts',(16.1559070823762,8.04468584505496,9.05808823529419));
#166121=CARTESIAN_POINT('Ctrl Pts',(16.9013570056506,6.54762058645456,7.56397058823533));
#166122=CARTESIAN_POINT('Ctrl Pts',(17.3590292079831,4.93906964482096,6.06985294117646));
#166123=CARTESIAN_POINT('Ctrl Pts',(17.8167014103155,3.33051870318735,4.57573529411759));
#166124=CARTESIAN_POINT('Ctrl Pts',(17.9710104137728,1.66525935159367,3.08161764705894));
#166125=CARTESIAN_POINT('Ctrl Pts',(18.1253194172301,3.32956716117513E-15,
1.58750000000007));
#166126=CARTESIAN_POINT('Ctrl Pts',(17.9710104137728,-1.66525935159367,
0.093382352941207));
#166127=CARTESIAN_POINT('Ctrl Pts',(17.8167014103155,-3.33051870318736,
-1.40073529411766));
#166128=CARTESIAN_POINT('Ctrl Pts',(17.3590292079831,-4.93906964482095,
-2.89485294117653));
#166129=CARTESIAN_POINT('Ctrl Pts',(16.9013570056506,-6.54762058645456,
-4.38897058823517));
#166130=CARTESIAN_POINT('Ctrl Pts',(16.1559070823762,-8.04468584505497,
-5.88308823529404));
#166131=CARTESIAN_POINT('Ctrl Pts',(15.4104571591017,-9.54175110365538,
-7.37720588235291));
#166132=CARTESIAN_POINT('Ctrl Pts',(14.4026149179538,-10.8763499173728,
-8.87132352941178));
#166133=CARTESIAN_POINT('Ctrl Pts',(13.3947726768058,-12.2109487310903,
-10.3654411764706));
#166134=CARTESIAN_POINT('Ctrl Pts',(12.1588589765331,-13.3376329379985,
-11.8595588235293));
#166135=CARTESIAN_POINT('Ctrl Pts',(10.9229452762603,-14.4643171449067,
-13.3536764705882));
#166136=CARTESIAN_POINT('Ctrl Pts',(9.50104767561053,-15.3447188656481,
-14.847794117647));
#166137=CARTESIAN_POINT('Ctrl Pts',(8.07915007496071,-16.2251205863895,
-16.3419117647059));
#166138=CARTESIAN_POINT('Ctrl Pts',(6.51968959134574,-16.8292587962898,
-17.8360294117648));
#166139=CARTESIAN_POINT('Ctrl Pts',(4.96022910773078,-17.4333970061901,
-19.3301470588234));
#166140=CARTESIAN_POINT('Ctrl Pts',(3.31631129755346,-17.7406985030951,
-20.8242647058823));
#166141=CARTESIAN_POINT('Ctrl Pts',(1.67239348737615,-18.048,-22.3183823529411));
#166142=CARTESIAN_POINT('Ctrl Pts',(0.,-18.048,-23.8125));
#166143=CARTESIAN_POINT('Ctrl Pts',(-1.67239348737615,-18.048,-25.3066176470589));
#166144=CARTESIAN_POINT('Ctrl Pts',(-3.31631129755346,-17.7406985030951,
-26.8007352941175));
#166145=CARTESIAN_POINT('Ctrl Pts',(-4.96022910773077,-17.4333970061901,
-28.2948529411764));
#166146=CARTESIAN_POINT('Ctrl Pts',(-6.51968959134574,-16.8292587962898,
-29.7889705882353));
#166147=CARTESIAN_POINT('Ctrl Pts',(-8.07915007496071,-16.2251205863895,
-31.2830882352941));
#166148=CARTESIAN_POINT('Ctrl Pts',(-9.50104767561052,-15.3447188656481,
-32.777205882353));
#166149=CARTESIAN_POINT('Ctrl Pts',(-10.9229452762603,-14.4643171449067,
-34.2713235294116));
#166150=CARTESIAN_POINT('Ctrl Pts',(-12.1588589765331,-13.3376329379985,
-35.7654411764705));
#166151=CARTESIAN_POINT('Ctrl Pts',(-13.3947726768058,-12.2109487310903,
-37.2595588235294));
#166152=CARTESIAN_POINT('Ctrl Pts',(-14.4026149179538,-10.8763499173728,
-38.7536764705882));
#166153=CARTESIAN_POINT('Ctrl Pts',(-15.4104571591017,-9.54175110365538,
-40.2477941176471));
#166154=CARTESIAN_POINT('Ctrl Pts',(-16.1559070823762,-8.04468584505497,
-41.7419117647058));
#166155=CARTESIAN_POINT('Ctrl Pts',(-16.9013570056506,-6.54762058645456,
-43.2360294117646));
#166156=CARTESIAN_POINT('Ctrl Pts',(-17.3590292079831,-4.93906964482095,
-44.7301470588235));
#166157=CARTESIAN_POINT('Ctrl Pts',(-17.8167014103155,-3.33051870318735,
-46.2242647058824));
#166158=CARTESIAN_POINT('Ctrl Pts',(-17.9710104137728,-1.66525935159368,
-47.7183823529412));
#166159=CARTESIAN_POINT('Ctrl Pts',(-18.1253194172301,-1.10985572039171E-15,
-49.2124999999999));
#166160=CARTESIAN_POINT('Ctrl Pts',(-17.9710104137728,1.66525935159367,
-50.7066176470587));
#166161=CARTESIAN_POINT('Ctrl Pts',(-17.8167014103155,3.33051870318735,
-52.2007352941176));
#166162=CARTESIAN_POINT('Ctrl Pts',(-17.3590292079831,4.93906964482096,
-53.6948529411765));
#166163=CARTESIAN_POINT('Ctrl Pts',(-16.9013570056506,6.54762058645456,
-55.1889705882354));
#166164=CARTESIAN_POINT('Ctrl Pts',(-16.1559070823762,8.04468584505497,
-56.683088235294));
#166165=CARTESIAN_POINT('Ctrl Pts',(-15.4104571591017,9.54175110365538,
-58.1772058823529));
#166166=CARTESIAN_POINT('Ctrl Pts',(-14.4026149179538,10.8763499173728,
-59.6713235294117));
#166167=CARTESIAN_POINT('Ctrl Pts',(-13.3947726768058,12.2109487310903,
-61.1654411764706));
#166168=CARTESIAN_POINT('Ctrl Pts',(-12.1588589765331,13.3376329379985,
-62.6595588235295));
#166169=CARTESIAN_POINT('Ctrl Pts',(-10.9229452762603,14.4643171449067,
-64.1536764705881));
#166170=CARTESIAN_POINT('Ctrl Pts',(-9.50104767561052,15.3447188656481,
-65.647794117647));
#166171=CARTESIAN_POINT('Ctrl Pts',(-8.07915007496071,16.2251205863895,
-67.1419117647059));
#166172=CARTESIAN_POINT('Ctrl Pts',(-6.51968959134574,16.8292587962898,
-68.6360294117647));
#166173=CARTESIAN_POINT('Ctrl Pts',(-4.96022910773078,17.4333970061901,
-70.1301470588236));
#166174=CARTESIAN_POINT('Ctrl Pts',(-3.31631129755346,17.7406985030951,
-71.6242647058822));
#166175=CARTESIAN_POINT('Ctrl Pts',(-1.67239348737615,18.048,-73.1183823529411));
#166176=CARTESIAN_POINT('Ctrl Pts',(-2.21024254310115E-15,18.048,-74.6125));
#166177=CARTESIAN_POINT('Ctrl Pts',(1.67239348737616,18.048,-76.1066176470589));
#166178=CARTESIAN_POINT('Ctrl Pts',(3.31631129755346,17.7406985030951,-77.6007352941177));
#166179=CARTESIAN_POINT('Ctrl Pts',(4.96022910773077,17.4333970061901,-79.0948529411764));
#166180=CARTESIAN_POINT('Ctrl Pts',(6.51968959134575,16.8292587962898,-80.5889705882352));
#166181=CARTESIAN_POINT('Ctrl Pts',(8.07915007496071,16.2251205863895,-82.0830882352941));
#166182=CARTESIAN_POINT('Ctrl Pts',(9.50104767561053,15.3447188656481,-83.577205882353));
#166183=CARTESIAN_POINT('Ctrl Pts',(10.9229452762603,14.4643171449067,-85.0713235294118));
#166184=CARTESIAN_POINT('Ctrl Pts',(12.1588589765331,13.3376329379985,-86.5654411764705));
#166185=CARTESIAN_POINT('Ctrl Pts',(13.3947726768058,12.2109487310903,-88.0595588235294));
#166186=CARTESIAN_POINT('Ctrl Pts',(14.4026149179538,10.8763499173728,-89.5536764705882));
#166187=CARTESIAN_POINT('Ctrl Pts',(15.4104571591017,9.54175110365538,-91.0477941176471));
#166188=CARTESIAN_POINT('Ctrl Pts',(16.1559070823762,8.04468584505496,-92.541911764706));
#166189=CARTESIAN_POINT('Ctrl Pts',(16.9013570056506,6.54762058645456,-94.0360294117646));
#166190=CARTESIAN_POINT('Ctrl Pts',(17.3590292079831,4.93906964482096,-95.5301470588235));
#166191=CARTESIAN_POINT('Ctrl Pts',(17.8167014103155,3.33051870318735,-97.0242647058824));
#166192=CARTESIAN_POINT('Ctrl Pts',(17.9710104137728,1.66525935159367,-98.5183823529412));
#166193=CARTESIAN_POINT('Ctrl Pts',(18.1253194172301,3.32956716117513E-15,
-100.0125));
#166194=CARTESIAN_POINT('Ctrl Pts',(17.9710104137728,-1.66525935159367,
-101.506617647059));
#166195=CARTESIAN_POINT('Ctrl Pts',(17.8167014103155,-3.33051870318736,
-103.000735294118));
#166196=CARTESIAN_POINT('Ctrl Pts',(17.3590292079831,-4.93906964482095,
-104.494852941176));
#166197=CARTESIAN_POINT('Ctrl Pts',(16.9013570056506,-6.54762058645456,
-105.988970588235));
#166198=CARTESIAN_POINT('Ctrl Pts',(16.1559070823762,-8.04468584505497,
-107.483088235294));
#166199=CARTESIAN_POINT('Ctrl Pts',(15.4104571591017,-9.54175110365538,
-108.977205882353));
#166200=CARTESIAN_POINT('Ctrl Pts',(14.4026149179538,-10.8763499173728,
-110.471323529412));
#166201=CARTESIAN_POINT('Ctrl Pts',(13.3947726768058,-12.2109487310903,
-111.965441176471));
#166202=CARTESIAN_POINT('Ctrl Pts',(12.1588589765331,-13.3376329379985,
-113.459558823529));
#166203=CARTESIAN_POINT('Ctrl Pts',(10.9229452762603,-14.4643171449067,
-114.953676470588));
#166204=CARTESIAN_POINT('Ctrl Pts',(9.50104767561053,-15.3447188656481,
-116.447794117647));
#166205=CARTESIAN_POINT('Ctrl Pts',(8.07915007496071,-16.2251205863895,
-117.941911764706));
#166206=CARTESIAN_POINT('Ctrl Pts',(6.51968959134574,-16.8292587962898,
-119.436029411765));
#166207=CARTESIAN_POINT('Ctrl Pts',(4.96022910773078,-17.4333970061901,
-120.930147058824));
#166208=CARTESIAN_POINT('Ctrl Pts',(3.31631129755346,-17.7406985030951,
-122.424264705882));
#166209=CARTESIAN_POINT('Ctrl Pts',(1.67239348737615,-18.048,-123.918382352941));
#166210=CARTESIAN_POINT('Ctrl Pts',(0.,-18.048,-125.4125));
#166211=CARTESIAN_POINT('Ctrl Pts',(-1.67239348737615,-18.048,-126.906617647059));
#166212=CARTESIAN_POINT('Ctrl Pts',(-3.31631129755346,-17.7406985030951,
-128.400735294118));
#166213=CARTESIAN_POINT('Ctrl Pts',(-4.96022910773077,-17.4333970061901,
-129.894852941177));
#166214=CARTESIAN_POINT('Ctrl Pts',(-6.51968959134574,-16.8292587962898,
-131.388970588235));
#166215=CARTESIAN_POINT('Ctrl Pts',(-8.07915007496071,-16.2251205863895,
-132.883088235294));
#166216=CARTESIAN_POINT('Ctrl Pts',(-9.50104767561052,-15.3447188656481,
-134.377205882353));
#166217=CARTESIAN_POINT('Ctrl Pts',(-10.9229452762603,-14.4643171449067,
-135.871323529412));
#166218=CARTESIAN_POINT('Ctrl Pts',(-12.1588589765331,-13.3376329379985,
-137.365441176471));
#166219=CARTESIAN_POINT('Ctrl Pts',(-13.3947726768058,-12.2109487310903,
-138.859558823529));
#166220=CARTESIAN_POINT('Ctrl Pts',(-14.4026149179538,-10.8763499173728,
-140.353676470588));
#166221=CARTESIAN_POINT('Ctrl Pts',(-15.4104571591017,-9.54175110365538,
-141.847794117647));
#166222=CARTESIAN_POINT('Ctrl Pts',(-16.1559070823762,-8.04468584505497,
-143.341911764706));
#166223=CARTESIAN_POINT('Ctrl Pts',(-16.9013570056506,-6.54762058645456,
-144.836029411765));
#166224=CARTESIAN_POINT('Ctrl Pts',(-17.3590292079831,-4.93906964482095,
-146.330147058823));
#166225=CARTESIAN_POINT('Ctrl Pts',(-17.8167014103155,-3.33051870318735,
-147.824264705882));
#166226=CARTESIAN_POINT('Ctrl Pts',(-17.9710104137728,-1.66525935159368,
-149.318382352941));
#166227=CARTESIAN_POINT('Ctrl Pts',(-18.1253194172301,-1.10985572039171E-15,
-150.8125));
#166228=CARTESIAN_POINT('Ctrl Pts',(-17.9710104137728,1.66525935159367,
-152.306617647059));
#166229=CARTESIAN_POINT('Ctrl Pts',(-17.8167014103155,3.33051870318735,
-153.800735294118));
#166230=CARTESIAN_POINT('Ctrl Pts',(-17.3590292079831,4.93906964482096,
-155.294852941176));
#166231=CARTESIAN_POINT('Ctrl Pts',(-16.9013570056506,6.54762058645456,
-156.788970588235));
#166232=CARTESIAN_POINT('Ctrl Pts',(-16.1559070823762,8.04468584505497,
-158.283088235294));
#166233=CARTESIAN_POINT('Ctrl Pts',(-15.4104571591017,9.54175110365538,
-159.777205882353));
#166234=CARTESIAN_POINT('Ctrl Pts',(-14.4026149179538,10.8763499173728,
-161.271323529412));
#166235=CARTESIAN_POINT('Ctrl Pts',(-13.3947726768058,12.2109487310903,
-162.765441176471));
#166236=CARTESIAN_POINT('Ctrl Pts',(-12.1588589765331,13.3376329379985,
-164.259558823529));
#166237=CARTESIAN_POINT('Ctrl Pts',(-10.9229452762603,14.4643171449067,
-165.753676470588));
#166238=CARTESIAN_POINT('Ctrl Pts',(-9.50104767561052,15.3447188656481,
-167.247794117647));
#166239=CARTESIAN_POINT('Ctrl Pts',(-8.07915007496071,16.2251205863895,
-168.741911764706));
#166240=CARTESIAN_POINT('Ctrl Pts',(-6.51968959134574,16.8292587962898,
-170.236029411765));
#166241=CARTESIAN_POINT('Ctrl Pts',(-4.96022910773078,17.4333970061901,
-171.730147058823));
#166242=CARTESIAN_POINT('Ctrl Pts',(-3.31631129755346,17.7406985030951,
-173.224264705882));
#166243=CARTESIAN_POINT('Ctrl Pts',(-1.67239348737615,18.048,-174.718382352941));
#166244=CARTESIAN_POINT('Ctrl Pts',(-2.21024254310115E-15,18.048,-176.2125));
#166245=CARTESIAN_POINT('Ctrl Pts',(1.67239348737616,18.048,-177.706617647059));
#166246=CARTESIAN_POINT('Ctrl Pts',(3.31631129755346,17.7406985030951,-179.200735294118));
#166247=CARTESIAN_POINT('Ctrl Pts',(4.96022910773077,17.4333970061901,-180.694852941176));
#166248=CARTESIAN_POINT('Ctrl Pts',(6.51968959134575,16.8292587962898,-182.188970588235));
#166249=CARTESIAN_POINT('Ctrl Pts',(8.07915007496071,16.2251205863895,-183.683088235294));
#166250=CARTESIAN_POINT('Ctrl Pts',(9.50104767561053,15.3447188656481,-185.177205882353));
#166251=CARTESIAN_POINT('Ctrl Pts',(10.9229452762603,14.4643171449067,-186.671323529412));
#166252=CARTESIAN_POINT('Ctrl Pts',(12.1588589765331,13.3376329379985,-188.165441176471));
#166253=CARTESIAN_POINT('Ctrl Pts',(13.3947726768058,12.2109487310903,-189.659558823529));
#166254=CARTESIAN_POINT('Ctrl Pts',(14.4026149179538,10.8763499173728,-191.153676470588));
#166255=CARTESIAN_POINT('Ctrl Pts',(15.4104571591017,9.54175110365538,-192.647794117647));
#166256=CARTESIAN_POINT('Ctrl Pts',(16.1559070823762,8.04468584505496,-194.141911764706));
#166257=CARTESIAN_POINT('Ctrl Pts',(16.9013570056506,6.54762058645456,-195.636029411765));
#166258=CARTESIAN_POINT('Ctrl Pts',(17.3590292079831,4.93906964482096,-197.130147058824));
#166259=CARTESIAN_POINT('Ctrl Pts',(17.8167014103155,3.33051870318735,-198.624264705882));
#166260=CARTESIAN_POINT('Ctrl Pts',(17.9710104137728,1.66525935159367,-200.118382352941));
#166261=CARTESIAN_POINT('Ctrl Pts',(18.1253194172301,3.32956716117513E-15,
-201.6125));
#166262=CARTESIAN_POINT('Ctrl Pts',(17.9710104137728,-1.66525935159367,
-203.106617647059));
#166263=CARTESIAN_POINT('Ctrl Pts',(17.8167014103155,-3.33051870318736,
-204.600735294118));
#166264=CARTESIAN_POINT('Ctrl Pts',(17.3590292079831,-4.93906964482095,
-206.094852941176));
#166265=CARTESIAN_POINT('Ctrl Pts',(16.9013570056506,-6.54762058645456,
-207.588970588235));
#166266=CARTESIAN_POINT('Ctrl Pts',(16.1559070823762,-8.04468584505497,
-209.083088235294));
#166267=CARTESIAN_POINT('Ctrl Pts',(15.4104571591017,-9.54175110365538,
-210.577205882353));
#166268=CARTESIAN_POINT('Ctrl Pts',(14.4026149179538,-10.8763499173728,
-212.071323529412));
#166269=CARTESIAN_POINT('Ctrl Pts',(13.3947726768058,-12.2109487310903,
-213.56544117647));
#166270=CARTESIAN_POINT('Ctrl Pts',(12.1588589765331,-13.3376329379985,
-215.059558823529));
#166271=CARTESIAN_POINT('Ctrl Pts',(10.9229452762603,-14.4643171449067,
-216.553676470588));
#166272=CARTESIAN_POINT('Ctrl Pts',(9.50104767561053,-15.3447188656481,
-218.047794117647));
#166273=CARTESIAN_POINT('Ctrl Pts',(8.07915007496071,-16.2251205863895,
-219.541911764706));
#166274=CARTESIAN_POINT('Ctrl Pts',(6.51968959134574,-16.8292587962898,
-221.036029411765));
#166275=CARTESIAN_POINT('Ctrl Pts',(4.96022910773078,-17.4333970061901,
-222.530147058823));
#166276=CARTESIAN_POINT('Ctrl Pts',(3.31631129755346,-17.7406985030951,
-224.024264705882));
#166277=CARTESIAN_POINT('Ctrl Pts',(1.67239348737615,-18.048,-225.518382352941));
#166278=CARTESIAN_POINT('Ctrl Pts',(0.,-18.048,-227.0125));
#166279=CARTESIAN_POINT('Ctrl Pts',(-1.67239348737615,-18.048,-228.506617647059));
#166280=CARTESIAN_POINT('Ctrl Pts',(-3.31631129755346,-17.7406985030951,
-230.000735294118));
#166281=CARTESIAN_POINT('Ctrl Pts',(-4.96022910773077,-17.4333970061901,
-231.494852941176));
#166282=CARTESIAN_POINT('Ctrl Pts',(-6.51968959134574,-16.8292587962898,
-232.988970588235));
#166283=CARTESIAN_POINT('Ctrl Pts',(-8.07915007496071,-16.2251205863895,
-234.483088235294));
#166284=CARTESIAN_POINT('Ctrl Pts',(-9.50104767561052,-15.3447188656481,
-235.977205882353));
#166285=CARTESIAN_POINT('Ctrl Pts',(-10.9229452762603,-14.4643171449067,
-237.471323529412));
#166286=CARTESIAN_POINT('Ctrl Pts',(-12.1588589765331,-13.3376329379985,
-238.965441176471));
#166287=CARTESIAN_POINT('Ctrl Pts',(-13.3947726768058,-12.2109487310903,
-240.459558823529));
#166288=CARTESIAN_POINT('Ctrl Pts',(-14.4026149179538,-10.8763499173728,
-241.953676470588));
#166289=CARTESIAN_POINT('Ctrl Pts',(-15.4104571591017,-9.54175110365538,
-243.447794117647));
#166290=CARTESIAN_POINT('Ctrl Pts',(-16.1559070823762,-8.04468584505497,
-244.941911764706));
#166291=CARTESIAN_POINT('Ctrl Pts',(-16.9013570056506,-6.54762058645456,
-246.436029411765));
#166292=CARTESIAN_POINT('Ctrl Pts',(-17.3590292079831,-4.93906964482095,
-247.930147058824));
#166293=CARTESIAN_POINT('Ctrl Pts',(-17.8167014103155,-3.33051870318735,
-249.424264705882));
#166294=CARTESIAN_POINT('Ctrl Pts',(-17.9710104137728,-1.66525935159368,
-250.918382352941));
#166295=CARTESIAN_POINT('Ctrl Pts',(-18.1253194172301,-1.10985572039171E-15,
-252.4125));
#166296=CARTESIAN_POINT('Ctrl Pts',(-17.9710104137728,1.66525935159367,
-253.906617647059));
#166297=CARTESIAN_POINT('Ctrl Pts',(-17.8167014103155,3.33051870318735,
-255.400735294118));
#166298=CARTESIAN_POINT('Ctrl Pts',(-17.3590292079831,4.93906964482096,
-256.894852941177));
#166299=CARTESIAN_POINT('Ctrl Pts',(-16.9013570056506,6.54762058645456,
-258.388970588235));
#166300=CARTESIAN_POINT('Ctrl Pts',(-16.1559070823762,8.04468584505497,
-259.883088235294));
#166301=CARTESIAN_POINT('Ctrl Pts',(-15.4104571591017,9.54175110365538,
-261.377205882353));
#166302=CARTESIAN_POINT('Ctrl Pts',(-14.4026149179538,10.8763499173728,
-262.871323529412));
#166303=CARTESIAN_POINT('Ctrl Pts',(-13.3947726768058,12.2109487310903,
-264.365441176471));
#166304=CARTESIAN_POINT('Ctrl Pts',(-12.1588589765331,13.3376329379985,
-265.859558823529));
#166305=CARTESIAN_POINT('Ctrl Pts',(-10.9229452762603,14.4643171449067,
-267.353676470588));
#166306=CARTESIAN_POINT('Ctrl Pts',(-9.50104767561052,15.3447188656481,
-268.847794117647));
#166307=CARTESIAN_POINT('Ctrl Pts',(-8.07915007496071,16.2251205863895,
-270.341911764706));
#166308=CARTESIAN_POINT('Ctrl Pts',(-6.51968959134574,16.8292587962898,
-271.836029411765));
#166309=CARTESIAN_POINT('Ctrl Pts',(-4.96022910773078,17.4333970061901,
-273.330147058823));
#166310=CARTESIAN_POINT('Ctrl Pts',(-3.31631129755346,17.7406985030951,
-274.824264705882));
#166311=CARTESIAN_POINT('Ctrl Pts',(-1.67239348737615,18.048,-276.318382352941));
#166312=CARTESIAN_POINT('Ctrl Pts',(-2.21024254310115E-15,18.048,-277.8125));
#166313=CARTESIAN_POINT('Ctrl Pts',(1.67239348737616,18.048,-279.306617647059));
#166314=CARTESIAN_POINT('Ctrl Pts',(3.31631129755346,17.7406985030951,-280.800735294118));
#166315=CARTESIAN_POINT('Ctrl Pts',(4.96022910773077,17.4333970061901,-282.294852941176));
#166316=CARTESIAN_POINT('Ctrl Pts',(6.51968959134575,16.8292587962898,-283.788970588235));
#166317=CARTESIAN_POINT('Ctrl Pts',(8.07915007496071,16.2251205863895,-285.283088235294));
#166318=CARTESIAN_POINT('Ctrl Pts',(9.50104767561053,15.3447188656481,-286.777205882353));
#166319=CARTESIAN_POINT('Ctrl Pts',(10.9229452762603,14.4643171449067,-288.271323529412));
#166320=CARTESIAN_POINT('Ctrl Pts',(12.1588589765331,13.3376329379985,-289.765441176471));
#166321=CARTESIAN_POINT('Ctrl Pts',(13.3947726768058,12.2109487310903,-291.259558823529));
#166322=CARTESIAN_POINT('Ctrl Pts',(14.4026149179538,10.8763499173728,-292.753676470588));
#166323=CARTESIAN_POINT('Ctrl Pts',(15.4104571591017,9.54175110365538,-294.247794117647));
#166324=CARTESIAN_POINT('Ctrl Pts',(16.1559070823762,8.04468584505496,-295.741911764706));
#166325=CARTESIAN_POINT('Ctrl Pts',(16.9013570056506,6.54762058645456,-297.236029411765));
#166326=CARTESIAN_POINT('Ctrl Pts',(17.3590292079831,4.93906964482096,-298.730147058823));
#166327=CARTESIAN_POINT('Ctrl Pts',(17.8167014103155,3.33051870318735,-300.224264705882));
#166328=CARTESIAN_POINT('Ctrl Pts',(17.9710104137728,1.66525935159367,-301.718382352941));
#166329=CARTESIAN_POINT('Ctrl Pts',(18.1253194172301,3.32956716117513E-15,
-303.2125));
#166330=CARTESIAN_POINT('Ctrl Pts',(17.9710104137728,-1.66525935159367,
-304.706617647059));
#166331=CARTESIAN_POINT('Ctrl Pts',(17.8167014103155,-3.33051870318736,
-306.200735294118));
#166332=CARTESIAN_POINT('Ctrl Pts',(17.3590292079831,-4.93906964482095,
-307.694852941176));
#166333=CARTESIAN_POINT('Ctrl Pts',(16.9013570056506,-6.54762058645456,
-309.188970588235));
#166334=CARTESIAN_POINT('Ctrl Pts',(16.1559070823762,-8.04468584505497,
-310.683088235294));
#166335=CARTESIAN_POINT('Ctrl Pts',(15.4104571591017,-9.54175110365538,
-312.177205882353));
#166336=CARTESIAN_POINT('Ctrl Pts',(14.4026149179538,-10.8763499173728,
-313.671323529412));
#166337=CARTESIAN_POINT('Ctrl Pts',(13.3947726768058,-12.2109487310903,
-315.165441176471));
#166338=CARTESIAN_POINT('Ctrl Pts',(12.1588589765331,-13.3376329379985,
-316.659558823529));
#166339=CARTESIAN_POINT('Ctrl Pts',(10.9229452762603,-14.4643171449067,
-318.153676470588));
#166340=CARTESIAN_POINT('Ctrl Pts',(9.50104767561053,-15.3447188656481,
-319.647794117647));
#166341=CARTESIAN_POINT('Ctrl Pts',(8.07915007496071,-16.2251205863895,
-321.141911764706));
#166342=CARTESIAN_POINT('Ctrl Pts',(6.51968959134574,-16.8292587962898,
-322.636029411765));
#166343=CARTESIAN_POINT('Ctrl Pts',(4.96022910773078,-17.4333970061901,
-324.130147058824));
#166344=CARTESIAN_POINT('Ctrl Pts',(3.31631129755346,-17.7406985030951,
-325.624264705882));
#166345=CARTESIAN_POINT('Ctrl Pts',(1.67239348737615,-18.048,-327.118382352941));
#166346=CARTESIAN_POINT('Ctrl Pts',(0.,-18.048,-328.6125));
#166347=CARTESIAN_POINT('Ctrl Pts',(-1.67239348737615,-18.048,-330.106617647059));
#166348=CARTESIAN_POINT('Ctrl Pts',(-3.31631129755346,-17.7406985030951,
-331.600735294118));
#166349=CARTESIAN_POINT('Ctrl Pts',(-4.96022910773077,-17.4333970061901,
-333.094852941176));
#166350=CARTESIAN_POINT('Ctrl Pts',(-6.51968959134574,-16.8292587962898,
-334.588970588235));
#166351=CARTESIAN_POINT('Ctrl Pts',(-8.07915007496071,-16.2251205863895,
-336.083088235294));
#166352=CARTESIAN_POINT('Ctrl Pts',(-9.50104767561052,-15.3447188656481,
-337.577205882353));
#166353=CARTESIAN_POINT('Ctrl Pts',(-10.9229452762603,-14.4643171449067,
-339.071323529412));
#166354=CARTESIAN_POINT('Ctrl Pts',(-12.1588589765331,-13.3376329379985,
-340.56544117647));
#166355=CARTESIAN_POINT('Ctrl Pts',(-13.3947726768058,-12.2109487310903,
-342.059558823529));
#166356=CARTESIAN_POINT('Ctrl Pts',(-14.4026149179538,-10.8763499173728,
-343.553676470588));
#166357=CARTESIAN_POINT('Ctrl Pts',(-15.4104571591017,-9.54175110365538,
-345.047794117647));
#166358=CARTESIAN_POINT('Ctrl Pts',(-16.1559070823762,-8.04468584505497,
-346.541911764706));
#166359=CARTESIAN_POINT('Ctrl Pts',(-16.9013570056506,-6.54762058645456,
-348.036029411765));
#166360=CARTESIAN_POINT('Ctrl Pts',(-17.3590292079831,-4.93906964482095,
-349.530147058823));
#166361=CARTESIAN_POINT('Ctrl Pts',(-17.8167014103155,-3.33051870318735,
-351.024264705883));
#166362=CARTESIAN_POINT('Ctrl Pts',(-17.9710104137728,-1.66525935159368,
-352.518382352941));
#166363=CARTESIAN_POINT('Ctrl Pts',(-18.1253194172301,-1.10985572039171E-15,
-354.0125));
#166364=CARTESIAN_POINT('Ctrl Pts',(-17.9710104137728,1.66525935159367,
-355.506617647059));
#166365=CARTESIAN_POINT('Ctrl Pts',(-17.8167014103155,3.33051870318735,
-357.000735294118));
#166366=CARTESIAN_POINT('Ctrl Pts',(-17.3590292079831,4.93906964482096,
-358.494852941176));
#166367=CARTESIAN_POINT('Ctrl Pts',(-16.9013570056506,6.54762058645456,
-359.988970588235));
#166368=CARTESIAN_POINT('Ctrl Pts',(-16.1559070823762,8.04468584505497,
-361.483088235294));
#166369=CARTESIAN_POINT('Ctrl Pts',(-15.4104571591017,9.54175110365538,
-362.977205882353));
#166370=CARTESIAN_POINT('Ctrl Pts',(-14.4026149179538,10.8763499173728,
-364.471323529412));
#166371=CARTESIAN_POINT('Ctrl Pts',(-13.3947726768058,12.2109487310903,
-365.965441176471));
#166372=CARTESIAN_POINT('Ctrl Pts',(-12.1588589765331,13.3376329379985,
-367.459558823529));
#166373=CARTESIAN_POINT('Ctrl Pts',(-10.9229452762603,14.4643171449067,
-368.953676470588));
#166374=CARTESIAN_POINT('Ctrl Pts',(-9.50104767561052,15.3447188656481,
-370.447794117647));
#166375=CARTESIAN_POINT('Ctrl Pts',(-8.07915007496071,16.2251205863895,
-371.941911764706));
#166376=CARTESIAN_POINT('Ctrl Pts',(-6.51968959134574,16.8292587962898,
-373.436029411765));
#166377=CARTESIAN_POINT('Ctrl Pts',(-4.96022910773078,17.4333970061901,
-374.930147058824));
#166378=CARTESIAN_POINT('Ctrl Pts',(-3.31631129755346,17.7406985030951,
-376.424264705882));
#166379=CARTESIAN_POINT('Ctrl Pts',(-1.67239348737615,18.048,-377.918382352941));
#166380=CARTESIAN_POINT('Ctrl Pts',(-2.21024254310115E-15,18.048,-379.4125));
#166381=CARTESIAN_POINT('Ctrl Pts',(1.67239348737616,18.048,-380.906617647059));
#166382=CARTESIAN_POINT('Ctrl Pts',(3.31631129755346,17.7406985030951,-382.400735294118));
#166383=CARTESIAN_POINT('Ctrl Pts',(4.96022910773077,17.4333970061901,-383.894852941177));
#166384=CARTESIAN_POINT('Ctrl Pts',(6.51968959134575,16.8292587962898,-385.388970588235));
#166385=CARTESIAN_POINT('Ctrl Pts',(8.07915007496071,16.2251205863895,-386.883088235294));
#166386=CARTESIAN_POINT('Ctrl Pts',(9.50104767561053,15.3447188656481,-388.377205882353));
#166387=CARTESIAN_POINT('Ctrl Pts',(10.9229452762603,14.4643171449067,-389.871323529412));
#166388=CARTESIAN_POINT('Ctrl Pts',(12.1588589765331,13.3376329379985,-391.365441176471));
#166389=CARTESIAN_POINT('Ctrl Pts',(13.3947726768058,12.2109487310903,-392.859558823529));
#166390=CARTESIAN_POINT('Ctrl Pts',(14.4026149179538,10.8763499173728,-394.353676470588));
#166391=CARTESIAN_POINT('Ctrl Pts',(15.4104571591017,9.54175110365538,-395.847794117647));
#166392=CARTESIAN_POINT('Ctrl Pts',(16.1559070823762,8.04468584505496,-397.341911764706));
#166393=CARTESIAN_POINT('Ctrl Pts',(16.9013570056506,6.54762058645456,-398.836029411765));
#166394=CARTESIAN_POINT('Ctrl Pts',(17.3590292079831,4.93906964482096,-400.330147058823));
#166395=CARTESIAN_POINT('Ctrl Pts',(17.8167014103155,3.33051870318735,-401.824264705882));
#166396=CARTESIAN_POINT('Ctrl Pts',(17.9710104137728,1.66525935159367,-403.318382352941));
#166397=CARTESIAN_POINT('Ctrl Pts',(18.1253194172301,3.32956716117513E-15,
-404.8125));
#166398=CARTESIAN_POINT('Ctrl Pts',(17.9710104137728,-1.66525935159367,
-406.306617647059));
#166399=CARTESIAN_POINT('Ctrl Pts',(17.8167014103155,-3.33051870318736,
-407.800735294118));
#166400=CARTESIAN_POINT('Ctrl Pts',(17.3590292079831,-4.93906964482095,
-409.294852941176));
#166401=CARTESIAN_POINT('Ctrl Pts',(16.9013570056506,-6.54762058645456,
-410.788970588235));
#166402=CARTESIAN_POINT('Ctrl Pts',(16.1559070823762,-8.04468584505497,
-412.283088235294));
#166403=CARTESIAN_POINT('Ctrl Pts',(15.4104571591017,-9.54175110365538,
-413.777205882353));
#166404=CARTESIAN_POINT('Ctrl Pts',(14.4026149179538,-10.8763499173728,
-415.271323529412));
#166405=CARTESIAN_POINT('Ctrl Pts',(13.3947726768058,-12.2109487310903,
-416.765441176471));
#166406=CARTESIAN_POINT('Ctrl Pts',(12.1588589765331,-13.3376329379985,
-418.259558823529));
#166407=CARTESIAN_POINT('Ctrl Pts',(10.9229452762603,-14.4643171449067,
-419.753676470588));
#166408=CARTESIAN_POINT('Ctrl Pts',(9.50104767561053,-15.3447188656481,
-421.247794117647));
#166409=CARTESIAN_POINT('Ctrl Pts',(8.07915007496071,-16.2251205863895,
-422.741911764706));
#166410=CARTESIAN_POINT('Ctrl Pts',(6.51968959134574,-16.8292587962898,
-424.236029411765));
#166411=CARTESIAN_POINT('Ctrl Pts',(4.96022910773078,-17.4333970061901,
-425.730147058824));
#166412=CARTESIAN_POINT('Ctrl Pts',(3.31631129755346,-17.7406985030951,
-427.224264705882));
#166413=CARTESIAN_POINT('Ctrl Pts',(1.67239348737615,-18.048,-428.718382352941));
#166414=CARTESIAN_POINT('Ctrl Pts',(0.,-18.048,-430.2125));
#166415=CARTESIAN_POINT('Ctrl Pts',(-1.67239348737615,-18.048,-431.706617647059));
#166416=CARTESIAN_POINT('Ctrl Pts',(-3.31631129755346,-17.7406985030951,
-433.200735294118));
#166417=CARTESIAN_POINT('Ctrl Pts',(-4.96022910773077,-17.4333970061901,
-434.694852941176));
#166418=CARTESIAN_POINT('Ctrl Pts',(-6.51968959134574,-16.8292587962898,
-436.188970588235));
#166419=CARTESIAN_POINT('Ctrl Pts',(-8.07915007496071,-16.2251205863895,
-437.683088235294));
#166420=CARTESIAN_POINT('Ctrl Pts',(-9.50104767561052,-15.3447188656481,
-439.177205882353));
#166421=CARTESIAN_POINT('Ctrl Pts',(-10.9229452762603,-14.4643171449067,
-440.671323529412));
#166422=CARTESIAN_POINT('Ctrl Pts',(-12.1588589765331,-13.3376329379985,
-442.165441176471));
#166423=CARTESIAN_POINT('Ctrl Pts',(-13.3947726768058,-12.2109487310903,
-443.65955882353));
#166424=CARTESIAN_POINT('Ctrl Pts',(-14.4026149179538,-10.8763499173728,
-445.153676470588));
#166425=CARTESIAN_POINT('Ctrl Pts',(-15.4104571591017,-9.54175110365538,
-446.647794117647));
#166426=CARTESIAN_POINT('Ctrl Pts',(-16.1559070823762,-8.04468584505497,
-448.141911764706));
#166427=CARTESIAN_POINT('Ctrl Pts',(-16.9013570056506,-6.54762058645456,
-449.636029411765));
#166428=CARTESIAN_POINT('Ctrl Pts',(-17.3590292079831,-4.93906964482095,
-451.130147058824));
#166429=CARTESIAN_POINT('Ctrl Pts',(-17.8167014103155,-3.33051870318735,
-452.624264705882));
#166430=CARTESIAN_POINT('Ctrl Pts',(-17.9710104137728,-1.66525935159368,
-454.118382352941));
#166431=CARTESIAN_POINT('Ctrl Pts',(-18.1253194172301,-1.10985572039171E-15,
-455.6125));
#166432=CARTESIAN_POINT('Ctrl Pts',(-17.9710104137728,1.66525935159367,
-457.106617647059));
#166433=CARTESIAN_POINT('Ctrl Pts',(-17.8167014103155,3.33051870318735,
-458.600735294118));
#166434=CARTESIAN_POINT('Ctrl Pts',(-17.3590292079831,4.93906964482096,
-460.094852941176));
#166435=CARTESIAN_POINT('Ctrl Pts',(-16.9013570056506,6.54762058645456,
-461.588970588235));
#166436=CARTESIAN_POINT('Ctrl Pts',(-16.1559070823762,8.04468584505497,
-463.083088235294));
#166437=CARTESIAN_POINT('Ctrl Pts',(-15.4104571591017,9.54175110365538,
-464.577205882353));
#166438=CARTESIAN_POINT('Ctrl Pts',(-14.4026149179538,10.8763499173728,
-466.071323529412));
#166439=CARTESIAN_POINT('Ctrl Pts',(-13.3947726768058,12.2109487310903,
-467.565441176471));
#166440=CARTESIAN_POINT('Ctrl Pts',(-12.1588589765331,13.3376329379985,
-469.059558823529));
#166441=CARTESIAN_POINT('Ctrl Pts',(-10.9229452762603,14.4643171449067,
-470.553676470588));
#166442=CARTESIAN_POINT('Ctrl Pts',(-9.50104767561052,15.3447188656481,
-472.047794117647));
#166443=CARTESIAN_POINT('Ctrl Pts',(-8.07915007496071,16.2251205863895,
-473.541911764706));
#166444=CARTESIAN_POINT('Ctrl Pts',(-6.51968959134574,16.8292587962898,
-475.036029411765));
#166445=CARTESIAN_POINT('Ctrl Pts',(-4.96022910773078,17.4333970061901,
-476.530147058824));
#166446=CARTESIAN_POINT('Ctrl Pts',(-3.31631129755346,17.7406985030951,
-478.024264705882));
#166447=CARTESIAN_POINT('Ctrl Pts',(-1.67239348737615,18.048,-479.518382352941));
#166448=CARTESIAN_POINT('Ctrl Pts',(-2.21024254310115E-15,18.048,-481.0125));
#166449=CARTESIAN_POINT('Ctrl Pts',(1.67239348737616,18.048,-482.506617647059));
#166450=CARTESIAN_POINT('Ctrl Pts',(3.31631129755346,17.7406985030951,-484.000735294118));
#166451=CARTESIAN_POINT('Ctrl Pts',(4.96022910773077,17.4333970061901,-485.494852941177));
#166452=CARTESIAN_POINT('Ctrl Pts',(6.51968959134575,16.8292587962898,-486.988970588235));
#166453=CARTESIAN_POINT('Ctrl Pts',(8.07915007496071,16.2251205863895,-488.483088235294));
#166454=CARTESIAN_POINT('Ctrl Pts',(9.50104767561053,15.3447188656481,-489.977205882353));
#166455=CARTESIAN_POINT('Ctrl Pts',(10.9229452762603,14.4643171449067,-491.471323529412));
#166456=CARTESIAN_POINT('Ctrl Pts',(12.1588589765331,13.3376329379985,-492.965441176471));
#166457=CARTESIAN_POINT('Ctrl Pts',(13.3947726768058,12.2109487310903,-494.45955882353));
#166458=CARTESIAN_POINT('Ctrl Pts',(14.4026149179538,10.8763499173728,-495.953676470588));
#166459=CARTESIAN_POINT('Ctrl Pts',(15.4104571591017,9.54175110365538,-497.447794117647));
#166460=CARTESIAN_POINT('Ctrl Pts',(16.1559070823762,8.04468584505496,-498.941911764706));
#166461=CARTESIAN_POINT('Ctrl Pts',(16.9013570056506,6.54762058645456,-500.436029411765));
#166462=CARTESIAN_POINT('Ctrl Pts',(17.3590292079831,4.93906964482096,-501.930147058824));
#166463=CARTESIAN_POINT('Ctrl Pts',(17.8167014103155,3.33051870318735,-503.424264705883));
#166464=CARTESIAN_POINT('Ctrl Pts',(17.9710104137728,1.66525935159367,-504.918382352941));
#166465=CARTESIAN_POINT('Ctrl Pts',(18.1253194172301,3.32956716117513E-15,
-506.4125));
#166466=CARTESIAN_POINT('Ctrl Pts',(17.9710104137728,-1.66525935159367,
-507.906617647059));
#166467=CARTESIAN_POINT('Ctrl Pts',(17.8167014103155,-3.33051870318736,
-509.400735294117));
#166468=CARTESIAN_POINT('Ctrl Pts',(17.3590292079831,-4.93906964482095,
-510.894852941176));
#166469=CARTESIAN_POINT('Ctrl Pts',(16.9013570056506,-6.54762058645456,
-512.388970588235));
#166470=CARTESIAN_POINT('Ctrl Pts',(16.1559070823762,-8.04468584505497,
-513.883088235294));
#166471=CARTESIAN_POINT('Ctrl Pts',(15.4104571591017,-9.54175110365538,
-515.377205882353));
#166472=CARTESIAN_POINT('Ctrl Pts',(14.4026149179538,-10.8763499173728,
-516.871323529412));
#166473=CARTESIAN_POINT('Ctrl Pts',(13.3947726768058,-12.2109487310903,
-518.365441176471));
#166474=CARTESIAN_POINT('Ctrl Pts',(12.1588589765331,-13.3376329379985,
-519.85955882353));
#166475=CARTESIAN_POINT('Ctrl Pts',(10.9229452762603,-14.4643171449067,
-521.353676470588));
#166476=CARTESIAN_POINT('Ctrl Pts',(9.50104767561053,-15.3447188656481,
-522.847794117647));
#166477=CARTESIAN_POINT('Ctrl Pts',(8.07915007496071,-16.2251205863895,
-524.341911764706));
#166478=CARTESIAN_POINT('Ctrl Pts',(6.51968959134574,-16.8292587962898,
-525.836029411765));
#166479=CARTESIAN_POINT('Ctrl Pts',(4.96022910773078,-17.4333970061901,
-527.330147058823));
#166480=CARTESIAN_POINT('Ctrl Pts',(3.31631129755346,-17.7406985030951,
-528.824264705882));
#166481=CARTESIAN_POINT('Ctrl Pts',(1.67239348737615,-18.048,-530.318382352941));
#166482=CARTESIAN_POINT('Ctrl Pts',(0.,-18.048,-531.8125));
#166483=CARTESIAN_POINT('Ctrl Pts',(-1.67239348737615,-18.048,-533.306617647059));
#166484=CARTESIAN_POINT('Ctrl Pts',(-3.31631129755346,-17.7406985030951,
-534.800735294118));
#166485=CARTESIAN_POINT('Ctrl Pts',(-4.96022910773077,-17.4333970061901,
-536.294852941177));
#166486=CARTESIAN_POINT('Ctrl Pts',(-6.51968959134574,-16.8292587962898,
-537.788970588235));
#166487=CARTESIAN_POINT('Ctrl Pts',(-8.07915007496071,-16.2251205863895,
-539.283088235294));
#166488=CARTESIAN_POINT('Ctrl Pts',(-9.50104767561052,-15.3447188656481,
-540.777205882353));
#166489=CARTESIAN_POINT('Ctrl Pts',(-10.9229452762603,-14.4643171449067,
-542.271323529412));
#166490=CARTESIAN_POINT('Ctrl Pts',(-12.1588589765331,-13.3376329379985,
-543.765441176471));
#166491=CARTESIAN_POINT('Ctrl Pts',(-13.3947726768058,-12.2109487310903,
-545.259558823529));
#166492=CARTESIAN_POINT('Ctrl Pts',(-14.4026149179538,-10.8763499173728,
-546.753676470588));
#166493=CARTESIAN_POINT('Ctrl Pts',(-15.4104571591017,-9.54175110365538,
-548.247794117647));
#166494=CARTESIAN_POINT('Ctrl Pts',(-16.1559070823762,-8.04468584505497,
-549.741911764706));
#166495=CARTESIAN_POINT('Ctrl Pts',(-16.9013570056506,-6.54762058645456,
-551.236029411765));
#166496=CARTESIAN_POINT('Ctrl Pts',(-17.3590292079831,-4.93906964482095,
-552.730147058823));
#166497=CARTESIAN_POINT('Ctrl Pts',(-17.8167014103155,-3.33051870318735,
-554.224264705882));
#166498=CARTESIAN_POINT('Ctrl Pts',(-17.9710104137728,-1.66525935159368,
-555.718382352941));
#166499=CARTESIAN_POINT('Ctrl Pts',(-18.1253194172301,-1.10985572039171E-15,
-557.2125));
#166500=CARTESIAN_POINT('Ctrl Pts',(-17.9710104137728,1.66525935159367,
-558.706617647059));
#166501=CARTESIAN_POINT('Ctrl Pts',(-17.8167014103155,3.33051870318735,
-560.200735294118));
#166502=CARTESIAN_POINT('Ctrl Pts',(-17.3590292079831,4.93906964482096,
-561.694852941176));
#166503=CARTESIAN_POINT('Ctrl Pts',(-16.9013570056506,6.54762058645456,
-563.188970588235));
#166504=CARTESIAN_POINT('Ctrl Pts',(-16.1559070823762,8.04468584505497,
-564.683088235294));
#166505=CARTESIAN_POINT('Ctrl Pts',(-15.4104571591017,9.54175110365538,
-566.177205882353));
#166506=CARTESIAN_POINT('Ctrl Pts',(-14.4026149179538,10.8763499173728,
-567.671323529412));
#166507=CARTESIAN_POINT('Ctrl Pts',(-13.3947726768058,12.2109487310903,
-569.16544117647));
#166508=CARTESIAN_POINT('Ctrl Pts',(-12.1588589765331,13.3376329379985,
-570.659558823529));
#166509=CARTESIAN_POINT('Ctrl Pts',(-10.9229452762603,14.4643171449067,
-572.153676470588));
#166510=CARTESIAN_POINT('Ctrl Pts',(-9.50104767561052,15.3447188656481,
-573.647794117647));
#166511=CARTESIAN_POINT('Ctrl Pts',(-8.07915007496071,16.2251205863895,
-575.141911764706));
#166512=CARTESIAN_POINT('Ctrl Pts',(-6.51968959134574,16.8292587962898,
-576.636029411765));
#166513=CARTESIAN_POINT('Ctrl Pts',(-4.96022910773078,17.4333970061901,
-578.130147058824));
#166514=CARTESIAN_POINT('Ctrl Pts',(-3.31631129755346,17.7406985030951,
-579.624264705882));
#166515=CARTESIAN_POINT('Ctrl Pts',(-1.67239348737615,18.048,-581.118382352941));
#166516=CARTESIAN_POINT('Ctrl Pts',(-2.21024254310115E-15,18.048,-582.6125));
#166517=CARTESIAN_POINT('Ctrl Pts',(1.67239348737616,18.048,-584.106617647059));
#166518=CARTESIAN_POINT('Ctrl Pts',(3.31631129755346,17.7406985030951,-585.600735294117));
#166519=CARTESIAN_POINT('Ctrl Pts',(4.96022910773077,17.4333970061901,-587.094852941176));
#166520=CARTESIAN_POINT('Ctrl Pts',(6.51968959134575,16.8292587962898,-588.588970588235));
#166521=CARTESIAN_POINT('Ctrl Pts',(8.07915007496071,16.2251205863895,-590.083088235294));
#166522=CARTESIAN_POINT('Ctrl Pts',(9.50104767561053,15.3447188656481,-591.577205882353));
#166523=CARTESIAN_POINT('Ctrl Pts',(10.9229452762603,14.4643171449067,-593.071323529412));
#166524=CARTESIAN_POINT('Ctrl Pts',(12.1588589765331,13.3376329379985,-594.565441176471));
#166525=CARTESIAN_POINT('Ctrl Pts',(13.3947726768058,12.2109487310903,-596.05955882353));
#166526=CARTESIAN_POINT('Ctrl Pts',(14.4026149179538,10.8763499173728,-597.553676470588));
#166527=CARTESIAN_POINT('Ctrl Pts',(15.4104571591017,9.54175110365538,-599.047794117647));
#166528=CARTESIAN_POINT('Ctrl Pts',(16.1559070823762,8.04468584505496,-600.541911764706));
#166529=CARTESIAN_POINT('Ctrl Pts',(16.9013570056506,6.54762058645456,-602.036029411765));
#166530=CARTESIAN_POINT('Ctrl Pts',(17.3590292079831,4.93906964482096,-603.530147058823));
#166531=CARTESIAN_POINT('Ctrl Pts',(17.8167014103155,3.33051870318735,-605.024264705882));
#166532=CARTESIAN_POINT('Ctrl Pts',(17.9710104137728,1.66525935159367,-606.518382352941));
#166533=CARTESIAN_POINT('Ctrl Pts',(18.1253194172301,3.32956716117513E-15,
-608.0125));
#166534=CARTESIAN_POINT('Ctrl Pts',(17.9710104137728,-1.66525935159367,
-609.506617647059));
#166535=CARTESIAN_POINT('Ctrl Pts',(17.8167014103155,-3.33051870318736,
-611.000735294118));
#166536=CARTESIAN_POINT('Ctrl Pts',(17.3590292079831,-4.93906964482095,
-612.494852941176));
#166537=CARTESIAN_POINT('Ctrl Pts',(16.9013570056506,-6.54762058645456,
-613.988970588235));
#166538=CARTESIAN_POINT('Ctrl Pts',(16.1559070823762,-8.04468584505497,
-615.483088235294));
#166539=CARTESIAN_POINT('Ctrl Pts',(15.4104571591017,-9.54175110365538,
-616.977205882353));
#166540=CARTESIAN_POINT('Ctrl Pts',(14.4026149179538,-10.8763499173728,
-618.471323529412));
#166541=CARTESIAN_POINT('Ctrl Pts',(13.3947726768058,-12.2109487310903,
-619.96544117647));
#166542=CARTESIAN_POINT('Ctrl Pts',(12.1588589765331,-13.3376329379985,
-621.459558823529));
#166543=CARTESIAN_POINT('Ctrl Pts',(10.9229452762603,-14.4643171449067,
-622.953676470588));
#166544=CARTESIAN_POINT('Ctrl Pts',(9.50104767561053,-15.3447188656481,
-624.447794117647));
#166545=CARTESIAN_POINT('Ctrl Pts',(8.07915007496071,-16.2251205863895,
-625.941911764706));
#166546=CARTESIAN_POINT('Ctrl Pts',(6.51968959134574,-16.8292587962898,
-627.436029411764));
#166547=CARTESIAN_POINT('Ctrl Pts',(4.96022910773078,-17.4333970061901,
-628.930147058823));
#166548=CARTESIAN_POINT('Ctrl Pts',(3.31631129755346,-17.7406985030951,
-630.424264705882));
#166549=CARTESIAN_POINT('Ctrl Pts',(1.67239348737615,-18.048,-631.918382352941));
#166550=CARTESIAN_POINT('Ctrl Pts',(0.,-18.048,-633.4125));
#166551=CARTESIAN_POINT('Ctrl Pts',(-1.67239348737615,-18.048,-634.906617647059));
#166552=CARTESIAN_POINT('Ctrl Pts',(-3.31631129755346,-17.7406985030951,
-636.400735294118));
#166553=CARTESIAN_POINT('Ctrl Pts',(-4.96022910773077,-17.4333970061901,
-637.894852941177));
#166554=CARTESIAN_POINT('Ctrl Pts',(-6.51968959134574,-16.8292587962898,
-639.388970588235));
#166555=CARTESIAN_POINT('Ctrl Pts',(-8.07915007496071,-16.2251205863895,
-640.883088235294));
#166556=CARTESIAN_POINT('Ctrl Pts',(-9.50104767561052,-15.3447188656481,
-642.377205882353));
#166557=CARTESIAN_POINT('Ctrl Pts',(-10.9229452762603,-14.4643171449067,
-643.871323529412));
#166558=CARTESIAN_POINT('Ctrl Pts',(-12.1588589765331,-13.3376329379985,
-645.36544117647));
#166559=CARTESIAN_POINT('Ctrl Pts',(-13.3947726768058,-12.2109487310903,
-646.859558823529));
#166560=CARTESIAN_POINT('Ctrl Pts',(-14.4026149179538,-10.8763499173728,
-648.353676470588));
#166561=CARTESIAN_POINT('Ctrl Pts',(-15.4104571591017,-9.54175110365538,
-649.847794117647));
#166562=CARTESIAN_POINT('Ctrl Pts',(-16.1559070823762,-8.04468584505497,
-651.341911764706));
#166563=CARTESIAN_POINT('Ctrl Pts',(-16.9013570056506,-6.54762058645456,
-652.836029411765));
#166564=CARTESIAN_POINT('Ctrl Pts',(-17.3590292079831,-4.93906964482095,
-654.330147058824));
#166565=CARTESIAN_POINT('Ctrl Pts',(-17.8167014103155,-3.33051870318735,
-655.824264705882));
#166566=CARTESIAN_POINT('Ctrl Pts',(-17.9710104137728,-1.66525935159368,
-657.318382352941));
#166567=CARTESIAN_POINT('Ctrl Pts',(-18.1253194172301,-1.10985572039171E-15,
-658.8125));
#166568=CARTESIAN_POINT('Ctrl Pts',(-17.9710104137728,1.66525935159367,
-660.306617647059));
#166569=CARTESIAN_POINT('Ctrl Pts',(-17.8167014103155,3.33051870318735,
-661.800735294117));
#166570=CARTESIAN_POINT('Ctrl Pts',(-17.3590292079831,4.93906964482096,
-663.294852941176));
#166571=CARTESIAN_POINT('Ctrl Pts',(-16.9013570056506,6.54762058645456,
-664.788970588236));
#166572=CARTESIAN_POINT('Ctrl Pts',(-16.1559070823762,8.04468584505497,
-666.283088235294));
#166573=CARTESIAN_POINT('Ctrl Pts',(-15.4104571591017,9.54175110365538,
-667.777205882353));
#166574=CARTESIAN_POINT('Ctrl Pts',(-14.4026149179538,10.8763499173728,
-669.271323529412));
#166575=CARTESIAN_POINT('Ctrl Pts',(-13.3947726768058,12.2109487310903,
-670.765441176471));
#166576=CARTESIAN_POINT('Ctrl Pts',(-12.1588589765331,13.3376329379985,
-672.259558823529));
#166577=CARTESIAN_POINT('Ctrl Pts',(-10.9229452762603,14.4643171449067,
-673.753676470588));
#166578=CARTESIAN_POINT('Ctrl Pts',(-9.50104767561052,15.3447188656481,
-675.247794117647));
#166579=CARTESIAN_POINT('Ctrl Pts',(-8.07915007496071,16.2251205863895,
-676.741911764706));
#166580=CARTESIAN_POINT('Ctrl Pts',(-6.51968959134574,16.8292587962898,
-678.236029411765));
#166581=CARTESIAN_POINT('Ctrl Pts',(-4.96022910773078,17.4333970061901,
-679.730147058824));
#166582=CARTESIAN_POINT('Ctrl Pts',(-3.31631129755346,17.7406985030951,
-681.224264705883));
#166583=CARTESIAN_POINT('Ctrl Pts',(-1.67239348737615,18.048,-682.718382352941));
#166584=CARTESIAN_POINT('Ctrl Pts',(-2.21024254310115E-15,18.048,-684.2125));
#166585=CARTESIAN_POINT('Ctrl Pts',(1.67239348737616,18.048,-685.706617647059));
#166586=CARTESIAN_POINT('Ctrl Pts',(3.31631129755346,17.7406985030951,-687.200735294118));
#166587=CARTESIAN_POINT('Ctrl Pts',(4.96022910773077,17.4333970061901,-688.694852941176));
#166588=CARTESIAN_POINT('Ctrl Pts',(6.51968959134575,16.8292587962898,-690.188970588235));
#166589=CARTESIAN_POINT('Ctrl Pts',(8.07915007496071,16.2251205863895,-691.683088235294));
#166590=CARTESIAN_POINT('Ctrl Pts',(9.50104767561053,15.3447188656481,-693.177205882353));
#166591=CARTESIAN_POINT('Ctrl Pts',(10.9229452762603,14.4643171449067,-694.671323529412));
#166592=CARTESIAN_POINT('Ctrl Pts',(12.1588589765331,13.3376329379985,-696.165441176471));
#166593=CARTESIAN_POINT('Ctrl Pts',(13.3947726768058,12.2109487310903,-697.659558823529));
#166594=CARTESIAN_POINT('Ctrl Pts',(14.4026149179538,10.8763499173728,-699.153676470588));
#166595=CARTESIAN_POINT('Ctrl Pts',(15.4104571591017,9.54175110365538,-700.647794117647));
#166596=CARTESIAN_POINT('Ctrl Pts',(16.1559070823762,8.04468584505496,-702.141911764706));
#166597=CARTESIAN_POINT('Ctrl Pts',(16.9013570056506,6.54762058645456,-703.636029411765));
#166598=CARTESIAN_POINT('Ctrl Pts',(17.3590292079831,4.93906964482096,-705.130147058823));
#166599=CARTESIAN_POINT('Ctrl Pts',(17.8167014103155,3.33051870318735,-706.624264705882));
#166600=CARTESIAN_POINT('Ctrl Pts',(17.9710104137728,1.66525935159367,-708.118382352941));
#166601=CARTESIAN_POINT('Ctrl Pts',(18.1253194172301,3.32956716117513E-15,
-709.6125));
#166602=CARTESIAN_POINT('Ctrl Pts',(17.9710104137728,-1.66525935159367,
-711.106617647059));
#166603=CARTESIAN_POINT('Ctrl Pts',(17.8167014103155,-3.33051870318736,
-712.600735294118));
#166604=CARTESIAN_POINT('Ctrl Pts',(17.3590292079831,-4.93906964482095,
-714.094852941177));
#166605=CARTESIAN_POINT('Ctrl Pts',(16.9013570056506,-6.54762058645456,
-715.588970588235));
#166606=CARTESIAN_POINT('Ctrl Pts',(16.1559070823762,-8.04468584505497,
-717.083088235294));
#166607=CARTESIAN_POINT('Ctrl Pts',(15.4104571591017,-9.54175110365538,
-718.577205882353));
#166608=CARTESIAN_POINT('Ctrl Pts',(14.4026149179538,-10.8763499173728,
-720.071323529412));
#166609=CARTESIAN_POINT('Ctrl Pts',(13.3947726768058,-12.2109487310903,
-721.56544117647));
#166610=CARTESIAN_POINT('Ctrl Pts',(12.1588589765331,-13.3376329379985,
-723.059558823529));
#166611=CARTESIAN_POINT('Ctrl Pts',(10.9229452762603,-14.4643171449067,
-724.553676470588));
#166612=CARTESIAN_POINT('Ctrl Pts',(9.50104767561053,-15.3447188656481,
-726.047794117647));
#166613=CARTESIAN_POINT('Ctrl Pts',(8.07915007496071,-16.2251205863895,
-727.541911764706));
#166614=CARTESIAN_POINT('Ctrl Pts',(6.51968959134574,-16.8292587962898,
-729.036029411765));
#166615=CARTESIAN_POINT('Ctrl Pts',(4.96022910773078,-17.4333970061901,
-730.530147058824));
#166616=CARTESIAN_POINT('Ctrl Pts',(3.31631129755346,-17.7406985030951,
-732.024264705882));
#166617=CARTESIAN_POINT('Ctrl Pts',(1.67239348737615,-18.048,-733.518382352941));
#166618=CARTESIAN_POINT('Ctrl Pts',(0.,-18.048,-735.0125));
#166619=CARTESIAN_POINT('Ctrl Pts',(-1.67239348737615,-18.048,-736.506617647059));
#166620=CARTESIAN_POINT('Ctrl Pts',(-3.31631129755346,-17.7406985030951,
-738.000735294118));
#166621=CARTESIAN_POINT('Ctrl Pts',(-4.96022910773077,-17.4333970061901,
-739.494852941177));
#166622=CARTESIAN_POINT('Ctrl Pts',(-6.51968959134574,-16.8292587962898,
-740.988970588235));
#166623=CARTESIAN_POINT('Ctrl Pts',(-8.07915007496071,-16.2251205863895,
-742.483088235294));
#166624=CARTESIAN_POINT('Ctrl Pts',(-9.50104767561052,-15.3447188656481,
-743.977205882353));
#166625=CARTESIAN_POINT('Ctrl Pts',(-10.9229452762603,-14.4643171449067,
-745.471323529412));
#166626=CARTESIAN_POINT('Ctrl Pts',(-12.1588589765331,-13.3376329379985,
-746.96544117647));
#166627=CARTESIAN_POINT('Ctrl Pts',(-13.3947726768058,-12.2109487310903,
-748.459558823529));
#166628=CARTESIAN_POINT('Ctrl Pts',(-14.4026149179538,-10.8763499173728,
-749.953676470588));
#166629=CARTESIAN_POINT('Ctrl Pts',(-15.4104571591017,-9.54175110365538,
-751.447794117647));
#166630=CARTESIAN_POINT('Ctrl Pts',(-16.1559070823762,-8.04468584505497,
-752.941911764706));
#166631=CARTESIAN_POINT('Ctrl Pts',(-16.9013570056506,-6.54762058645456,
-754.436029411765));
#166632=CARTESIAN_POINT('Ctrl Pts',(-17.3590292079831,-4.93906964482095,
-755.930147058824));
#166633=CARTESIAN_POINT('Ctrl Pts',(-17.8167014103155,-3.33051870318735,
-757.424264705882));
#166634=CARTESIAN_POINT('Ctrl Pts',(-17.9710104137728,-1.66525935159368,
-758.918382352941));
#166635=CARTESIAN_POINT('Ctrl Pts',(-18.1253194172301,-1.10985572039171E-15,
-760.4125));
#166636=CARTESIAN_POINT('Ctrl Pts',(-17.9710104137728,1.66525935159367,
-761.906617647059));
#166637=CARTESIAN_POINT('Ctrl Pts',(-17.8167014103155,3.33051870318735,
-763.400735294118));
#166638=CARTESIAN_POINT('Ctrl Pts',(-17.3590292079831,4.93906964482096,
-764.894852941176));
#166639=CARTESIAN_POINT('Ctrl Pts',(-16.9013570056506,6.54762058645456,
-766.388970588235));
#166640=CARTESIAN_POINT('Ctrl Pts',(-16.1559070823762,8.04468584505497,
-767.883088235294));
#166641=CARTESIAN_POINT('Ctrl Pts',(-15.4104571591017,9.54175110365538,
-769.377205882353));
#166642=CARTESIAN_POINT('Ctrl Pts',(-14.4026149179538,10.8763499173728,
-770.871323529412));
#166643=CARTESIAN_POINT('Ctrl Pts',(-13.3947726768058,12.2109487310903,
-772.365441176471));
#166644=CARTESIAN_POINT('Ctrl Pts',(-12.1588589765331,13.3376329379985,
-773.85955882353));
#166645=CARTESIAN_POINT('Ctrl Pts',(-10.9229452762603,14.4643171449067,
-775.353676470589));
#166646=CARTESIAN_POINT('Ctrl Pts',(-9.50104767561052,15.3447188656481,
-776.847794117647));
#166647=CARTESIAN_POINT('Ctrl Pts',(-8.07915007496071,16.2251205863895,
-778.341911764706));
#166648=CARTESIAN_POINT('Ctrl Pts',(-6.51968959134574,16.8292587962898,
-779.836029411765));
#166649=CARTESIAN_POINT('Ctrl Pts',(-4.96022910773078,17.4333970061901,
-781.330147058823));
#166650=CARTESIAN_POINT('Ctrl Pts',(-3.31631129755346,17.7406985030951,
-782.824264705882));
#166651=CARTESIAN_POINT('Ctrl Pts',(-1.67239348737615,18.048,-784.318382352941));
#166652=CARTESIAN_POINT('Ctrl Pts',(-2.21024254310115E-15,18.048,-785.8125));
#166653=CARTESIAN_POINT('Ctrl Pts',(1.67239348737616,18.048,-787.306617647059));
#166654=CARTESIAN_POINT('Ctrl Pts',(3.31631129755346,17.7406985030951,-788.800735294118));
#166655=CARTESIAN_POINT('Ctrl Pts',(4.96022910773077,17.4333970061901,-790.294852941177));
#166656=CARTESIAN_POINT('Ctrl Pts',(6.51968959134575,16.8292587962898,-791.788970588235));
#166657=CARTESIAN_POINT('Ctrl Pts',(8.07915007496071,16.2251205863895,-793.283088235294));
#166658=CARTESIAN_POINT('Ctrl Pts',(9.50104767561053,15.3447188656481,-794.777205882353));
#166659=CARTESIAN_POINT('Ctrl Pts',(10.9229452762603,14.4643171449067,-796.271323529412));
#166660=CARTESIAN_POINT('Ctrl Pts',(12.1588589765331,13.3376329379985,-797.765441176471));
#166661=CARTESIAN_POINT('Ctrl Pts',(13.3947726768058,12.2109487310903,-799.259558823529));
#166662=CARTESIAN_POINT('Ctrl Pts',(14.4026149179538,10.8763499173728,-800.753676470588));
#166663=CARTESIAN_POINT('Ctrl Pts',(15.4104571591017,9.54175110365538,-802.247794117647));
#166664=CARTESIAN_POINT('Ctrl Pts',(16.1559070823762,8.04468584505496,-803.741911764706));
#166665=CARTESIAN_POINT('Ctrl Pts',(16.9013570056506,6.54762058645456,-805.236029411765));
#166666=CARTESIAN_POINT('Ctrl Pts',(17.3590292079831,4.93906964482096,-806.730147058823));
#166667=CARTESIAN_POINT('Ctrl Pts',(17.8167014103155,3.33051870318735,-808.224264705882));
#166668=CARTESIAN_POINT('Ctrl Pts',(17.9710104137728,1.66525935159367,-809.718382352941));
#166669=CARTESIAN_POINT('Ctrl Pts',(18.1253194172301,3.32956716117513E-15,
-811.2125));
#166670=CARTESIAN_POINT('Ctrl Pts',(17.9710104137728,-1.66525935159367,
-812.706617647059));
#166671=CARTESIAN_POINT('Ctrl Pts',(17.8167014103155,-3.33051870318736,
-814.200735294118));
#166672=CARTESIAN_POINT('Ctrl Pts',(17.3590292079831,-4.93906964482095,
-815.694852941177));
#166673=CARTESIAN_POINT('Ctrl Pts',(16.9013570056506,-6.54762058645456,
-817.188970588235));
#166674=CARTESIAN_POINT('Ctrl Pts',(16.1559070823762,-8.04468584505497,
-818.683088235294));
#166675=CARTESIAN_POINT('Ctrl Pts',(15.4104571591017,-9.54175110365538,
-820.177205882353));
#166676=CARTESIAN_POINT('Ctrl Pts',(14.4026149179538,-10.8763499173728,
-821.671323529412));
#166677=CARTESIAN_POINT('Ctrl Pts',(13.3947726768058,-12.2109487310903,
-823.16544117647));
#166678=CARTESIAN_POINT('Ctrl Pts',(12.1588589765331,-13.3376329379985,
-824.659558823529));
#166679=CARTESIAN_POINT('Ctrl Pts',(10.9229452762603,-14.4643171449067,
-826.153676470588));
#166680=CARTESIAN_POINT('Ctrl Pts',(9.50104767561053,-15.3447188656481,
-827.647794117647));
#166681=CARTESIAN_POINT('Ctrl Pts',(8.07915007496071,-16.2251205863895,
-829.141911764706));
#166682=CARTESIAN_POINT('Ctrl Pts',(6.51968959134574,-16.8292587962898,
-830.636029411765));
#166683=CARTESIAN_POINT('Ctrl Pts',(4.96022910773078,-17.4333970061901,
-832.130147058824));
#166684=CARTESIAN_POINT('Ctrl Pts',(3.31631129755346,-17.7406985030951,
-833.624264705883));
#166685=CARTESIAN_POINT('Ctrl Pts',(1.67239348737615,-18.048,-835.118382352941));
#166686=CARTESIAN_POINT('Ctrl Pts',(0.,-18.048,-836.6125));
#166687=CARTESIAN_POINT('Ctrl Pts',(-1.67239348737615,-18.048,-838.106617647059));
#166688=CARTESIAN_POINT('Ctrl Pts',(-3.31631129755346,-17.7406985030951,
-839.600735294118));
#166689=CARTESIAN_POINT('Ctrl Pts',(-4.96022910773077,-17.4333970061901,
-841.094852941176));
#166690=CARTESIAN_POINT('Ctrl Pts',(-6.51968959134574,-16.8292587962898,
-842.588970588235));
#166691=CARTESIAN_POINT('Ctrl Pts',(-8.07915007496071,-16.2251205863895,
-844.083088235294));
#166692=CARTESIAN_POINT('Ctrl Pts',(-9.50104767561052,-15.3447188656481,
-845.577205882353));
#166693=CARTESIAN_POINT('Ctrl Pts',(-10.9229452762603,-14.4643171449067,
-847.071323529412));
#166694=CARTESIAN_POINT('Ctrl Pts',(-12.1588589765331,-13.3376329379985,
-848.565441176471));
#166695=CARTESIAN_POINT('Ctrl Pts',(-13.3947726768058,-12.2109487310903,
-850.05955882353));
#166696=CARTESIAN_POINT('Ctrl Pts',(-14.4026149179538,-10.8763499173728,
-851.553676470588));
#166697=CARTESIAN_POINT('Ctrl Pts',(-15.4104571591017,-9.54175110365538,
-853.047794117647));
#166698=CARTESIAN_POINT('Ctrl Pts',(-16.1559070823762,-8.04468584505497,
-854.541911764706));
#166699=CARTESIAN_POINT('Ctrl Pts',(-16.9013570056506,-6.54762058645456,
-856.036029411765));
#166700=CARTESIAN_POINT('Ctrl Pts',(-17.3590292079831,-4.93906964482095,
-857.530147058824));
#166701=CARTESIAN_POINT('Ctrl Pts',(-17.8167014103155,-3.33051870318735,
-859.024264705882));
#166702=CARTESIAN_POINT('Ctrl Pts',(-17.9710104137728,-1.66525935159368,
-860.518382352941));
#166703=CARTESIAN_POINT('Ctrl Pts',(-18.1253194172301,-1.10985572039171E-15,
-862.0125));
#166704=CARTESIAN_POINT('Ctrl Pts',(-17.9710104137728,1.66525935159367,
-863.506617647059));
#166705=CARTESIAN_POINT('Ctrl Pts',(-17.8167014103155,3.33051870318735,
-865.000735294118));
#166706=CARTESIAN_POINT('Ctrl Pts',(-17.3590292079831,4.93906964482096,
-866.494852941176));
#166707=CARTESIAN_POINT('Ctrl Pts',(-16.9013570056506,6.54762058645456,
-867.988970588235));
#166708=CARTESIAN_POINT('Ctrl Pts',(-16.1559070823762,8.04468584505497,
-869.483088235294));
#166709=CARTESIAN_POINT('Ctrl Pts',(-15.4104571591017,9.54175110365538,
-870.977205882353));
#166710=CARTESIAN_POINT('Ctrl Pts',(-14.4026149179538,10.8763499173728,
-872.471323529412));
#166711=CARTESIAN_POINT('Ctrl Pts',(-13.3947726768058,12.2109487310903,
-873.965441176471));
#166712=CARTESIAN_POINT('Ctrl Pts',(-12.1588589765331,13.3376329379985,
-875.459558823529));
#166713=CARTESIAN_POINT('Ctrl Pts',(-10.9229452762603,14.4643171449067,
-876.953676470588));
#166714=CARTESIAN_POINT('Ctrl Pts',(-9.50104767561052,15.3447188656481,
-878.447794117647));
#166715=CARTESIAN_POINT('Ctrl Pts',(-8.07915007496071,16.2251205863895,
-879.941911764706));
#166716=CARTESIAN_POINT('Ctrl Pts',(-6.51968959134574,16.8292587962898,
-881.436029411765));
#166717=CARTESIAN_POINT('Ctrl Pts',(-4.96022910773078,17.4333970061901,
-882.930147058823));
#166718=CARTESIAN_POINT('Ctrl Pts',(-3.31631129755346,17.7406985030951,
-884.424264705882));
#166719=CARTESIAN_POINT('Ctrl Pts',(-1.67239348737615,18.048,-885.918382352941));
#166720=CARTESIAN_POINT('Ctrl Pts',(-2.21024254310115E-15,18.048,-887.4125));
#166721=CARTESIAN_POINT('Ctrl Pts',(1.67239348737616,18.048,-888.906617647059));
#166722=CARTESIAN_POINT('Ctrl Pts',(3.31631129755346,17.7406985030951,-890.400735294118));
#166723=CARTESIAN_POINT('Ctrl Pts',(4.96022910773077,17.4333970061901,-891.894852941177));
#166724=CARTESIAN_POINT('Ctrl Pts',(6.51968959134575,16.8292587962898,-893.388970588235));
#166725=CARTESIAN_POINT('Ctrl Pts',(8.07915007496071,16.2251205863895,-894.883088235295));
#166726=CARTESIAN_POINT('Ctrl Pts',(9.50104767561053,15.3447188656481,-896.377205882353));
#166727=CARTESIAN_POINT('Ctrl Pts',(10.9229452762603,14.4643171449067,-897.871323529412));
#166728=CARTESIAN_POINT('Ctrl Pts',(12.1588589765331,13.3376329379985,-899.36544117647));
#166729=CARTESIAN_POINT('Ctrl Pts',(13.3947726768058,12.2109487310903,-900.859558823529));
#166730=CARTESIAN_POINT('Ctrl Pts',(14.4026149179538,10.8763499173728,-902.353676470588));
#166731=CARTESIAN_POINT('Ctrl Pts',(15.4104571591017,9.54175110365538,-903.847794117647));
#166732=CARTESIAN_POINT('Ctrl Pts',(16.1559070823762,8.04468584505496,-905.341911764706));
#166733=CARTESIAN_POINT('Ctrl Pts',(16.9013570056506,6.54762058645456,-906.836029411765));
#166734=CARTESIAN_POINT('Ctrl Pts',(17.3590292079831,4.93906964482096,-908.330147058824));
#166735=CARTESIAN_POINT('Ctrl Pts',(17.8167014103155,3.33051870318735,-909.824264705883));
#166736=CARTESIAN_POINT('Ctrl Pts',(17.9710104137728,1.66525935159367,-911.318382352941));
#166737=CARTESIAN_POINT('Ctrl Pts',(18.1253194172301,3.32956716117513E-15,
-912.8125));
#166738=CARTESIAN_POINT('Ctrl Pts',(17.9710104137728,-1.66525935159367,
-914.306617647059));
#166739=CARTESIAN_POINT('Ctrl Pts',(17.8167014103155,-3.33051870318736,
-915.800735294118));
#166740=CARTESIAN_POINT('Ctrl Pts',(17.3590292079831,-4.93906964482095,
-917.294852941176));
#166741=CARTESIAN_POINT('Ctrl Pts',(16.9013570056506,-6.54762058645456,
-918.788970588235));
#166742=CARTESIAN_POINT('Ctrl Pts',(16.1559070823762,-8.04468584505497,
-920.283088235294));
#166743=CARTESIAN_POINT('Ctrl Pts',(15.4104571591017,-9.54175110365538,
-921.777205882353));
#166744=CARTESIAN_POINT('Ctrl Pts',(14.4026149179538,-10.8763499173728,
-923.271323529412));
#166745=CARTESIAN_POINT('Ctrl Pts',(13.3947726768058,-12.2109487310903,
-924.765441176471));
#166746=CARTESIAN_POINT('Ctrl Pts',(12.1588589765331,-13.3376329379985,
-926.259558823529));
#166747=CARTESIAN_POINT('Ctrl Pts',(10.9229452762603,-14.4643171449067,
-927.753676470588));
#166748=CARTESIAN_POINT('Ctrl Pts',(9.50104767561053,-15.3447188656481,
-929.247794117647));
#166749=CARTESIAN_POINT('Ctrl Pts',(8.07915007496071,-16.2251205863895,
-930.741911764706));
#166750=CARTESIAN_POINT('Ctrl Pts',(6.51968959134574,-16.8292587962898,
-932.236029411765));
#166751=CARTESIAN_POINT('Ctrl Pts',(4.96022910773078,-17.4333970061901,
-933.730147058824));
#166752=CARTESIAN_POINT('Ctrl Pts',(3.31631129755346,-17.7406985030951,
-935.224264705882));
#166753=CARTESIAN_POINT('Ctrl Pts',(1.67239348737615,-18.048,-936.718382352941));
#166754=CARTESIAN_POINT('Ctrl Pts',(0.,-18.048,-938.2125));
#166755=CARTESIAN_POINT('Ctrl Pts',(-1.67239348737615,-18.048,-939.706617647059));
#166756=CARTESIAN_POINT('Ctrl Pts',(-3.31631129755346,-17.7406985030951,
-941.200735294117));
#166757=CARTESIAN_POINT('Ctrl Pts',(-4.96022910773077,-17.4333970061901,
-942.694852941176));
#166758=CARTESIAN_POINT('Ctrl Pts',(-6.51968959134574,-16.8292587962898,
-944.188970588235));
#166759=CARTESIAN_POINT('Ctrl Pts',(-8.07915007496071,-16.2251205863895,
-945.683088235294));
#166760=CARTESIAN_POINT('Ctrl Pts',(-9.50104767561052,-15.3447188656481,
-947.177205882353));
#166761=CARTESIAN_POINT('Ctrl Pts',(-10.9229452762603,-14.4643171449067,
-948.671323529412));
#166762=CARTESIAN_POINT('Ctrl Pts',(-12.1588589765331,-13.3376329379985,
-950.165441176471));
#166763=CARTESIAN_POINT('Ctrl Pts',(-13.3947726768058,-12.2109487310903,
-951.65955882353));
#166764=CARTESIAN_POINT('Ctrl Pts',(-14.4026149179538,-10.8763499173728,
-953.153676470588));
#166765=CARTESIAN_POINT('Ctrl Pts',(-15.4104571591017,-9.54175110365538,
-954.647794117647));
#166766=CARTESIAN_POINT('Ctrl Pts',(-16.1559070823762,-8.04468584505497,
-956.141911764706));
#166767=CARTESIAN_POINT('Ctrl Pts',(-16.9013570056506,-6.54762058645456,
-957.636029411764));
#166768=CARTESIAN_POINT('Ctrl Pts',(-17.3590292079831,-4.93906964482095,
-959.130147058823));
#166769=CARTESIAN_POINT('Ctrl Pts',(-17.8167014103155,-3.33051870318735,
-960.624264705882));
#166770=CARTESIAN_POINT('Ctrl Pts',(-17.9710104137728,-1.66525935159368,
-962.118382352941));
#166771=CARTESIAN_POINT('Ctrl Pts',(-18.1253194172301,-1.10985572039171E-15,
-963.6125));
#166772=CARTESIAN_POINT('Ctrl Pts',(-17.9710104137728,1.66525935159367,
-965.106617647059));
#166773=CARTESIAN_POINT('Ctrl Pts',(-17.8167014103155,3.33051870318735,
-966.600735294118));
#166774=CARTESIAN_POINT('Ctrl Pts',(-17.3590292079831,4.93906964482096,
-968.094852941177));
#166775=CARTESIAN_POINT('Ctrl Pts',(-16.9013570056506,6.54762058645456,
-969.588970588235));
#166776=CARTESIAN_POINT('Ctrl Pts',(-16.1559070823762,8.04468584505497,
-971.083088235294));
#166777=CARTESIAN_POINT('Ctrl Pts',(-15.4104571591017,9.54175110365538,
-972.577205882353));
#166778=CARTESIAN_POINT('Ctrl Pts',(-14.4026149179538,10.8763499173728,
-974.071323529412));
#166779=CARTESIAN_POINT('Ctrl Pts',(-13.3947726768058,12.2109487310903,
-975.565441176471));
#166780=CARTESIAN_POINT('Ctrl Pts',(-12.1588589765331,13.3376329379985,
-977.059558823529));
#166781=CARTESIAN_POINT('Ctrl Pts',(-10.9229452762603,14.4643171449067,
-978.553676470588));
#166782=CARTESIAN_POINT('Ctrl Pts',(-9.50104767561052,15.3447188656481,
-980.047794117647));
#166783=CARTESIAN_POINT('Ctrl Pts',(-8.07915007496071,16.2251205863895,
-981.541911764706));
#166784=CARTESIAN_POINT('Ctrl Pts',(-6.51968959134574,16.8292587962898,
-983.036029411765));
#166785=CARTESIAN_POINT('Ctrl Pts',(-4.96022910773078,17.4333970061901,
-984.530147058824));
#166786=CARTESIAN_POINT('Ctrl Pts',(-3.31631129755346,17.7406985030951,
-986.024264705882));
#166787=CARTESIAN_POINT('Ctrl Pts',(-1.67239348737615,18.048,-987.518382352941));
#166788=CARTESIAN_POINT('Ctrl Pts',(-2.21024254310115E-15,18.048,-989.0125));
#166789=CARTESIAN_POINT('Ctrl Pts',(1.67239348737616,18.048,-990.506617647059));
#166790=CARTESIAN_POINT('Ctrl Pts',(3.31631129755346,17.7406985030951,-992.000735294118));
#166791=CARTESIAN_POINT('Ctrl Pts',(4.96022910773077,17.4333970061901,-993.494852941176));
#166792=CARTESIAN_POINT('Ctrl Pts',(6.51968959134575,16.8292587962898,-994.988970588235));
#166793=CARTESIAN_POINT('Ctrl Pts',(8.07915007496071,16.2251205863895,-996.483088235294));
#166794=CARTESIAN_POINT('Ctrl Pts',(9.50104767561053,15.3447188656481,-997.977205882353));
#166795=CARTESIAN_POINT('Ctrl Pts',(10.9229452762603,14.4643171449067,-999.471323529412));
#166796=CARTESIAN_POINT('Ctrl Pts',(12.1588589765331,13.3376329379985,-1000.96544117647));
#166797=CARTESIAN_POINT('Ctrl Pts',(13.3947726768058,12.2109487310903,-1002.45955882353));
#166798=CARTESIAN_POINT('Ctrl Pts',(14.4026149179538,10.8763499173728,-1003.95367647059));
#166799=CARTESIAN_POINT('Ctrl Pts',(15.4104571591017,9.54175110365538,-1005.44779411765));
#166800=CARTESIAN_POINT('Ctrl Pts',(16.1559070823762,8.04468584505496,-1006.94191176471));
#166801=CARTESIAN_POINT('Ctrl Pts',(16.9013570056506,6.54762058645456,-1008.43602941176));
#166802=CARTESIAN_POINT('Ctrl Pts',(17.3590292079831,4.93906964482096,-1009.93014705882));
#166803=CARTESIAN_POINT('Ctrl Pts',(17.8167014103155,3.33051870318735,-1011.42426470588));
#166804=CARTESIAN_POINT('Ctrl Pts',(17.9710104137728,1.66525935159367,-1012.91838235294));
#166805=CARTESIAN_POINT('Ctrl Pts',(18.1253194172301,3.32956716117513E-15,
-1014.4125));
#166806=CARTESIAN_POINT('Ctrl Pts',(17.9710104137728,-1.66525935159367,
-1015.90661764706));
#166807=CARTESIAN_POINT('Ctrl Pts',(17.8167014103155,-3.33051870318736,
-1017.40073529412));
#166808=CARTESIAN_POINT('Ctrl Pts',(17.3590292079831,-4.93906964482095,
-1018.89485294118));
#166809=CARTESIAN_POINT('Ctrl Pts',(16.9013570056506,-6.54762058645456,
-1020.38897058824));
#166810=CARTESIAN_POINT('Ctrl Pts',(16.1559070823762,-8.04468584505497,
-1021.88308823529));
#166811=CARTESIAN_POINT('Ctrl Pts',(15.4104571591017,-9.54175110365538,
-1023.37720588235));
#166812=CARTESIAN_POINT('Ctrl Pts',(14.4026149179538,-10.8763499173728,
-1024.87132352941));
#166813=CARTESIAN_POINT('Ctrl Pts',(13.3947726768058,-12.2109487310903,
-1026.36544117647));
#166814=CARTESIAN_POINT('Ctrl Pts',(12.1588589765331,-13.3376329379985,
-1027.85955882353));
#166815=CARTESIAN_POINT('Ctrl Pts',(10.9229452762603,-14.4643171449067,
-1029.35367647059));
#166816=CARTESIAN_POINT('Ctrl Pts',(9.50104767561053,-15.3447188656481,
-1030.84779411765));
#166817=CARTESIAN_POINT('Ctrl Pts',(8.07915007496071,-16.2251205863895,
-1032.34191176471));
#166818=CARTESIAN_POINT('Ctrl Pts',(6.51968959134574,-16.8292587962898,
-1033.83602941176));
#166819=CARTESIAN_POINT('Ctrl Pts',(4.96022910773078,-17.4333970061901,
-1035.33014705882));
#166820=CARTESIAN_POINT('Ctrl Pts',(3.31631129755346,-17.7406985030951,
-1036.82426470588));
#166821=CARTESIAN_POINT('Ctrl Pts',(1.67239348737615,-18.048,-1038.31838235294));
#166822=CARTESIAN_POINT('Ctrl Pts',(0.,-18.048,-1039.8125));
#166823=CARTESIAN_POINT('Ctrl Pts',(-1.67239348737615,-18.048,-1041.30661764706));
#166824=CARTESIAN_POINT('Ctrl Pts',(-3.31631129755346,-17.7406985030951,
-1042.80073529412));
#166825=CARTESIAN_POINT('Ctrl Pts',(-4.96022910773077,-17.4333970061901,
-1044.29485294118));
#166826=CARTESIAN_POINT('Ctrl Pts',(-6.51968959134574,-16.8292587962898,
-1045.78897058824));
#166827=CARTESIAN_POINT('Ctrl Pts',(-8.07915007496071,-16.2251205863895,
-1047.28308823529));
#166828=CARTESIAN_POINT('Ctrl Pts',(-9.50104767561052,-15.3447188656481,
-1048.77720588235));
#166829=CARTESIAN_POINT('Ctrl Pts',(-10.9229452762603,-14.4643171449067,
-1050.27132352941));
#166830=CARTESIAN_POINT('Ctrl Pts',(-12.1588589765331,-13.3376329379985,
-1051.76544117647));
#166831=CARTESIAN_POINT('Ctrl Pts',(-13.3947726768058,-12.2109487310903,
-1053.25955882353));
#166832=CARTESIAN_POINT('Ctrl Pts',(-14.4026149179538,-10.8763499173728,
-1054.75367647059));
#166833=CARTESIAN_POINT('Ctrl Pts',(-15.4104571591017,-9.54175110365538,
-1056.24779411765));
#166834=CARTESIAN_POINT('Ctrl Pts',(-16.1559070823762,-8.04468584505497,
-1057.74191176471));
#166835=CARTESIAN_POINT('Ctrl Pts',(-16.9013570056506,-6.54762058645456,
-1059.23602941177));
#166836=CARTESIAN_POINT('Ctrl Pts',(-17.3590292079831,-4.93906964482095,
-1060.73014705882));
#166837=CARTESIAN_POINT('Ctrl Pts',(-17.8167014103155,-3.33051870318735,
-1062.22426470588));
#166838=CARTESIAN_POINT('Ctrl Pts',(-17.9710104137728,-1.66525935159368,
-1063.71838235294));
#166839=CARTESIAN_POINT('Ctrl Pts',(-18.1253194172301,-1.10985572039171E-15,
-1065.2125));
#166840=CARTESIAN_POINT('Ctrl Pts',(-17.9710104137728,1.66525935159367,
-1066.70661764706));
#166841=CARTESIAN_POINT('Ctrl Pts',(-17.8167014103155,3.33051870318735,
-1068.20073529412));
#166842=CARTESIAN_POINT('Ctrl Pts',(-17.3590292079831,4.93906964482096,
-1069.69485294118));
#166843=CARTESIAN_POINT('Ctrl Pts',(-16.9013570056506,6.54762058645456,
-1071.18897058824));
#166844=CARTESIAN_POINT('Ctrl Pts',(-16.1559070823762,8.04468584505497,
-1072.68308823529));
#166845=CARTESIAN_POINT('Ctrl Pts',(-15.4104571591017,9.54175110365538,
-1074.17720588235));
#166846=CARTESIAN_POINT('Ctrl Pts',(-14.4026149179538,10.8763499173728,
-1075.67132352941));
#166847=CARTESIAN_POINT('Ctrl Pts',(-13.3947726768058,12.2109487310903,
-1077.16544117647));
#166848=CARTESIAN_POINT('Ctrl Pts',(-12.1588589765331,13.3376329379985,
-1078.65955882353));
#166849=CARTESIAN_POINT('Ctrl Pts',(-10.9229452762603,14.4643171449067,
-1080.15367647059));
#166850=CARTESIAN_POINT('Ctrl Pts',(-9.50104767561052,15.3447188656481,
-1081.64779411765));
#166851=CARTESIAN_POINT('Ctrl Pts',(-8.07915007496071,16.2251205863895,
-1083.14191176471));
#166852=CARTESIAN_POINT('Ctrl Pts',(-6.51968959134574,16.8292587962898,
-1084.63602941176));
#166853=CARTESIAN_POINT('Ctrl Pts',(-4.96022910773078,17.4333970061901,
-1086.13014705882));
#166854=CARTESIAN_POINT('Ctrl Pts',(-3.31631129755346,17.7406985030951,
-1087.62426470588));
#166855=CARTESIAN_POINT('Ctrl Pts',(-1.67239348737615,18.048,-1089.11838235294));
#166856=CARTESIAN_POINT('Ctrl Pts',(-2.21024254310115E-15,18.048,-1090.6125));
#166857=CARTESIAN_POINT('Ctrl Pts',(1.67239348737616,18.048,-1092.10661764706));
#166858=CARTESIAN_POINT('Ctrl Pts',(3.31631129755346,17.7406985030951,-1093.60073529412));
#166859=CARTESIAN_POINT('Ctrl Pts',(4.96022910773077,17.4333970061901,-1095.09485294118));
#166860=CARTESIAN_POINT('Ctrl Pts',(6.51968959134575,16.8292587962898,-1096.58897058824));
#166861=CARTESIAN_POINT('Ctrl Pts',(8.07915007496071,16.2251205863895,-1098.08308823529));
#166862=CARTESIAN_POINT('Ctrl Pts',(9.50104767561053,15.3447188656481,-1099.57720588235));
#166863=CARTESIAN_POINT('Ctrl Pts',(10.9229452762603,14.4643171449067,-1101.07132352941));
#166864=CARTESIAN_POINT('Ctrl Pts',(12.1588589765331,13.3376329379985,-1102.56544117647));
#166865=CARTESIAN_POINT('Ctrl Pts',(13.3947726768058,12.2109487310903,-1104.05955882353));
#166866=CARTESIAN_POINT('Ctrl Pts',(14.4026149179538,10.8763499173728,-1105.55367647059));
#166867=CARTESIAN_POINT('Ctrl Pts',(15.4104571591017,9.54175110365538,-1107.04779411765));
#166868=CARTESIAN_POINT('Ctrl Pts',(16.1559070823762,8.04468584505496,-1108.54191176471));
#166869=CARTESIAN_POINT('Ctrl Pts',(16.9013570056506,6.54762058645456,-1110.03602941176));
#166870=CARTESIAN_POINT('Ctrl Pts',(17.3590292079831,4.93906964482096,-1111.53014705882));
#166871=CARTESIAN_POINT('Ctrl Pts',(17.8167014103155,3.33051870318735,-1113.02426470588));
#166872=CARTESIAN_POINT('Ctrl Pts',(17.9710104137728,1.66525935159367,-1114.51838235294));
#166873=CARTESIAN_POINT('Ctrl Pts',(18.1253194172301,3.32956716117513E-15,
-1116.0125));
#166874=CARTESIAN_POINT('Ctrl Pts',(17.9710104137728,-1.66525935159367,
-1117.50661764706));
#166875=CARTESIAN_POINT('Ctrl Pts',(17.8167014103155,-3.33051870318736,
-1119.00073529412));
#166876=CARTESIAN_POINT('Ctrl Pts',(17.3590292079831,-4.93906964482095,
-1120.49485294118));
#166877=CARTESIAN_POINT('Ctrl Pts',(16.9013570056506,-6.54762058645456,
-1121.98897058824));
#166878=CARTESIAN_POINT('Ctrl Pts',(16.1559070823762,-8.04468584505497,
-1123.48308823529));
#166879=CARTESIAN_POINT('Ctrl Pts',(15.4104571591017,-9.54175110365538,
-1124.97720588235));
#166880=CARTESIAN_POINT('Ctrl Pts',(14.4026149179538,-10.8763499173728,
-1126.47132352941));
#166881=CARTESIAN_POINT('Ctrl Pts',(13.3947726768058,-12.2109487310903,
-1127.96544117647));
#166882=CARTESIAN_POINT('Ctrl Pts',(12.1588589765331,-13.3376329379985,
-1129.45955882353));
#166883=CARTESIAN_POINT('Ctrl Pts',(10.9229452762603,-14.4643171449067,
-1130.95367647059));
#166884=CARTESIAN_POINT('Ctrl Pts',(9.50104767561053,-15.3447188656481,
-1132.44779411765));
#166885=CARTESIAN_POINT('Ctrl Pts',(8.07915007496071,-16.2251205863895,
-1133.94191176471));
#166886=CARTESIAN_POINT('Ctrl Pts',(6.51968959134574,-16.8292587962898,
-1135.43602941176));
#166887=CARTESIAN_POINT('Ctrl Pts',(4.96022910773078,-17.4333970061901,
-1136.93014705882));
#166888=CARTESIAN_POINT('Ctrl Pts',(3.31631129755346,-17.7406985030951,
-1138.42426470588));
#166889=CARTESIAN_POINT('Ctrl Pts',(1.67239348737615,-18.048,-1139.91838235294));
#166890=CARTESIAN_POINT('Ctrl Pts',(0.,-18.048,-1141.4125));
#166891=CARTESIAN_POINT('Ctrl Pts',(-1.67239348737615,-18.048,-1142.90661764706));
#166892=CARTESIAN_POINT('Ctrl Pts',(-3.31631129755346,-17.7406985030951,
-1144.40073529412));
#166893=CARTESIAN_POINT('Ctrl Pts',(-4.96022910773077,-17.4333970061901,
-1145.89485294118));
#166894=CARTESIAN_POINT('Ctrl Pts',(-6.51968959134574,-16.8292587962898,
-1147.38897058824));
#166895=CARTESIAN_POINT('Ctrl Pts',(-8.07915007496071,-16.2251205863895,
-1148.88308823529));
#166896=CARTESIAN_POINT('Ctrl Pts',(-9.50104767561052,-15.3447188656481,
-1150.37720588235));
#166897=CARTESIAN_POINT('Ctrl Pts',(-10.9229452762603,-14.4643171449067,
-1151.87132352941));
#166898=CARTESIAN_POINT('Ctrl Pts',(-12.1588589765331,-13.3376329379985,
-1153.36544117647));
#166899=CARTESIAN_POINT('Ctrl Pts',(-13.3947726768058,-12.2109487310903,
-1154.85955882353));
#166900=CARTESIAN_POINT('Ctrl Pts',(-14.4026149179538,-10.8763499173728,
-1156.35367647059));
#166901=CARTESIAN_POINT('Ctrl Pts',(-15.4104571591017,-9.54175110365538,
-1157.84779411765));
#166902=CARTESIAN_POINT('Ctrl Pts',(-16.1559070823762,-8.04468584505497,
-1159.34191176471));
#166903=CARTESIAN_POINT('Ctrl Pts',(-16.9013570056506,-6.54762058645456,
-1160.83602941176));
#166904=CARTESIAN_POINT('Ctrl Pts',(-17.3590292079831,-4.93906964482095,
-1162.33014705882));
#166905=CARTESIAN_POINT('Ctrl Pts',(-17.8167014103155,-3.33051870318735,
-1163.82426470588));
#166906=CARTESIAN_POINT('Ctrl Pts',(-17.9710104137728,-1.66525935159368,
-1165.31838235294));
#166907=CARTESIAN_POINT('Ctrl Pts',(-18.1253194172301,-1.10985572039171E-15,
-1166.8125));
#166908=CARTESIAN_POINT('Ctrl Pts',(-17.9710104137728,1.66525935159367,
-1168.30661764706));
#166909=CARTESIAN_POINT('Ctrl Pts',(-17.8167014103155,3.33051870318735,
-1169.80073529412));
#166910=CARTESIAN_POINT('Ctrl Pts',(-17.3590292079831,4.93906964482096,
-1171.29485294118));
#166911=CARTESIAN_POINT('Ctrl Pts',(-16.9013570056506,6.54762058645456,
-1172.78897058824));
#166912=CARTESIAN_POINT('Ctrl Pts',(-16.1559070823762,8.04468584505497,
-1174.28308823529));
#166913=CARTESIAN_POINT('Ctrl Pts',(-15.4104571591017,9.54175110365538,
-1175.77720588235));
#166914=CARTESIAN_POINT('Ctrl Pts',(-14.4026149179538,10.8763499173728,
-1177.27132352941));
#166915=CARTESIAN_POINT('Ctrl Pts',(-13.3947726768058,12.2109487310903,
-1178.76544117647));
#166916=CARTESIAN_POINT('Ctrl Pts',(-12.1588589765331,13.3376329379985,
-1180.25955882353));
#166917=CARTESIAN_POINT('Ctrl Pts',(-10.9229452762603,14.4643171449067,
-1181.75367647059));
#166918=CARTESIAN_POINT('Ctrl Pts',(-9.50104767561052,15.3447188656481,
-1183.24779411765));
#166919=CARTESIAN_POINT('Ctrl Pts',(-8.07915007496071,16.2251205863895,
-1184.74191176471));
#166920=CARTESIAN_POINT('Ctrl Pts',(-6.51968959134574,16.8292587962898,
-1186.23602941176));
#166921=CARTESIAN_POINT('Ctrl Pts',(-4.96022910773078,17.4333970061901,
-1187.73014705882));
#166922=CARTESIAN_POINT('Ctrl Pts',(-3.31631129755346,17.7406985030951,
-1189.22426470588));
#166923=CARTESIAN_POINT('Ctrl Pts',(-1.67239348737615,18.048,-1190.71838235294));
#166924=CARTESIAN_POINT('Ctrl Pts',(-2.21024254310115E-15,18.048,-1192.2125));
#166925=CARTESIAN_POINT('Ctrl Pts',(1.67239348737616,18.048,-1193.70661764706));
#166926=CARTESIAN_POINT('Ctrl Pts',(3.31631129755346,17.7406985030951,-1195.20073529412));
#166927=CARTESIAN_POINT('Ctrl Pts',(4.96022910773077,17.4333970061901,-1196.69485294118));
#166928=CARTESIAN_POINT('Ctrl Pts',(6.51968959134575,16.8292587962898,-1198.18897058824));
#166929=CARTESIAN_POINT('Ctrl Pts',(8.07915007496071,16.2251205863895,-1199.68308823529));
#166930=CARTESIAN_POINT('Ctrl Pts',(9.50104767561053,15.3447188656481,-1201.17720588235));
#166931=CARTESIAN_POINT('Ctrl Pts',(10.9229452762603,14.4643171449067,-1202.67132352941));
#166932=CARTESIAN_POINT('Ctrl Pts',(12.1588589765331,13.3376329379985,-1204.16544117647));
#166933=CARTESIAN_POINT('Ctrl Pts',(13.3947726768058,12.2109487310903,-1205.65955882353));
#166934=CARTESIAN_POINT('Ctrl Pts',(14.4026149179538,10.8763499173728,-1207.15367647059));
#166935=CARTESIAN_POINT('Ctrl Pts',(15.4104571591017,9.54175110365538,-1208.64779411765));
#166936=CARTESIAN_POINT('Ctrl Pts',(16.1559070823762,8.04468584505496,-1210.14191176471));
#166937=CARTESIAN_POINT('Ctrl Pts',(16.9013570056506,6.54762058645456,-1211.63602941176));
#166938=CARTESIAN_POINT('Ctrl Pts',(17.3590292079831,4.93906964482096,-1213.13014705882));
#166939=CARTESIAN_POINT('Ctrl Pts',(17.8167014103155,3.33051870318735,-1214.62426470588));
#166940=CARTESIAN_POINT('Ctrl Pts',(17.9710104137728,1.66525935159367,-1216.11838235294));
#166941=CARTESIAN_POINT('Ctrl Pts',(18.1253194172301,3.32956716117513E-15,
-1217.6125));
#166942=CARTESIAN_POINT('Ctrl Pts',(17.9710104137728,-1.66525935159367,
-1219.10661764706));
#166943=CARTESIAN_POINT('Ctrl Pts',(17.8167014103155,-3.33051870318736,
-1220.60073529412));
#166944=CARTESIAN_POINT('Ctrl Pts',(17.3590292079831,-4.93906964482095,
-1222.09485294118));
#166945=CARTESIAN_POINT('Ctrl Pts',(16.9013570056506,-6.54762058645456,
-1223.58897058824));
#166946=CARTESIAN_POINT('Ctrl Pts',(16.1559070823762,-8.04468584505497,
-1225.08308823529));
#166947=CARTESIAN_POINT('Ctrl Pts',(15.4104571591017,-9.54175110365538,
-1226.57720588235));
#166948=CARTESIAN_POINT('Ctrl Pts',(14.4026149179538,-10.8763499173728,
-1228.07132352941));
#166949=CARTESIAN_POINT('Ctrl Pts',(13.3947726768058,-12.2109487310903,
-1229.56544117647));
#166950=CARTESIAN_POINT('Ctrl Pts',(12.1588589765331,-13.3376329379985,
-1231.05955882353));
#166951=CARTESIAN_POINT('Ctrl Pts',(10.9229452762603,-14.4643171449067,
-1232.55367647059));
#166952=CARTESIAN_POINT('Ctrl Pts',(9.50104767561053,-15.3447188656481,
-1234.04779411765));
#166953=CARTESIAN_POINT('Ctrl Pts',(8.07915007496071,-16.2251205863895,
-1235.54191176471));
#166954=CARTESIAN_POINT('Ctrl Pts',(6.51968959134574,-16.8292587962898,
-1237.03602941176));
#166955=CARTESIAN_POINT('Ctrl Pts',(4.96022910773078,-17.4333970061901,
-1238.53014705882));
#166956=CARTESIAN_POINT('Ctrl Pts',(3.31631129755346,-17.7406985030951,
-1240.02426470588));
#166957=CARTESIAN_POINT('Ctrl Pts',(1.67239348737615,-18.048,-1241.51838235294));
#166958=CARTESIAN_POINT('Ctrl Pts',(0.,-18.048,-1243.0125));
#166959=CARTESIAN_POINT('Ctrl Pts',(-1.67239348737615,-18.048,-1244.50661764706));
#166960=CARTESIAN_POINT('Ctrl Pts',(-3.31631129755346,-17.7406985030951,
-1246.00073529412));
#166961=CARTESIAN_POINT('Ctrl Pts',(-4.96022910773077,-17.4333970061901,
-1247.49485294118));
#166962=CARTESIAN_POINT('Ctrl Pts',(-6.51968959134574,-16.8292587962898,
-1248.98897058824));
#166963=CARTESIAN_POINT('Ctrl Pts',(-8.07915007496071,-16.2251205863895,
-1250.48308823529));
#166964=CARTESIAN_POINT('Ctrl Pts',(-9.50104767561052,-15.3447188656481,
-1251.97720588235));
#166965=CARTESIAN_POINT('Ctrl Pts',(-10.9229452762603,-14.4643171449067,
-1253.47132352941));
#166966=CARTESIAN_POINT('Ctrl Pts',(-12.1588589765331,-13.3376329379985,
-1254.96544117647));
#166967=CARTESIAN_POINT('Ctrl Pts',(-13.3947726768058,-12.2109487310903,
-1256.45955882353));
#166968=CARTESIAN_POINT('Ctrl Pts',(-14.4026149179538,-10.8763499173728,
-1257.95367647059));
#166969=CARTESIAN_POINT('Ctrl Pts',(-15.4104571591017,-9.54175110365538,
-1259.44779411765));
#166970=CARTESIAN_POINT('Ctrl Pts',(-16.1559070823762,-8.04468584505497,
-1260.94191176471));
#166971=CARTESIAN_POINT('Ctrl Pts',(-16.9013570056506,-6.54762058645456,
-1262.43602941176));
#166972=CARTESIAN_POINT('Ctrl Pts',(-17.3590292079831,-4.93906964482095,
-1263.93014705882));
#166973=CARTESIAN_POINT('Ctrl Pts',(-17.8167014103155,-3.33051870318735,
-1265.42426470588));
#166974=CARTESIAN_POINT('Ctrl Pts',(-17.9710104137728,-1.66525935159368,
-1266.91838235294));
#166975=CARTESIAN_POINT('Ctrl Pts',(-18.1253194172301,-1.10985572039171E-15,
-1268.4125));
#166976=CARTESIAN_POINT('Ctrl Pts',(-17.9710104137728,1.66525935159367,
-1269.90661764706));
#166977=CARTESIAN_POINT('Ctrl Pts',(-17.8167014103155,3.33051870318735,
-1271.40073529412));
#166978=CARTESIAN_POINT('Ctrl Pts',(-17.3590292079831,4.93906964482096,
-1272.89485294118));
#166979=CARTESIAN_POINT('Ctrl Pts',(-16.9013570056506,6.54762058645456,
-1274.38897058824));
#166980=CARTESIAN_POINT('Ctrl Pts',(-16.1559070823762,8.04468584505497,
-1275.88308823529));
#166981=CARTESIAN_POINT('Ctrl Pts',(-15.4104571591017,9.54175110365538,
-1277.37720588235));
#166982=CARTESIAN_POINT('Ctrl Pts',(-14.4026149179538,10.8763499173728,
-1278.87132352941));
#166983=CARTESIAN_POINT('Ctrl Pts',(-13.3947726768058,12.2109487310903,
-1280.36544117647));
#166984=CARTESIAN_POINT('Ctrl Pts',(-12.1588589765331,13.3376329379985,
-1281.85955882353));
#166985=CARTESIAN_POINT('Ctrl Pts',(-10.9229452762603,14.4643171449067,
-1283.35367647059));
#166986=CARTESIAN_POINT('Ctrl Pts',(-9.50104767561052,15.3447188656481,
-1284.84779411765));
#166987=CARTESIAN_POINT('Ctrl Pts',(-8.07915007496071,16.2251205863895,
-1286.34191176471));
#166988=CARTESIAN_POINT('Ctrl Pts',(-6.51968959134574,16.8292587962898,
-1287.83602941176));
#166989=CARTESIAN_POINT('Ctrl Pts',(-4.96022910773078,17.4333970061901,
-1289.33014705882));
#166990=CARTESIAN_POINT('Ctrl Pts',(-3.31631129755346,17.7406985030951,
-1290.82426470588));
#166991=CARTESIAN_POINT('Ctrl Pts',(-1.67239348737615,18.048,-1292.31838235294));
#166992=CARTESIAN_POINT('Ctrl Pts',(-2.21024254310115E-15,18.048,-1293.8125));
#166993=CARTESIAN_POINT('Ctrl Pts',(1.67239348737616,18.048,-1295.30661764706));
#166994=CARTESIAN_POINT('Ctrl Pts',(3.31631129755346,17.7406985030951,-1296.80073529412));
#166995=CARTESIAN_POINT('Ctrl Pts',(4.96022910773077,17.4333970061901,-1298.29485294118));
#166996=CARTESIAN_POINT('Ctrl Pts',(6.51968959134575,16.8292587962898,-1299.78897058824));
#166997=CARTESIAN_POINT('Ctrl Pts',(8.07915007496071,16.2251205863895,-1301.28308823529));
#166998=CARTESIAN_POINT('Ctrl Pts',(9.50104767561053,15.3447188656481,-1302.77720588235));
#166999=CARTESIAN_POINT('Ctrl Pts',(10.9229452762603,14.4643171449067,-1304.27132352941));
#167000=CARTESIAN_POINT('Ctrl Pts',(12.1588589765331,13.3376329379985,-1305.76544117647));
#167001=CARTESIAN_POINT('Ctrl Pts',(13.3947726768058,12.2109487310903,-1307.25955882353));
#167002=CARTESIAN_POINT('Ctrl Pts',(14.4026149179538,10.8763499173728,-1308.75367647059));
#167003=CARTESIAN_POINT('Ctrl Pts',(15.4104571591017,9.54175110365538,-1310.24779411765));
#167004=CARTESIAN_POINT('Ctrl Pts',(16.1559070823762,8.04468584505496,-1311.74191176471));
#167005=CARTESIAN_POINT('Ctrl Pts',(16.9013570056506,6.54762058645456,-1313.23602941176));
#167006=CARTESIAN_POINT('Ctrl Pts',(17.3590292079831,4.93906964482096,-1314.73014705882));
#167007=CARTESIAN_POINT('Ctrl Pts',(17.8167014103155,3.33051870318735,-1316.22426470588));
#167008=CARTESIAN_POINT('Ctrl Pts',(17.9710104137728,1.66525935159367,-1317.71838235294));
#167009=CARTESIAN_POINT('Ctrl Pts',(18.1253194172301,3.32956716117513E-15,
-1319.2125));
#167010=CARTESIAN_POINT('Ctrl Pts',(17.9710104137728,-1.66525935159367,
-1320.70661764706));
#167011=CARTESIAN_POINT('Ctrl Pts',(17.8167014103155,-3.33051870318736,
-1322.20073529412));
#167012=CARTESIAN_POINT('Ctrl Pts',(17.3590292079831,-4.93906964482095,
-1323.69485294118));
#167013=CARTESIAN_POINT('Ctrl Pts',(16.9013570056506,-6.54762058645456,
-1325.18897058824));
#167014=CARTESIAN_POINT('Ctrl Pts',(16.1559070823762,-8.04468584505497,
-1326.68308823529));
#167015=CARTESIAN_POINT('Ctrl Pts',(15.4104571591017,-9.54175110365538,
-1328.17720588235));
#167016=CARTESIAN_POINT('Ctrl Pts',(14.4026149179538,-10.8763499173728,
-1329.67132352941));
#167017=CARTESIAN_POINT('Ctrl Pts',(13.3947726768058,-12.2109487310903,
-1331.16544117647));
#167018=CARTESIAN_POINT('Ctrl Pts',(12.1588589765331,-13.3376329379985,
-1332.65955882353));
#167019=CARTESIAN_POINT('Ctrl Pts',(10.9229452762603,-14.4643171449067,
-1334.15367647059));
#167020=CARTESIAN_POINT('Ctrl Pts',(9.50104767561053,-15.3447188656481,
-1335.64779411765));
#167021=CARTESIAN_POINT('Ctrl Pts',(8.07915007496071,-16.2251205863895,
-1337.14191176471));
#167022=CARTESIAN_POINT('Ctrl Pts',(6.51968959134574,-16.8292587962898,
-1338.63602941176));
#167023=CARTESIAN_POINT('Ctrl Pts',(4.96022910773078,-17.4333970061901,
-1340.13014705882));
#167024=CARTESIAN_POINT('Ctrl Pts',(3.31631129755346,-17.7406985030951,
-1341.62426470588));
#167025=CARTESIAN_POINT('Ctrl Pts',(1.67239348737615,-18.048,-1343.11838235294));
#167026=CARTESIAN_POINT('Ctrl Pts',(0.,-18.048,-1344.6125));
#167027=CARTESIAN_POINT('Ctrl Pts',(-1.67239348737615,-18.048,-1346.10661764706));
#167028=CARTESIAN_POINT('Ctrl Pts',(-3.31631129755346,-17.7406985030951,
-1347.60073529412));
#167029=CARTESIAN_POINT('Ctrl Pts',(-4.96022910773077,-17.4333970061901,
-1349.09485294118));
#167030=CARTESIAN_POINT('Ctrl Pts',(-6.51968959134574,-16.8292587962898,
-1350.58897058824));
#167031=CARTESIAN_POINT('Ctrl Pts',(-8.07915007496071,-16.2251205863895,
-1352.08308823529));
#167032=CARTESIAN_POINT('Ctrl Pts',(-9.50104767561052,-15.3447188656481,
-1353.57720588235));
#167033=CARTESIAN_POINT('Ctrl Pts',(-10.9229452762603,-14.4643171449067,
-1355.07132352941));
#167034=CARTESIAN_POINT('Ctrl Pts',(-12.1588589765331,-13.3376329379985,
-1356.56544117647));
#167035=CARTESIAN_POINT('Ctrl Pts',(-13.3947726768058,-12.2109487310903,
-1358.05955882353));
#167036=CARTESIAN_POINT('Ctrl Pts',(-14.4026149179538,-10.8763499173728,
-1359.55367647059));
#167037=CARTESIAN_POINT('Ctrl Pts',(-15.4104571591017,-9.54175110365538,
-1361.04779411765));
#167038=CARTESIAN_POINT('Ctrl Pts',(-16.1559070823762,-8.04468584505497,
-1362.54191176471));
#167039=CARTESIAN_POINT('Ctrl Pts',(-16.9013570056506,-6.54762058645456,
-1364.03602941176));
#167040=CARTESIAN_POINT('Ctrl Pts',(-17.3590292079831,-4.93906964482095,
-1365.53014705882));
#167041=CARTESIAN_POINT('Ctrl Pts',(-17.8167014103155,-3.33051870318735,
-1367.02426470588));
#167042=CARTESIAN_POINT('Ctrl Pts',(-17.9710104137728,-1.66525935159368,
-1368.51838235294));
#167043=CARTESIAN_POINT('Ctrl Pts',(-18.1253194172301,-1.10985572039171E-15,
-1370.0125));
#167044=CARTESIAN_POINT('Ctrl Pts',(-17.9710104137728,1.66525935159367,
-1371.50661764706));
#167045=CARTESIAN_POINT('Ctrl Pts',(-17.8167014103155,3.33051870318735,
-1373.00073529412));
#167046=CARTESIAN_POINT('Ctrl Pts',(-17.3590292079831,4.93906964482096,
-1374.49485294118));
#167047=CARTESIAN_POINT('Ctrl Pts',(-16.9013570056506,6.54762058645456,
-1375.98897058824));
#167048=CARTESIAN_POINT('Ctrl Pts',(-16.1559070823762,8.04468584505497,
-1377.48308823529));
#167049=CARTESIAN_POINT('Ctrl Pts',(-15.4104571591017,9.54175110365538,
-1378.97720588235));
#167050=CARTESIAN_POINT('Ctrl Pts',(-14.4026149179538,10.8763499173728,
-1380.47132352941));
#167051=CARTESIAN_POINT('Ctrl Pts',(-13.3947726768058,12.2109487310903,
-1381.96544117647));
#167052=CARTESIAN_POINT('Ctrl Pts',(-12.1588589765331,13.3376329379985,
-1383.45955882353));
#167053=CARTESIAN_POINT('Ctrl Pts',(-10.9229452762603,14.4643171449067,
-1384.95367647059));
#167054=CARTESIAN_POINT('Ctrl Pts',(-9.50104767561052,15.3447188656481,
-1386.44779411765));
#167055=CARTESIAN_POINT('Ctrl Pts',(-8.07915007496071,16.2251205863895,
-1387.94191176471));
#167056=CARTESIAN_POINT('Ctrl Pts',(-6.51968959134574,16.8292587962898,
-1389.43602941176));
#167057=CARTESIAN_POINT('Ctrl Pts',(-4.96022910773078,17.4333970061901,
-1390.93014705882));
#167058=CARTESIAN_POINT('Ctrl Pts',(-3.31631129755346,17.7406985030951,
-1392.42426470588));
#167059=CARTESIAN_POINT('Ctrl Pts',(-1.67239348737615,18.048,-1393.91838235294));
#167060=CARTESIAN_POINT('Ctrl Pts',(-2.21024254310115E-15,18.048,-1395.4125));
#167061=CARTESIAN_POINT('Ctrl Pts',(1.67239348737616,18.048,-1396.90661764706));
#167062=CARTESIAN_POINT('Ctrl Pts',(3.31631129755346,17.7406985030951,-1398.40073529412));
#167063=CARTESIAN_POINT('Ctrl Pts',(4.96022910773077,17.4333970061901,-1399.89485294118));
#167064=CARTESIAN_POINT('Ctrl Pts',(6.51968959134575,16.8292587962898,-1401.38897058824));
#167065=CARTESIAN_POINT('Ctrl Pts',(8.07915007496071,16.2251205863895,-1402.88308823529));
#167066=CARTESIAN_POINT('Ctrl Pts',(9.50104767561053,15.3447188656481,-1404.37720588235));
#167067=CARTESIAN_POINT('Ctrl Pts',(10.9229452762603,14.4643171449067,-1405.87132352941));
#167068=CARTESIAN_POINT('Ctrl Pts',(12.1588589765331,13.3376329379985,-1407.36544117647));
#167069=CARTESIAN_POINT('Ctrl Pts',(13.3947726768058,12.2109487310903,-1408.85955882353));
#167070=CARTESIAN_POINT('Ctrl Pts',(14.4026149179538,10.8763499173728,-1410.35367647059));
#167071=CARTESIAN_POINT('Ctrl Pts',(15.4104571591017,9.54175110365538,-1411.84779411765));
#167072=CARTESIAN_POINT('Ctrl Pts',(16.1559070823762,8.04468584505496,-1413.34191176471));
#167073=CARTESIAN_POINT('Ctrl Pts',(16.9013570056506,6.54762058645456,-1414.83602941176));
#167074=CARTESIAN_POINT('Ctrl Pts',(17.3590292079831,4.93906964482096,-1416.33014705882));
#167075=CARTESIAN_POINT('Ctrl Pts',(17.8167014103155,3.33051870318735,-1417.82426470588));
#167076=CARTESIAN_POINT('Ctrl Pts',(17.9710104137728,1.66525935159367,-1419.31838235294));
#167077=CARTESIAN_POINT('Ctrl Pts',(18.1253194172301,3.32956716117513E-15,
-1420.8125));
#167078=CARTESIAN_POINT('Ctrl Pts',(17.9710104137728,-1.66525935159367,
-1422.30661764706));
#167079=CARTESIAN_POINT('Ctrl Pts',(17.8167014103155,-3.33051870318736,
-1423.80073529412));
#167080=CARTESIAN_POINT('Ctrl Pts',(17.3590292079831,-4.93906964482095,
-1425.29485294118));
#167081=CARTESIAN_POINT('Ctrl Pts',(16.9013570056506,-6.54762058645456,
-1426.78897058824));
#167082=CARTESIAN_POINT('Ctrl Pts',(16.1559070823762,-8.04468584505497,
-1428.28308823529));
#167083=CARTESIAN_POINT('Ctrl Pts',(15.4104571591017,-9.54175110365538,
-1429.77720588235));
#167084=CARTESIAN_POINT('Ctrl Pts',(14.4026149179538,-10.8763499173728,
-1431.27132352941));
#167085=CARTESIAN_POINT('Ctrl Pts',(13.3947726768058,-12.2109487310903,
-1432.76544117647));
#167086=CARTESIAN_POINT('Ctrl Pts',(12.1588589765331,-13.3376329379985,
-1434.25955882353));
#167087=CARTESIAN_POINT('Ctrl Pts',(10.9229452762603,-14.4643171449067,
-1435.75367647059));
#167088=CARTESIAN_POINT('Ctrl Pts',(9.50104767561053,-15.3447188656481,
-1437.24779411765));
#167089=CARTESIAN_POINT('Ctrl Pts',(8.07915007496071,-16.2251205863895,
-1438.74191176471));
#167090=CARTESIAN_POINT('Ctrl Pts',(6.51968959134574,-16.8292587962898,
-1440.23602941176));
#167091=CARTESIAN_POINT('Ctrl Pts',(4.96022910773078,-17.4333970061901,
-1441.73014705882));
#167092=CARTESIAN_POINT('Ctrl Pts',(3.31631129755346,-17.7406985030951,
-1443.22426470588));
#167093=CARTESIAN_POINT('Ctrl Pts',(1.67239348737615,-18.048,-1444.71838235294));
#167094=CARTESIAN_POINT('Ctrl Pts',(0.,-18.048,-1446.2125));
#167095=CARTESIAN_POINT('Ctrl Pts',(-1.67239348737615,-18.048,-1447.70661764706));
#167096=CARTESIAN_POINT('Ctrl Pts',(-3.31631129755346,-17.7406985030951,
-1449.20073529412));
#167097=CARTESIAN_POINT('Ctrl Pts',(-4.96022910773077,-17.4333970061901,
-1450.69485294118));
#167098=CARTESIAN_POINT('Ctrl Pts',(-6.51968959134574,-16.8292587962898,
-1452.18897058824));
#167099=CARTESIAN_POINT('Ctrl Pts',(-8.07915007496071,-16.2251205863895,
-1453.68308823529));
#167100=CARTESIAN_POINT('Ctrl Pts',(-9.50104767561052,-15.3447188656481,
-1455.17720588235));
#167101=CARTESIAN_POINT('Ctrl Pts',(-10.9229452762603,-14.4643171449067,
-1456.67132352941));
#167102=CARTESIAN_POINT('Ctrl Pts',(-12.1588589765331,-13.3376329379985,
-1458.16544117647));
#167103=CARTESIAN_POINT('Ctrl Pts',(-13.3947726768058,-12.2109487310903,
-1459.65955882353));
#167104=CARTESIAN_POINT('Ctrl Pts',(-14.4026149179538,-10.8763499173728,
-1461.15367647059));
#167105=CARTESIAN_POINT('Ctrl Pts',(-15.4104571591017,-9.54175110365538,
-1462.64779411765));
#167106=CARTESIAN_POINT('Ctrl Pts',(-16.1559070823762,-8.04468584505497,
-1464.14191176471));
#167107=CARTESIAN_POINT('Ctrl Pts',(-16.9013570056506,-6.54762058645456,
-1465.63602941176));
#167108=CARTESIAN_POINT('Ctrl Pts',(-17.3590292079831,-4.93906964482095,
-1467.13014705882));
#167109=CARTESIAN_POINT('Ctrl Pts',(-17.8167014103155,-3.33051870318735,
-1468.62426470588));
#167110=CARTESIAN_POINT('Ctrl Pts',(-17.9710104137728,-1.66525935159368,
-1470.11838235294));
#167111=CARTESIAN_POINT('Ctrl Pts',(-18.1253194172301,-1.10985572039171E-15,
-1471.6125));
#167112=CARTESIAN_POINT('Ctrl Pts',(-17.9710104137728,1.66525935159367,
-1473.10661764706));
#167113=CARTESIAN_POINT('Ctrl Pts',(-17.8167014103155,3.33051870318735,
-1474.60073529412));
#167114=CARTESIAN_POINT('Ctrl Pts',(-17.3590292079831,4.93906964482096,
-1476.09485294118));
#167115=CARTESIAN_POINT('Ctrl Pts',(-16.9013570056506,6.54762058645456,
-1477.58897058824));
#167116=CARTESIAN_POINT('Ctrl Pts',(-16.1559070823762,8.04468584505497,
-1479.08308823529));
#167117=CARTESIAN_POINT('Ctrl Pts',(-15.4104571591017,9.54175110365538,
-1480.57720588235));
#167118=CARTESIAN_POINT('Ctrl Pts',(-14.4026149179538,10.8763499173728,
-1482.07132352941));
#167119=CARTESIAN_POINT('Ctrl Pts',(-13.3947726768058,12.2109487310903,
-1483.56544117647));
#167120=CARTESIAN_POINT('Ctrl Pts',(-12.1588589765331,13.3376329379985,
-1485.05955882353));
#167121=CARTESIAN_POINT('Ctrl Pts',(-10.9229452762603,14.4643171449067,
-1486.55367647059));
#167122=CARTESIAN_POINT('Ctrl Pts',(-9.50104767561052,15.3447188656481,
-1488.04779411765));
#167123=CARTESIAN_POINT('Ctrl Pts',(-8.07915007496071,16.2251205863895,
-1489.54191176471));
#167124=CARTESIAN_POINT('Ctrl Pts',(-6.51968959134574,16.8292587962898,
-1491.03602941176));
#167125=CARTESIAN_POINT('Ctrl Pts',(-4.96022910773078,17.4333970061901,
-1492.53014705882));
#167126=CARTESIAN_POINT('Ctrl Pts',(-3.31631129755346,17.7406985030951,
-1494.02426470588));
#167127=CARTESIAN_POINT('Ctrl Pts',(-1.67239348737615,18.048,-1495.51838235294));
#167128=CARTESIAN_POINT('Ctrl Pts',(-2.21024254310115E-15,18.048,-1497.0125));
#167129=CARTESIAN_POINT('Ctrl Pts',(1.67239348737616,18.048,-1498.50661764706));
#167130=CARTESIAN_POINT('Ctrl Pts',(3.31631129755346,17.7406985030951,-1500.00073529412));
#167131=CARTESIAN_POINT('Ctrl Pts',(4.96022910773077,17.4333970061901,-1501.49485294118));
#167132=CARTESIAN_POINT('Ctrl Pts',(6.51968959134575,16.8292587962898,-1502.98897058824));
#167133=CARTESIAN_POINT('Ctrl Pts',(7.54128438222173,16.4334908658498,-1503.96775961253));
#167134=CARTESIAN_POINT('Ctrl Pts',(8.50750525179015,15.9170555816949,-1504.9503325767));
#167135=CARTESIAN_POINT('Ctrl Pts',(23.3054664377218,8.00769496792138,-1519.99873097503));
#167136=CARTESIAN_POINT('Ctrl Pts',(38.1034276236535,0.0983343541478931,
-1535.04712937335));
#167137=CARTESIAN_POINT('Origin',(-4.55601018023444E-6,1.49069329302698E-5,
692.00000002901));
#167138=CARTESIAN_POINT('',(0.,-18.048,1500.28886941341));
#167139=CARTESIAN_POINT('Origin',(5.37704275891775E-14,4.44089209850063E-14,
1504.8993152933));
#167140=CARTESIAN_POINT('Origin',(1.20502921845816E-6,0.00017779754810876,
692.00000007199));
#167141=CARTESIAN_POINT('Origin',(0.,-16.524,1504.95));
#167142=CARTESIAN_POINT('Origin',(0.,15.,1504.95));
#167143=CARTESIAN_POINT('Origin',(0.,0.,692.));
#167144=CARTESIAN_POINT('',(0.,0.,0.));
#167145=CARTESIAN_POINT('Origin',(0.,88.06196,30.1625));
#167146=CARTESIAN_POINT('',(-2.19545458095144E-14,88.8392,27.2224678294277));
#167147=CARTESIAN_POINT('Origin',(0.,88.8392,30.1625));
#167148=CARTESIAN_POINT('',(4.63595923051442E-16,86.5786,26.3769520087407));
#167149=CARTESIAN_POINT('Origin',(-5.27423947715602E-16,88.06196,25.8557566346246));
#167150=CARTESIAN_POINT('',(-4.63595923051442E-16,86.5786,33.9480479912593));
#167151=CARTESIAN_POINT('Origin',(0.,86.5786,30.1625));
#167152=CARTESIAN_POINT('Origin',(0.,86.5786,30.1625));
#167153=CARTESIAN_POINT('Origin',(8.67361737988404E-16,85.9309,24.3332830071269));
#167154=CARTESIAN_POINT('',(0.253999999997468,85.5163328910991,23.893342102003));
#167155=CARTESIAN_POINT('',(-0.254,85.5163328910999,23.8933421020044));
#167156=CARTESIAN_POINT('Ctrl Pts',(-0.253999999999999,85.5163328910999,
23.8933421020044));
#167157=CARTESIAN_POINT('Ctrl Pts',(-0.239161970832706,85.5117377397736,
23.8847753618705));
#167158=CARTESIAN_POINT('Ctrl Pts',(-0.223780545620189,85.5075216342437,
23.876898996833));
#167159=CARTESIAN_POINT('Ctrl Pts',(-0.142699715976584,85.4880734540668,
23.8405156203159));
#167160=CARTESIAN_POINT('Ctrl Pts',(-0.0697029152864557,85.4800084964366,
23.8252830071269));
#167161=CARTESIAN_POINT('Ctrl Pts',(0.0697029152864574,85.4800084964366,
23.8252830071269));
#167162=CARTESIAN_POINT('Ctrl Pts',(0.142699715976585,85.4880734540668,
23.8405156203159));
#167163=CARTESIAN_POINT('Ctrl Pts',(0.223780545619289,85.5075216342435,
23.8768989968326));
#167164=CARTESIAN_POINT('Ctrl Pts',(0.239161970830955,85.5117377397731,
23.8847753618696));
#167165=CARTESIAN_POINT('Ctrl Pts',(0.253999999997466,85.5163328910991,
23.893342102003));
#167166=CARTESIAN_POINT('',(0.254,82.4084671089001,23.8933421020044));
#167167=CARTESIAN_POINT('',(0.254000000000001,85.9309,23.8933421020044));
#167168=CARTESIAN_POINT('',(-0.253999999997468,82.4084671089009,23.893342102003));
#167169=CARTESIAN_POINT('Ctrl Pts',(0.254000000000002,82.4084671089001,
23.8933421020044));
#167170=CARTESIAN_POINT('Ctrl Pts',(0.23916197083271,82.4130622602264,23.8847753618705));
#167171=CARTESIAN_POINT('Ctrl Pts',(0.223780545620191,82.4172783657563,
23.876898996833));
#167172=CARTESIAN_POINT('Ctrl Pts',(0.142699715976589,82.4367265459332,
23.8405156203159));
#167173=CARTESIAN_POINT('Ctrl Pts',(0.0697029152864575,82.4447915035635,
23.8252830071269));
#167174=CARTESIAN_POINT('Ctrl Pts',(-0.0697029152864557,82.4447915035635,
23.8252830071269));
#167175=CARTESIAN_POINT('Ctrl Pts',(-0.142699715976587,82.4367265459332,
23.8405156203159));
#167176=CARTESIAN_POINT('Ctrl Pts',(-0.223780545619291,82.4172783657565,
23.8768989968326));
#167177=CARTESIAN_POINT('Ctrl Pts',(-0.239161970830955,82.4130622602269,
23.8847753618696));
#167178=CARTESIAN_POINT('Ctrl Pts',(-0.253999999997466,82.4084671089009,
23.893342102003));
#167179=CARTESIAN_POINT('',(-0.254,85.9309,23.8933421020044));
#167180=CARTESIAN_POINT('Origin',(0.,81.9939,30.1625));
#167181=CARTESIAN_POINT('',(-2.778125,81.9939,25.3506463502227));
#167182=CARTESIAN_POINT('',(2.778125,81.9939,25.3506463502227));
#167183=CARTESIAN_POINT('Origin',(0.,81.9939,30.1625));
#167184=CARTESIAN_POINT('Ctrl Pts',(-0.253999999996936,82.4084671089011,
23.8933421020027));
#167185=CARTESIAN_POINT('Ctrl Pts',(-1.59266295510872,81.9939,24.6662195194906));
#167186=CARTESIAN_POINT('Ctrl Pts',(-2.778125,81.9939,25.3506463502227));
#167187=CARTESIAN_POINT('Ctrl Pts',(2.77812500000002,81.9939,25.3506463502227));
#167188=CARTESIAN_POINT('Ctrl Pts',(1.59266295510979,81.9939,24.6662195194913));
#167189=CARTESIAN_POINT('Ctrl Pts',(0.253999999999473,82.4084671089003,
23.8933421020041));
#167190=CARTESIAN_POINT('Origin',(0.,92.3825,30.1625));
#167191=CARTESIAN_POINT('',(-6.29897081141441E-16,81.9939,25.019));
#167192=CARTESIAN_POINT('Origin',(0.,81.9939,30.1625));
#167193=CARTESIAN_POINT('',(-6.29897081141441E-16,76.444,25.019));
#167194=CARTESIAN_POINT('',(-6.29897081141441E-16,92.3825,25.019));
#167195=CARTESIAN_POINT('Origin',(0.,76.444,30.1625));
#167196=CARTESIAN_POINT('Origin',(0.,85.9309,30.1625));
#167197=CARTESIAN_POINT('',(-2.778125,85.9309,34.9743536497773));
#167198=CARTESIAN_POINT('',(-6.80444377776248E-16,85.9309,35.71875));
#167199=CARTESIAN_POINT('Origin',(0.,85.9309,30.1625));
#167200=CARTESIAN_POINT('',(-0.25399999999747,85.5163328910991,36.431657897997));
#167201=CARTESIAN_POINT('Ctrl Pts',(-0.253999999996926,85.5163328910989,
36.4316578979973));
#167202=CARTESIAN_POINT('Ctrl Pts',(-1.59266295510872,85.9309,35.6587804805094));
#167203=CARTESIAN_POINT('Ctrl Pts',(-2.77812499999999,85.9309,34.9743536497773));
#167204=CARTESIAN_POINT('',(0.253999999999998,85.5163328910999,36.4316578979955));
#167205=CARTESIAN_POINT('Ctrl Pts',(-0.253999999997471,85.5163328910991,
36.431657897997));
#167206=CARTESIAN_POINT('Ctrl Pts',(-0.239161970830961,85.5117377397731,
36.4402246381304));
#167207=CARTESIAN_POINT('Ctrl Pts',(-0.22378054561929,85.5075216342435,
36.4481010031674));
#167208=CARTESIAN_POINT('Ctrl Pts',(-0.142699715976586,85.4880734540668,
36.4844843796841));
#167209=CARTESIAN_POINT('Ctrl Pts',(-0.0697029152864572,85.4800084964366,
36.4997169928731));
#167210=CARTESIAN_POINT('Ctrl Pts',(0.0697029152864559,85.4800084964366,
36.4997169928731));
#167211=CARTESIAN_POINT('Ctrl Pts',(0.142699715976579,85.4880734540668,
36.4844843796841));
#167212=CARTESIAN_POINT('Ctrl Pts',(0.223780545620182,85.5075216342437,
36.448101003167));
#167213=CARTESIAN_POINT('Ctrl Pts',(0.239161970832703,85.5117377397736,
36.4402246381295));
#167214=CARTESIAN_POINT('Ctrl Pts',(0.253999999999996,85.5163328910999,
36.4316578979955));
#167215=CARTESIAN_POINT('',(2.778125,85.9309,34.9743536497773));
#167216=CARTESIAN_POINT('Ctrl Pts',(2.77812499999997,85.9309,34.9743536497773));
#167217=CARTESIAN_POINT('Ctrl Pts',(1.59266295510976,85.9309,35.6587804805088));
#167218=CARTESIAN_POINT('Ctrl Pts',(0.253999999999462,85.5163328910997,
36.4316578979959));
#167219=CARTESIAN_POINT('Origin',(0.,85.9309,30.1625));
#167220=CARTESIAN_POINT('Origin',(0.,86.5786,30.1625));
#167221=CARTESIAN_POINT('',(2.778125,85.9309,25.3506463502227));
#167222=CARTESIAN_POINT('',(-2.778125,85.9309,25.3506463502227));
#167223=CARTESIAN_POINT('Origin',(0.,85.9309,30.1625));
#167224=CARTESIAN_POINT('',(-5.55625,85.9309,30.1625));
#167225=CARTESIAN_POINT('Origin',(0.,85.9309,30.1625));
#167226=CARTESIAN_POINT('Origin',(0.,85.9309,30.1625));
#167227=CARTESIAN_POINT('',(-4.63595923051442E-16,86.5786,33.9480479912593));
#167228=CARTESIAN_POINT('',(5.55625,85.9309,30.1625));
#167229=CARTESIAN_POINT('Origin',(0.,85.9309,30.1625));
#167230=CARTESIAN_POINT('Origin',(0.,85.9309,30.1625));
#167231=CARTESIAN_POINT('Origin',(0.,90.50036,30.1625));
#167232=CARTESIAN_POINT('',(4.10011707243361E-16,90.0597468392398,26.8145003356982));
#167233=CARTESIAN_POINT('Origin',(0.,90.0597468392398,30.1625));
#167234=CARTESIAN_POINT('Origin',(0.,90.1426015156173,30.1625));
#167235=CARTESIAN_POINT('',(4.05855902421057E-16,90.3626969268466,33.4765649426727));
#167236=CARTESIAN_POINT('',(-4.05855902421057E-16,90.3626969268466,26.8484350573273));
#167237=CARTESIAN_POINT('Origin',(0.,90.3626969268466,30.1625));
#167238=CARTESIAN_POINT('Origin',(0.,90.3626969268466,30.1625));
#167239=CARTESIAN_POINT('Origin',(-3.32911451644902E-16,90.1426015156173,
27.4440716998837));
#167240=CARTESIAN_POINT('Origin',(0.,92.8100477056147,30.1625));
#167241=CARTESIAN_POINT('',(-2.95107708105312E-16,92.8100477056147,32.5722373080204));
#167242=CARTESIAN_POINT('',(-2.95107708105312E-16,92.8100477056147,32.5722373080204));
#167243=CARTESIAN_POINT('',(2.95107708105313E-16,92.8100477056147,27.7527626919796));
#167244=CARTESIAN_POINT('Origin',(0.,92.8100477056147,30.1625));
#167245=CARTESIAN_POINT('Origin',(0.,92.8100477056147,30.1625));
#167246=CARTESIAN_POINT('Origin',(0.,92.7,30.1625));
#167247=CARTESIAN_POINT('',(-2.58635482717236E-16,93.0175,28.0505810132578));
#167248=CARTESIAN_POINT('Origin',(0.,93.0175,30.1625));
#167249=CARTESIAN_POINT('Origin',(-2.58635482717236E-16,92.7,28.0505810132578));
#167250=CARTESIAN_POINT('Origin',(0.,92.3825,30.1625));
#167251=CARTESIAN_POINT('',(-1.16647607618785E-16,92.3825,29.21));
#167252=CARTESIAN_POINT('Origin',(0.,92.3825,30.1625));
#167253=CARTESIAN_POINT('',(-1.16647607618785E-16,93.0175,29.21));
#167254=CARTESIAN_POINT('',(-1.16647607618785E-16,92.3825,29.21));
#167255=CARTESIAN_POINT('Origin',(0.,93.0175,30.1625));
#167256=CARTESIAN_POINT('Origin',(-6.65127195049617E-15,93.0175,29.21));
#167257=CARTESIAN_POINT('Origin',(-6.65127195049617E-15,92.3825,29.21));
#167258=CARTESIAN_POINT('Origin',(0.,85.9309,30.1625));
#167259=CARTESIAN_POINT('Ctrl Pts',(0.253999999996886,85.5163328910989,
23.8933421020026));
#167260=CARTESIAN_POINT('Ctrl Pts',(1.5926629551087,85.9309,24.6662195194906));
#167261=CARTESIAN_POINT('Ctrl Pts',(2.77812499999999,85.9309,25.3506463502227));
#167262=CARTESIAN_POINT('Ctrl Pts',(-2.77812500000002,85.9309,25.3506463502227));
#167263=CARTESIAN_POINT('Ctrl Pts',(-1.59266295510979,85.9309,24.6662195194913));
#167264=CARTESIAN_POINT('Ctrl Pts',(-0.253999999999478,85.5163328910998,
23.8933421020042));
#167265=CARTESIAN_POINT('Origin',(0.,85.9309,30.1625));
#167266=CARTESIAN_POINT('',(5.55625,85.5163328910998,27.2478915035631));
#167267=CARTESIAN_POINT('Ctrl Pts',(5.55625,85.5163328910997,27.2478915035625));
#167268=CARTESIAN_POINT('Ctrl Pts',(5.55625,85.9309,28.7936463385369));
#167269=CARTESIAN_POINT('Ctrl Pts',(5.55625,85.9309,30.1625));
#167270=CARTESIAN_POINT('',(5.30225,85.5163328910999,26.807950598441));
#167271=CARTESIAN_POINT('Ctrl Pts',(5.55625,85.5163328910998,27.2478915035631));
#167272=CARTESIAN_POINT('Ctrl Pts',(5.55624999999999,85.5117377397735,27.2307580232952));
#167273=CARTESIAN_POINT('Ctrl Pts',(5.55538041960567,85.5075216342437,27.2134991357962));
#167274=CARTESIAN_POINT('Ctrl Pts',(5.54634893312311,85.4880734540669,27.1250893893065));
#167275=CARTESIAN_POINT('Ctrl Pts',(5.52304236276573,85.4800084964366,27.0542559989194));
#167276=CARTESIAN_POINT('Ctrl Pts',(5.45333944747927,85.4800084964365,26.9335270082076));
#167277=CARTESIAN_POINT('Ctrl Pts',(5.40364921714652,85.4880734540669,26.8779262310094));
#167278=CARTESIAN_POINT('Ctrl Pts',(5.3315998739855,85.5075216342438,26.8258998610367));
#167279=CARTESIAN_POINT('Ctrl Pts',(5.31708802916729,85.5117377397736,26.816517338575));
#167280=CARTESIAN_POINT('Ctrl Pts',(5.30225,85.5163328910999,26.807950598441));
#167281=CARTESIAN_POINT('Ctrl Pts',(2.77812499999999,85.9309,25.3506463502227));
#167282=CARTESIAN_POINT('Ctrl Pts',(3.96358704489022,85.9309,26.0350731809542));
#167283=CARTESIAN_POINT('Ctrl Pts',(5.30225000000053,85.5163328910998,26.8079505984413));
#167284=CARTESIAN_POINT('Origin',(0.,85.9309,30.1625));
#167285=CARTESIAN_POINT('',(5.30225000000253,85.5163328910991,33.5170494015576));
#167286=CARTESIAN_POINT('Ctrl Pts',(5.30225000000307,85.5163328910989,33.5170494015572));
#167287=CARTESIAN_POINT('Ctrl Pts',(3.96358704489126,85.9309,34.2899268190452));
#167288=CARTESIAN_POINT('Ctrl Pts',(2.77812499999997,85.9309,34.9743536497773));
#167289=CARTESIAN_POINT('',(5.55625,85.5163328910999,33.0771084964365));
#167290=CARTESIAN_POINT('Ctrl Pts',(5.30225000000253,85.5163328910991,33.5170494015576));
#167291=CARTESIAN_POINT('Ctrl Pts',(5.31708802916894,85.5117377397731,33.508482661424));
#167292=CARTESIAN_POINT('Ctrl Pts',(5.33159987398629,85.5075216342435,33.4991001389628));
#167293=CARTESIAN_POINT('Ctrl Pts',(5.40364921714653,85.4880734540669,33.4470737689906));
#167294=CARTESIAN_POINT('Ctrl Pts',(5.45333944747927,85.4800084964366,33.3914729917924));
#167295=CARTESIAN_POINT('Ctrl Pts',(5.52304236276573,85.4800084964366,33.2707440010806));
#167296=CARTESIAN_POINT('Ctrl Pts',(5.54634893312311,85.4880734540668,33.1999106106935));
#167297=CARTESIAN_POINT('Ctrl Pts',(5.55538041960568,85.5075216342437,33.1115008642037));
#167298=CARTESIAN_POINT('Ctrl Pts',(5.55625,85.5117377397736,33.0942419767045));
#167299=CARTESIAN_POINT('Ctrl Pts',(5.55625,85.5163328910999,33.0771084964365));
#167300=CARTESIAN_POINT('Ctrl Pts',(5.55625,85.9309,30.1625));
#167301=CARTESIAN_POINT('Ctrl Pts',(5.55625,85.9309,31.5313536614629));
#167302=CARTESIAN_POINT('Ctrl Pts',(5.55625,85.5163328910997,33.0771084964371));
#167303=CARTESIAN_POINT('Origin',(0.,85.9309,30.1625));
#167304=CARTESIAN_POINT('',(-5.55625,85.5163328910999,33.0771084964365));
#167305=CARTESIAN_POINT('Ctrl Pts',(-5.55625,85.5163328910998,33.0771084964371));
#167306=CARTESIAN_POINT('Ctrl Pts',(-5.55625,85.9309000000001,31.5313536614629));
#167307=CARTESIAN_POINT('Ctrl Pts',(-5.55625,85.9309000000001,30.1625));
#167308=CARTESIAN_POINT('',(-5.30225,85.5163328910999,33.517049401559));
#167309=CARTESIAN_POINT('Ctrl Pts',(-5.55625,85.5163328910999,33.0771084964365));
#167310=CARTESIAN_POINT('Ctrl Pts',(-5.55625,85.5117377397736,33.0942419767045));
#167311=CARTESIAN_POINT('Ctrl Pts',(-5.55538041960568,85.5075216342438,
33.1115008642037));
#167312=CARTESIAN_POINT('Ctrl Pts',(-5.54634893312311,85.4880734540669,
33.1999106106935));
#167313=CARTESIAN_POINT('Ctrl Pts',(-5.52304236276573,85.4800084964366,
33.2707440010806));
#167314=CARTESIAN_POINT('Ctrl Pts',(-5.45333944747927,85.4800084964366,
33.3914729917924));
#167315=CARTESIAN_POINT('Ctrl Pts',(-5.40364921714652,85.4880734540669,
33.4470737689906));
#167316=CARTESIAN_POINT('Ctrl Pts',(-5.33159987398549,85.5075216342438,
33.4991001389633));
#167317=CARTESIAN_POINT('Ctrl Pts',(-5.31708802916729,85.5117377397736,
33.5084826614251));
#167318=CARTESIAN_POINT('Ctrl Pts',(-5.30225,85.5163328910999,33.517049401559));
#167319=CARTESIAN_POINT('Ctrl Pts',(-2.77812499999999,85.9309,34.9743536497773));
#167320=CARTESIAN_POINT('Ctrl Pts',(-3.96358704489021,85.9309,34.2899268190458));
#167321=CARTESIAN_POINT('Ctrl Pts',(-5.30225000000052,85.5163328910997,
33.5170494015587));
#167322=CARTESIAN_POINT('Origin',(0.,85.9309,30.1625));
#167323=CARTESIAN_POINT('',(-5.30225000000253,85.5163328910991,26.8079505984424));
#167324=CARTESIAN_POINT('Ctrl Pts',(-5.30225000000299,85.516332891099,26.8079505984427));
#167325=CARTESIAN_POINT('Ctrl Pts',(-3.96358704489126,85.9309,26.0350731809548));
#167326=CARTESIAN_POINT('Ctrl Pts',(-2.77812500000002,85.9309,25.3506463502227));
#167327=CARTESIAN_POINT('',(-5.55625,85.5163328910998,27.2478915035631));
#167328=CARTESIAN_POINT('Ctrl Pts',(-5.30225000000253,85.5163328910991,
26.8079505984424));
#167329=CARTESIAN_POINT('Ctrl Pts',(-5.31708802916895,85.5117377397731,
26.816517338576));
#167330=CARTESIAN_POINT('Ctrl Pts',(-5.3315998739863,85.5075216342435,26.8258998610372));
#167331=CARTESIAN_POINT('Ctrl Pts',(-5.40364921714653,85.4880734540668,
26.8779262310094));
#167332=CARTESIAN_POINT('Ctrl Pts',(-5.45333944747927,85.4800084964366,
26.9335270082076));
#167333=CARTESIAN_POINT('Ctrl Pts',(-5.52304236276573,85.4800084964366,
27.0542559989194));
#167334=CARTESIAN_POINT('Ctrl Pts',(-5.54634893312311,85.4880734540668,
27.1250893893065));
#167335=CARTESIAN_POINT('Ctrl Pts',(-5.55538041960567,85.5075216342437,
27.2134991357962));
#167336=CARTESIAN_POINT('Ctrl Pts',(-5.55624999999999,85.5117377397735,
27.2307580232952));
#167337=CARTESIAN_POINT('Ctrl Pts',(-5.55625,85.5163328910998,27.2478915035631));
#167338=CARTESIAN_POINT('Ctrl Pts',(-5.55625,85.9309000000001,30.1625));
#167339=CARTESIAN_POINT('Ctrl Pts',(-5.55625,85.9309000000001,28.7936463385369));
#167340=CARTESIAN_POINT('Ctrl Pts',(-5.55625,85.5163328910997,27.2478915035624));
#167341=CARTESIAN_POINT('Origin',(-3.59168685326793E-14,76.444,25.019));
#167342=CARTESIAN_POINT('Origin',(-3.87990863778943E-14,81.9939,24.60625));
#167343=CARTESIAN_POINT('',(5.55625,81.9939,30.1625));
#167344=CARTESIAN_POINT('Origin',(0.,81.9939,30.1625));
#167345=CARTESIAN_POINT('',(2.778125,81.9939,34.9743536497773));
#167346=CARTESIAN_POINT('Origin',(0.,81.9939,30.1625));
#167347=CARTESIAN_POINT('',(-2.778125,81.9939,34.9743536497773));
#167348=CARTESIAN_POINT('Origin',(0.,81.9939,30.1625));
#167349=CARTESIAN_POINT('',(-5.55625,81.9939,30.1625));
#167350=CARTESIAN_POINT('Origin',(0.,81.9939,30.1625));
#167351=CARTESIAN_POINT('Origin',(0.,81.9939,30.1625));
#167352=CARTESIAN_POINT('Origin',(0.,81.9939,30.1625));
#167353=CARTESIAN_POINT('',(-5.55625,82.4084671089002,27.2478915035631));
#167354=CARTESIAN_POINT('Ctrl Pts',(-5.55625,82.4084671089004,27.2478915035625));
#167355=CARTESIAN_POINT('Ctrl Pts',(-5.55625,81.9939,28.793646338537));
#167356=CARTESIAN_POINT('Ctrl Pts',(-5.55625,81.9939,30.1625000000001));
#167357=CARTESIAN_POINT('',(-5.30225,82.4084671089001,26.807950598441));
#167358=CARTESIAN_POINT('Ctrl Pts',(-5.55625,82.4084671089002,27.2478915035631));
#167359=CARTESIAN_POINT('Ctrl Pts',(-5.55624999999999,82.4130622602265,
27.2307580232952));
#167360=CARTESIAN_POINT('Ctrl Pts',(-5.55538041960567,82.4172783657563,
27.2134991357962));
#167361=CARTESIAN_POINT('Ctrl Pts',(-5.54634893312311,82.4367265459332,
27.1250893893065));
#167362=CARTESIAN_POINT('Ctrl Pts',(-5.52304236276573,82.4447915035635,
27.0542559989194));
#167363=CARTESIAN_POINT('Ctrl Pts',(-5.45333944747927,82.4447915035635,
26.9335270082076));
#167364=CARTESIAN_POINT('Ctrl Pts',(-5.40364921714653,82.4367265459332,
26.8779262310094));
#167365=CARTESIAN_POINT('Ctrl Pts',(-5.3315998739855,82.4172783657563,26.8258998610367));
#167366=CARTESIAN_POINT('Ctrl Pts',(-5.3170880291673,82.4130622602264,26.816517338575));
#167367=CARTESIAN_POINT('Ctrl Pts',(-5.30225000000001,82.4084671089001,
26.807950598441));
#167368=CARTESIAN_POINT('Ctrl Pts',(-2.77812500000003,81.9939,25.3506463502227));
#167369=CARTESIAN_POINT('Ctrl Pts',(-3.96358704489024,81.9939,26.0350731809542));
#167370=CARTESIAN_POINT('Ctrl Pts',(-5.30225000000053,82.4084671089003,
26.8079505984413));
#167371=CARTESIAN_POINT('Origin',(0.,81.9939,30.1625));
#167372=CARTESIAN_POINT('',(-5.30225000000254,82.4084671089009,33.5170494015576));
#167373=CARTESIAN_POINT('Ctrl Pts',(-5.30225000000307,82.4084671089011,
33.5170494015573));
#167374=CARTESIAN_POINT('Ctrl Pts',(-3.96358704489128,81.9939,34.2899268190452));
#167375=CARTESIAN_POINT('Ctrl Pts',(-2.778125,81.9939,34.9743536497773));
#167376=CARTESIAN_POINT('',(-5.55625,82.4084671089001,33.0771084964365));
#167377=CARTESIAN_POINT('Ctrl Pts',(-5.30225000000254,82.4084671089009,
33.5170494015576));
#167378=CARTESIAN_POINT('Ctrl Pts',(-5.31708802916895,82.4130622602269,
33.508482661424));
#167379=CARTESIAN_POINT('Ctrl Pts',(-5.33159987398629,82.4172783657565,
33.4991001389628));
#167380=CARTESIAN_POINT('Ctrl Pts',(-5.40364921714652,82.4367265459332,
33.4470737689906));
#167381=CARTESIAN_POINT('Ctrl Pts',(-5.45333944747927,82.4447915035635,
33.3914729917924));
#167382=CARTESIAN_POINT('Ctrl Pts',(-5.52304236276573,82.4447915035635,
33.2707440010806));
#167383=CARTESIAN_POINT('Ctrl Pts',(-5.54634893312311,82.4367265459332,
33.1999106106935));
#167384=CARTESIAN_POINT('Ctrl Pts',(-5.55538041960568,82.4172783657563,
33.1115008642037));
#167385=CARTESIAN_POINT('Ctrl Pts',(-5.55625,82.4130622602264,33.0942419767045));
#167386=CARTESIAN_POINT('Ctrl Pts',(-5.55625,82.4084671089001,33.0771084964365));
#167387=CARTESIAN_POINT('Ctrl Pts',(-5.55625,81.9939,30.1625000000001));
#167388=CARTESIAN_POINT('Ctrl Pts',(-5.55625,81.9939,31.531353661463));
#167389=CARTESIAN_POINT('Ctrl Pts',(-5.55625,82.4084671089003,33.0771084964372));
#167390=CARTESIAN_POINT('Origin',(0.,81.9939,30.1625));
#167391=CARTESIAN_POINT('',(0.253999999997469,82.4084671089009,36.431657897997));
#167392=CARTESIAN_POINT('Ctrl Pts',(0.253999999996946,82.4084671089011,
36.4316578979973));
#167393=CARTESIAN_POINT('Ctrl Pts',(1.59266295510873,81.9939,35.6587804805093));
#167394=CARTESIAN_POINT('Ctrl Pts',(2.77812500000001,81.9939,34.9743536497773));
#167395=CARTESIAN_POINT('',(-0.253999999999999,82.4084671089001,36.4316578979955));
#167396=CARTESIAN_POINT('Ctrl Pts',(0.253999999997469,82.4084671089009,
36.431657897997));
#167397=CARTESIAN_POINT('Ctrl Pts',(0.239161970830958,82.4130622602269,
36.4402246381304));
#167398=CARTESIAN_POINT('Ctrl Pts',(0.22378054561929,82.4172783657565,36.4481010031674));
#167399=CARTESIAN_POINT('Ctrl Pts',(0.142699715976588,82.4367265459332,
36.4844843796841));
#167400=CARTESIAN_POINT('Ctrl Pts',(0.0697029152864558,82.4447915035635,
36.4997169928731));
#167401=CARTESIAN_POINT('Ctrl Pts',(-0.0697029152864573,82.4447915035635,
36.4997169928731));
#167402=CARTESIAN_POINT('Ctrl Pts',(-0.142699715976586,82.4367265459332,
36.4844843796841));
#167403=CARTESIAN_POINT('Ctrl Pts',(-0.223780545620187,82.4172783657563,
36.448101003167));
#167404=CARTESIAN_POINT('Ctrl Pts',(-0.239161970832704,82.4130622602264,
36.4402246381295));
#167405=CARTESIAN_POINT('Ctrl Pts',(-0.253999999999999,82.4084671089001,
36.4316578979955));
#167406=CARTESIAN_POINT('Ctrl Pts',(-2.778125,81.9939,34.9743536497773));
#167407=CARTESIAN_POINT('Ctrl Pts',(-1.59266295510978,81.9939,35.6587804805087));
#167408=CARTESIAN_POINT('Ctrl Pts',(-0.253999999999474,82.4084671089003,
36.4316578979959));
#167409=CARTESIAN_POINT('Origin',(0.,81.9939,30.1625));
#167410=CARTESIAN_POINT('',(5.55625,82.4084671089001,33.0771084964365));
#167411=CARTESIAN_POINT('Ctrl Pts',(5.55625,82.4084671089003,33.0771084964372));
#167412=CARTESIAN_POINT('Ctrl Pts',(5.55625,81.9939,31.5313536614629));
#167413=CARTESIAN_POINT('Ctrl Pts',(5.55625,81.9939,30.1625));
#167414=CARTESIAN_POINT('',(5.30225000000001,82.4084671089001,33.517049401559));
#167415=CARTESIAN_POINT('Ctrl Pts',(5.55625,82.4084671089001,33.0771084964365));
#167416=CARTESIAN_POINT('Ctrl Pts',(5.55625,82.4130622602264,33.0942419767045));
#167417=CARTESIAN_POINT('Ctrl Pts',(5.55538041960568,82.4172783657563,33.1115008642037));
#167418=CARTESIAN_POINT('Ctrl Pts',(5.54634893312311,82.4367265459332,33.1999106106935));
#167419=CARTESIAN_POINT('Ctrl Pts',(5.52304236276573,82.4447915035635,33.2707440010806));
#167420=CARTESIAN_POINT('Ctrl Pts',(5.45333944747927,82.4447915035635,33.3914729917924));
#167421=CARTESIAN_POINT('Ctrl Pts',(5.40364921714653,82.4367265459332,33.4470737689906));
#167422=CARTESIAN_POINT('Ctrl Pts',(5.3315998739855,82.4172783657563,33.4991001389633));
#167423=CARTESIAN_POINT('Ctrl Pts',(5.3170880291673,82.4130622602264,33.508482661425));
#167424=CARTESIAN_POINT('Ctrl Pts',(5.30225000000001,82.4084671089001,33.517049401559));
#167425=CARTESIAN_POINT('Ctrl Pts',(2.77812500000001,81.9939,34.9743536497773));
#167426=CARTESIAN_POINT('Ctrl Pts',(3.96358704489023,81.9939,34.2899268190458));
#167427=CARTESIAN_POINT('Ctrl Pts',(5.30225000000053,82.4084671089003,33.5170494015587));
#167428=CARTESIAN_POINT('Origin',(0.,81.9939,30.1625));
#167429=CARTESIAN_POINT('',(5.30225000000253,82.4084671089009,26.8079505984424));
#167430=CARTESIAN_POINT('Ctrl Pts',(5.30225000000308,82.4084671089011,26.8079505984428));
#167431=CARTESIAN_POINT('Ctrl Pts',(3.96358704489129,81.9939,26.0350731809548));
#167432=CARTESIAN_POINT('Ctrl Pts',(2.77812500000002,81.9939,25.3506463502227));
#167433=CARTESIAN_POINT('',(5.55625,82.4084671089002,27.2478915035631));
#167434=CARTESIAN_POINT('Ctrl Pts',(5.30225000000254,82.4084671089009,26.8079505984424));
#167435=CARTESIAN_POINT('Ctrl Pts',(5.31708802916896,82.4130622602269,26.816517338576));
#167436=CARTESIAN_POINT('Ctrl Pts',(5.33159987398629,82.4172783657565,26.8258998610373));
#167437=CARTESIAN_POINT('Ctrl Pts',(5.40364921714653,82.4367265459332,26.8779262310094));
#167438=CARTESIAN_POINT('Ctrl Pts',(5.45333944747927,82.4447915035635,26.9335270082076));
#167439=CARTESIAN_POINT('Ctrl Pts',(5.52304236276573,82.4447915035635,27.0542559989194));
#167440=CARTESIAN_POINT('Ctrl Pts',(5.54634893312311,82.4367265459332,27.1250893893065));
#167441=CARTESIAN_POINT('Ctrl Pts',(5.55538041960567,82.4172783657563,27.2134991357962));
#167442=CARTESIAN_POINT('Ctrl Pts',(5.55624999999999,82.4130622602265,27.2307580232952));
#167443=CARTESIAN_POINT('Ctrl Pts',(5.55625,82.4084671089002,27.2478915035631));
#167444=CARTESIAN_POINT('Ctrl Pts',(5.55625,81.9939,30.1625));
#167445=CARTESIAN_POINT('Ctrl Pts',(5.55625,81.9939,28.7936463385369));
#167446=CARTESIAN_POINT('Ctrl Pts',(5.55625,82.4084671089004,27.2478915035625));
#167447=CARTESIAN_POINT('Origin',(0.,85.9309,23.7466951336303));
#167448=CARTESIAN_POINT('',(5.30225,85.9309,26.807950598441));
#167449=CARTESIAN_POINT('Origin',(5.55625,85.9309,26.9545975668151));
#167450=CARTESIAN_POINT('',(5.55625,85.9309,27.2478915035635));
#167451=CARTESIAN_POINT('',(5.55625,85.9309,33.0771084964365));
#167452=CARTESIAN_POINT('Origin',(0.,85.9309,36.5783048663697));
#167453=CARTESIAN_POINT('',(5.30225,85.9309,33.517049401559));
#167454=CARTESIAN_POINT('',(0.254000000000001,85.9309,36.4316578979955));
#167455=CARTESIAN_POINT('Origin',(-5.55625,85.9309,33.3704024331849));
#167456=CARTESIAN_POINT('',(-5.30225,85.9309,33.517049401559));
#167457=CARTESIAN_POINT('',(-0.254000000000001,85.9309,36.4316578979955));
#167458=CARTESIAN_POINT('Origin',(-5.55625,85.9309,26.9545975668151));
#167459=CARTESIAN_POINT('',(-5.55625,85.9309,27.2478915035635));
#167460=CARTESIAN_POINT('',(-5.55625,85.9309,33.0771084964365));
#167461=CARTESIAN_POINT('Origin',(-5.55625,85.9309,26.9545975668151));
#167462=CARTESIAN_POINT('',(-5.30225,85.9309,26.807950598441));
#167463=CARTESIAN_POINT('Origin',(5.04825,85.9309,27.2478915035635));
#167464=CARTESIAN_POINT('Origin',(-5.04825,85.9309,27.2478915035635));
#167465=CARTESIAN_POINT('Origin',(-5.04825,85.9309,33.0771084964365));
#167466=CARTESIAN_POINT('Origin',(5.04825,85.9309,33.0771084964365));
#167467=CARTESIAN_POINT('Origin',(-6.50521303491303E-16,85.9309,35.9917169928731));
#167468=CARTESIAN_POINT('Origin',(90.,90.,41.3499812820439));
#167469=CARTESIAN_POINT('',(97.9375,90.,17.4625));
#167470=CARTESIAN_POINT('Origin',(90.,90.,17.4625));
#167471=CARTESIAN_POINT('',(97.9375,90.,3.17499999999999));
#167472=CARTESIAN_POINT('',(97.9375,90.,41.3499812820439));
#167473=CARTESIAN_POINT('Origin',(90.,90.,3.175));
#167474=CARTESIAN_POINT('Origin',(90.,90.,41.3499812820439));
#167475=CARTESIAN_POINT('',(98.4455,90.,3.175));
#167476=CARTESIAN_POINT('Origin',(90.,90.,3.175));
#167477=CARTESIAN_POINT('',(98.4455,90.,17.4625));
#167478=CARTESIAN_POINT('',(98.4455,90.,41.3499812820439));
#167479=CARTESIAN_POINT('Origin',(90.,90.,17.4625));
#167480=CARTESIAN_POINT('Origin',(90.,90.,3.175));
#167481=CARTESIAN_POINT('Origin',(-90.,-90.,17.4625));
#167482=CARTESIAN_POINT('Origin',(-90.,90.,41.3499812820439));
#167483=CARTESIAN_POINT('',(-82.0625,90.,17.4625));
#167484=CARTESIAN_POINT('Origin',(-90.,90.,17.4625));
#167485=CARTESIAN_POINT('',(-82.0625,90.,3.17499999999999));
#167486=CARTESIAN_POINT('',(-82.0625,90.,41.3499812820439));
#167487=CARTESIAN_POINT('Origin',(-90.,90.,3.175));
#167488=CARTESIAN_POINT('Origin',(-90.,90.,41.3499812820439));
#167489=CARTESIAN_POINT('',(-81.5545,90.,3.175));
#167490=CARTESIAN_POINT('Origin',(-90.,90.,3.175));
#167491=CARTESIAN_POINT('',(-81.5545,90.,17.4625));
#167492=CARTESIAN_POINT('',(-81.5545,90.,41.3499812820439));
#167493=CARTESIAN_POINT('Origin',(-90.,90.,17.4625));
#167494=CARTESIAN_POINT('Origin',(-90.,90.,3.175));
#167495=CARTESIAN_POINT('Origin',(-90.,-90.,17.4625));
#167496=CARTESIAN_POINT('Origin',(-90.,-90.,41.3499812820439));
#167497=CARTESIAN_POINT('',(-82.0625,-90.,17.4625));
#167498=CARTESIAN_POINT('Origin',(-90.,-90.,17.4625));
#167499=CARTESIAN_POINT('',(-82.0625,-90.,3.17499999999999));
#167500=CARTESIAN_POINT('',(-82.0625,-90.,41.3499812820439));
#167501=CARTESIAN_POINT('Origin',(-90.,-90.,3.175));
#167502=CARTESIAN_POINT('Origin',(-90.,-90.,41.3499812820439));
#167503=CARTESIAN_POINT('',(-81.5545,-90.,3.175));
#167504=CARTESIAN_POINT('Origin',(-90.,-90.,3.175));
#167505=CARTESIAN_POINT('',(-81.5545,-90.,17.4625));
#167506=CARTESIAN_POINT('',(-81.5545,-90.,41.3499812820439));
#167507=CARTESIAN_POINT('Origin',(-90.,-90.,17.4625));
#167508=CARTESIAN_POINT('Origin',(-90.,-90.,3.175));
#167509=CARTESIAN_POINT('Origin',(-90.,-90.,17.4625));
#167510=CARTESIAN_POINT('Origin',(90.,-90.,41.3499812820439));
#167511=CARTESIAN_POINT('',(97.9375,-90.,17.4625));
#167512=CARTESIAN_POINT('Origin',(90.,-90.,17.4625));
#167513=CARTESIAN_POINT('',(97.9375,-90.,3.17499999999999));
#167514=CARTESIAN_POINT('',(97.9375,-90.,41.3499812820439));
#167515=CARTESIAN_POINT('Origin',(90.,-90.,3.175));
#167516=CARTESIAN_POINT('Origin',(90.,-90.,41.3499812820439));
#167517=CARTESIAN_POINT('',(98.4455,-90.,3.175));
#167518=CARTESIAN_POINT('Origin',(90.,-90.,3.175));
#167519=CARTESIAN_POINT('',(98.4455,-90.,17.4625));
#167520=CARTESIAN_POINT('',(98.4455,-90.,41.3499812820439));
#167521=CARTESIAN_POINT('Origin',(90.,-90.,17.4625));
#167522=CARTESIAN_POINT('Origin',(90.,-90.,3.175));
#167523=CARTESIAN_POINT('Origin',(-90.,-90.,17.4625));
#167524=CARTESIAN_POINT('Origin',(-1.38777878078145E-14,-1.38777878078145E-14,
2.79399999999999));
#167525=CARTESIAN_POINT('',(-50.,-7.75455381207769E-15,2.79399999999999));
#167526=CARTESIAN_POINT('',(50.,-2.00010218035512E-14,2.79399999999999));
#167527=CARTESIAN_POINT('Origin',(-1.38777878078145E-14,-1.38777878078145E-14,
2.79399999999999));
#167528=CARTESIAN_POINT('Origin',(-1.38777878078145E-14,-1.38777878078145E-14,
2.79399999999999));
#167529=CARTESIAN_POINT('',(50.254,-2.00321278322496E-14,2.54));
#167530=CARTESIAN_POINT('Origin',(50.254,-2.00321278322496E-14,2.79399999999999));
#167531=CARTESIAN_POINT('Origin',(-1.38777878078145E-14,-1.38777878078145E-14,
2.54));
#167532=CARTESIAN_POINT('Origin',(-1.38777878078145E-14,-1.38777878078145E-14,
2.79399999999999));
#167533=CARTESIAN_POINT('',(51.016,-2.01254459183446E-14,2.54));
#167534=CARTESIAN_POINT('Origin',(-1.38777878078145E-14,-1.38777878078145E-14,
2.54));
#167535=CARTESIAN_POINT('',(51.27,-2.01565519470429E-14,2.79399999999999));
#167536=CARTESIAN_POINT('Origin',(51.016,-2.01254459183446E-14,2.79399999999999));
#167537=CARTESIAN_POINT('',(-51.27,-7.59902366858598E-15,2.79399999999999));
#167538=CARTESIAN_POINT('Origin',(-1.38777878078145E-14,-1.38777878078145E-14,
2.79399999999999));
#167539=CARTESIAN_POINT('Origin',(-1.38777878078145E-14,-1.38777878078145E-14,
2.79399999999999));
#167540=CARTESIAN_POINT('Origin',(-1.38777878078145E-14,-1.38777878078145E-14,
-158.32679271994));
#167541=CARTESIAN_POINT('',(-51.27,-2.01565519470429E-14,17.4625));
#167542=CARTESIAN_POINT('Origin',(-1.38777878078145E-14,-1.38777878078145E-14,
17.4625));
#167543=CARTESIAN_POINT('',(-51.27,-2.01565519470429E-14,-158.32679271994));
#167544=CARTESIAN_POINT('Origin',(-1.38777878078145E-14,-1.38777878078145E-14,
-158.32679271994));
#167545=CARTESIAN_POINT('',(-50.,-2.00010218035512E-14,17.4625));
#167546=CARTESIAN_POINT('',(-50.,-2.00010218035512E-14,-158.32679271994));
#167547=CARTESIAN_POINT('Origin',(-1.38777878078145E-14,-1.38777878078145E-14,
17.4625));
#167548=CARTESIAN_POINT('Origin',(0.,0.,17.4625));
#167549=CARTESIAN_POINT('Origin',(-90.,-90.,2.54));
#167550=CARTESIAN_POINT('Origin',(-1.38777878078145E-14,-1.38777878078145E-14,
2.79399999999999));
#167551=CARTESIAN_POINT('',(56.621,-2.08118604492667E-14,2.54));
#167552=CARTESIAN_POINT('Origin',(-1.38777878078145E-14,-1.38777878078145E-14,
2.54));
#167553=CARTESIAN_POINT('',(56.875,-2.0842966477965E-14,2.79399999999999));
#167554=CARTESIAN_POINT('Origin',(56.621,-2.08118604492667E-14,2.79399999999999));
#167555=CARTESIAN_POINT('',(-56.875,-6.91260913766388E-15,2.79399999999999));
#167556=CARTESIAN_POINT('Origin',(-1.38777878078145E-14,-1.38777878078145E-14,
2.79399999999999));
#167557=CARTESIAN_POINT('Origin',(-1.38777878078145E-14,-1.38777878078145E-14,
2.79399999999999));
#167558=CARTESIAN_POINT('Origin',(-1.38777878078145E-14,-1.38777878078145E-14,
2.79399999999999));
#167559=CARTESIAN_POINT('',(-55.605,-7.0681392811556E-15,2.79399999999999));
#167560=CARTESIAN_POINT('',(55.605,-2.06874363344733E-14,2.79399999999999));
#167561=CARTESIAN_POINT('Origin',(-1.38777878078145E-14,-1.38777878078145E-14,
2.79399999999999));
#167562=CARTESIAN_POINT('Origin',(-1.38777878078145E-14,-1.38777878078145E-14,
2.79399999999999));
#167563=CARTESIAN_POINT('',(55.859,-2.07185423631717E-14,2.54));
#167564=CARTESIAN_POINT('Origin',(55.859,-2.07185423631717E-14,2.79399999999999));
#167565=CARTESIAN_POINT('Origin',(-1.38777878078145E-14,-1.38777878078145E-14,
2.54));
#167566=CARTESIAN_POINT('Origin',(-1.38777878078145E-14,-1.38777878078145E-14,
-158.32679271994));
#167567=CARTESIAN_POINT('',(-56.875,-2.0842966477965E-14,17.4625));
#167568=CARTESIAN_POINT('Origin',(-1.38777878078145E-14,-1.38777878078145E-14,
17.4625));
#167569=CARTESIAN_POINT('',(-56.875,-2.0842966477965E-14,-158.32679271994));
#167570=CARTESIAN_POINT('Origin',(-1.38777878078145E-14,-1.38777878078145E-14,
-158.32679271994));
#167571=CARTESIAN_POINT('',(-55.605,-2.06874363344733E-14,17.4625));
#167572=CARTESIAN_POINT('',(-55.605,-2.06874363344733E-14,-158.32679271994));
#167573=CARTESIAN_POINT('Origin',(-1.38777878078145E-14,-1.38777878078145E-14,
17.4625));
#167574=CARTESIAN_POINT('Origin',(0.,0.,17.4625));
#167575=CARTESIAN_POINT('Origin',(-90.,-90.,2.54));
#167576=CARTESIAN_POINT('Origin',(-1.38777878078145E-14,-1.38777878078145E-14,
-154.734690271512));
#167577=CARTESIAN_POINT('',(-51.27,-2.01565519470429E-14,2.53999999999998));
#167578=CARTESIAN_POINT('Origin',(-1.38777878078145E-14,-1.38777878078145E-14,
2.53999999999999));
#167579=CARTESIAN_POINT('',(-51.27,-2.01565519470429E-14,17.4625));
#167580=CARTESIAN_POINT('',(-51.27,-2.01565519470429E-14,-154.734690271512));
#167581=CARTESIAN_POINT('Origin',(-1.38777878078145E-14,-1.38777878078145E-14,
17.4625));
#167582=CARTESIAN_POINT('Origin',(-1.38777878078145E-14,-1.38777878078145E-14,
-154.734690271512));
#167583=CARTESIAN_POINT('',(-55.605,-2.06874363344733E-14,17.4625));
#167584=CARTESIAN_POINT('Origin',(-1.38777878078145E-14,-1.38777878078145E-14,
17.4625));
#167585=CARTESIAN_POINT('',(-55.605,-2.06874363344733E-14,2.53999999999998));
#167586=CARTESIAN_POINT('',(-55.605,-2.06874363344733E-14,-154.734690271512));
#167587=CARTESIAN_POINT('Origin',(-1.38777878078145E-14,-1.38777878078145E-14,
2.53999999999999));
#167588=CARTESIAN_POINT('Origin',(-1.38777878078145E-14,-1.38777878078145E-14,
17.4625));
#167589=CARTESIAN_POINT('Origin',(-90.,-90.,2.54));
#167590=CARTESIAN_POINT('Origin',(5.66467691768715E-15,5.31136514129714E-15,
40.22725));
#167591=CARTESIAN_POINT('',(-0.0152399999993761,59.0285534841296,40.10025));
#167592=CARTESIAN_POINT('',(0.0152400000006239,59.0285534841296,40.10025));
#167593=CARTESIAN_POINT('Origin',(5.64679317051214E-15,5.32924888847216E-15,
40.10025));
#167594=CARTESIAN_POINT('',(-0.015212193455297,58.9208513795073,40.1599502534424));
#167595=CARTESIAN_POINT('Origin',(-0.015239999999376,59.0285534841296,40.22725));
#167596=CARTESIAN_POINT('',(0.0152121934565426,58.9208513795073,40.1599502534424));
#167597=CARTESIAN_POINT('Origin',(5.65519997554244E-15,5.32084208344186E-15,
40.1599502534424));
#167598=CARTESIAN_POINT('Origin',(0.0152400000006239,59.0285534841296,40.22725));
#167599=CARTESIAN_POINT('Origin',(5.66467691768715E-15,5.52999499151977E-15,
40.22725));
#167600=CARTESIAN_POINT('',(-0.0152661173102018,62.9541448057648,40.1599502534424));
#167601=CARTESIAN_POINT('',(0.0152661173115319,62.9541448057648,40.1599502534424));
#167602=CARTESIAN_POINT('Origin',(5.65519997554243E-15,5.53947193366449E-15,
40.1599502534424));
#167603=CARTESIAN_POINT('',(-0.0152399999993361,62.8464427007196,40.10025));
#167604=CARTESIAN_POINT('Origin',(-0.015239999999336,62.8464427007196,40.22725));
#167605=CARTESIAN_POINT('',(0.0152400000006639,62.8464427007196,40.10025));
#167606=CARTESIAN_POINT('Origin',(5.64679317051213E-15,5.54787873869479E-15,
40.10025));
#167607=CARTESIAN_POINT('Origin',(0.0152400000006639,62.8464427007196,40.22725));
#167608=CARTESIAN_POINT('Origin',(3.5331177639001E-16,0.,40.22725));
#167609=CARTESIAN_POINT('',(-59.0285534841296,-0.01524,40.10025));
#167610=CARTESIAN_POINT('',(-59.0285534841296,0.01524,40.10025));
#167611=CARTESIAN_POINT('Origin',(3.17544282039971E-16,0.,40.10025));
#167612=CARTESIAN_POINT('',(-58.9208513795073,-0.0152121934559198,40.1599502534424));
#167613=CARTESIAN_POINT('Origin',(-59.0285534841296,-0.01524,40.22725));
#167614=CARTESIAN_POINT('',(-58.9208513795073,0.0152121934559198,40.1599502534424));
#167615=CARTESIAN_POINT('Origin',(3.34357892100574E-16,0.,40.1599502534424));
#167616=CARTESIAN_POINT('Origin',(-59.0285534841296,0.01524,40.22725));
#167617=CARTESIAN_POINT('Origin',(1.34681926167381E-16,0.,40.22725));
#167618=CARTESIAN_POINT('',(-62.9541448057648,-0.0152661173108668,40.1599502534424));
#167619=CARTESIAN_POINT('',(-62.9541466567496,-7.70965941962415E-15,40.1599502534424));
#167620=CARTESIAN_POINT('Origin',(1.15728041877948E-16,0.,40.1599502534424));
#167621=CARTESIAN_POINT('',(-62.8464427007196,-0.01524,40.10025));
#167622=CARTESIAN_POINT('Origin',(-62.8464427007196,-0.01524,40.22725));
#167623=CARTESIAN_POINT('',(-62.8464427007196,0.01524,40.10025));
#167624=CARTESIAN_POINT('Origin',(9.89144318173425E-17,0.,40.10025));
#167625=CARTESIAN_POINT('',(-62.9541448057648,0.0152661173108668,40.1599502534424));
#167626=CARTESIAN_POINT('Origin',(-62.8464427007196,0.01524,40.22725));
#167627=CARTESIAN_POINT('Origin',(1.15728041877948E-16,0.,40.1599502534424));
#167628=CARTESIAN_POINT('Origin',(5.62443848654336E-15,0.,39.9415));
#167629=CARTESIAN_POINT('',(58.2189663438286,-7.12976707826372E-15,40.5765));
#167630=CARTESIAN_POINT('Origin',(5.71385722241845E-15,0.,40.5765));
#167631=CARTESIAN_POINT('',(57.6804558027693,-7.06381855722217E-15,40.2779987327881));
#167632=CARTESIAN_POINT('Origin',(58.2189663438286,-7.12976707826372E-15,
39.9415));
#167633=CARTESIAN_POINT('',(-57.6804558027693,7.06381855722218E-15,40.2779987327881));
#167634=CARTESIAN_POINT('Origin',(5.67182319726696E-15,0.,40.2779987327881));
#167635=CARTESIAN_POINT('Origin',(5.67182319726696E-15,0.,40.2779987327881));
#167636=CARTESIAN_POINT('Origin',(5.62443848654336E-15,0.,39.9415));
#167637=CARTESIAN_POINT('',(58.8470884664677,-7.20668985296008E-15,40.2779987327881));
#167638=CARTESIAN_POINT('Origin',(5.67182319726695E-15,0.,40.2779987327881));
#167639=CARTESIAN_POINT('',(58.3085779254084,-7.14074133191854E-15,40.5765));
#167640=CARTESIAN_POINT('Origin',(58.3085779254084,-7.14074133191854E-15,
39.9415));
#167641=CARTESIAN_POINT('Origin',(5.71385722241845E-15,0.,40.5765));
#167642=CARTESIAN_POINT('Origin',(5.62443848654336E-15,0.,39.9415));
#167643=CARTESIAN_POINT('',(63.5664220745916,-7.78464153268983E-15,40.5765));
#167644=CARTESIAN_POINT('Origin',(5.71385722241845E-15,0.,40.5765));
#167645=CARTESIAN_POINT('',(63.0279115335323,-7.71869301164828E-15,40.2779987327881));
#167646=CARTESIAN_POINT('Origin',(63.5664220745916,-7.78464153268983E-15,
39.9415));
#167647=CARTESIAN_POINT('',(-63.0279115335323,7.71869301164829E-15,40.2779987327881));
#167648=CARTESIAN_POINT('Origin',(5.67182319726696E-15,0.,40.2779987327881));
#167649=CARTESIAN_POINT('Origin',(5.67182319726696E-15,0.,40.2779987327881));
#167650=CARTESIAN_POINT('Origin',(5.62443848654336E-15,0.,39.9415));
#167651=CARTESIAN_POINT('',(64.1945441972308,-7.8615643073862E-15,40.2779987327881));
#167652=CARTESIAN_POINT('Origin',(5.67182319726695E-15,0.,40.2779987327881));
#167653=CARTESIAN_POINT('',(63.6560336561714,-7.79561578634465E-15,40.5765));
#167654=CARTESIAN_POINT('Origin',(63.6560336561714,-7.79561578634465E-15,
39.9415));
#167655=CARTESIAN_POINT('Origin',(5.71385722241845E-15,0.,40.5765));
#167656=CARTESIAN_POINT('Origin',(0.,0.,0.));
#167657=CARTESIAN_POINT('',(65.,-7.96020419445779E-15,38.6715));
#167658=CARTESIAN_POINT('Origin',(5.44560101479317E-15,0.,38.6715));
#167659=CARTESIAN_POINT('',(65.,-7.96020419445779E-15,38.989));
#167660=CARTESIAN_POINT('',(65.,-7.96020419445779E-15,-9.15309894784418E-15));
#167661=CARTESIAN_POINT('Origin',(5.49031038273072E-15,0.,38.989));
#167662=CARTESIAN_POINT('Origin',(5.71385722241845E-15,0.,40.5765));
#167663=CARTESIAN_POINT('',(64.008019903844,-7.83872166950026E-15,40.5765));
#167664=CARTESIAN_POINT('Origin',(5.49031038273072E-15,0.,38.989));
#167665=CARTESIAN_POINT('',(62.9541448057648,0.0152661173108668,40.1599502534424));
#167666=CARTESIAN_POINT('',(62.9541448057648,-0.0152661173108668,40.1599502534424));
#167667=CARTESIAN_POINT('Origin',(-1.95097259456047E-16,0.,40.1599502534424));
#167668=CARTESIAN_POINT('',(62.7644678366119,-0.318045750793045,39.8576902534424));
#167669=CARTESIAN_POINT('Ctrl Pts',(62.9541448057648,-0.0152661173108668,
40.1599502534424));
#167670=CARTESIAN_POINT('Ctrl Pts',(62.9541438736292,-0.019087735244646,
40.1599502447858));
#167671=CARTESIAN_POINT('Ctrl Pts',(62.9540952129414,-0.0228988721022198,
40.1598744685927));
#167672=CARTESIAN_POINT('Ctrl Pts',(62.9539999459718,-0.0266975986403399,
40.1597246934279));
#167673=CARTESIAN_POINT('Ctrl Pts',(62.953449420412,-0.0486495517930185,
40.1588591777434));
#167674=CARTESIAN_POINT('Ctrl Pts',(62.9513443281453,-0.0701898812469889,
40.1555254706015));
#167675=CARTESIAN_POINT('Ctrl Pts',(62.9479003565106,-0.0909392844447056,
40.1500631826367));
#167676=CARTESIAN_POINT('Ctrl Pts',(62.9465113235258,-0.0993079960697583,
40.1478601162471));
#167677=CARTESIAN_POINT('Ctrl Pts',(62.9449047668209,-0.107548428339421,
40.1453112228301));
#167678=CARTESIAN_POINT('Ctrl Pts',(62.9430957254317,-0.115637319282189,
40.1424401896328));
#167679=CARTESIAN_POINT('Ctrl Pts',(62.9424282989905,-0.118621628943446,
40.1413809526906));
#167680=CARTESIAN_POINT('Ctrl Pts',(62.9417332466658,-0.121585194085533,
40.1402777640512));
#167681=CARTESIAN_POINT('Ctrl Pts',(62.941011293136,-0.124526788072755,
40.1391317641987));
#167682=CARTESIAN_POINT('Ctrl Pts',(62.9396576302675,-0.130042276798797,
40.1369830144753));
#167683=CARTESIAN_POINT('Ctrl Pts',(62.938209392844,-0.135480523183572,
40.134683756585));
#167684=CARTESIAN_POINT('Ctrl Pts',(62.9366713579026,-0.14083344149334,
40.1322415082996));
#167685=CARTESIAN_POINT('Ctrl Pts',(62.9312882356078,-0.159568655577527,
40.1236936393009));
#167686=CARTESIAN_POINT('Ctrl Pts',(62.9248050892389,-0.177258600738952,
40.113394140767));
#167687=CARTESIAN_POINT('Ctrl Pts',(62.9174267595942,-0.193556601113636,
40.101665321223));
#167688=CARTESIAN_POINT('Ctrl Pts',(62.9137375947718,-0.201705601300978,
40.095800911451));
#167689=CARTESIAN_POINT('Ctrl Pts',(62.9098246351408,-0.209506615291396,
40.0895791707949));
#167690=CARTESIAN_POINT('Ctrl Pts',(62.9057134946881,-0.216916308650389,
40.0830403822906));
#167691=CARTESIAN_POINT('Ctrl Pts',(62.9036579244618,-0.220621155329885,
40.0797709880385));
#167692=CARTESIAN_POINT('Ctrl Pts',(62.9015528091474,-0.224228171852543,
40.0764223317514));
#167693=CARTESIAN_POINT('Ctrl Pts',(62.8994013510256,-0.227731941419532,
40.0729994484778));
#167694=CARTESIAN_POINT('Ctrl Pts',(62.8972498929038,-0.231235710986522,
40.0695765652042));
#167695=CARTESIAN_POINT('Ctrl Pts',(62.8950520414621,-0.234636114276735,
40.0660793733488));
#167696=CARTESIAN_POINT('Ctrl Pts',(62.8928111037451,-0.237927978230923,
40.0625130768817));
#167697=CARTESIAN_POINT('Ctrl Pts',(62.8927919932396,-0.237956050936217,
40.0624826638418));
#167698=CARTESIAN_POINT('Ctrl Pts',(62.8927728797351,-0.237984115711008,
40.0624522459912));
#167699=CARTESIAN_POINT('Ctrl Pts',(62.8927537632335,-0.238012172552841,
40.0624218233329));
#167700=CARTESIAN_POINT('Ctrl Pts',(62.882990686785,-0.252341211296126,
40.0468845275922));
#167701=CARTESIAN_POINT('Ctrl Pts',(62.8725309380423,-0.264702219189255,
40.0302263329287));
#167702=CARTESIAN_POINT('Ctrl Pts',(62.8615664772849,-0.275152816745115,
40.0127515884821));
#167703=CARTESIAN_POINT('Ctrl Pts',(62.8502312057454,-0.285956846570894,
39.994685859782));
#167704=CARTESIAN_POINT('Ctrl Pts',(62.8383556508917,-0.294719332055952,
39.9757460620624));
#167705=CARTESIAN_POINT('Ctrl Pts',(62.8261370346475,-0.301453885678947,
39.9562444559293));
#167706=CARTESIAN_POINT('Ctrl Pts',(62.8141508421947,-0.308060333921169,
39.9371138113801));
#167707=CARTESIAN_POINT('Ctrl Pts',(62.8018335935216,-0.312715155744622,
39.9174410654569));
#167708=CARTESIAN_POINT('Ctrl Pts',(62.7893708783698,-0.315383336840266,
39.8975196504386));
#167709=CARTESIAN_POINT('Ctrl Pts',(62.7811147664994,-0.31715091327508,
39.8843224113936));
#167710=CARTESIAN_POINT('Ctrl Pts',(62.7727948225175,-0.318045664008453,
39.8710160447212));
#167711=CARTESIAN_POINT('Ctrl Pts',(62.7644678366119,-0.318045750793045,
39.8576902534424));
#167712=CARTESIAN_POINT('',(62.4081695979768,-0.318048871877129,39.2875012672119));
#167713=CARTESIAN_POINT('',(62.7644678366119,-0.318045750793045,39.8576902534424));
#167714=CARTESIAN_POINT('',(62.0995362748659,-6.20712349654464,39.2875012672119));
#167715=CARTESIAN_POINT('Origin',(5.53234440788222E-15,0.,39.2875012672119));
#167716=CARTESIAN_POINT('',(62.4538823482275,-6.2443699078806,39.8576902534424));
#167717=CARTESIAN_POINT('',(62.0995362748659,-6.20712349654464,39.2875012672119));
#167718=CARTESIAN_POINT('',(62.6108711573006,-6.56531752495302,40.1599502534424));
#167719=CARTESIAN_POINT('Ctrl Pts',(62.4538823482275,-6.2443699078806,39.8576902534424));
#167720=CARTESIAN_POINT('Ctrl Pts',(62.4661208561102,-6.2456563596144,39.8773836120348));
#167721=CARTESIAN_POINT('Ctrl Pts',(62.4781153572947,-6.24887816048055,
39.8969946442101));
#167722=CARTESIAN_POINT('Ctrl Pts',(62.489703469055,-6.25393874389324,39.9162525288194));
#167723=CARTESIAN_POINT('Ctrl Pts',(62.5015244311524,-6.25910101415343,
39.9358973794));
#167724=CARTESIAN_POINT('Ctrl Pts',(62.5129234356945,-6.26617675898116,
39.9551762199662));
#167725=CARTESIAN_POINT('Ctrl Pts',(62.523731436973,-6.27511683300192,39.9738152034151));
#167726=CARTESIAN_POINT('Ctrl Pts',(62.5341195571996,-6.28370959325135,
39.9917300792536));
#167727=CARTESIAN_POINT('Ctrl Pts',(62.5439624606626,-6.29402509233189,
40.0090551157999));
#167728=CARTESIAN_POINT('Ctrl Pts',(62.5531007542688,-6.30606398946847,
40.02553945514));
#167729=CARTESIAN_POINT('Ctrl Pts',(62.5601204743137,-6.31531185249311,
40.0382021526063));
#167730=CARTESIAN_POINT('Ctrl Pts',(62.5667243349245,-6.32557753707731,
40.0503687782082));
#167731=CARTESIAN_POINT('Ctrl Pts',(62.5728320301413,-6.33687803771691,
40.0619155352442));
#167732=CARTESIAN_POINT('Ctrl Pts',(62.5728480373212,-6.33690765431375,
40.0619457972351));
#167733=CARTESIAN_POINT('Ctrl Pts',(62.5728640408535,-6.33693727882097,
40.0619760547304));
#167734=CARTESIAN_POINT('Ctrl Pts',(62.5728800407364,-6.33696691123577,
40.0620063077269));
#167735=CARTESIAN_POINT('Ctrl Pts',(62.5745955535553,-6.34014410870328,
40.06525004417));
#167736=CARTESIAN_POINT('Ctrl Pts',(62.5762674929177,-6.34341121944319,
40.0684393223556));
#167737=CARTESIAN_POINT('Ctrl Pts',(62.5778935423008,-6.34676388583387,
40.0715697951759));
#167738=CARTESIAN_POINT('Ctrl Pts',(62.586942137402,-6.36542071200092,40.0889901646436));
#167739=CARTESIAN_POINT('Ctrl Pts',(62.5945741278866,-6.38672471011642,
40.104596309827));
#167740=CARTESIAN_POINT('Ctrl Pts',(62.600410948358,-6.40987366744635,40.117663465076));
#167741=CARTESIAN_POINT('Ctrl Pts',(62.603030594215,-6.42026324006751,40.1235281853083));
#167742=CARTESIAN_POINT('Ctrl Pts',(62.6052889671231,-6.43102458681719,
40.1288820140929));
#167743=CARTESIAN_POINT('Ctrl Pts',(62.6071534261453,-6.44208677567865,
40.1336621774101));
#167744=CARTESIAN_POINT('Ctrl Pts',(62.6079636948179,-6.44689425333218,
40.1357395717319));
#167745=CARTESIAN_POINT('Ctrl Pts',(62.6086994224563,-6.45175840517988,
40.1377083672883));
#167746=CARTESIAN_POINT('Ctrl Pts',(62.6093578414453,-6.45667331290429,
40.1395632548791));
#167747=CARTESIAN_POINT('Ctrl Pts',(62.6116623079068,-6.47387548993976,
40.1460553614469));
#167748=CARTESIAN_POINT('Ctrl Pts',(62.6130197402063,-6.49169942613405,
40.1511520974629));
#167749=CARTESIAN_POINT('Ctrl Pts',(62.6133114945132,-6.50989137546619,
40.1546258197408));
#167750=CARTESIAN_POINT('Ctrl Pts',(62.6134573716666,-6.51898735013226,
40.1563626808798));
#167751=CARTESIAN_POINT('Ctrl Pts',(62.6133368299269,-6.52817532814393,
40.1576937882008));
#167752=CARTESIAN_POINT('Ctrl Pts',(62.6129350466932,-6.53742359207002,
40.1585906813668));
#167753=CARTESIAN_POINT('Ctrl Pts',(62.6127341550764,-6.54204772403306,
40.1590391279498));
#167754=CARTESIAN_POINT('Ctrl Pts',(62.6124629532086,-6.54668692748761,
40.1593790209175));
#167755=CARTESIAN_POINT('Ctrl Pts',(62.6121195889602,-6.55133723782952,
40.1596068022931));
#167756=CARTESIAN_POINT('Ctrl Pts',(62.6117762247118,-6.55598754817143,
40.1598345836687));
#167757=CARTESIAN_POINT('Ctrl Pts',(62.6113606963859,-6.56064896522272,
40.1599502506864));
#167758=CARTESIAN_POINT('Ctrl Pts',(62.6108711573006,-6.56531752495302,
40.1599502534424));
#167759=CARTESIAN_POINT('',(62.6076796697354,-6.59568250079886,40.1599502534424));
#167760=CARTESIAN_POINT('Origin',(5.50063869163689E-15,5.71112962987806E-15,
40.1599502534424));
#167761=CARTESIAN_POINT('',(62.3873926810691,-6.87697683366565,39.8576902534424));
#167762=CARTESIAN_POINT('Ctrl Pts',(62.6076796697354,-6.59568250079886,
40.1599502534424));
#167763=CARTESIAN_POINT('Ctrl Pts',(62.6072792748563,-6.59948308607503,
40.1599502447857));
#167764=CARTESIAN_POINT('Ctrl Pts',(62.6068325084578,-6.60326825869922,
40.1598744685927));
#167765=CARTESIAN_POINT('Ctrl Pts',(62.6063406883232,-6.60703621730596,
40.1597246934279));
#167766=CARTESIAN_POINT('Ctrl Pts',(62.6034985746717,-6.62881036976826,
40.1588591777435));
#167767=CARTESIAN_POINT('Ctrl Pts',(62.5991534367855,-6.65001265698081,
40.1555254706025));
#167768=CARTESIAN_POINT('Ctrl Pts',(62.593559428359,-6.67028839971139,40.1500631826393));
#167769=CARTESIAN_POINT('Ctrl Pts',(62.5913032360759,-6.67846607317848,
40.147860116249));
#167770=CARTESIAN_POINT('Ctrl Pts',(62.5888441205341,-6.68649343259762,
40.1453112228312));
#167771=CARTESIAN_POINT('Ctrl Pts',(62.5861994699221,-6.69434891543609,
40.1424401896328));
#167772=CARTESIAN_POINT('Ctrl Pts',(62.5852237544099,-6.69724711167652,
40.1413809526905));
#167773=CARTESIAN_POINT('Ctrl Pts',(62.5842227327444,-6.70012178934728,
40.1402777640511));
#167774=CARTESIAN_POINT('Ctrl Pts',(62.5831972538526,-6.70297180428183,
40.1391317641987));
#167775=CARTESIAN_POINT('Ctrl Pts',(62.5812744809303,-6.70831558228412,
40.1369830144753));
#167776=CARTESIAN_POINT('Ctrl Pts',(62.5792657255654,-6.71357265535385,
40.1346837565849));
#167777=CARTESIAN_POINT('Ctrl Pts',(62.5771765838154,-6.71873548138815,
40.1322415082996));
#167778=CARTESIAN_POINT('Ctrl Pts',(62.5698645876906,-6.73680537250822,
40.1236936393008));
#167779=CARTESIAN_POINT('Ctrl Pts',(62.5615678538928,-6.75372073697203,
40.113394140767));
#167780=CARTESIAN_POINT('Ctrl Pts',(62.5525263385764,-6.76915820973612,
40.101665321223));
#167781=CARTESIAN_POINT('Ctrl Pts',(62.5480055809182,-6.77687694611817,
40.095800911451));
#167782=CARTESIAN_POINT('Ctrl Pts',(62.5432986288851,-6.78422620968065,
40.0895791707949));
#167783=CARTESIAN_POINT('Ctrl Pts',(62.5384354858299,-6.79116558077034,
40.0830403822906));
#167784=CARTESIAN_POINT('Ctrl Pts',(62.5360039143023,-6.79463526631518,
40.0797709880385));
#167785=CARTESIAN_POINT('Ctrl Pts',(62.5335332951358,-6.7980024787551,40.0764223317514));
#167786=CARTESIAN_POINT('Ctrl Pts',(62.5310273792782,-6.80126216569454,
40.0729994484778));
#167787=CARTESIAN_POINT('Ctrl Pts',(62.5285214634206,-6.80452185263398,
40.0695765652042));
#167788=CARTESIAN_POINT('Ctrl Pts',(62.5259802131086,-6.80767389012548,
40.0660793733488));
#167789=CARTESIAN_POINT('Ctrl Pts',(62.5234074580025,-6.81071347912866,
40.0625130768816));
#167790=CARTESIAN_POINT('Ctrl Pts',(62.5233855177896,-6.81073940045697,
40.0624826638418));
#167791=CARTESIAN_POINT('Ctrl Pts',(62.5233635754231,-6.81076531358473,
40.0624522459912));
#167792=CARTESIAN_POINT('Ctrl Pts',(62.5233416309052,-6.81079121850972,
40.0624218233329));
#167793=CARTESIAN_POINT('Ctrl Pts',(62.5121342452084,-6.82402124190459,
40.0468845275886));
#167794=CARTESIAN_POINT('Ctrl Pts',(62.5004397189015,-6.83522119344303,
40.0302263329211));
#167795=CARTESIAN_POINT('Ctrl Pts',(62.4884429377018,-6.84446844329974,
40.0127515884702));
#167796=CARTESIAN_POINT('Ctrl Pts',(62.4760404333281,-6.85402842900616,
39.9946858597657));
#167797=CARTESIAN_POINT('Ctrl Pts',(62.4633140048613,-6.86150157917988,
39.9757460620414));
#167798=CARTESIAN_POINT('Ctrl Pts',(62.4504583709314,-6.86692204703359,
39.9562444559034));
#167799=CARTESIAN_POINT('Ctrl Pts',(62.43784727821,-6.87223940618281,39.93711381135));
#167800=CARTESIAN_POINT('Ctrl Pts',(62.4251109433393,-6.87558122532823,
39.9174410654225));
#167801=CARTESIAN_POINT('Ctrl Pts',(62.4124375993731,-6.87693208138335,
39.8975196504));
#167802=CARTESIAN_POINT('Ctrl Pts',(62.4040419533072,-6.87782697616054,
39.8843224113677));
#167803=CARTESIAN_POINT('Ctrl Pts',(62.3956740599381,-6.87784715439598,
39.8710160447083));
#167804=CARTESIAN_POINT('Ctrl Pts',(62.3873926810691,-6.87697683366565,
39.8576902534424));
#167805=CARTESIAN_POINT('',(62.0330459552232,-6.8397366303026,39.2875012672119));
#167806=CARTESIAN_POINT('',(62.3873926810691,-6.87697683366565,39.8576902534424));
#167807=CARTESIAN_POINT('',(61.1105274371641,-12.6642893210142,39.2875012672119));
#167808=CARTESIAN_POINT('Origin',(5.53234440788222E-15,0.,39.2875012672119));
#167809=CARTESIAN_POINT('',(61.4590390555209,-12.7383709431251,39.8576902534424));
#167810=CARTESIAN_POINT('',(61.1105274371641,-12.6642893210142,39.2875012672119));
#167811=CARTESIAN_POINT('',(61.5816197022698,-13.0739701745325,40.1599502534424));
#167812=CARTESIAN_POINT('Ctrl Pts',(61.4590390555209,-12.7383709431251,
39.8576902534424));
#167813=CARTESIAN_POINT('Ctrl Pts',(61.4710760487545,-12.7409296199635,
39.8773836120357));
#167814=CARTESIAN_POINT('Ctrl Pts',(61.4826680729135,-12.7453875382442,
39.8969946442118));
#167815=CARTESIAN_POINT('Ctrl Pts',(61.4936637287782,-12.7516316867663,
39.916252528822));
#167816=CARTESIAN_POINT('Ctrl Pts',(61.5048803302315,-12.7580013045727,
39.9358973794034));
#167817=CARTESIAN_POINT('Ctrl Pts',(61.5154772731011,-12.7662298081581,
39.9551762199704));
#167818=CARTESIAN_POINT('Ctrl Pts',(61.5252915748192,-12.7762506512834,
39.97381520342));
#167819=CARTESIAN_POINT('Ctrl Pts',(61.5347245998124,-12.7858821937373,
39.9917300792592));
#167820=CARTESIAN_POINT('Ctrl Pts',(61.5434353195539,-12.7971700470085,
40.0090551158061));
#167821=CARTESIAN_POINT('Ctrl Pts',(61.5512651452145,-12.8100982055954,
40.0255394551466));
#167822=CARTESIAN_POINT('Ctrl Pts',(61.5572797455868,-12.8200291684063,
40.0382021526106));
#167823=CARTESIAN_POINT('Ctrl Pts',(61.5627743733232,-12.8309289078957,
40.0503687782102));
#167824=CARTESIAN_POINT('Ctrl Pts',(61.5676673859796,-12.8428059312035,
40.0619155352442));
#167825=CARTESIAN_POINT('Ctrl Pts',(61.5676802096931,-12.8428370587634,
40.0619457972351));
#167826=CARTESIAN_POINT('Ctrl Pts',(61.5676930289522,-12.8428681938091,
40.0619760547305));
#167827=CARTESIAN_POINT('Ctrl Pts',(61.5677058437553,-12.8428993363376,
40.0620063077269));
#167828=CARTESIAN_POINT('Ctrl Pts',(61.5690798512467,-12.8462384487037,
40.06525004417));
#167829=CARTESIAN_POINT('Ctrl Pts',(61.5704011254854,-12.8496624271213,
40.0684393223556));
#167830=CARTESIAN_POINT('Ctrl Pts',(61.5716678181342,-12.8531666956979,
40.0715697951759));
#167831=CARTESIAN_POINT('Ctrl Pts',(61.5787166747157,-12.8726671535591,
40.0889901646429));
#167832=CARTESIAN_POINT('Ctrl Pts',(61.5840799821732,-12.8946522063799,
40.1045963098259));
#167833=CARTESIAN_POINT('Ctrl Pts',(61.5874651029954,-12.9182844651727,
40.1176634650745));
#167834=CARTESIAN_POINT('Ctrl Pts',(61.5889843920985,-12.9288909501846,
40.1235281853075));
#167835=CARTESIAN_POINT('Ctrl Pts',(61.5901055263652,-12.9398294094013,
40.1288820140925));
#167836=CARTESIAN_POINT('Ctrl Pts',(61.5908034580838,-12.951025887472,40.1336621774101));
#167837=CARTESIAN_POINT('Ctrl Pts',(61.5911067697685,-12.9558917253992,
40.1357395717319));
#167838=CARTESIAN_POINT('Ctrl Pts',(61.5913300246961,-12.9608061353935,
40.1377083672884));
#167839=CARTESIAN_POINT('Ctrl Pts',(61.5914710890455,-12.9657629422643,
40.1395632548792));
#167840=CARTESIAN_POINT('Ctrl Pts',(61.5919648142682,-12.9831117663119,
40.146055361447));
#167841=CARTESIAN_POINT('Ctrl Pts',(61.5914517017518,-13.000979951431,40.151152097463));
#167842=CARTESIAN_POINT('Ctrl Pts',(61.5898402812905,-13.0191027399906,
40.1546258197409));
#167843=CARTESIAN_POINT('Ctrl Pts',(61.5890345710599,-13.0281641342704,
40.1563626808798));
#167844=CARTESIAN_POINT('Ctrl Pts',(61.5879542844384,-13.0372891795344,
40.1576937882008));
#167845=CARTESIAN_POINT('Ctrl Pts',(61.5865879953992,-13.046444782719,40.1585906813668));
#167846=CARTESIAN_POINT('Ctrl Pts',(61.5859048508796,-13.0510225843113,
40.1590391279498));
#167847=CARTESIAN_POINT('Ctrl Pts',(61.5851502058761,-13.0556080254095,
40.1593790209175));
#167848=CARTESIAN_POINT('Ctrl Pts',(61.5843226328192,-13.0601969695275,
40.1596068022931));
#167849=CARTESIAN_POINT('Ctrl Pts',(61.5834950597624,-13.0647859136456,
40.1598345836687));
#167850=CARTESIAN_POINT('Ctrl Pts',(61.5825945569831,-13.0693783604292,
40.1599502506864));
#167851=CARTESIAN_POINT('Ctrl Pts',(61.5816197022698,-13.0739701745325,
40.1599502534424));
#167852=CARTESIAN_POINT('',(61.5752716937451,-13.1038352065728,40.1599502534424));
#167853=CARTESIAN_POINT('Origin',(5.50318346416883E-15,5.72719669130613E-15,
40.1599502534424));
#167854=CARTESIAN_POINT('',(61.3267881959113,-13.3605623192487,39.8576902534424));
#167855=CARTESIAN_POINT('Ctrl Pts',(61.5752716937451,-13.1038352065728,
40.1599502534424));
#167856=CARTESIAN_POINT('Ctrl Pts',(61.5744762229326,-13.1075731191838,
40.1599502447858));
#167857=CARTESIAN_POINT('Ctrl Pts',(61.5736362456896,-13.1112908564312,
40.1598744685927));
#167858=CARTESIAN_POINT('Ctrl Pts',(61.5727532608743,-13.1149867645636,
40.1597246934279));
#167859=CARTESIAN_POINT('Ctrl Pts',(61.5676506979226,-13.1363445541695,
40.1588591777435));
#167860=CARTESIAN_POINT('Ctrl Pts',(61.5611131206557,-13.1569765024498,
40.1555254706021));
#167861=CARTESIAN_POINT('Ctrl Pts',(61.5534303645627,-13.1765564394372,
40.1500631826381));
#167862=CARTESIAN_POINT('Ctrl Pts',(61.5503317322969,-13.1844534784397,
40.1478601162481));
#167863=CARTESIAN_POINT('Ctrl Pts',(61.5470470005037,-13.192179815574,40.1453112228307));
#167864=CARTESIAN_POINT('Ctrl Pts',(61.5435957160157,-13.1997158239898,
40.1424401896328));
#167865=CARTESIAN_POINT('Ctrl Pts',(61.542322401576,-13.2024961535649,40.1413809526906));
#167866=CARTESIAN_POINT('Ctrl Pts',(61.5410263779726,-13.2052504481942,
40.1402777640512));
#167867=CARTESIAN_POINT('Ctrl Pts',(61.53970860908,-13.2079776587161,40.1391317641987));
#167868=CARTESIAN_POINT('Ctrl Pts',(61.5372377924063,-13.2130911784445,
40.1369830144753));
#167869=CARTESIAN_POINT('Ctrl Pts',(61.5346905274442,-13.2181094806066,
40.134683756585));
#167870=CARTESIAN_POINT('Ctrl Pts',(61.5320731679599,-13.223025649363,40.1322415082996));
#167871=CARTESIAN_POINT('Ctrl Pts',(61.5229124097647,-13.2402322400105,
40.1236936393009));
#167872=CARTESIAN_POINT('Ctrl Pts',(61.5128929892897,-13.2561876955039,
40.113394140767));
#167873=CARTESIAN_POINT('Ctrl Pts',(61.5022873490355,-13.2705955044753,
40.101665321223));
#167874=CARTESIAN_POINT('Ctrl Pts',(61.4969845289084,-13.277799408961,40.095800911451));
#167875=CARTESIAN_POINT('Ctrl Pts',(61.4915351548247,-13.284616402026,40.0895791707949));
#167876=CARTESIAN_POINT('Ctrl Pts',(61.4859732907799,-13.2910094216446,
40.0830403822907));
#167877=CARTESIAN_POINT('Ctrl Pts',(61.4831923587575,-13.2942059314539,
40.0797709880385));
#167878=CARTESIAN_POINT('Ctrl Pts',(61.4803833043595,-13.2972964479269,
40.0764223317514));
#167879=CARTESIAN_POINT('Ctrl Pts',(61.4775503861047,-13.3002763384266,
40.0729994484778));
#167880=CARTESIAN_POINT('Ctrl Pts',(61.4747174678498,-13.3032562289262,
40.0695765652042));
#167881=CARTESIAN_POINT('Ctrl Pts',(61.4718606611378,-13.3061253662367,
40.0660793733488));
#167882=CARTESIAN_POINT('Ctrl Pts',(61.4689842762858,-13.3088793779156,
40.0625130768817));
#167883=CARTESIAN_POINT('Ctrl Pts',(61.4689597467471,-13.3089028638675,
40.0624826638418));
#167884=CARTESIAN_POINT('Ctrl Pts',(61.4689352159238,-13.3089263414386,
40.0624522459912));
#167885=CARTESIAN_POINT('Ctrl Pts',(61.4689106838182,-13.3089498106269,
40.0624218233329));
#167886=CARTESIAN_POINT('Ctrl Pts',(61.4563817793396,-13.3209358677642,
40.04688452759));
#167887=CARTESIAN_POINT('Ctrl Pts',(61.4435806031496,-13.330852053932,40.030226332924));
#167888=CARTESIAN_POINT('Ctrl Pts',(61.4306829407567,-13.3387946412831,
40.0127515884748));
#167889=CARTESIAN_POINT('Ctrl Pts',(61.417349087986,-13.3470058416643,39.9946858597719));
#167890=CARTESIAN_POINT('Ctrl Pts',(61.4039112193236,-13.353107779129,39.9757460620493));
#167891=CARTESIAN_POINT('Ctrl Pts',(61.3905594167276,-13.357154773434,39.956244455913));
#167892=CARTESIAN_POINT('Ctrl Pts',(61.3774615935119,-13.3611247853915,
39.9371138113611));
#167893=CARTESIAN_POINT('Ctrl Pts',(61.3644457143973,-13.363116988191,39.917441065435));
#167894=CARTESIAN_POINT('Ctrl Pts',(61.3517005934285,-13.363135718947,39.897519650414));
#167895=CARTESIAN_POINT('Ctrl Pts',(61.3432573976113,-13.3631481274162,
39.884322411377));
#167896=CARTESIAN_POINT('Ctrl Pts',(61.3349332352346,-13.3622935120785,
39.8710160447129));
#167897=CARTESIAN_POINT('Ctrl Pts',(61.3267881959113,-13.3605623192487,
39.8576902534424));
#167898=CARTESIAN_POINT('',(60.9782752797348,-13.2864868028996,39.2875012672119));
#167899=CARTESIAN_POINT('',(61.3267881959113,-13.3605623192487,39.8576902534424));
#167900=CARTESIAN_POINT('',(59.4519788726607,-18.9827025415097,39.2875012672119));
#167901=CARTESIAN_POINT('Origin',(5.53234440788222E-15,0.,39.2875012672119));
#167902=CARTESIAN_POINT('',(59.7908376697911,-19.0928077206412,39.8576902534424));
#167903=CARTESIAN_POINT('',(59.4519788726608,-18.9827025415097,39.2875012672119));
#167904=CARTESIAN_POINT('',(59.8776671349985,-19.4393816709757,40.1599502534424));
#167905=CARTESIAN_POINT('Ctrl Pts',(59.7908376697911,-19.0928077206412,
39.8576902534424));
#167906=CARTESIAN_POINT('Ctrl Pts',(59.8025412685588,-19.0966105891853,
39.8773836120362));
#167907=CARTESIAN_POINT('Ctrl Pts',(59.8136038110496,-19.1022557829949,
39.8969946442128));
#167908=CARTESIAN_POINT('Ctrl Pts',(59.8238865403118,-19.1096150844286,
39.9162525288235));
#167909=CARTESIAN_POINT('Ctrl Pts',(59.8343758896881,-19.1171222629155,
39.9358973794055));
#167910=CARTESIAN_POINT('Ctrl Pts',(59.8440546685613,-19.1264133720511,
39.955176219973));
#167911=CARTESIAN_POINT('Ctrl Pts',(59.8527677431753,-19.1374051938264,
39.973815203423));
#167912=CARTESIAN_POINT('Ctrl Pts',(59.8611423227391,-19.14796999329,39.9917300792627));
#167913=CARTESIAN_POINT('Ctrl Pts',(59.8686254222905,-19.160106528669,40.00905511581));
#167914=CARTESIAN_POINT('Ctrl Pts',(59.8750609947969,-19.1737823050951,
40.0255394551508));
#167915=CARTESIAN_POINT('Ctrl Pts',(59.880004578277,-19.1842875619857,40.0382021526133));
#167916=CARTESIAN_POINT('Ctrl Pts',(59.8843297728483,-19.1957019365542,
40.0503687782115));
#167917=CARTESIAN_POINT('Ctrl Pts',(59.8879544940744,-19.2080253553779,
40.0619155352442));
#167918=CARTESIAN_POINT('Ctrl Pts',(59.8879639938223,-19.2080576528609,
40.0619457972351));
#167919=CARTESIAN_POINT('Ctrl Pts',(59.8879734883577,-19.208089957323,40.0619760547305));
#167920=CARTESIAN_POINT('Ctrl Pts',(59.8879829776793,-19.2081222687611,
40.0620063077269));
#167921=CARTESIAN_POINT('Ctrl Pts',(59.8890004259296,-19.2115867120118,
40.06525004417));
#167922=CARTESIAN_POINT('Ctrl Pts',(59.8899565588875,-19.2151300442832,
40.0684393223556));
#167923=CARTESIAN_POINT('Ctrl Pts',(59.8908500166522,-19.2187475215459,
40.0715697951759));
#167924=CARTESIAN_POINT('Ctrl Pts',(59.8958219059664,-19.2388779600041,
40.0889901646423));
#167925=CARTESIAN_POINT('Ctrl Pts',(59.8988577688783,-19.261303194691,40.1045963098248));
#167926=CARTESIAN_POINT('Ctrl Pts',(59.8997541019594,-19.285159834974,40.1176634650732));
#167927=CARTESIAN_POINT('Ctrl Pts',(59.9001563886589,-19.2958670255072,
40.1235281853067));
#167928=CARTESIAN_POINT('Ctrl Pts',(59.9001280009024,-19.3068627531426,
40.1288820140922));
#167929=CARTESIAN_POINT('Ctrl Pts',(59.8996517586312,-19.3180708494659,
40.1336621774101));
#167930=CARTESIAN_POINT('Ctrl Pts',(59.8994447901818,-19.322941736528,40.1357395717319));
#167931=CARTESIAN_POINT('Ctrl Pts',(59.8991531263709,-19.3278525613647,
40.1377083672884));
#167932=CARTESIAN_POINT('Ctrl Pts',(59.8987752905501,-19.3327969595684,
40.1395632548792));
#167933=CARTESIAN_POINT('Ctrl Pts',(59.8974528651773,-19.3501023532815,
40.146055361447));
#167934=CARTESIAN_POINT('Ctrl Pts',(59.895074829613,-19.3678190197501,40.1511520974629));
#167935=CARTESIAN_POINT('Ctrl Pts',(59.8915778894434,-19.3856740904733,
40.1546258197408));
#167936=CARTESIAN_POINT('Ctrl Pts',(59.8898294193586,-19.3946016258349,
40.1563626808798));
#167937=CARTESIAN_POINT('Ctrl Pts',(59.8878012237015,-19.4035637624457,
40.1576937882008));
#167938=CARTESIAN_POINT('Ctrl Pts',(59.8854853982054,-19.4125263941844,
40.1585906813668));
#167939=CARTESIAN_POINT('Ctrl Pts',(59.8843274854574,-19.4170077100538,
40.1590391279498));
#167940=CARTESIAN_POINT('Ctrl Pts',(59.8830976653668,-19.4214891497433,
40.1593790209175));
#167941=CARTESIAN_POINT('Ctrl Pts',(59.881794950565,-19.4259664502055,40.1596068022931));
#167942=CARTESIAN_POINT('Ctrl Pts',(59.8804922357633,-19.4304437506676,
40.1598345836687));
#167943=CARTESIAN_POINT('Ctrl Pts',(59.8791166246276,-19.4349169113756,
40.1599502506865));
#167944=CARTESIAN_POINT('Ctrl Pts',(59.8776671349985,-19.4393816709757,
40.1599502534424));
#167945=CARTESIAN_POINT('',(59.8682321556242,-19.4684195516697,40.1599502534424));
#167946=CARTESIAN_POINT('Origin',(5.50739376141089E-15,5.74290973452844E-15,
40.1599502534424));
#167947=CARTESIAN_POINT('',(59.5942745858235,-19.6977666881846,39.8576902534424));
#167948=CARTESIAN_POINT('Ctrl Pts',(59.8682321556242,-19.4684195516697,
40.1599502534424));
#167949=CARTESIAN_POINT('Ctrl Pts',(59.8670503242229,-19.4720538382627,
40.1599502447858));
#167950=CARTESIAN_POINT('Ctrl Pts',(59.8658263391019,-19.4756634078261,
40.1598744685927));
#167951=CARTESIAN_POINT('Ctrl Pts',(59.8645618637724,-19.4792467723412,
40.1597246934279));
#167952=CARTESIAN_POINT('Ctrl Pts',(59.8572547562668,-19.4999541986804,
40.1588591777433));
#167953=CARTESIAN_POINT('Ctrl Pts',(59.8485963666826,-19.5197897600872,
40.1555254706009));
#167954=CARTESIAN_POINT('Ctrl Pts',(59.8389090368052,-19.5384593694458,
40.1500631826353));
#167955=CARTESIAN_POINT('Ctrl Pts',(59.8350019138213,-19.5459892523701,
40.147860116246));
#167956=CARTESIAN_POINT('Ctrl Pts',(59.8309275539868,-19.5533299158514,
40.1453112228295));
#167957=CARTESIAN_POINT('Ctrl Pts',(59.8267074486193,-19.5604638837579,
40.1424401896328));
#167958=CARTESIAN_POINT('Ctrl Pts',(59.8251504859514,-19.563095884795,40.1413809526905));
#167959=CARTESIAN_POINT('Ctrl Pts',(59.8235736599159,-19.5656996197545,
40.1402777640511));
#167960=CARTESIAN_POINT('Ctrl Pts',(59.8219780387743,-19.5682741459745,
40.1391317641986));
#167961=CARTESIAN_POINT('Ctrl Pts',(59.8189862491338,-19.573101382637,40.1369830144753));
#167962=CARTESIAN_POINT('Ctrl Pts',(59.8159283829425,-19.5778259323227,
40.1346837565849));
#167963=CARTESIAN_POINT('Ctrl Pts',(59.812811482062,-19.5824415812275,40.1322415082995));
#167964=CARTESIAN_POINT('Ctrl Pts',(59.8019023289803,-19.5985963523946,
40.1236936393008));
#167965=CARTESIAN_POINT('Ctrl Pts',(59.7902699966956,-19.6134170876082,
40.113394140767));
#167966=CARTESIAN_POINT('Ctrl Pts',(59.7782164291175,-19.6266373778168,
40.101665321223));
#167967=CARTESIAN_POINT('Ctrl Pts',(59.7721896453285,-19.6332475229211,
40.095800911451));
#167968=CARTESIAN_POINT('Ctrl Pts',(59.7660575536771,-19.6394575570861,
40.0895791707949));
#167969=CARTESIAN_POINT('Ctrl Pts',(59.7598579055891,-19.6452341819728,
40.0830403822906));
#167970=CARTESIAN_POINT('Ctrl Pts',(59.7567580815451,-19.6481224944161,
40.0797709880385));
#167971=CARTESIAN_POINT('Ctrl Pts',(59.7536413685033,-19.6509024545771,
40.0764223317514));
#167972=CARTESIAN_POINT('Ctrl Pts',(59.7505124858965,-19.6535699003331,
40.0729994484778));
#167973=CARTESIAN_POINT('Ctrl Pts',(59.7473836032896,-19.656237346089,40.0695765652042));
#167974=CARTESIAN_POINT('Ctrl Pts',(59.7442425399497,-19.6587921483496,
40.0660793733488));
#167975=CARTESIAN_POINT('Ctrl Pts',(59.7410940396263,-19.6612304091761,
40.0625130768817));
#167976=CARTESIAN_POINT('Ctrl Pts',(59.7410671895125,-19.6612512024345,
40.0624826638418));
#167977=CARTESIAN_POINT('Ctrl Pts',(59.7410403389972,-19.6612719872237,
40.0624522459912));
#167978=CARTESIAN_POINT('Ctrl Pts',(59.7410134880829,-19.6612927635421,
40.0624218233329));
#167979=CARTESIAN_POINT('Ctrl Pts',(59.7273003341212,-19.6719035326722,
40.0468845275906));
#167980=CARTESIAN_POINT('Ctrl Pts',(59.7135327604127,-19.6804273096593,
40.0302263329252));
#167981=CARTESIAN_POINT('Ctrl Pts',(59.6998755263142,-19.6869782138561,
40.0127515884767));
#167982=CARTESIAN_POINT('Ctrl Pts',(59.6857564136272,-19.6937506652829,
39.9946858597746));
#167983=CARTESIAN_POINT('Ctrl Pts',(59.6717543328698,-19.6984145359349,
39.9757460620528));
#167984=CARTESIAN_POINT('Ctrl Pts',(59.6580526467503,-19.7010437169746,
39.9562444559175));
#167985=CARTESIAN_POINT('Ctrl Pts',(59.6446115955321,-19.7036228854586,
39.9371138113664));
#167986=CARTESIAN_POINT('Ctrl Pts',(59.6314587768685,-19.7042436449211,
39.9174410654413));
#167987=CARTESIAN_POINT('Ctrl Pts',(59.6187815171093,-19.7029300451595,
39.8975196504211));
#167988=CARTESIAN_POINT('Ctrl Pts',(59.6103832769623,-19.7020598313701,
39.8843224113819));
#167989=CARTESIAN_POINT('Ctrl Pts',(59.6021940468446,-19.7003397858032,
39.8710160447154));
#167990=CARTESIAN_POINT('Ctrl Pts',(59.5942745858236,-19.6977666881846,
39.8576902534424));
#167991=CARTESIAN_POINT('',(59.2554138597571,-19.5876674457079,39.2875012672119));
#167992=CARTESIAN_POINT('',(59.5942745858236,-19.6977666881846,39.8576902534424));
#167993=CARTESIAN_POINT('',(57.1420619865021,-25.0931373005746,39.2875012672119));
#167994=CARTESIAN_POINT('Origin',(5.53234440788222E-15,0.,39.2875012672119));
#167995=CARTESIAN_POINT('',(57.467555354514,-25.2380597013431,39.8576902534424));
#167996=CARTESIAN_POINT('',(57.1420619865021,-25.0931373005746,39.2875012672119));
#167997=CARTESIAN_POINT('',(57.5176823163888,-25.5918112338795,40.1599502534424));
#167998=CARTESIAN_POINT('Ctrl Pts',(57.467555354514,-25.2380597013431,39.8576902534424));
#167999=CARTESIAN_POINT('Ctrl Pts',(57.4787973317376,-25.2430650965691,
39.8773836120353));
#168000=CARTESIAN_POINT('Ctrl Pts',(57.489209189029,-25.2498357159823,39.896994644211));
#168001=CARTESIAN_POINT('Ctrl Pts',(57.4986663319544,-25.2582295402801,
39.9162525288208));
#168002=CARTESIAN_POINT('Ctrl Pts',(57.5083135057462,-25.2667920292282,
39.9358973794019));
#168003=CARTESIAN_POINT('Ctrl Pts',(57.5169680778957,-25.2770439485771,
39.9551762199685));
#168004=CARTESIAN_POINT('Ctrl Pts',(57.5244844631365,-25.2888863203014,
39.9738152034178));
#168005=CARTESIAN_POINT('Ctrl Pts',(57.5317088436245,-25.3002686266197,
39.9917300792568));
#168006=CARTESIAN_POINT('Ctrl Pts',(57.537882336581,-25.3131208736838,40.0090551158036));
#168007=CARTESIAN_POINT('Ctrl Pts',(57.5428531464542,-25.3273944332791,
40.025539455144));
#168008=CARTESIAN_POINT('Ctrl Pts',(57.5466715501087,-25.3383588864591,
40.0382021526089));
#168009=CARTESIAN_POINT('Ctrl Pts',(57.5497799237794,-25.3501628378332,
40.0503687782094));
#168010=CARTESIAN_POINT('Ctrl Pts',(57.552096640372,-25.362797634221,40.0619155352442));
#168011=CARTESIAN_POINT('Ctrl Pts',(57.552102712073,-25.3628307477691,40.0619457972351));
#168012=CARTESIAN_POINT('Ctrl Pts',(57.5521087778605,-25.3628638677132,
40.0619760547304));
#168013=CARTESIAN_POINT('Ctrl Pts',(57.5521148377337,-25.3628969940501,
40.0620063077269));
#168014=CARTESIAN_POINT('Ctrl Pts',(57.552764579367,-25.3664488110202,40.06525004417));
#168015=CARTESIAN_POINT('Ctrl Pts',(57.5533450954513,-25.3700726756554,
40.0684393223556));
#168016=CARTESIAN_POINT('Ctrl Pts',(57.5538555294217,-25.3737637277663,
40.0715697951758));
#168017=CARTESIAN_POINT('Ctrl Pts',(57.5566959784089,-25.3943035935241,
40.0889901646408));
#168018=CARTESIAN_POINT('Ctrl Pts',(57.5573711352259,-25.4169233145116,
40.104596309822));
#168019=CARTESIAN_POINT('Ctrl Pts',(57.5557688601537,-25.4407429579403,
40.1176634650697));
#168020=CARTESIAN_POINT('Ctrl Pts',(57.5550497369122,-25.4514335437759,
40.1235281853045));
#168021=CARTESIAN_POINT('Ctrl Pts',(57.5538721381544,-25.4623660683384,
40.1288820140912));
#168022=CARTESIAN_POINT('Ctrl Pts',(57.5522269397031,-25.4734629846667,
40.1336621774101));
#168023=CARTESIAN_POINT('Ctrl Pts',(57.5515119587091,-25.4782855544059,
40.1357395717319));
#168024=CARTESIAN_POINT('Ctrl Pts',(57.5507085716896,-25.4831389900603,
40.1377083672884));
#168025=CARTESIAN_POINT('Ctrl Pts',(57.5498159753469,-25.4880168077357,
40.1395632548792));
#168026=CARTESIAN_POINT('Ctrl Pts',(57.5466918881476,-25.5050891695993,
40.146055361447));
#168027=CARTESIAN_POINT('Ctrl Pts',(57.5424749837907,-25.5224602099121,
40.1511520974629));
#168028=CARTESIAN_POINT('Ctrl Pts',(57.5371308371211,-25.5398519389076,
40.1546258197408));
#168029=CARTESIAN_POINT('Ctrl Pts',(57.5344587637862,-25.5485478034053,
40.1563626808798));
#168030=CARTESIAN_POINT('Ctrl Pts',(57.5315048804296,-25.5572488403188,
40.1576937882008));
#168031=CARTESIAN_POINT('Ctrl Pts',(57.5282648911454,-25.5659203041428,
40.1585906813668));
#168032=CARTESIAN_POINT('Ctrl Pts',(57.5266448965033,-25.5702560360549,
40.1590391279498));
#168033=CARTESIAN_POINT('Ctrl Pts',(57.5249533754919,-25.5745843747447,
40.1593790209175));
#168034=CARTESIAN_POINT('Ctrl Pts',(57.5231897917613,-25.5789009773101,
40.1596068022931));
#168035=CARTESIAN_POINT('Ctrl Pts',(57.5214262080306,-25.5832175798756,
40.1598345836687));
#168036=CARTESIAN_POINT('Ctrl Pts',(57.5195905600219,-25.587522445623,40.1599502506865));
#168037=CARTESIAN_POINT('Ctrl Pts',(57.5176823163888,-25.5918112338795,
40.1599502534424));
#168038=CARTESIAN_POINT('',(57.5052637377732,-25.6197038181298,40.1599502534424));
#168039=CARTESIAN_POINT('Origin',(5.5132234544654E-15,5.75809660415529E-15,
40.1599502534424));
#168040=CARTESIAN_POINT('',(57.2088336324698,-25.8191582032621,39.8576902534424));
#168041=CARTESIAN_POINT('Ctrl Pts',(57.5052637377732,-25.6197038181299,
40.1599502534424));
#168042=CARTESIAN_POINT('Ctrl Pts',(57.5037084941754,-25.6231946607004,
40.1599502447858));
#168043=CARTESIAN_POINT('Ctrl Pts',(57.5021139114133,-25.6266565153803,
40.1598744685927));
#168044=CARTESIAN_POINT('Ctrl Pts',(57.5004817994259,-25.6300880761866,
40.1597246934279));
#168045=CARTESIAN_POINT('Ctrl Pts',(57.4910502055677,-25.6499182643563,
40.1588591777434));
#168046=CARTESIAN_POINT('Ctrl Pts',(57.4803658667974,-25.6687401163222,
40.1555254706019));
#168047=CARTESIAN_POINT('Ctrl Pts',(57.4687800995525,-25.6862948498998,
40.1500631826377));
#168048=CARTESIAN_POINT('Ctrl Pts',(57.4641072931049,-25.6933750777789,
40.1478601162478));
#168049=CARTESIAN_POINT('Ctrl Pts',(57.4592879447652,-25.7002496417679,
40.1453112228305));
#168050=CARTESIAN_POINT('Ctrl Pts',(57.4543452548725,-25.7069034079251,
40.1424401896328));
#168051=CARTESIAN_POINT('Ctrl Pts',(57.4525217023852,-25.7093582436701,
40.1413809526906));
#168052=CARTESIAN_POINT('Ctrl Pts',(57.4506813499537,-25.7117828918948,
40.1402777640512));
#168053=CARTESIAN_POINT('Ctrl Pts',(57.4488253585223,-25.7141765267649,
40.1391317641987));
#168054=CARTESIAN_POINT('Ctrl Pts',(57.4453453745883,-25.7186645921463,
40.1369830144753));
#168055=CARTESIAN_POINT('Ctrl Pts',(57.4418104097897,-25.7230436262006,
40.134683756585));
#168056=CARTESIAN_POINT('Ctrl Pts',(57.4382281169313,-25.7273081852386,
40.1322415082996));
#168057=CARTESIAN_POINT('Ctrl Pts',(57.4256900919271,-25.7422341418718,
40.1236936393009));
#168058=CARTESIAN_POINT('Ctrl Pts',(57.4125722940993,-25.7557577777292,
40.113394140767));
#168059=CARTESIAN_POINT('Ctrl Pts',(57.3992028606062,-25.767645704909,40.101665321223));
#168060=CARTESIAN_POINT('Ctrl Pts',(57.3925181438596,-25.7735896684989,
40.095800911451));
#168061=CARTESIAN_POINT('Ctrl Pts',(57.3857705191197,-25.7791247053301,
40.0895791707949));
#168062=CARTESIAN_POINT('Ctrl Pts',(57.3790010116303,-25.7842216455737,
40.0830403822906));
#168063=CARTESIAN_POINT('Ctrl Pts',(57.3756162578857,-25.7867701156956,
40.0797709880385));
#168064=CARTESIAN_POINT('Ctrl Pts',(57.3722260335605,-25.7892090617192,
40.0764223317514));
#168065=CARTESIAN_POINT('Ctrl Pts',(57.3688354672942,-25.7915348376376,
40.0729994484778));
#168066=CARTESIAN_POINT('Ctrl Pts',(57.3654449010279,-25.793860613556,40.0695765652042));
#168067=CARTESIAN_POINT('Ctrl Pts',(57.3620539952074,-25.7960730898185,
40.0660793733488));
#168068=CARTESIAN_POINT('Ctrl Pts',(57.358667875041,-25.7981688856967,40.0625130768817));
#168069=CARTESIAN_POINT('Ctrl Pts',(57.3586389985276,-25.7981867584462,
40.0624826638418));
#168070=CARTESIAN_POINT('Ctrl Pts',(57.3586101225001,-25.7982046227311,
40.0624522459912));
#168071=CARTESIAN_POINT('Ctrl Pts',(57.3585812469612,-25.7982224785499,
40.0624218233329));
#168072=CARTESIAN_POINT('Ctrl Pts',(57.3438340877008,-25.8073417058662,
40.0468845275908));
#168073=CARTESIAN_POINT('Ctrl Pts',(57.3292509568922,-25.8143796853882,
40.0302263329259));
#168074=CARTESIAN_POINT('Ctrl Pts',(57.3149837826027,-25.8194671333536,
40.0127515884777));
#168075=CARTESIAN_POINT('Ctrl Pts',(57.3002341019524,-25.8247266354309,
39.9946858597759));
#168076=CARTESIAN_POINT('Ctrl Pts',(57.2858212188265,-25.8279013409274,
39.9757460620546));
#168077=CARTESIAN_POINT('Ctrl Pts',(57.2719197677237,-25.8290839028441,
39.9562444559196));
#168078=CARTESIAN_POINT('Ctrl Pts',(57.2582827514725,-25.8302439699449,
39.9371138113688));
#168079=CARTESIAN_POINT('Ctrl Pts',(57.2451370982931,-25.8294864848997,
39.9174410654439));
#168080=CARTESIAN_POINT('Ctrl Pts',(57.2326665944538,-25.8268549466943,
39.897519650424));
#168081=CARTESIAN_POINT('Ctrl Pts',(57.2244053228545,-25.8251116448903,
39.8843224113838));
#168082=CARTESIAN_POINT('Ctrl Pts',(57.2164407479154,-25.8225450142734,
39.8710160447163));
#168083=CARTESIAN_POINT('Ctrl Pts',(57.2088336324698,-25.8191582032621,
39.8576902534424));
#168084=CARTESIAN_POINT('',(56.8833377255394,-25.6742415049981,39.2875012672119));
#168085=CARTESIAN_POINT('',(57.2088336324698,-25.8191582032621,39.8576902534424));
#168086=CARTESIAN_POINT('',(54.2060847114741,-30.9286463962979,39.2875012672119));
#168087=CARTESIAN_POINT('Origin',(5.53234440788222E-15,0.,39.2875012672119));
#168088=CARTESIAN_POINT('',(54.5146464769137,-31.1067982185536,39.8576902534424));
#168089=CARTESIAN_POINT('',(54.2060847114741,-30.9286463962979,39.2875012672119));
#168090=CARTESIAN_POINT('',(54.5275217339719,-31.4638515574741,40.1599502534424));
#168091=CARTESIAN_POINT('Ctrl Pts',(54.5146464769138,-31.1067982185536,
39.8576902534424));
#168092=CARTESIAN_POINT('Ctrl Pts',(54.5253036631384,-31.1129513003039,
39.8773836120346));
#168093=CARTESIAN_POINT('Ctrl Pts',(54.5349507607431,-31.1207731649977,
39.8969946442096));
#168094=CARTESIAN_POINT('Ctrl Pts',(54.543478702895,-31.1301095476642,39.9162525288187));
#168095=CARTESIAN_POINT('Ctrl Pts',(54.5521780046476,-31.1396335346527,
39.935897379399));
#168096=CARTESIAN_POINT('Ctrl Pts',(54.5597135487701,-31.1507339420411,
39.9551762199648));
#168097=CARTESIAN_POINT('Ctrl Pts',(54.5659508935483,-31.1632971162118,
39.9738152034134));
#168098=CARTESIAN_POINT('Ctrl Pts',(54.5719459231361,-31.1753722224548,
39.9917300792516));
#168099=CARTESIAN_POINT('Ctrl Pts',(54.5767421714171,-31.1887993692954,
40.0090551157976));
#168100=CARTESIAN_POINT('Ctrl Pts',(54.580193757424,-31.2035143279539,40.0255394551374));
#168101=CARTESIAN_POINT('Ctrl Pts',(54.582845146023,-31.21481784858,40.0382021526047));
#168102=CARTESIAN_POINT('Ctrl Pts',(54.5847026428005,-31.2268820501984,
40.0503687782074));
#168103=CARTESIAN_POINT('Ctrl Pts',(54.5856859723272,-31.2396897946771,
40.0619155352442));
#168104=CARTESIAN_POINT('Ctrl Pts',(54.5856885494585,-31.2397233614912,
40.0619457972351));
#168105=CARTESIAN_POINT('Ctrl Pts',(54.5856911200402,-31.2397569340482,
40.0619760547304));
#168106=CARTESIAN_POINT('Ctrl Pts',(54.5856936840716,-31.2397905123448,
40.0620063077269));
#168107=CARTESIAN_POINT('Ctrl Pts',(54.5859686003825,-31.2433907885844,
40.06525004417));
#168108=CARTESIAN_POINT('Ctrl Pts',(54.5861671393376,-31.2470554817642,
40.0684393223556));
#168109=CARTESIAN_POINT('Ctrl Pts',(54.5862889570923,-31.2507796687839,
40.0715697951759));
#168110=CARTESIAN_POINT('Ctrl Pts',(54.5869668451994,-31.2715039227768,
40.0889901646418));
#168111=CARTESIAN_POINT('Ctrl Pts',(54.5852738987621,-31.294070303672,40.1045963098239));
#168112=CARTESIAN_POINT('Ctrl Pts',(54.5811905703967,-31.3175919772521,
40.117663465072));
#168113=CARTESIAN_POINT('Ctrl Pts',(54.5793579160789,-31.3281488300913,
40.123528185306));
#168114=CARTESIAN_POINT('Ctrl Pts',(54.5770440083384,-31.3388983725505,
40.1288820140919));
#168115=CARTESIAN_POINT('Ctrl Pts',(54.5742478788459,-31.3497625287428,
40.1336621774101));
#168116=CARTESIAN_POINT('Ctrl Pts',(54.5730327187888,-31.3544839440758,
40.1357395717319));
#168117=CARTESIAN_POINT('Ctrl Pts',(54.5717264106368,-31.3592268152913,
40.1377083672884));
#168118=CARTESIAN_POINT('Ctrl Pts',(54.5703288332446,-31.363984610047,40.1395632548792));
#168119=CARTESIAN_POINT('Ctrl Pts',(54.5654373123719,-31.380636891692,40.146055361447));
#168120=CARTESIAN_POINT('Ctrl Pts',(54.559427740509,-31.3974719850962,40.1511520974629));
#168121=CARTESIAN_POINT('Ctrl Pts',(54.5522949389285,-31.4142098249417,
40.1546258197408));
#168122=CARTESIAN_POINT('Ctrl Pts',(54.5487285381383,-31.4225787448644,
40.1563626808798));
#168123=CARTESIAN_POINT('Ctrl Pts',(54.5448813304464,-31.4309233516993,
40.1576937882008));
#168124=CARTESIAN_POINT('Ctrl Pts',(54.5407526753747,-31.4392086412363,
40.1585906813668));
#168125=CARTESIAN_POINT('Ctrl Pts',(54.5386883478389,-31.4433512860048,
40.1590391279498));
#168126=CARTESIAN_POINT('Ctrl Pts',(54.5365536585648,-31.4474791015105,
40.1593790209175));
#168127=CARTESIAN_POINT('Ctrl Pts',(54.5343485280976,-31.4515877125783,
40.1596068022931));
#168128=CARTESIAN_POINT('Ctrl Pts',(54.5321433976304,-31.455696323646,40.1598345836687));
#168129=CARTESIAN_POINT('Ctrl Pts',(54.5298678244924,-31.459785729423,40.1599502506864));
#168130=CARTESIAN_POINT('Ctrl Pts',(54.5275217339719,-31.4638515574741,
40.1599502534424));
#168131=CARTESIAN_POINT('',(54.5122556166611,-31.4902932482908,40.1599502534424));
#168132=CARTESIAN_POINT('Origin',(5.52060867199534E-15,5.77259090966498E-15,
40.1599502534424));
#168133=CARTESIAN_POINT('',(54.1966007261207,-31.6576696180585,39.8576902534424));
#168134=CARTESIAN_POINT('Ctrl Pts',(54.512255616661,-31.4902932482908,40.1599502534424));
#168135=CARTESIAN_POINT('Ctrl Pts',(54.510344000441,-31.4936024004372,40.1599502447858));
#168136=CARTESIAN_POINT('Ctrl Pts',(54.5083962906204,-31.4968786114293,
40.1598744685927));
#168137=CARTESIAN_POINT('Ctrl Pts',(54.5064144237356,-31.5001207716285,
40.1597246934279));
#168138=CARTESIAN_POINT('Ctrl Pts',(54.4949616780398,-31.5188564579403,
40.1588591777435));
#168139=CARTESIAN_POINT('Ctrl Pts',(54.4823684499334,-31.5364583843189,
40.1555254706019));
#168140=CARTESIAN_POINT('Ctrl Pts',(54.4690111814099,-31.5527059087832,
40.1500631826378));
#168141=CARTESIAN_POINT('Ctrl Pts',(54.4636238877451,-31.5592589091562,
40.1478601162479));
#168142=CARTESIAN_POINT('Ctrl Pts',(54.4581123526903,-31.5655920544886,
40.1453112228306));
#168143=CARTESIAN_POINT('Ctrl Pts',(54.4525012314185,-31.5716927188399,
40.1424401896328));
#168144=CARTESIAN_POINT('Ctrl Pts',(54.4504310683346,-31.5739434935987,
40.1413809526906));
#168145=CARTESIAN_POINT('Ctrl Pts',(54.4483473527934,-31.5761624901351,
40.1402777640511));
#168146=CARTESIAN_POINT('Ctrl Pts',(54.4462513257026,-31.5783490084907,
40.1391317641987));
#168147=CARTESIAN_POINT('Ctrl Pts',(54.4423212749073,-31.5824487304076,
40.1369830144753));
#168148=CARTESIAN_POINT('Ctrl Pts',(54.4383479413154,-31.5864342712171,
40.1346837565849));
#168149=CARTESIAN_POINT('Ctrl Pts',(54.4343395048294,-31.590301016987,40.1322415082996));
#168150=CARTESIAN_POINT('Ctrl Pts',(54.4203099771284,-31.6038346271819,
40.1236936393008));
#168151=CARTESIAN_POINT('Ctrl Pts',(54.4058504350957,-31.6159129958987,
40.113394140767));
#168152=CARTESIAN_POINT('Ctrl Pts',(54.3913116139986,-31.6263383134317,
40.101665321223));
#168153=CARTESIAN_POINT('Ctrl Pts',(54.38404220345,-31.6315509721983,40.095800911451));
#168154=CARTESIAN_POINT('Ctrl Pts',(54.3767529740103,-31.6363503686737,
40.0895791707949));
#168155=CARTESIAN_POINT('Ctrl Pts',(54.3694877752603,-31.6407117811305,
40.0830403822906));
#168156=CARTESIAN_POINT('Ctrl Pts',(54.3658551758852,-31.6428924873589,
40.0797709880385));
#168157=CARTESIAN_POINT('Ctrl Pts',(54.3622285842838,-31.6449636976422,
40.0764223317514));
#168158=CARTESIAN_POINT('Ctrl Pts',(54.3586134821116,-31.6469223220353,
40.0729994484778));
#168159=CARTESIAN_POINT('Ctrl Pts',(54.3549983799394,-31.6488809464285,
40.0695765652042));
#168160=CARTESIAN_POINT('Ctrl Pts',(54.3513947831121,-31.65072685634,40.0660793733488));
#168161=CARTESIAN_POINT('Ctrl Pts',(54.3478081421437,-31.6524572252917,
40.0625130768817));
#168162=CARTESIAN_POINT('Ctrl Pts',(54.3477775556079,-31.6524719817149,
40.0624826638418));
#168163=CARTESIAN_POINT('Ctrl Pts',(54.34774697044,-31.6524867297705,40.0624522459912));
#168164=CARTESIAN_POINT('Ctrl Pts',(54.3477163866431,-31.6525014694575,
40.0624218233329));
#168165=CARTESIAN_POINT('Ctrl Pts',(54.3320967950454,-31.6600292427979,
40.0468845275897));
#168166=CARTESIAN_POINT('Ctrl Pts',(54.3168578829681,-31.665504315279,40.0302263329234));
#168167=CARTESIAN_POINT('Ctrl Pts',(54.3021370826333,-31.6690725678684,
40.0127515884738));
#168168=CARTESIAN_POINT('Ctrl Pts',(54.2869184346062,-31.672761496391,39.9946858597706));
#168169=CARTESIAN_POINT('Ctrl Pts',(54.2722526596743,-31.6744122539939,
39.9757460620476));
#168170=CARTESIAN_POINT('Ctrl Pts',(54.2583037507945,-31.6741352403912,
39.9562444559111));
#168171=CARTESIAN_POINT('Ctrl Pts',(54.2446201795132,-31.6738634961701,
39.9371138113589));
#168172=CARTESIAN_POINT('Ctrl Pts',(54.2316257183445,-31.671736065781,39.9174410654326));
#168173=CARTESIAN_POINT('Ctrl Pts',(54.2194985998743,-31.6678154208136,
39.8975196504113));
#168174=CARTESIAN_POINT('Ctrl Pts',(54.2114648090467,-31.6652181309748,
39.8843224113753));
#168175=CARTESIAN_POINT('Ctrl Pts',(54.2038121508392,-31.6618330358508,
39.871016044712));
#168176=CARTESIAN_POINT('Ctrl Pts',(54.1966007261207,-31.6576696180585,
39.8576902534424));
#168177=CARTESIAN_POINT('',(53.888035839597,-31.479523201679,39.2875012672119));
#168178=CARTESIAN_POINT('',(54.1966007261207,-31.6576696180585,39.8576902534424));
#168179=CARTESIAN_POINT('',(50.6762142289948,-36.4252947698679,39.2875012672119));
#168180=CARTESIAN_POINT('Origin',(5.53234440788222E-15,0.,39.2875012672119));
#168181=CARTESIAN_POINT('',(50.9644637245892,-36.6347241449655,39.8576902534424));
#168182=CARTESIAN_POINT('',(50.6762142289948,-36.4252947698679,39.2875012672119));
#168183=CARTESIAN_POINT('',(50.9399462128201,-36.9911673391708,40.1599502534424));
#168184=CARTESIAN_POINT('Ctrl Pts',(50.9644637245892,-36.6347241449655,
39.8576902534424));
#168185=CARTESIAN_POINT('Ctrl Pts',(50.9744193574531,-36.641957498789,39.8773836120347));
#168186=CARTESIAN_POINT('Ctrl Pts',(50.9831959997515,-36.6507449107773,
39.8969946442099));
#168187=CARTESIAN_POINT('Ctrl Pts',(50.9907013072115,-36.6609215604507,
39.9162525288192));
#168188=CARTESIAN_POINT('Ctrl Pts',(50.9983574255548,-36.6713026986859,
39.9358973793998));
#168189=CARTESIAN_POINT('Ctrl Pts',(51.0046913806523,-36.6831299757284,
39.9551762199659));
#168190=CARTESIAN_POINT('Ctrl Pts',(51.0095813473133,-36.6962763075813,
39.9738152034147));
#168191=CARTESIAN_POINT('Ctrl Pts',(51.0142813432023,-36.7089119163592,
39.9917300792533));
#168192=CARTESIAN_POINT('Ctrl Pts',(51.0176477981081,-36.7227668523472,
40.0090551157996));
#168193=CARTESIAN_POINT('Ctrl Pts',(51.01954234395,-36.7377619899041,40.0255394551396));
#168194=CARTESIAN_POINT('Ctrl Pts',(51.0209976683241,-36.7492807342367,
40.0382021526061));
#168195=CARTESIAN_POINT('Ctrl Pts',(51.021583937084,-36.7614730081793,40.0503687782081));
#168196=CARTESIAN_POINT('Ctrl Pts',(51.0212231059804,-36.7743133764172,
40.0619155352442));
#168197=CARTESIAN_POINT('Ctrl Pts',(51.0212221603065,-36.7743470287324,
40.0619457972351));
#168198=CARTESIAN_POINT('Ctrl Pts',(51.0212212075184,-36.7743806860744,
40.0619760547304));
#168199=CARTESIAN_POINT('Ctrl Pts',(51.021220247616,-36.7744143484398,40.0620063077269));
#168200=CARTESIAN_POINT('Ctrl Pts',(51.021117326564,-36.778023638569,40.06525004417));
#168201=CARTESIAN_POINT('Ctrl Pts',(51.0209317131555,-36.7816890091479,
40.0684393223556));
#168202=CARTESIAN_POINT('Ctrl Pts',(51.0206635800337,-36.7854055281042,
40.0715697951759));
#168203=CARTESIAN_POINT('Ctrl Pts',(51.0191714801764,-36.8060871110687,
40.0889901646429));
#168204=CARTESIAN_POINT('Ctrl Pts',(51.01512897876,-36.8283529098803,40.1045963098259));
#168205=CARTESIAN_POINT('Ctrl Pts',(51.008609334901,-36.8513189052339,40.1176634650745));
#168206=CARTESIAN_POINT('Ctrl Pts',(51.0056832284514,-36.8616263619877,
40.1235281853075));
#168207=CARTESIAN_POINT('Ctrl Pts',(51.0022583633859,-36.8720751481068,
40.1288820140926));
#168208=CARTESIAN_POINT('Ctrl Pts',(50.9983419378324,-36.8825875141943,
40.1336621774101));
#168209=CARTESIAN_POINT('Ctrl Pts',(50.9966399122601,-36.8871560463067,
40.1357395717319));
#168210=CARTESIAN_POINT('Ctrl Pts',(50.9948449951612,-36.8917363891938,
40.1377083672884));
#168211=CARTESIAN_POINT('Ctrl Pts',(50.9929577488698,-36.8963220336349,
40.1395632548792));
#168212=CARTESIAN_POINT('Ctrl Pts',(50.98635238685,-36.9123717891788,40.146055361447));
#168213=CARTESIAN_POINT('Ctrl Pts',(50.9786159896081,-36.9284864868682,
40.151152097463));
#168214=CARTESIAN_POINT('Ctrl Pts',(50.9697726815835,-36.9443870542876,
40.1546258197409));
#168215=CARTESIAN_POINT('Ctrl Pts',(50.9653510275712,-36.9523373379973,
40.1563626808798));
#168216=CARTESIAN_POINT('Ctrl Pts',(50.9606526463565,-36.960234089495,40.1576937882008));
#168217=CARTESIAN_POINT('Ctrl Pts',(50.9556805599063,-36.968042429379,40.1585906813668));
#168218=CARTESIAN_POINT('Ctrl Pts',(50.9531945166812,-36.9719465993211,
40.1590391279498));
#168219=CARTESIAN_POINT('Ctrl Pts',(50.9506400472468,-36.9758286664321,
40.1593790209175));
#168220=CARTESIAN_POINT('Ctrl Pts',(50.948017529914,-36.9796842711995,40.1596068022931));
#168221=CARTESIAN_POINT('Ctrl Pts',(50.9453950125812,-36.9835398759669,
40.1598345836687));
#168222=CARTESIAN_POINT('Ctrl Pts',(50.9427044459693,-36.987369017388,40.1599502506864));
#168223=CARTESIAN_POINT('Ctrl Pts',(50.9399462128201,-36.9911673391708,
40.1599502534424));
#168224=CARTESIAN_POINT('',(50.9219998155899,-37.015868435856,40.1599502534424));
#168225=CARTESIAN_POINT('Origin',(5.52946850001198E-15,5.78623384841323E-15,
40.1599502534424));
#168226=CARTESIAN_POINT('',(50.5905785208484,-37.1493329797261,39.8576902534424));
#168227=CARTESIAN_POINT('Ctrl Pts',(50.9219998155899,-37.015868435856,40.1599502534424));
#168228=CARTESIAN_POINT('Ctrl Pts',(50.919752770815,-37.0189596418149,40.1599502447858));
#168229=CARTESIAN_POINT('Ctrl Pts',(50.9174732734523,-37.0220143142659,
40.1598744685927));
#168230=CARTESIAN_POINT('Ctrl Pts',(50.9151633654183,-37.0250315520725,
40.1597246934279));
#168231=CARTESIAN_POINT('Ctrl Pts',(50.9018149465639,-37.0424674644257,
40.1588591777435));
#168232=CARTESIAN_POINT('Ctrl Pts',(50.8874508031645,-37.0586566148276,
40.1555254706022));
#168233=CARTESIAN_POINT('Ctrl Pts',(50.8724683783922,-37.0734189189002,
40.1500631826386));
#168234=CARTESIAN_POINT('Ctrl Pts',(50.8664256218263,-37.0793728957243,
40.1478601162485));
#168235=CARTESIAN_POINT('Ctrl Pts',(50.8602822855873,-37.085095235135,40.1453112228309));
#168236=CARTESIAN_POINT('Ctrl Pts',(50.8540642095546,-37.0905759575255,
40.1424401896328));
#168237=CARTESIAN_POINT('Ctrl Pts',(50.851770117014,-37.0925980113388,40.1413809526905));
#168238=CARTESIAN_POINT('Ctrl Pts',(50.8494658679866,-37.0945870443967,
40.1402777640511));
#168239=CARTESIAN_POINT('Ctrl Pts',(50.8471527697479,-37.0965424902852,
40.1391317641987));
#168240=CARTESIAN_POINT('Ctrl Pts',(50.8428157105503,-37.1002089513262,
40.1369830144753));
#168241=CARTESIAN_POINT('Ctrl Pts',(50.8384475408394,-37.1037573324717,
40.1346837565849));
#168242=CARTESIAN_POINT('Ctrl Pts',(50.8340568779947,-37.1071839000978,
40.1322415082996));
#168243=CARTESIAN_POINT('Ctrl Pts',(50.8186895580382,-37.119176886789,40.1236936393008));
#168244=CARTESIAN_POINT('Ctrl Pts',(50.803046693569,-37.12967765523,40.113394140767));
#168245=CARTESIAN_POINT('Ctrl Pts',(50.7874977752343,-37.1385261411558,
40.101665321223));
#168246=CARTESIAN_POINT('Ctrl Pts',(50.7797233160669,-37.1429503841186,
40.095800911451));
#168247=CARTESIAN_POINT('Ctrl Pts',(50.7719723442506,-37.1469615570463,
40.0895791707949));
#168248=CARTESIAN_POINT('Ctrl Pts',(50.7642910532777,-37.1505396571686,
40.0830403822906));
#168249=CARTESIAN_POINT('Ctrl Pts',(50.7604504077912,-37.1523287072298,
40.0797709880385));
#168250=CARTESIAN_POINT('Ctrl Pts',(50.75662718261,-37.1540094891595,40.0764223317514));
#168251=CARTESIAN_POINT('Ctrl Pts',(50.7528271523479,-37.1555795029286,
40.0729994484778));
#168252=CARTESIAN_POINT('Ctrl Pts',(50.7490271220858,-37.1571495166978,
40.0695765652042));
#168253=CARTESIAN_POINT('Ctrl Pts',(50.7452503160124,-37.1586086360831,
40.0660793733488));
#168254=CARTESIAN_POINT('Ctrl Pts',(50.7415024502312,-37.1599546198238,
40.0625130768817));
#168255=CARTESIAN_POINT('Ctrl Pts',(50.7414704887854,-37.1599660982462,
40.0624826638418));
#168256=CARTESIAN_POINT('Ctrl Pts',(50.7414385295747,-37.1599775684899,
40.0624522459912));
#168257=CARTESIAN_POINT('Ctrl Pts',(50.7414065726022,-37.159989030554,40.0624218233329));
#168258=CARTESIAN_POINT('Ctrl Pts',(50.7250856801828,-37.1658428740577,
40.0468845275901));
#168259=CARTESIAN_POINT('Ctrl Pts',(50.709357947548,-37.1696950534575,40.0302263329242));
#168260=CARTESIAN_POINT('Ctrl Pts',(50.6943448053384,-37.1717050161488,
40.012751588475));
#168261=CARTESIAN_POINT('Ctrl Pts',(50.6788239286281,-37.1737829544436,
39.994685859772));
#168262=CARTESIAN_POINT('Ctrl Pts',(50.6640659431905,-37.1738916781074,
39.9757460620494));
#168263=CARTESIAN_POINT('Ctrl Pts',(50.6502224036994,-37.1721581240049,
39.9562444559131));
#168264=CARTESIAN_POINT('Ctrl Pts',(50.636642197459,-37.1704575457491,39.9371138113609));
#168265=CARTESIAN_POINT('Ctrl Pts',(50.6239412983375,-37.1669834785894,
39.9174410654346));
#168266=CARTESIAN_POINT('Ctrl Pts',(50.6122904324844,-37.161816682268,39.8975196504132));
#168267=CARTESIAN_POINT('Ctrl Pts',(50.6045721423186,-37.1583938608452,
39.8843224113766));
#168268=CARTESIAN_POINT('Ctrl Pts',(50.5973152449644,-37.154227389024,39.8710160447127));
#168269=CARTESIAN_POINT('Ctrl Pts',(50.5905785208484,-37.1493329797261,
39.8576902534424));
#168270=CARTESIAN_POINT('',(50.3023253561995,-36.9399086546487,39.2875012672119));
#168271=CARTESIAN_POINT('',(50.5905785208484,-37.1493329797261,39.8576902534424));
#168272=CARTESIAN_POINT('',(46.5911245387429,-41.5228599914563,39.2875012672119));
#168273=CARTESIAN_POINT('Origin',(5.53234440788222E-15,0.,39.2875012672119));
#168274=CARTESIAN_POINT('',(46.8559036426985,-41.7612723673363,39.8576902534424));
#168275=CARTESIAN_POINT('',(46.5911245387429,-41.5228599914563,39.2875012672119));
#168276=CARTESIAN_POINT('',(46.7942619810916,-42.1132001506002,40.1599502534424));
#168277=CARTESIAN_POINT('Ctrl Pts',(46.8559036426985,-41.7612723673363,
39.8576902534424));
#168278=CARTESIAN_POINT('Ctrl Pts',(46.8650486462049,-41.7695067430954,
39.877383612036));
#168279=CARTESIAN_POINT('Ctrl Pts',(46.8728586744677,-41.7791634256542,
39.8969946442124));
#168280=CARTESIAN_POINT('Ctrl Pts',(46.8792591175167,-41.7900688448319,
39.9162525288229));
#168281=CARTESIAN_POINT('Ctrl Pts',(46.8857881704163,-41.8011933963915,
39.9358973794046));
#168282=CARTESIAN_POINT('Ctrl Pts',(46.8908511403511,-41.8136179609666,
39.9551762199718));
#168283=CARTESIAN_POINT('Ctrl Pts',(46.8943401533967,-41.8272034165397,
39.9738152034217));
#168284=CARTESIAN_POINT('Ctrl Pts',(46.8976936214484,-41.8402610894794,
39.9917300792612));
#168285=CARTESIAN_POINT('Ctrl Pts',(46.8995933993941,-41.8543920170376,
40.0090551158084));
#168286=CARTESIAN_POINT('Ctrl Pts',(46.8999101480297,-41.8695030436287,
40.0255394551492));
#168287=CARTESIAN_POINT('Ctrl Pts',(46.9001534633402,-41.8811108098924,
40.0382021526122));
#168288=CARTESIAN_POINT('Ctrl Pts',(46.8994620807995,-41.8932975750523,
40.050368778211));
#168289=CARTESIAN_POINT('Ctrl Pts',(46.8977610424072,-41.9060298852855,
40.0619155352442));
#168290=CARTESIAN_POINT('Ctrl Pts',(46.8977565842889,-41.9060632544,40.0619457972351));
#168291=CARTESIAN_POINT('Ctrl Pts',(46.8977521185701,-41.90609662777,40.0619760547305));
#168292=CARTESIAN_POINT('Ctrl Pts',(46.8977476452508,-41.9061300053924,
40.0620063077269));
#168293=CARTESIAN_POINT('Ctrl Pts',(46.8972680144604,-41.9097087652732,
40.06525004417));
#168294=CARTESIAN_POINT('Ctrl Pts',(46.8967002823076,-41.9133346546842,
40.0684393223556));
#168295=CARTESIAN_POINT('Ctrl Pts',(46.8960451360319,-41.9170027866176,
40.0715697951759));
#168296=CARTESIAN_POINT('Ctrl Pts',(46.8923993959694,-41.9374151067973,
40.0889901646393));
#168297=CARTESIAN_POINT('Ctrl Pts',(46.8860516300673,-41.9591363747677,
40.1045963098194));
#168298=CARTESIAN_POINT('Ctrl Pts',(46.8771671013008,-41.9812950716373,
40.1176634650663));
#168299=CARTESIAN_POINT('Ctrl Pts',(46.8731796017524,-41.9912402016585,
40.1235281853025));
#168300=CARTESIAN_POINT('Ctrl Pts',(46.8686813028982,-42.0012737523564,
40.1288820140903));
#168301=CARTESIAN_POINT('Ctrl Pts',(46.863687490459,-42.0113191526625,40.1336621774101));
#168302=CARTESIAN_POINT('Ctrl Pts',(46.8615172471197,-42.0156847477605,
40.1357395717319));
#168303=CARTESIAN_POINT('Ctrl Pts',(46.8592533865613,-42.020052379124,40.1377083672883));
#168304=CARTESIAN_POINT('Ctrl Pts',(46.8568971484361,-42.0244156319704,
40.1395632548791));
#168305=CARTESIAN_POINT('Ctrl Pts',(46.8486503149976,-42.0396870169328,
40.1460553614469));
#168306=CARTESIAN_POINT('Ctrl Pts',(46.8392718539638,-42.0549047629073,
40.1511520974629));
#168307=CARTESIAN_POINT('Ctrl Pts',(46.8288149286284,-42.0697938479567,
40.1546258197408));
#168308=CARTESIAN_POINT('Ctrl Pts',(46.8235864659607,-42.0772383904814,
40.1563626808798));
#168309=CARTESIAN_POINT('Ctrl Pts',(46.8180883876711,-42.0846007681799,
40.1576937882008));
#168310=CARTESIAN_POINT('Ctrl Pts',(46.8123273450619,-42.0918466086052,
40.1585906813668));
#168311=CARTESIAN_POINT('Ctrl Pts',(46.8094468237573,-42.0954695288179,
40.1590391279498));
#168312=CARTESIAN_POINT('Ctrl Pts',(46.8065005614644,-42.0990633147947,
40.1593790209175));
#168313=CARTESIAN_POINT('Ctrl Pts',(46.8034893901146,-42.102623670449,40.1596068022931));
#168314=CARTESIAN_POINT('Ctrl Pts',(46.8004782187648,-42.1061840261034,
40.1598345836687));
#168315=CARTESIAN_POINT('Ctrl Pts',(46.79740213709,-42.1097109502939,40.1599502506865));
#168316=CARTESIAN_POINT('Ctrl Pts',(46.7942619810916,-42.1132001506002,
40.1599502534424));
#168317=CARTESIAN_POINT('',(46.7738319284257,-42.1358900227696,40.1599502534424));
#168318=CARTESIAN_POINT('Origin',(5.53970586838553E-15,5.79887594550813E-15,
40.1599502534424));
#168319=CARTESIAN_POINT('',(46.4302753505424,-42.2339804752702,39.8576902534424));
#168320=CARTESIAN_POINT('Ctrl Pts',(46.7738319284257,-42.1358900227696,
40.1599502534424));
#168321=CARTESIAN_POINT('Ctrl Pts',(46.7712740741886,-42.1387294146415,
40.1599502447857));
#168322=CARTESIAN_POINT('Ctrl Pts',(46.7686877639338,-42.1415290809209,
40.1598744685927));
#168323=CARTESIAN_POINT('Ctrl Pts',(46.7660751225865,-42.144288338846,40.1597246934279));
#168324=CARTESIAN_POINT('Ctrl Pts',(46.7509772786445,-42.1602334457358,
40.1588591777436));
#168325=CARTESIAN_POINT('Ctrl Pts',(46.7349995965139,-42.1748324484412,
40.1555254706028));
#168326=CARTESIAN_POINT('Ctrl Pts',(46.7185561660745,-42.1879477932292,
40.1500631826399));
#168327=CARTESIAN_POINT('Ctrl Pts',(46.7119241523123,-42.1932375134886,
40.1478601162495));
#168328=CARTESIAN_POINT('Ctrl Pts',(46.7052163225658,-42.1982863518299,
40.1453112228315));
#168329=CARTESIAN_POINT('Ctrl Pts',(46.6984594183138,-42.2030870843185,
40.1424401896328));
#168330=CARTESIAN_POINT('Ctrl Pts',(46.6959665308745,-42.2048582631416,
40.1413809526906));
#168331=CARTESIAN_POINT('Ctrl Pts',(46.6934669941954,-42.2065955404584,
40.1402777640511));
#168332=CARTESIAN_POINT('Ctrl Pts',(46.6909621675971,-42.2082984896054,
40.1391317641987));
#168333=CARTESIAN_POINT('Ctrl Pts',(46.6862656177254,-42.2114915192562,
40.1369830144753));
#168334=CARTESIAN_POINT('Ctrl Pts',(46.6815504704771,-42.2145638639314,
40.134683756585));
#168335=CARTESIAN_POINT('Ctrl Pts',(46.6768256862946,-42.2175127112216,
40.1322415082996));
#168336=CARTESIAN_POINT('Ctrl Pts',(46.6602889416559,-42.2278336767372,
40.1236936393009));
#168337=CARTESIAN_POINT('Ctrl Pts',(46.6436341412467,-42.236641796286,40.113394140767));
#168338=CARTESIAN_POINT('Ctrl Pts',(46.6272454828774,-42.243816504741,40.101665321223));
#168339=CARTESIAN_POINT('Ctrl Pts',(46.6190511536928,-42.2474038589685,
40.095800911451));
#168340=CARTESIAN_POINT('Ctrl Pts',(46.610923360769,-42.2505828610984,40.0895791707949));
#168341=CARTESIAN_POINT('Ctrl Pts',(46.6029101354046,-42.2533384464725,
40.0830403822906));
#168342=CARTESIAN_POINT('Ctrl Pts',(46.5989035227223,-42.2547162391596,
40.0797709880385));
#168343=CARTESIAN_POINT('Ctrl Pts',(46.5949255520165,-42.2559881777371,
40.0764223317514));
#168344=CARTESIAN_POINT('Ctrl Pts',(46.5909822275911,-42.2571523794829,
40.0729994484778));
#168345=CARTESIAN_POINT('Ctrl Pts',(46.5870389031658,-42.2583165812286,
40.0695765652042));
#168346=CARTESIAN_POINT('Ctrl Pts',(46.5831302673242,-42.2593729236704,
40.0660793733488));
#168347=CARTESIAN_POINT('Ctrl Pts',(46.5792622391319,-42.2603197753207,
40.0625130768817));
#168348=CARTESIAN_POINT('Ctrl Pts',(46.5792292529523,-42.2603278499823,
40.0624826638418));
#168349=CARTESIAN_POINT('Ctrl Pts',(46.5791962698506,-42.2603359167436,
40.0624522459912));
#168350=CARTESIAN_POINT('Ctrl Pts',(46.5791632898298,-42.2603439756041,
40.0624218233329));
#168351=CARTESIAN_POINT('Ctrl Pts',(46.5623199117009,-42.264459753337,40.0468845275898));
#168352=CARTESIAN_POINT('Ctrl Pts',(46.5462756748379,-42.2666468343719,
40.0302263329236));
#168353=CARTESIAN_POINT('Ctrl Pts',(46.5311346778806,-42.2670764855932,
40.0127515884741));
#168354=CARTESIAN_POINT('Ctrl Pts',(46.51548162246,-42.2675206673335,39.9946858597709));
#168355=CARTESIAN_POINT('Ctrl Pts',(46.5007931180932,-42.2660861658588,
39.975746062048));
#168356=CARTESIAN_POINT('Ctrl Pts',(46.4872066207061,-42.2629150644377,
39.9562444559114));
#168357=CARTESIAN_POINT('Ctrl Pts',(46.4738785670881,-42.2598042840382,
39.9371138113589));
#168358=CARTESIAN_POINT('Ctrl Pts',(46.4616103837223,-42.2550216427145,
39.9174410654322));
#168359=CARTESIAN_POINT('Ctrl Pts',(46.4505634198108,-42.2486653035403,
39.8975196504106));
#168360=CARTESIAN_POINT('Ctrl Pts',(46.44324519351,-42.2444544516815,39.8843224113748));
#168361=CARTESIAN_POINT('Ctrl Pts',(46.436463565096,-42.2395522519007,39.8710160447118));
#168362=CARTESIAN_POINT('Ctrl Pts',(46.4302753505424,-42.2339804752702,
39.8576902534424));
#168363=CARTESIAN_POINT('',(46.1654920697611,-41.9955727382252,39.2875012672119));
#168364=CARTESIAN_POINT('',(46.4302753505424,-42.2339804752702,39.8576902534424));
#168365=CARTESIAN_POINT('',(41.995572738225,-46.1654920697613,39.2875012672119));
#168366=CARTESIAN_POINT('Origin',(5.53234440788222E-15,0.,39.2875012672119));
#168367=CARTESIAN_POINT('',(42.23398047527,-46.4302753505426,39.8576902534424));
#168368=CARTESIAN_POINT('',(41.995572738225,-46.1654920697613,39.2875012672119));
#168369=CARTESIAN_POINT('',(42.1358900227694,-46.7738319284258,40.1599502534424));
#168370=CARTESIAN_POINT('Ctrl Pts',(42.23398047527,-46.4302753505426,39.8576902534424));
#168371=CARTESIAN_POINT('Ctrl Pts',(42.2422146548454,-46.439420530692,39.8773836120339));
#168372=CARTESIAN_POINT('Ctrl Pts',(42.2489725007673,-46.4498406831845,
39.8969946442083));
#168373=CARTESIAN_POINT('Ctrl Pts',(42.2541979548115,-46.4613553898097,
39.9162525288168));
#168374=CARTESIAN_POINT('Ctrl Pts',(42.2595284085967,-46.4731014717765,
39.9358973793964));
#168375=CARTESIAN_POINT('Ctrl Pts',(42.2632649224108,-46.4859871977518,
39.9551762199615));
#168376=CARTESIAN_POINT('Ctrl Pts',(42.2653147554845,-46.4998629319477,
39.9738152034094));
#168377=CARTESIAN_POINT('Ctrl Pts',(42.2672849544016,-46.5131996064485,
39.9917300792466));
#168378=CARTESIAN_POINT('Ctrl Pts',(42.2676972410237,-46.5274517041735,
40.0090551157917));
#168379=CARTESIAN_POINT('Ctrl Pts',(42.2664327220907,-46.5425130602251,
40.0255394551308));
#168380=CARTESIAN_POINT('Ctrl Pts',(42.2654613625255,-46.5540826713113,
40.0382021526004));
#168381=CARTESIAN_POINT('Ctrl Pts',(42.2634999036159,-46.5661304069476,
40.0503687782054));
#168382=CARTESIAN_POINT('Ctrl Pts',(42.2604772948659,-46.5786151613301,
40.0619155352442));
#168383=CARTESIAN_POINT('Ctrl Pts',(42.2604693731474,-46.5786478816448,
40.0619457972351));
#168384=CARTESIAN_POINT('Ctrl Pts',(42.2604614434252,-46.5786806053973,
40.0619760547304));
#168385=CARTESIAN_POINT('Ctrl Pts',(42.2604535056997,-46.5787133325844,
40.0620063077269));
#168386=CARTESIAN_POINT('Ctrl Pts',(42.2596024201061,-46.5822223525746,
40.06525004417));
#168387=CARTESIAN_POINT('Ctrl Pts',(42.2586587894014,-46.5857690348146,
40.0684393223556));
#168388=CARTESIAN_POINT('Ctrl Pts',(42.2576238078915,-46.5893485909041,
40.0715697951759));
#168389=CARTESIAN_POINT('Ctrl Pts',(42.2518643711122,-46.6092680066592,
40.0889901646458));
#168390=CARTESIAN_POINT('Ctrl Pts',(42.2432808881705,-46.6302067610441,
40.1045963098309));
#168391=CARTESIAN_POINT('Ctrl Pts',(42.2321288152444,-46.6513153841229,
40.1176634650808));
#168392=CARTESIAN_POINT('Ctrl Pts',(42.2271236104809,-46.6607892264734,
40.1235281853113));
#168393=CARTESIAN_POINT('Ctrl Pts',(42.2216011621471,-46.6702976120563,
40.1288820140942));
#168394=CARTESIAN_POINT('Ctrl Pts',(42.2155846760829,-46.6797659870606,
40.13366217741));
#168395=CARTESIAN_POINT('Ctrl Pts',(42.2129699926169,-46.6838808147706,
40.1357395717318));
#168396=CARTESIAN_POINT('Ctrl Pts',(42.210261991929,-46.6879878819273,40.1377083672883));
#168397=CARTESIAN_POINT('Ctrl Pts',(42.2074625774079,-46.6920809384678,
40.1395632548791));
#168398=CARTESIAN_POINT('Ctrl Pts',(42.1976646265838,-46.7064066363594,
40.1460553614469));
#168399=CARTESIAN_POINT('Ctrl Pts',(42.1867468541397,-46.7205607018095,
40.1511520974629));
#168400=CARTESIAN_POINT('Ctrl Pts',(42.1747908797557,-46.7342751765573,
40.1546258197408));
#168401=CARTESIAN_POINT('Ctrl Pts',(42.1688128925637,-46.7411324139312,
40.1563626808798));
#168402=CARTESIAN_POINT('Ctrl Pts',(42.1625753552954,-46.7478797540798,
40.1576937882008));
#168403=CARTESIAN_POINT('Ctrl Pts',(42.1560884757157,-46.7544837081024,
40.1585906813668));
#168404=CARTESIAN_POINT('Ctrl Pts',(42.1528450359258,-46.7577856851136,
40.1590391279498));
#168405=CARTESIAN_POINT('Ctrl Pts',(42.1495392606406,-46.761051815685,40.1593790209175));
#168406=CARTESIAN_POINT('Ctrl Pts',(42.1461724262973,-46.7642779142247,
40.1596068022931));
#168407=CARTESIAN_POINT('Ctrl Pts',(42.142805591954,-46.7675040127644,40.1598345836687));
#168408=CARTESIAN_POINT('Ctrl Pts',(42.1393776974107,-46.7706900780048,
40.1599502506864));
#168409=CARTESIAN_POINT('Ctrl Pts',(42.1358900227694,-46.7738319284258,
40.1599502534424));
#168410=CARTESIAN_POINT('',(42.1132001506,-46.7942619810918,40.1599502534424));
#168411=CARTESIAN_POINT('Origin',(5.55120861436579E-15,5.81037869148839E-15,
40.1599502534424));
#168412=CARTESIAN_POINT('',(41.7612723673362,-46.8559036426986,39.8576902534424));
#168413=CARTESIAN_POINT('Ctrl Pts',(42.1132001506,-46.7942619810918,40.1599502534424));
#168414=CARTESIAN_POINT('Ctrl Pts',(42.1103595112871,-46.7968184499053,
40.1599502447858));
#168415=CARTESIAN_POINT('Ctrl Pts',(42.1074947242967,-46.7993324362834,
40.1598744685927));
#168416=CARTESIAN_POINT('Ctrl Pts',(42.1046079742813,-46.8018034833197,
40.1597246934279));
#168417=CARTESIAN_POINT('Ctrl Pts',(42.0879261203911,-46.8160830868174,
40.1588591777437));
#168418=CARTESIAN_POINT('Ctrl Pts',(42.0705099543599,-46.8289319920969,
40.1555254706039));
#168419=CARTESIAN_POINT('Ctrl Pts',(42.0527856759201,-46.8402566831377,
40.1500631826426));
#168420=CARTESIAN_POINT('Ctrl Pts',(42.0456370666904,-46.8448241915513,
40.1478601162516));
#168421=CARTESIAN_POINT('Ctrl Pts',(42.0384382358211,-46.8491442126946,
40.1453112228326));
#168422=CARTESIAN_POINT('Ctrl Pts',(42.031216533405,-46.853212357452,40.1424401896328));
#168423=CARTESIAN_POINT('Ctrl Pts',(42.0285521636633,-46.854713255879,40.1413809526905));
#168424=CARTESIAN_POINT('Ctrl Pts',(42.0258847247795,-46.856179743481,40.1402777640511));
#168425=CARTESIAN_POINT('Ctrl Pts',(42.0232156132261,-46.8576115380194,
40.1391317641987));
#168426=CARTESIAN_POINT('Ctrl Pts',(42.0182110290634,-46.8602961527789,
40.1369830144753));
#168427=CARTESIAN_POINT('Ctrl Pts',(42.0132005644175,-46.8628587997325,
40.1346837565849));
#168428=CARTESIAN_POINT('Ctrl Pts',(42.0081934246215,-46.8652976184988,
40.1322415082996));
#168429=CARTESIAN_POINT('Ctrl Pts',(41.9906684353354,-46.8738334841809,
40.1236936393008));
#168430=CARTESIAN_POINT('Ctrl Pts',(41.9731841724648,-46.8808524512363,
40.113394140767));
#168431=CARTESIAN_POINT('Ctrl Pts',(41.9561353316316,-46.8862747746134,
40.101665321223));
#168432=CARTESIAN_POINT('Ctrl Pts',(41.9476109112151,-46.8889859363019,
40.095800911451));
#168433=CARTESIAN_POINT('Ctrl Pts',(41.939195346984,-46.8912979378214,40.0895791707949));
#168434=CARTESIAN_POINT('Ctrl Pts',(41.930937981802,-46.8932008176774,40.0830403822906));
#168435=CARTESIAN_POINT('Ctrl Pts',(41.926809299211,-46.8941522576054,40.0797709880385));
#168436=CARTESIAN_POINT('Ctrl Pts',(41.92272016646,-46.8950014172055,40.0764223317514));
#168437=CARTESIAN_POINT('Ctrl Pts',(41.918676751759,-46.8957470516899,40.0729994484778));
#168438=CARTESIAN_POINT('Ctrl Pts',(41.9146333370581,-46.8964926861744,
40.0695765652042));
#168439=CARTESIAN_POINT('Ctrl Pts',(41.9106356952805,-46.8971346781637,
40.0660793733488));
#168440=CARTESIAN_POINT('Ctrl Pts',(41.9066898836034,-46.8976720238188,
40.0625130768816));
#168441=CARTESIAN_POINT('Ctrl Pts',(41.9066562340936,-46.8976766062519,
40.0624826638418));
#168442=CARTESIAN_POINT('Ctrl Pts',(41.9066225884706,-46.8976811811497,
40.0624522459912));
#168443=CARTESIAN_POINT('Ctrl Pts',(41.9065889467375,-46.897685748512,40.0624218233329));
#168444=CARTESIAN_POINT('Ctrl Pts',(41.889407622474,-46.9000183671518,40.0468845275891));
#168445=CARTESIAN_POINT('Ctrl Pts',(41.873222665399,-46.9005163877045,40.0302263329222));
#168446=CARTESIAN_POINT('Ctrl Pts',(41.8581197016247,-46.899361020107,40.012751588472));
#168447=CARTESIAN_POINT('Ctrl Pts',(41.8425059656445,-46.8981665787446,
39.9946858597683));
#168448=CARTESIAN_POINT('Ctrl Pts',(41.8280478726759,-46.8952045688299,
39.9757460620449));
#168449=CARTESIAN_POINT('Ctrl Pts',(41.8148672739013,-46.8906306633408,
39.9562444559078));
#168450=CARTESIAN_POINT('Ctrl Pts',(41.8019373978504,-46.8861437631587,
39.9371138113554));
#168451=CARTESIAN_POINT('Ctrl Pts',(41.7902363430249,-46.8801049472901,
39.9174410654289));
#168452=CARTESIAN_POINT('Ctrl Pts',(41.7799143139038,-46.8726287066454,
39.8975196504074));
#168453=CARTESIAN_POINT('Ctrl Pts',(41.773076331487,-46.8676759593248,39.8843224113726));
#168454=CARTESIAN_POINT('Ctrl Pts',(41.7668442729534,-46.8620917411111,
39.8710160447107));
#168455=CARTESIAN_POINT('Ctrl Pts',(41.7612723673362,-46.8559036426986,
39.8576902534424));
#168456=CARTESIAN_POINT('',(41.5228599914562,-46.5911245387431,39.2875012672119));
#168457=CARTESIAN_POINT('',(41.7612723673362,-46.8559036426986,39.8576902534424));
#168458=CARTESIAN_POINT('',(36.9399086546485,-50.3023253561996,39.2875012672119));
#168459=CARTESIAN_POINT('Origin',(5.53234440788222E-15,0.,39.2875012672119));
#168460=CARTESIAN_POINT('',(37.149332979726,-50.5905785208485,39.8576902534424));
#168461=CARTESIAN_POINT('',(36.9399086546485,-50.3023253561996,39.2875012672119));
#168462=CARTESIAN_POINT('',(37.0158684358559,-50.9219998155901,40.1599502534424));
#168463=CARTESIAN_POINT('Ctrl Pts',(37.149332979726,-50.5905785208485,39.8576902534424));
#168464=CARTESIAN_POINT('Ctrl Pts',(37.156566119978,-50.6005343088827,39.8773836120369));
#168465=CARTESIAN_POINT('Ctrl Pts',(37.1621977431866,-50.6116037659405,
39.8969946442141));
#168466=CARTESIAN_POINT('Ctrl Pts',(37.1661909570584,-50.6236016024811,
39.9162525288254));
#168467=CARTESIAN_POINT('Ctrl Pts',(37.1702644101629,-50.6358405223268,
39.9358973794081));
#168468=CARTESIAN_POINT('Ctrl Pts',(37.1726335298287,-50.6490462309966,
39.9551762199761));
#168469=CARTESIAN_POINT('Ctrl Pts',(37.1732217245291,-50.6630602183728,
39.9738152034268));
#168470=CARTESIAN_POINT('Ctrl Pts',(37.1737870683986,-50.6765297750435,
39.9917300792672));
#168471=CARTESIAN_POINT('Ctrl Pts',(37.1727073465962,-50.6907468939765,
40.0090551158152));
#168472=CARTESIAN_POINT('Ctrl Pts',(37.1698754144249,-50.7055935641267,
40.0255394551566));
#168473=CARTESIAN_POINT('Ctrl Pts',(37.1677000224016,-50.716998260943,40.038202152617));
#168474=CARTESIAN_POINT('Ctrl Pts',(37.1644899772785,-50.7287749695296,
40.0503687782133));
#168475=CARTESIAN_POINT('Ctrl Pts',(37.1601789145086,-50.7408753824653,
40.0619155352442));
#168476=CARTESIAN_POINT('Ctrl Pts',(37.160167615982,-50.7409070954897,40.0619457972351));
#168477=CARTESIAN_POINT('Ctrl Pts',(37.160156309136,-50.7409388110964,40.0619760547305));
#168478=CARTESIAN_POINT('Ctrl Pts',(37.1601449939716,-50.7409705292822,
40.0620063077269));
#168479=CARTESIAN_POINT('Ctrl Pts',(37.1589317782469,-50.7443713638246,
40.06525004417));
#168480=CARTESIAN_POINT('Ctrl Pts',(37.1576225876056,-50.7477999807007,
40.0684393223556));
#168481=CARTESIAN_POINT('Ctrl Pts',(37.1562191103355,-50.7512517425806,
40.0715697951759));
#168482=CARTESIAN_POINT('Ctrl Pts',(37.1484090784384,-50.7704600126088,
40.088990164639));
#168483=CARTESIAN_POINT('Ctrl Pts',(37.1376839209011,-50.7903868440169,
40.1045963098188));
#168484=CARTESIAN_POINT('Ctrl Pts',(37.1243864882723,-50.8102141227971,
40.1176634650657));
#168485=CARTESIAN_POINT('Ctrl Pts',(37.1184184163579,-50.8191128800934,
40.1235281853021));
#168486=CARTESIAN_POINT('Ctrl Pts',(37.1119323236356,-50.8279919247151,
40.1288820140901));
#168487=CARTESIAN_POINT('Ctrl Pts',(37.1049590818167,-50.8367795369354,
40.1336621774101));
#168488=CARTESIAN_POINT('Ctrl Pts',(37.1019286052431,-50.8405985143441,
40.1357395717319));
#168489=CARTESIAN_POINT('Ctrl Pts',(37.0988061338479,-50.8444000194068,
40.1377083672883));
#168490=CARTESIAN_POINT('Ctrl Pts',(37.0955942139022,-50.8481780352573,
40.1395632548791));
#168491=CARTESIAN_POINT('Ctrl Pts',(37.0843524940921,-50.8614010907341,
40.146055361447));
#168492=CARTESIAN_POINT('Ctrl Pts',(37.0720150276373,-50.8743364007568,
40.1511520974629));
#168493=CARTESIAN_POINT('Ctrl Pts',(37.058690996362,-50.8867260065478,40.1546258197408));
#168494=CARTESIAN_POINT('Ctrl Pts',(37.0520289807244,-50.8929208094433,
40.1563626808798));
#168495=CARTESIAN_POINT('Ctrl Pts',(37.045120324241,-50.8989791867713,40.1576937882008));
#168496=CARTESIAN_POINT('Ctrl Pts',(37.0379786793009,-50.9048689000888,
40.1585906813668));
#168497=CARTESIAN_POINT('Ctrl Pts',(37.0344078568308,-50.9078137567476,
40.1590391279498));
#168498=CARTESIAN_POINT('Ctrl Pts',(37.030778787319,-50.9107164475034,40.1593790209175));
#168499=CARTESIAN_POINT('Ctrl Pts',(37.0270931777238,-50.9135729431178,
40.1596068022931));
#168500=CARTESIAN_POINT('Ctrl Pts',(37.0234075681286,-50.9164294387322,
40.1598345836687));
#168501=CARTESIAN_POINT('Ctrl Pts',(37.019665417447,-50.9192397378251,40.1599502506865));
#168502=CARTESIAN_POINT('Ctrl Pts',(37.0158684358559,-50.92199981559,40.1599502534424));
#168503=CARTESIAN_POINT('',(36.9911673391707,-50.9399462128202,40.1599502534424));
#168504=CARTESIAN_POINT('Origin',(5.56385071146069E-15,5.82061605986194E-15,
40.1599502534424));
#168505=CARTESIAN_POINT('',(36.6347241449654,-50.9644637245894,39.8576902534424));
#168506=CARTESIAN_POINT('Ctrl Pts',(36.9911673391707,-50.9399462128202,
40.1599502534424));
#168507=CARTESIAN_POINT('Ctrl Pts',(36.9880750374206,-50.942191749368,40.1599502447858));
#168508=CARTESIAN_POINT('Ctrl Pts',(36.9849631609003,-50.944392512084,40.1598744685927));
#168509=CARTESIAN_POINT('Ctrl Pts',(36.9818339300542,-50.9465482749232,
40.1597246934279));
#168510=CARTESIAN_POINT('Ctrl Pts',(36.9637508360892,-50.9590059247115,
40.1588591777434));
#168511=CARTESIAN_POINT('Ctrl Pts',(36.9450870013077,-50.9699639572754,
40.1555254706016));
#168512=CARTESIAN_POINT('Ctrl Pts',(36.9262760657617,-50.9793739188881,
40.150063182637));
#168513=CARTESIAN_POINT('Ctrl Pts',(36.9186891827323,-50.9831691728718,
40.1478601162473));
#168514=CARTESIAN_POINT('Ctrl Pts',(36.9110782226468,-50.9867130457559,
40.1453112228302));
#168515=CARTESIAN_POINT('Ctrl Pts',(36.9034708445588,-50.9900040313322,
40.1424401896328));
#168516=CARTESIAN_POINT('Ctrl Pts',(36.9006641839072,-50.9912182052059,
40.1413809526905));
#168517=CARTESIAN_POINT('Ctrl Pts',(36.8978580678373,-50.9923978359479,
40.1402777640511));
#168518=CARTESIAN_POINT('Ctrl Pts',(36.8950539146734,-50.9935427888371,
40.1391317641987));
#168519=CARTESIAN_POINT('Ctrl Pts',(36.8897961274911,-50.9956895755043,
40.1369830144753));
#168520=CARTESIAN_POINT('Ctrl Pts',(36.8845452411468,-50.99771444784,40.134683756585));
#168521=CARTESIAN_POINT('Ctrl Pts',(36.8793106050087,-50.9996165178737,
40.1322415082996));
#168522=CARTESIAN_POINT('Ctrl Pts',(36.8609893785252,-51.0062737629917,
40.1236936393009));
#168523=CARTESIAN_POINT('Ctrl Pts',(36.8428672144359,-51.0114266762819,
40.113394140767));
#168524=CARTESIAN_POINT('Ctrl Pts',(36.8253449818068,-51.0150372064713,
40.101665321223));
#168525=CARTESIAN_POINT('Ctrl Pts',(36.8165838654922,-51.0168424715661,
40.095800911451));
#168526=CARTESIAN_POINT('Ctrl Pts',(36.8079727326366,-51.0182621417027,
40.0895791707949));
#168527=CARTESIAN_POINT('Ctrl Pts',(36.7995616970579,-51.0192914676907,
40.0830403822906));
#168528=CARTESIAN_POINT('Ctrl Pts',(36.7953561792686,-51.0198061306846,
40.0797709880385));
#168529=CARTESIAN_POINT('Ctrl Pts',(36.7912006858666,-51.020223207737,40.0764223317514));
#168530=CARTESIAN_POINT('Ctrl Pts',(36.7871014813876,-51.0205421056327,
40.0729994484778));
#168531=CARTESIAN_POINT('Ctrl Pts',(36.7830022769086,-51.0208610035283,
40.0695765652042));
#168532=CARTESIAN_POINT('Ctrl Pts',(36.7789594281949,-51.0210816112667,
40.0660793733488));
#168533=CARTESIAN_POINT('Ctrl Pts',(36.7749790641714,-51.0212035636551,
40.0625130768817));
#168534=CARTESIAN_POINT('Ctrl Pts',(36.7749451200025,-51.0212046036536,
40.0624826638418));
#168535=CARTESIAN_POINT('Ctrl Pts',(36.7749111804867,-51.0212056365644,
40.0624522459912));
#168536=CARTESIAN_POINT('Ctrl Pts',(36.7748772456271,-51.0212066623876,
40.0624218233329));
#168537=CARTESIAN_POINT('Ctrl Pts',(36.7575462174155,-51.0217305652762,
40.0468845275906));
#168538=CARTESIAN_POINT('Ctrl Pts',(36.7413978659072,-51.0205340689292,
40.0302263329253));
#168539=CARTESIAN_POINT('Ctrl Pts',(36.7264984065494,-51.0178063409627,
40.0127515884767));
#168540=CARTESIAN_POINT('Ctrl Pts',(36.7110950573695,-51.0149863630476,
39.9946858597744));
#168541=CARTESIAN_POINT('Ctrl Pts',(36.6970257816922,-51.0105292970939,
39.9757460620525));
#168542=CARTESIAN_POINT('Ctrl Pts',(36.6843954909291,-51.0046027002037,
39.9562444559169));
#168543=CARTESIAN_POINT('Ctrl Pts',(36.6720054548731,-50.9987888396571,
39.9371138113653));
#168544=CARTESIAN_POINT('Ctrl Pts',(36.6609997277928,-50.9915600117749,
39.9174410654397));
#168545=CARTESIAN_POINT('Ctrl Pts',(36.6515157237725,-50.9830457809177,
39.8975196504191));
#168546=CARTESIAN_POINT('Ctrl Pts',(36.645232903603,-50.97740540147,39.8843224113805));
#168547=CARTESIAN_POINT('Ctrl Pts',(36.6396186946846,-50.9712003466848,
39.8710160447147));
#168548=CARTESIAN_POINT('Ctrl Pts',(36.6347241449654,-50.9644637245894,
39.8576902534424));
#168549=CARTESIAN_POINT('',(36.4252947698678,-50.6762142289949,39.2875012672119));
#168550=CARTESIAN_POINT('',(36.6347241449653,-50.9644637245894,39.8576902534424));
#168551=CARTESIAN_POINT('',(31.4795232016789,-53.8880358395971,39.2875012672119));
#168552=CARTESIAN_POINT('Origin',(5.53234440788222E-15,0.,39.2875012672119));
#168553=CARTESIAN_POINT('',(31.6576696180583,-54.1966007261208,39.8576902534424));
#168554=CARTESIAN_POINT('',(31.4795232016789,-53.8880358395971,39.2875012672119));
#168555=CARTESIAN_POINT('',(31.4902932482907,-54.5122556166612,40.1599502534424));
#168556=CARTESIAN_POINT('Ctrl Pts',(31.6576696180583,-54.1966007261208,
39.8576902534424));
#168557=CARTESIAN_POINT('Ctrl Pts',(31.6638224711874,-54.2072580443422,
39.8773836120376));
#168558=CARTESIAN_POINT('Ctrl Pts',(31.6682661704393,-54.2188555266763,
39.8969946442155));
#168559=CARTESIAN_POINT('Ctrl Pts',(31.6709833936515,-54.231205042323,39.9162525288275));
#168560=CARTESIAN_POINT('Ctrl Pts',(31.67375521647,-54.2438027078788,39.9358973794106));
#168561=CARTESIAN_POINT('Ctrl Pts',(31.6747309854167,-54.2571837147331,
39.9551762199791));
#168562=CARTESIAN_POINT('Ctrl Pts',(31.6738510973601,-54.2711824151086,
39.9738152034302));
#168563=CARTESIAN_POINT('Ctrl Pts',(31.673005392157,-54.2846372786644,39.9917300792704));
#168564=CARTESIAN_POINT('Ctrl Pts',(31.6704454915893,-54.2986636530715,
40.0090551158181));
#168565=CARTESIAN_POINT('Ctrl Pts',(31.6660771734232,-54.3131329740911,
40.0255394551594));
#168566=CARTESIAN_POINT('Ctrl Pts',(31.6627215829929,-54.3242478043989,
40.0382021526188));
#168567=CARTESIAN_POINT('Ctrl Pts',(31.6582981215823,-54.3356244578591,
40.0503687782141));
#168568=CARTESIAN_POINT('Ctrl Pts',(31.6527458376967,-54.3472079546994,
40.0619155352442));
#168569=CARTESIAN_POINT('Ctrl Pts',(31.6527312861508,-54.3472383129789,
40.0619457972351));
#168570=CARTESIAN_POINT('Ctrl Pts',(31.6527167260613,-54.3472686729569,
40.0619760547305));
#168571=CARTESIAN_POINT('Ctrl Pts',(31.6527021574293,-54.3472990346305,
40.0620063077269));
#168572=CARTESIAN_POINT('Ctrl Pts',(31.6511401038187,-54.3505544234701,
40.06525004417));
#168573=CARTESIAN_POINT('Ctrl Pts',(31.6494796970076,-54.3538274103384,
40.0684393223556));
#168574=CARTESIAN_POINT('Ctrl Pts',(31.6477231007679,-54.3571135597833,
40.0715697951759));
#168575=CARTESIAN_POINT('Ctrl Pts',(31.6379480420923,-54.3754002342707,
40.0889901646433));
#168576=CARTESIAN_POINT('Ctrl Pts',(31.6251987170214,-54.3940968201805,
40.1045963098266));
#168577=CARTESIAN_POINT('Ctrl Pts',(31.6099016141331,-54.4124255228592,
40.1176634650754));
#168578=CARTESIAN_POINT('Ctrl Pts',(31.6030360625191,-54.4206516984414,
40.123528185308));
#168579=CARTESIAN_POINT('Ctrl Pts',(31.5956573884055,-54.4288041214182,
40.1288820140928));
#168580=CARTESIAN_POINT('Ctrl Pts',(31.5878037911381,-54.4368146919236,
40.1336621774101));
#168581=CARTESIAN_POINT('Ctrl Pts',(31.5843907239925,-54.4402959775153,
40.1357395717319));
#168582=CARTESIAN_POINT('Ctrl Pts',(31.58088799234,-54.4437502703989,40.1377083672883));
#168583=CARTESIAN_POINT('Ctrl Pts',(31.5772987574368,-54.4471718528272,
40.1395632548791));
#168584=CARTESIAN_POINT('Ctrl Pts',(31.5647364352753,-54.4591473913263,
40.1460553614469));
#168585=CARTESIAN_POINT('Ctrl Pts',(31.5511144466741,-54.4707222239581,
40.151152097463));
#168586=CARTESIAN_POINT('Ctrl Pts',(31.5365683393825,-54.4816512176785,
40.1546258197409));
#168587=CARTESIAN_POINT('Ctrl Pts',(31.5292952857367,-54.4871157145387,
40.1563626808798));
#168588=CARTESIAN_POINT('Ctrl Pts',(31.5217912027244,-54.4924187521963,
40.1576937882008));
#168589=CARTESIAN_POINT('Ctrl Pts',(31.5140730377804,-54.4975296958773,
40.1585906813668));
#168590=CARTESIAN_POINT('Ctrl Pts',(31.5102139553083,-54.5000851677177,
40.1590391279498));
#168591=CARTESIAN_POINT('Ctrl Pts',(31.5063013524149,-54.5025926161708,
40.1593790209175));
#168592=CARTESIAN_POINT('Ctrl Pts',(31.5023373478779,-54.5050482124961,
40.1596068022931));
#168593=CARTESIAN_POINT('Ctrl Pts',(31.4983733433408,-54.5075038088215,
40.1598345836687));
#168594=CARTESIAN_POINT('Ctrl Pts',(31.4943579363066,-54.5099075515417,
40.1599502506865));
#168595=CARTESIAN_POINT('Ctrl Pts',(31.4902932482907,-54.5122556166611,
40.1599502534424));
#168596=CARTESIAN_POINT('',(31.4638515574739,-54.527521733972,40.1599502534424));
#168597=CARTESIAN_POINT('Origin',(5.57749365020894E-15,5.82947588787858E-15,
40.1599502534424));
#168598=CARTESIAN_POINT('',(31.1067982185534,-54.5146464769138,39.8576902534424));
#168599=CARTESIAN_POINT('Ctrl Pts',(31.4638515574739,-54.527521733972,40.1599502534424));
#168600=CARTESIAN_POINT('Ctrl Pts',(31.4605414731919,-54.5294317356858,
40.1599502447858));
#168601=CARTESIAN_POINT('Ctrl Pts',(31.457216601512,-54.5312951627228,40.1598744685927));
#168602=CARTESIAN_POINT('Ctrl Pts',(31.4538791743432,-54.533112022376,40.1597246934279));
#168603=CARTESIAN_POINT('Ctrl Pts',(31.434592962471,-54.5436112298318,40.1588591777434));
#168604=CARTESIAN_POINT('Ctrl Pts',(31.4148859438252,-54.5525583311782,
40.1555254706017));
#168605=CARTESIAN_POINT('Ctrl Pts',(31.3951944477259,-54.5599504658514,
40.1500631826373));
#168606=CARTESIAN_POINT('Ctrl Pts',(31.3872524143686,-54.5629318838127,
40.1478601162475));
#168607=CARTESIAN_POINT('Ctrl Pts',(31.3793127123318,-54.5656607810288,
40.1453112228303));
#168608=CARTESIAN_POINT('Ctrl Pts',(31.3714030065917,-54.5681385507008,
40.1424401896328));
#168609=CARTESIAN_POINT('Ctrl Pts',(31.3684848053917,-54.5690526972782,
40.1413809526905));
#168610=CARTESIAN_POINT('Ctrl Pts',(31.3655707565305,-54.569932546879,40.1402777640511));
#168611=CARTESIAN_POINT('Ctrl Pts',(31.3626622846451,-54.5707781137755,
40.1391317641987));
#168612=CARTESIAN_POINT('Ctrl Pts',(31.3572088998598,-54.5723635517063,
40.1369830144753));
#168613=CARTESIAN_POINT('Ctrl Pts',(31.3517751216268,-54.5738284644992,
40.1346837565849));
#168614=CARTESIAN_POINT('Ctrl Pts',(31.3463703409154,-54.5751729463229,
40.1322415082996));
#168615=CARTESIAN_POINT('Ctrl Pts',(31.3274536084258,-54.579878632706,40.1236936393008));
#168616=CARTESIAN_POINT('Ctrl Pts',(31.30889209334,-54.5831090358348,40.113394140767));
#168617=CARTESIAN_POINT('Ctrl Pts',(31.2910884461624,-54.5848682151123,
40.101665321223));
#168618=CARTESIAN_POINT('Ctrl Pts',(31.2821866225735,-54.5857478047511,
40.095800911451));
#168619=CARTESIAN_POINT('Ctrl Pts',(31.273474266467,-54.5862595893019,40.0895791707949));
#168620=CARTESIAN_POINT('Ctrl Pts',(31.2650017135576,-54.5864040839108,
40.0830403822906));
#168621=CARTESIAN_POINT('Ctrl Pts',(31.2607654371028,-54.5864763312152,
40.0797709880385));
#168622=CARTESIAN_POINT('Ctrl Pts',(31.2565891115051,-54.5864567561364,
40.0764223317514));
#168623=CARTESIAN_POINT('Ctrl Pts',(31.2524790289902,-54.5863454235313,
40.0729994484778));
#168624=CARTESIAN_POINT('Ctrl Pts',(31.2483689464753,-54.5862340909261,
40.0695765652042));
#168625=CARTESIAN_POINT('Ctrl Pts',(31.244325185122,-54.5860308973889,40.0660793733488));
#168626=CARTESIAN_POINT('Ctrl Pts',(31.2403538784534,-54.5857361203748,
40.0625130768817));
#168627=CARTESIAN_POINT('Ctrl Pts',(31.2403200115247,-54.5857336065442,
40.0624826638418));
#168628=CARTESIAN_POINT('Ctrl Pts',(31.2402861499645,-54.5857310861512,
40.0624522459912));
#168629=CARTESIAN_POINT('Ctrl Pts',(31.240252293776,-54.5857285591961,40.0624218233329));
#168630=CARTESIAN_POINT('Ctrl Pts',(31.2229614439864,-54.584438006344,40.0468845275906));
#168631=CARTESIAN_POINT('Ctrl Pts',(31.2070266227617,-54.5815601021618,
40.0302263329253));
#168632=CARTESIAN_POINT('Ctrl Pts',(31.1924939094138,-54.5772898993843,
40.0127515884768));
#168633=CARTESIAN_POINT('Ctrl Pts',(31.1774697093504,-54.5728752811845,
39.9946858597746));
#168634=CARTESIAN_POINT('Ctrl Pts',(31.1639433968922,-54.5669719917386,
39.9757460620528));
#168635=CARTESIAN_POINT('Ctrl Pts',(31.1520017942489,-54.5597576364823,
39.9562444559174));
#168636=CARTESIAN_POINT('Ctrl Pts',(31.1402873460154,-54.5526805134434,
39.9371138113662));
#168637=CARTESIAN_POINT('Ctrl Pts',(31.1300975277295,-54.544340874098,39.9174410654408));
#168638=CARTESIAN_POINT('Ctrl Pts',(31.1215554575431,-54.5348819367227,
39.8975196504205));
#168639=CARTESIAN_POINT('Ctrl Pts',(31.1158966355154,-54.5286157223262,
39.8843224113815));
#168640=CARTESIAN_POINT('Ctrl Pts',(31.1109617866619,-54.5218578148494,
39.8710160447152));
#168641=CARTESIAN_POINT('Ctrl Pts',(31.1067982185534,-54.5146464769138,
39.8576902534424));
#168642=CARTESIAN_POINT('',(30.9286463962977,-54.2060847114742,39.2875012672119));
#168643=CARTESIAN_POINT('',(31.1067982185534,-54.5146464769138,39.8576902534424));
#168644=CARTESIAN_POINT('',(25.6742415049979,-56.8833377255395,39.2875012672119));
#168645=CARTESIAN_POINT('Origin',(5.53234440788222E-15,0.,39.2875012672119));
#168646=CARTESIAN_POINT('',(25.8191582032619,-57.2088336324699,39.8576902534424));
#168647=CARTESIAN_POINT('',(25.6742415049979,-56.8833377255395,39.2875012672119));
#168648=CARTESIAN_POINT('',(25.6197038181297,-57.5052637377732,40.1599502534424));
#168649=CARTESIAN_POINT('Ctrl Pts',(25.8191582032619,-57.2088336324699,
39.8576902534424));
#168650=CARTESIAN_POINT('Ctrl Pts',(25.8241633573212,-57.2200757170683,
39.8773836120359));
#168651=CARTESIAN_POINT('Ctrl Pts',(25.8273704465175,-57.2320741602337,
39.8969946442123));
#168652=CARTESIAN_POINT('Ctrl Pts',(25.8287819086041,-57.2446400511071,
39.9162525288227));
#168653=CARTESIAN_POINT('Ctrl Pts',(25.8302217324661,-57.2574584397114,
39.9358973794043));
#168654=CARTESIAN_POINT('Ctrl Pts',(25.8297934599654,-57.2708681396374,
39.9551762199714));
#168655=CARTESIAN_POINT('Ctrl Pts',(25.8274551293905,-57.2846981803199,
39.9738152034211));
#168656=CARTESIAN_POINT('Ctrl Pts',(25.8252076408387,-57.297990936459,39.9917300792603));
#168657=CARTESIAN_POINT('Ctrl Pts',(25.8211956083131,-57.3116728904459,
40.0090551158071));
#168658=CARTESIAN_POINT('Ctrl Pts',(25.8153387643616,-57.325606333425,40.0255394551476));
#168659=CARTESIAN_POINT('Ctrl Pts',(25.8108397400745,-57.3363095208216,
40.0382021526112));
#168660=CARTESIAN_POINT('Ctrl Pts',(25.8052513267436,-57.3471614741636,
40.0503687782105));
#168661=CARTESIAN_POINT('Ctrl Pts',(25.798518653724,-57.3581011436975,40.0619155352442));
#168662=CARTESIAN_POINT('Ctrl Pts',(25.7985010085887,-57.3581298146203,
40.0619457972351));
#168663=CARTESIAN_POINT('Ctrl Pts',(25.798483354779,-57.3581584863394,40.0619760547305));
#168664=CARTESIAN_POINT('Ctrl Pts',(25.7984656922965,-57.3581871588519,
40.0620063077269));
#168665=CARTESIAN_POINT('Ctrl Pts',(25.7965719149862,-57.3612614352674,
40.06525004417));
#168666=CARTESIAN_POINT('Ctrl Pts',(25.7945784837697,-57.3643429325988,
40.0684393223556));
#168667=CARTESIAN_POINT('Ctrl Pts',(25.7924880141965,-57.3674274658676,
40.0715697951759));
#168668=CARTESIAN_POINT('Ctrl Pts',(25.7808550263334,-57.384592192176,40.0889901646422));
#168669=CARTESIAN_POINT('Ctrl Pts',(25.7662212180069,-57.4018536888734,
40.1045963098245));
#168670=CARTESIAN_POINT('Ctrl Pts',(25.7490920431255,-57.4184830023427,
40.1176634650729));
#168671=CARTESIAN_POINT('Ctrl Pts',(25.7414042322284,-57.4259464685158,
40.1235281853064));
#168672=CARTESIAN_POINT('Ctrl Pts',(25.7332138190169,-57.4332829502016,
40.1288820140921));
#168673=CARTESIAN_POINT('Ctrl Pts',(25.724565911951,-57.4404287135112,40.1336621774101));
#168674=CARTESIAN_POINT('Ctrl Pts',(25.7208076485112,-57.4435341655924,
40.1357395717319));
#168675=CARTESIAN_POINT('Ctrl Pts',(25.7169630332624,-57.4466034003412,
40.1377083672884));
#168676=CARTESIAN_POINT('Ctrl Pts',(25.7130358078103,-57.4496310617743,
40.1395632548792));
#168677=CARTESIAN_POINT('Ctrl Pts',(25.699290518728,-57.4602278767899,40.146055361447));
#168678=CARTESIAN_POINT('Ctrl Pts',(25.6845332533381,-57.4703154157423,
40.1511520974629));
#168679=CARTESIAN_POINT('Ctrl Pts',(25.6689244402255,-57.4796640570498,
40.1546258197408));
#168680=CARTESIAN_POINT('Ctrl Pts',(25.6611200336693,-57.4843383777036,
40.1563626808798));
#168681=CARTESIAN_POINT('Ctrl Pts',(25.6531027404319,-57.4888279745006,
40.1576937882008));
#168682=CARTESIAN_POINT('Ctrl Pts',(25.6448926173141,-57.4931041519764,
40.1585906813668));
#168683=CARTESIAN_POINT('Ctrl Pts',(25.6407875557553,-57.4952422407143,
40.1590391279498));
#168684=CARTESIAN_POINT('Ctrl Pts',(25.6366342867764,-57.4973269747345,
40.1593790209175));
#168685=CARTESIAN_POINT('Ctrl Pts',(25.6324353177606,-57.4993547677436,
40.1596068022931));
#168686=CARTESIAN_POINT('Ctrl Pts',(25.6282363487449,-57.5013825607528,
40.1598345836687));
#168687=CARTESIAN_POINT('Ctrl Pts',(25.6239916789979,-57.5033534111922,
40.1599502506864));
#168688=CARTESIAN_POINT('Ctrl Pts',(25.6197038181297,-57.5052637377733,
40.1599502534424));
#168689=CARTESIAN_POINT('',(25.5918112338793,-57.5176823163889,40.1599502534424));
#168690=CARTESIAN_POINT('Origin',(5.59198795571863E-15,5.83686110540852E-15,
40.1599502534424));
#168691=CARTESIAN_POINT('',(25.2380597013429,-57.4675553545141,39.8576902534424));
#168692=CARTESIAN_POINT('Ctrl Pts',(25.5918112338793,-57.5176823163889,
40.1599502534424));
#168693=CARTESIAN_POINT('Ctrl Pts',(25.5883196330413,-57.5192358568901,
40.1599502447858));
#168694=CARTESIAN_POINT('Ctrl Pts',(25.5848181941918,-57.5207415321516,
40.1598744685927));
#168695=CARTESIAN_POINT('Ctrl Pts',(25.5813091362507,-57.5221995827243,
40.1597246934279));
#168696=CARTESIAN_POINT('Ctrl Pts',(25.5610311102425,-57.5306253163346,
40.1588591777434));
#168697=CARTESIAN_POINT('Ctrl Pts',(25.5404968219507,-57.5374634601495,
40.1555254706012));
#168698=CARTESIAN_POINT('Ctrl Pts',(25.5201405094481,-57.5427567781089,
40.1500631826359));
#168699=CARTESIAN_POINT('Ctrl Pts',(25.5119303403444,-57.5448916950081,
40.1478601162464));
#168700=CARTESIAN_POINT('Ctrl Pts',(25.5037488853954,-57.5467757181865,
40.1453112228297));
#168701=CARTESIAN_POINT('Ctrl Pts',(25.4956235123965,-57.5484131249908,
40.1424401896328));
#168702=CARTESIAN_POINT('Ctrl Pts',(25.492625743071,-57.5490172286906,40.1413809526905));
#168703=CARTESIAN_POINT('Ctrl Pts',(25.4896356883477,-57.5495876573339,
40.1402777640511));
#168704=CARTESIAN_POINT('Ctrl Pts',(25.4866547635673,-57.5501245740298,
40.1391317641987));
#168705=CARTESIAN_POINT('Ctrl Pts',(25.481065529604,-57.5511312928345,40.1369830144753));
#168706=CARTESIAN_POINT('Ctrl Pts',(25.4755083930936,-57.5520201961934,
40.1346837565849));
#168707=CARTESIAN_POINT('Ctrl Pts',(25.4699926837176,-57.552792359383,40.1322415082996));
#168708=CARTESIAN_POINT('Ctrl Pts',(25.4506877009016,-57.5554949305466,
40.1236936393008));
#168709=CARTESIAN_POINT('Ctrl Pts',(25.4318901986628,-57.5567674305411,
40.113394140767));
#168710=CARTESIAN_POINT('Ctrl Pts',(25.4140001974206,-57.5566559849705,
40.101665321223));
#168711=CARTESIAN_POINT('Ctrl Pts',(25.4050551967996,-57.5566002621852,
40.095800911451));
#168712=CARTESIAN_POINT('Ctrl Pts',(25.3963370718388,-57.5561985539314,
40.0895791707949));
#168713=CARTESIAN_POINT('Ctrl Pts',(25.3878958286612,-57.5554566340481,
40.0830403822906));
#168714=CARTESIAN_POINT('Ctrl Pts',(25.3836752070724,-57.5550856741065,
40.0797709880385));
#168715=CARTESIAN_POINT('Ctrl Pts',(25.3795238059763,-57.5546296613652,
40.0764223317514));
#168716=CARTESIAN_POINT('Ctrl Pts',(25.3754478763495,-57.5540893180425,
40.0729994484778));
#168717=CARTESIAN_POINT('Ctrl Pts',(25.3713719467228,-57.5535489747198,
40.0695765652042));
#168718=CARTESIAN_POINT('Ctrl Pts',(25.3673715770255,-57.552924206138,40.0660793733488));
#168719=CARTESIAN_POINT('Ctrl Pts',(25.3634528381786,-57.55221592936,40.0625130768817));
#168720=CARTESIAN_POINT('Ctrl Pts',(25.3634194195433,-57.5522098892424,
40.0624826638418));
#168721=CARTESIAN_POINT('Ctrl Pts',(25.3633860069332,-57.5522038431595,
40.0624522459912));
#168722=CARTESIAN_POINT('Ctrl Pts',(25.3633526003511,-57.552197791112,40.0624218233329));
#168723=CARTESIAN_POINT('Ctrl Pts',(25.3462913711534,-57.5491069220866,
40.0468845275917));
#168724=CARTESIAN_POINT('Ctrl Pts',(25.3307446654493,-57.54457914099,40.0302263329276));
#168725=CARTESIAN_POINT('Ctrl Pts',(25.3167379215606,-57.5388132486373,
40.0127515884805));
#168726=CARTESIAN_POINT('Ctrl Pts',(25.3022574788943,-57.532852357634,39.9946858597797));
#168727=CARTESIAN_POINT('Ctrl Pts',(25.2894223267656,-57.5255675223713,
39.9757460620594));
#168728=CARTESIAN_POINT('Ctrl Pts',(25.2783002469397,-57.5171444507355,
39.9562444559255));
#168729=CARTESIAN_POINT('Ctrl Pts',(25.2673897324753,-57.5088816036461,
39.9371138113757));
#168730=CARTESIAN_POINT('Ctrl Pts',(25.2581274647651,-57.4995225236723,
39.9174410654518));
#168731=CARTESIAN_POINT('Ctrl Pts',(25.2506209171206,-57.4892225138769,
39.8975196504329));
#168732=CARTESIAN_POINT('Ctrl Pts',(25.2456480924715,-57.4823991184863,
39.8843224113898));
#168733=CARTESIAN_POINT('Ctrl Pts',(25.2414466709183,-57.4751623993644,
39.8710160447193));
#168734=CARTESIAN_POINT('Ctrl Pts',(25.2380597013429,-57.4675553545141,
39.8576902534424));
#168735=CARTESIAN_POINT('',(25.0931373005745,-57.1420619865022,39.2875012672119));
#168736=CARTESIAN_POINT('',(25.2380597013429,-57.4675553545141,39.8576902534424));
#168737=CARTESIAN_POINT('',(19.5876674457077,-59.2554138597572,39.2875012672119));
#168738=CARTESIAN_POINT('Origin',(5.53234440788222E-15,0.,39.2875012672119));
#168739=CARTESIAN_POINT('',(19.6977666881844,-59.5942745858236,39.8576902534424));
#168740=CARTESIAN_POINT('',(19.5876674457077,-59.2554138597572,39.2875012672119));
#168741=CARTESIAN_POINT('',(19.4684195516695,-59.8682321556242,40.1599502534424));
#168742=CARTESIAN_POINT('Ctrl Pts',(19.6977666881844,-59.5942745858236,
39.8576902534424));
#168743=CARTESIAN_POINT('Ctrl Pts',(19.7015693056589,-59.6059782661672,
39.8773836120338));
#168744=CARTESIAN_POINT('Ctrl Pts',(19.7035046472594,-59.6182462127093,
39.8969946442081));
#168745=CARTESIAN_POINT('Ctrl Pts',(19.7035948839469,-59.6308908042792,
39.9162525288166));
#168746=CARTESIAN_POINT('Ctrl Pts',(19.7036869338411,-59.6437894749839,
39.9358973793963));
#168747=CARTESIAN_POINT('Ctrl Pts',(19.7018593121365,-59.6570809485028,
39.9551762199616));
#168748=CARTESIAN_POINT('Ctrl Pts',(19.6980881582828,-59.6705908046724,
39.9738152034098));
#168749=CARTESIAN_POINT('Ctrl Pts',(19.6944635103376,-59.683575815177,39.9917300792478));
#168750=CARTESIAN_POINT('Ctrl Pts',(19.6890433025225,-59.6967634463928,
40.0090551157937));
#168751=CARTESIAN_POINT('Ctrl Pts',(19.6817621015939,-59.7100083536145,
40.0255394551334));
#168752=CARTESIAN_POINT('Ctrl Pts',(19.6761689357006,-59.7201826317395,
40.0382021526021));
#168753=CARTESIAN_POINT('Ctrl Pts',(19.6694767982743,-59.7303909886918,
40.0503687782062));
#168754=CARTESIAN_POINT('Ctrl Pts',(19.661637500694,-59.7405669736108,40.0619155352442));
#168755=CARTESIAN_POINT('Ctrl Pts',(19.6616169552931,-59.7405936430524,
40.0619457972351));
#168756=CARTESIAN_POINT('Ctrl Pts',(19.6615964011821,-59.7406203123793,
40.0619760547305));
#168757=CARTESIAN_POINT('Ctrl Pts',(19.6615758383628,-59.7406469815886,
40.0620063077269));
#168758=CARTESIAN_POINT('Ctrl Pts',(19.6593710859735,-59.7435064631642,
40.06525004417));
#168759=CARTESIAN_POINT('Ctrl Pts',(19.6570664708011,-59.7463627094291,
40.0684393223557));
#168760=CARTESIAN_POINT('Ctrl Pts',(19.6546650315164,-59.74921183173,40.0715697951759));
#168761=CARTESIAN_POINT('Ctrl Pts',(19.6413015679154,-59.7650665495262,
40.0889901646412));
#168762=CARTESIAN_POINT('Ctrl Pts',(19.6249436073997,-59.7807038364415,
40.1045963098227));
#168763=CARTESIAN_POINT('Ctrl Pts',(19.6061700313499,-59.7954515664635,
40.1176634650705));
#168764=CARTESIAN_POINT('Ctrl Pts',(19.5977441904346,-59.80207055193,40.123528185305));
#168765=CARTESIAN_POINT('Ctrl Pts',(19.5888317740061,-59.8085107122958,
40.1288820140915));
#168766=CARTESIAN_POINT('Ctrl Pts',(19.5794843054211,-59.814713377931,40.1336621774101));
#168767=CARTESIAN_POINT('Ctrl Pts',(19.5754220220079,-59.8174089725188,
40.1357395717319));
#168768=CARTESIAN_POINT('Ctrl Pts',(19.571277645572,-59.8200595219548,40.1377083672883));
#168769=CARTESIAN_POINT('Ctrl Pts',(19.5670554570749,-59.8226600907003,
40.1395632548791));
#168770=CARTESIAN_POINT('Ctrl Pts',(19.5522777973353,-59.8317620813095,
40.1460553614469));
#168771=CARTESIAN_POINT('Ctrl Pts',(19.5365469388443,-59.8402518053948,
40.1511520974629));
#168772=CARTESIAN_POINT('Ctrl Pts',(19.5200464333337,-59.847917668619,40.1546258197408));
#168773=CARTESIAN_POINT('Ctrl Pts',(19.5117961805784,-59.8517506002311,
40.1563626808798));
#168774=CARTESIAN_POINT('Ctrl Pts',(19.5033535162583,-59.8553775672055,
40.1576937882008));
#168775=CARTESIAN_POINT('Ctrl Pts',(19.4947413867939,-59.858772127781,40.1585906813668));
#168776=CARTESIAN_POINT('Ctrl Pts',(19.4904353220616,-59.8604694080687,
40.1590391279498));
#168777=CARTESIAN_POINT('Ctrl Pts',(19.4860868910813,-59.8621085868739,
40.1593790209175));
#168778=CARTESIAN_POINT('Ctrl Pts',(19.4816989623701,-59.8636863596422,
40.1596068022931));
#168779=CARTESIAN_POINT('Ctrl Pts',(19.4773110336589,-59.8652641324105,
40.1598345836687));
#168780=CARTESIAN_POINT('Ctrl Pts',(19.4728836066891,-59.8667804975193,
40.1599502506865));
#168781=CARTESIAN_POINT('Ctrl Pts',(19.4684195516695,-59.8682321556242,
40.1599502534424));
#168782=CARTESIAN_POINT('',(19.4393816709755,-59.8776671349986,40.1599502534424));
#168783=CARTESIAN_POINT('Origin',(5.60717482534548E-15,5.84269079846304E-15,
40.1599502534424));
#168784=CARTESIAN_POINT('',(19.092807720641,-59.7908376697912,39.8576902534424));
#168785=CARTESIAN_POINT('Ctrl Pts',(19.4393816709755,-59.8776671349986,
40.1599502534424));
#168786=CARTESIAN_POINT('Ctrl Pts',(19.435746808291,-59.8788471933725,40.1599502447858));
#168787=CARTESIAN_POINT('Ctrl Pts',(19.4321071647686,-59.8799786203651,
40.1598744685927));
#168788=CARTESIAN_POINT('Ctrl Pts',(19.4284649220283,-59.8810618871501,
40.1597246934279));
#168789=CARTESIAN_POINT('Ctrl Pts',(19.4074172521856,-59.8873218328123,
40.1588591777435));
#168790=CARTESIAN_POINT('Ctrl Pts',(19.3862806722126,-59.89197609896,40.1555254706023));
#168791=CARTESIAN_POINT('Ctrl Pts',(19.3654825713311,-59.8951126055061,
40.1500631826386));
#168792=CARTESIAN_POINT('Ctrl Pts',(19.3570942188067,-59.8963776307482,
40.1478601162485));
#168793=CARTESIAN_POINT('Ctrl Pts',(19.3487606486729,-59.897396138138,40.1453112228309));
#168794=CARTESIAN_POINT('Ctrl Pts',(19.3405086316971,-59.8981752423037,
40.1424401896328));
#168795=CARTESIAN_POINT('Ctrl Pts',(19.3374641384343,-59.8984626844394,
40.1413809526906));
#168796=CARTESIAN_POINT('Ctrl Pts',(19.3344308375141,-59.8987174423897,
40.1402777640511));
#168797=CARTESIAN_POINT('Ctrl Pts',(19.3314101194744,-59.8989398263133,
40.1391317641987));
#168798=CARTESIAN_POINT('Ctrl Pts',(19.3257462731499,-59.89935679617,40.1369830144753));
#168799=CARTESIAN_POINT('Ctrl Pts',(19.3201266635127,-59.8996599510837,
40.1346837565849));
#168800=CARTESIAN_POINT('Ctrl Pts',(19.3145604567382,-59.8998513356576,
40.1322415082996));
#168801=CARTESIAN_POINT('Ctrl Pts',(19.2950787330274,-59.9005211816664,
40.1236936393008));
#168802=CARTESIAN_POINT('Ctrl Pts',(19.2762511930037,-59.8998218367506,
40.113394140767));
#168803=CARTESIAN_POINT('Ctrl Pts',(19.2584708442944,-59.8978409873527,
40.101665321223));
#168804=CARTESIAN_POINT('Ctrl Pts',(19.2495806699398,-59.8968505626538,
40.095800911451));
#168805=CARTESIAN_POINT('Ctrl Pts',(19.2409522937263,-59.8955397627951,
40.0895791707949));
#168806=CARTESIAN_POINT('Ctrl Pts',(19.2326348443073,-59.8939195570492,
40.0830403822906));
#168807=CARTESIAN_POINT('Ctrl Pts',(19.2284761195978,-59.8931094541763,
40.0797709880385));
#168808=CARTESIAN_POINT('Ctrl Pts',(19.2243951266223,-59.8922219999435,
40.0764223317514));
#168809=CARTESIAN_POINT('Ctrl Pts',(19.2203980066217,-59.8912585660178,
40.0729994484778));
#168810=CARTESIAN_POINT('Ctrl Pts',(19.2164008866211,-59.8902951320921,
40.0695765652042));
#168811=CARTESIAN_POINT('Ctrl Pts',(19.2124877374673,-59.889255633561,40.0660793733488));
#168812=CARTESIAN_POINT('Ctrl Pts',(19.208664500965,-59.8881416170476,40.0625130768817));
#168813=CARTESIAN_POINT('Ctrl Pts',(19.2086318967648,-59.8881321168199,
40.0624826638418));
#168814=CARTESIAN_POINT('Ctrl Pts',(19.2085992991801,-59.8881226112892,
40.0624522459912));
#168815=CARTESIAN_POINT('Ctrl Pts',(19.208566708214,-59.8881131004568,40.0624218233329));
#168816=CARTESIAN_POINT('Ctrl Pts',(19.1919220260051,-59.883255779466,40.0468845275922));
#168817=CARTESIAN_POINT('Ctrl Pts',(19.176933768782,-59.8771277287721,40.0302263329289));
#168818=CARTESIAN_POINT('Ctrl Pts',(19.1636064551692,-59.8699293191674,
40.0127515884825));
#168819=CARTESIAN_POINT('Ctrl Pts',(19.1498284206597,-59.8624874641298,
39.9946858597826));
#168820=CARTESIAN_POINT('Ctrl Pts',(19.1378250534729,-59.8539008972296,
39.9757460620633));
#168821=CARTESIAN_POINT('Ctrl Pts',(19.1276443522982,-59.8443613941496,
39.9562444559305));
#168822=CARTESIAN_POINT('Ctrl Pts',(19.1176573094822,-59.8350033524913,
39.9371138113817));
#168823=CARTESIAN_POINT('Ctrl Pts',(19.109424071691,-59.8247273719274,39.9174410654588));
#168824=CARTESIAN_POINT('Ctrl Pts',(19.1030352898953,-59.8136991387744,
39.8975196504409));
#168825=CARTESIAN_POINT('Ctrl Pts',(19.0988029459332,-59.8063933209376,
39.8843224113952));
#168826=CARTESIAN_POINT('Ctrl Pts',(19.0953809833349,-59.7987570771804,
39.871016044722));
#168827=CARTESIAN_POINT('Ctrl Pts',(19.092807720641,-59.7908376697912,39.8576902534424));
#168828=CARTESIAN_POINT('',(18.9827025415095,-59.4519788726608,39.2875012672119));
#168829=CARTESIAN_POINT('',(19.092807720641,-59.7908376697912,39.8576902534424));
#168830=CARTESIAN_POINT('',(13.2864868028994,-60.9782752797348,39.2875012672119));
#168831=CARTESIAN_POINT('Origin',(5.53234440788222E-15,0.,39.2875012672119));
#168832=CARTESIAN_POINT('',(13.3605623192485,-61.3267881959113,39.8576902534424));
#168833=CARTESIAN_POINT('',(13.2864868028994,-60.9782752797348,39.2875012672119));
#168834=CARTESIAN_POINT('',(13.1038352065726,-61.5752716937452,40.1599502534424));
#168835=CARTESIAN_POINT('Ctrl Pts',(13.3605623192485,-61.3267881959113,
39.8576902534424));
#168836=CARTESIAN_POINT('Ctrl Pts',(13.3631207378657,-61.338825244031,39.8773836120348));
#168837=CARTESIAN_POINT('Ctrl Pts',(13.3637631278628,-61.3512282837623,
39.8969946442099));
#168838=CARTESIAN_POINT('Ctrl Pts',(13.3625311504986,-61.3638130392394,
39.9162525288192));
#168839=CARTESIAN_POINT('Ctrl Pts',(13.3612744179067,-61.3766506715109,
39.9358973793998));
#168840=CARTESIAN_POINT('Ctrl Pts',(13.3580674708032,-61.3896782944596,
39.9551762199659));
#168841=CARTESIAN_POINT('Ctrl Pts',(13.3529048112199,-61.402719949307,39.9738152034148));
#168842=CARTESIAN_POINT('Ctrl Pts',(13.3479427162813,-61.4152549476863,
39.9917300792534));
#168843=CARTESIAN_POINT('Ctrl Pts',(13.341173718106,-61.4278037696855,40.0090551157998));
#168844=CARTESIAN_POINT('Ctrl Pts',(13.3325479345591,-61.4402150271762,
40.0255394551399));
#168845=CARTESIAN_POINT('Ctrl Pts',(13.3259219069573,-61.4497489245038,
40.0382021526063));
#168846=CARTESIAN_POINT('Ctrl Pts',(13.3181993658965,-61.4592018401658,
40.0503687782082));
#168847=CARTESIAN_POINT('Ctrl Pts',(13.3093393327442,-61.4685026502439,
40.0619155352442));
#168848=CARTESIAN_POINT('Ctrl Pts',(13.3093161121774,-61.4685270260084,
40.0619457972351));
#168849=CARTESIAN_POINT('Ctrl Pts',(13.3092928829602,-61.4685514007482,
40.0619760547305));
#168850=CARTESIAN_POINT('Ctrl Pts',(13.3092696450948,-61.4685757744609,
40.0620063077269));
#168851=CARTESIAN_POINT('Ctrl Pts',(13.3067780733549,-61.4711891321181,
40.06525004417));
#168852=CARTESIAN_POINT('Ctrl Pts',(13.3041875240728,-61.4737888336847,
40.0684393223557));
#168853=CARTESIAN_POINT('Ctrl Pts',(13.301501425748,-61.4763713294375,40.0715697951759));
#168854=CARTESIAN_POINT('Ctrl Pts',(13.2865538993123,-61.4907423311162,
40.0889901646409));
#168855=CARTESIAN_POINT('Ctrl Pts',(13.2686510078454,-61.5045840828626,
40.1045963098221));
#168856=CARTESIAN_POINT('Ctrl Pts',(13.248438717854,-61.5172886502217,40.1176634650698));
#168857=CARTESIAN_POINT('Ctrl Pts',(13.2393671621973,-61.5229906359909,
40.1235281853046));
#168858=CARTESIAN_POINT('Ctrl Pts',(13.2298303888519,-61.5284639152914,
40.1288820140913));
#168859=CARTESIAN_POINT('Ctrl Pts',(13.2198857715704,-61.5336555255488,
40.1336621774101));
#168860=CARTESIAN_POINT('Ctrl Pts',(13.2155639754109,-61.5359117291449,
40.1357395717319));
#168861=CARTESIAN_POINT('Ctrl Pts',(13.2111652444434,-61.5381145532937,
40.1377083672884));
#168862=CARTESIAN_POINT('Ctrl Pts',(13.2066943520821,-61.5402595369763,
40.1395632548792));
#168863=CARTESIAN_POINT('Ctrl Pts',(13.1910462288177,-61.5477669798653,
40.146055361447));
#168864=CARTESIAN_POINT('Ctrl Pts',(13.1745141278033,-61.5545658738898,
40.1511520974629));
#168865=CARTESIAN_POINT('Ctrl Pts',(13.1573027128859,-61.560464970229,40.1546258197408));
#168866=CARTESIAN_POINT('Ctrl Pts',(13.1486970054272,-61.5634145183986,
40.1563626808798));
#168867=CARTESIAN_POINT('Ctrl Pts',(13.1399214696215,-61.5661391177411,
40.1576937882008));
#168868=CARTESIAN_POINT('Ctrl Pts',(13.1310016901029,-61.5686148699002,
40.1585906813668));
#168869=CARTESIAN_POINT('Ctrl Pts',(13.1265418003436,-61.5698527459797,
40.1590391279498));
#168870=CARTESIAN_POINT('Ctrl Pts',(13.1220458496817,-61.5710284103839,
40.1593790209175));
#168871=CARTESIAN_POINT('Ctrl Pts',(13.1175170363402,-61.5721388765028,
40.1596068022931));
#168872=CARTESIAN_POINT('Ctrl Pts',(13.1129882229987,-61.5732493426217,
40.1598345836687));
#168873=CARTESIAN_POINT('Ctrl Pts',(13.1084265466226,-61.5742946087864,
40.1599502506865));
#168874=CARTESIAN_POINT('Ctrl Pts',(13.1038352065726,-61.5752716937452,
40.1599502534424));
#168875=CARTESIAN_POINT('',(13.0739701745323,-61.5816197022698,40.1599502534424));
#168876=CARTESIAN_POINT('Origin',(5.62288786856779E-15,5.84690109570509E-15,
40.1599502534424));
#168877=CARTESIAN_POINT('',(12.7383709431249,-61.4590390555209,39.8576902534424));
#168878=CARTESIAN_POINT('Ctrl Pts',(13.0739701745323,-61.5816197022698,
40.1599502534424));
#168879=CARTESIAN_POINT('Ctrl Pts',(13.0702318743176,-61.5824133495499,
40.1599502447858));
#168880=CARTESIAN_POINT('Ctrl Pts',(13.0664939028184,-61.5831581321228,
40.1598744685927));
#168881=CARTESIAN_POINT('Ctrl Pts',(13.0627583804525,-61.5838547466226,
40.1597246934279));
#168882=CARTESIAN_POINT('Ctrl Pts',(13.0411716694466,-61.5878803190635,
40.1588591777435));
#168883=CARTESIAN_POINT('Ctrl Pts',(13.0196643745814,-61.590299714431,40.155525470602));
#168884=CARTESIAN_POINT('Ctrl Pts',(12.9986523536628,-61.5912450453419,
40.1500631826381));
#168885=CARTESIAN_POINT('Ctrl Pts',(12.9901777222673,-61.5916263190447,
40.1478601162481));
#168886=CARTESIAN_POINT('Ctrl Pts',(12.9817833412911,-61.5917681516647,
40.1453112228307));
#168887=CARTESIAN_POINT('Ctrl Pts',(12.9734950911672,-61.5916804171629,
40.1424401896328));
#168888=CARTESIAN_POINT('Ctrl Pts',(12.9704372300723,-61.5916480484584,
40.1413809526905));
#168889=CARTESIAN_POINT('Ctrl Pts',(12.9673939164349,-61.5915843445341,
40.1402777640511));
#168890=CARTESIAN_POINT('Ctrl Pts',(12.9643665007549,-61.5914897592007,
40.1391317641987));
#168891=CARTESIAN_POINT('Ctrl Pts',(12.9586900963549,-61.5913124117004,
40.1369830144753));
#168892=CARTESIAN_POINT('Ctrl Pts',(12.95306958321,-61.5910264967402,40.1346837565849));
#168893=CARTESIAN_POINT('Ctrl Pts',(12.9475138635631,-61.5906350058491,
40.1322415082996));
#168894=CARTESIAN_POINT('Ctrl Pts',(12.9280688447993,-61.58926478773,40.1236936393008));
#168895=CARTESIAN_POINT('Ctrl Pts',(12.9094175454591,-61.586601260073,40.113394140767));
#168896=CARTESIAN_POINT('Ctrl Pts',(12.8919416545041,-61.5827727094485,
40.101665321223));
#168897=CARTESIAN_POINT('Ctrl Pts',(12.8832037090265,-61.5808584341363,
40.095800911451));
#168898=CARTESIAN_POINT('Ctrl Pts',(12.8747596158555,-61.5786529040703,
40.0895791707949));
#168899=CARTESIAN_POINT('Ctrl Pts',(12.8666570879116,-61.5761721637749,
40.0830403822906));
#168900=CARTESIAN_POINT('Ctrl Pts',(12.8626058239396,-61.5749317936272,
40.0797709880385));
#168901=CARTESIAN_POINT('Ctrl Pts',(12.8586399512977,-61.5736226210372,
40.0764223317514));
#168902=CARTESIAN_POINT('Ctrl Pts',(12.8547654342064,-61.5722466520922,
40.0729994484778));
#168903=CARTESIAN_POINT('Ctrl Pts',(12.8508909171151,-61.5708706831472,
40.0695765652042));
#168904=CARTESIAN_POINT('Ctrl Pts',(12.8471078617859,-61.5694278436302,
40.0660793733488));
#168905=CARTESIAN_POINT('Ctrl Pts',(12.8434220158074,-61.5679202927796,
40.0625130768817));
#168906=CARTESIAN_POINT('Ctrl Pts',(12.8433905832605,-61.5679074365281,
40.0624826638418));
#168907=CARTESIAN_POINT('Ctrl Pts',(12.8433591578474,-61.5678945756943,
40.0624522459912));
#168908=CARTESIAN_POINT('Ctrl Pts',(12.8433277395707,-61.5678817102796,
40.0624218233329));
#168909=CARTESIAN_POINT('Ctrl Pts',(12.8272819669698,-61.561311155148,40.0468845275908));
#168910=CARTESIAN_POINT('Ctrl Pts',(12.8130163727087,-61.5536499750616,
40.0302263329259));
#168911=CARTESIAN_POINT('Ctrl Pts',(12.8005145062075,-61.5450979154855,
40.0127515884777));
#168912=CARTESIAN_POINT('Ctrl Pts',(12.7875898348827,-61.5362566309333,
39.9946858597759));
#168913=CARTESIAN_POINT('Ctrl Pts',(12.7765497640396,-61.5264624086177,
39.9757460620546));
#168914=CARTESIAN_POINT('Ctrl Pts',(12.7674219834083,-61.5159109908837,
39.9562444559197));
#168915=CARTESIAN_POINT('Ctrl Pts',(12.7584678323715,-61.5055602833174,
39.9371138113689));
#168916=CARTESIAN_POINT('Ctrl Pts',(12.7513538295754,-61.4944799879548,
39.9174410654441));
#168917=CARTESIAN_POINT('Ctrl Pts',(12.7461528104596,-61.4828443590724,
39.8975196504242));
#168918=CARTESIAN_POINT('Ctrl Pts',(12.742707317634,-61.4751361628628,39.884322411384));
#168919=CARTESIAN_POINT('Ctrl Pts',(12.7401023057314,-61.4671840587593,
39.8710160447164));
#168920=CARTESIAN_POINT('Ctrl Pts',(12.7383709431249,-61.4590390555209,
39.8576902534424));
#168921=CARTESIAN_POINT('',(12.664289321014,-61.1105274371641,39.2875012672119));
#168922=CARTESIAN_POINT('',(12.7383709431249,-61.4590390555209,39.8576902534424));
#168923=CARTESIAN_POINT('',(6.8397366303024,-62.0330459552233,39.2875012672119));
#168924=CARTESIAN_POINT('Origin',(5.53234440788222E-15,0.,39.2875012672119));
#168925=CARTESIAN_POINT('',(6.87697683366544,-62.3873926810691,39.8576902534424));
#168926=CARTESIAN_POINT('',(6.8397366303024,-62.0330459552233,39.2875012672119));
#168927=CARTESIAN_POINT('',(6.59568250079865,-62.6076796697354,40.1599502534424));
#168928=CARTESIAN_POINT('Ctrl Pts',(6.87697683366544,-62.3873926810691,
39.8576902534424));
#168929=CARTESIAN_POINT('Ctrl Pts',(6.87826302285563,-62.3996312165467,
39.8773836120355));
#168930=CARTESIAN_POINT('Ctrl Pts',(6.87760542309009,-62.4120334591682,
39.8969946442113));
#168931=CARTESIAN_POINT('Ctrl Pts',(6.87506472947593,-62.4244204973379,
39.9162525288213));
#168932=CARTESIAN_POINT('Ctrl Pts',(6.87247298342313,-62.4370564393905,
39.9358973794026));
#168933=CARTESIAN_POINT('Ctrl Pts',(6.86792184690411,-62.4496774784054,
39.9551762199694));
#168934=CARTESIAN_POINT('Ctrl Pts',(6.86142424476998,-62.4621080448309,
39.9738152034189));
#168935=CARTESIAN_POINT('Ctrl Pts',(6.85517906858854,-62.4740556950194,
39.991730079258));
#168936=CARTESIAN_POINT('Ctrl Pts',(6.84713544261344,-62.4858282202819,
40.0090551158049));
#168937=CARTESIAN_POINT('Ctrl Pts',(6.83725958233785,-62.4972698477072,
40.0255394551454));
#168938=CARTESIAN_POINT('Ctrl Pts',(6.82967328917275,-62.5060589088635,
40.0382021526098));
#168939=CARTESIAN_POINT('Ctrl Pts',(6.82100495425341,-62.5146528151136,
40.0503687782099));
#168940=CARTESIAN_POINT('Ctrl Pts',(6.8112212579066,-62.5229765487297,40.0619155352442));
#168941=CARTESIAN_POINT('Ctrl Pts',(6.8111956165833,-62.5229983637511,40.0619457972351));
#168942=CARTESIAN_POINT('Ctrl Pts',(6.8111699667641,-62.5230201768492,40.0619760547305));
#168943=CARTESIAN_POINT('Ctrl Pts',(6.81114430845137,-62.5230419880217,
40.0620063077269));
#168944=CARTESIAN_POINT('Ctrl Pts',(6.80839321554227,-62.5253805892671,
40.06525004417));
#168945=CARTESIAN_POINT('Ctrl Pts',(6.80554511475049,-62.5276952632611,
40.0684393223556));
#168946=CARTESIAN_POINT('Ctrl Pts',(6.80260378684096,-62.5299828381018,
40.0715697951759));
#168947=CARTESIAN_POINT('Ctrl Pts',(6.78623596579486,-62.5427126719642,
40.0889901646441));
#168948=CARTESIAN_POINT('Ctrl Pts',(6.7669842911974,-62.5546072354152,40.104596309828));
#168949=CARTESIAN_POINT('Ctrl Pts',(6.74555473733804,-62.5651294462146,
40.1176634650772));
#168950=CARTESIAN_POINT('Ctrl Pts',(6.7359368568061,-62.5698519601346,40.1235281853091));
#168951=CARTESIAN_POINT('Ctrl Pts',(6.72588021343273,-62.5742983919741,
40.1288820140933));
#168952=CARTESIAN_POINT('Ctrl Pts',(6.71544740276754,-62.5784220664834,
40.1336621774101));
#168953=CARTESIAN_POINT('Ctrl Pts',(6.7109134443649,-62.580214159649,40.1357395717319));
#168954=CARTESIAN_POINT('Ctrl Pts',(6.70630855228273,-62.5819451239082,
40.1377083672883));
#168955=CARTESIAN_POINT('Ctrl Pts',(6.70163794008953,-62.5836110216378,
40.1395632548791));
#168956=CARTESIAN_POINT('Ctrl Pts',(6.68529079741335,-62.5894416636913,
40.146055361447));
#168957=CARTESIAN_POINT('Ctrl Pts',(6.66813858303382,-62.5944752375494,
40.1511520974629));
#168958=CARTESIAN_POINT('Ctrl Pts',(6.65040483057317,-62.5985429352696,
40.1546258197408));
#168959=CARTESIAN_POINT('Ctrl Pts',(6.64153795434284,-62.6005767841297,
40.1563626808798));
#168960=CARTESIAN_POINT('Ctrl Pts',(6.63252569365821,-62.6023691645599,
40.1576937882008));
#168961=CARTESIAN_POINT('Ctrl Pts',(6.62339599105649,-62.6038989834438,
40.1585906813668));
#168962=CARTESIAN_POINT('Ctrl Pts',(6.61883113975563,-62.6046638928858,
40.1590391279498));
#168963=CARTESIAN_POINT('Ctrl Pts',(6.61423692798836,-62.6053631620637,
40.1593790209175));
#168964=CARTESIAN_POINT('Ctrl Pts',(6.60961684864331,-62.605994155034,40.1596068022931));
#168965=CARTESIAN_POINT('Ctrl Pts',(6.60499676929825,-62.6066251480043,
40.1598345836687));
#168966=CARTESIAN_POINT('Ctrl Pts',(6.6003508221967,-62.60718786307,40.1599502506864));
#168967=CARTESIAN_POINT('Ctrl Pts',(6.59568250079866,-62.6076796697354,
40.1599502534424));
#168968=CARTESIAN_POINT('',(6.56531752495282,-62.6108711573006,40.1599502534424));
#168969=CARTESIAN_POINT('Origin',(5.63895492999586E-15,5.84944586823703E-15,
40.1599502534424));
#168970=CARTESIAN_POINT('',(6.24436990788039,-62.4538823482276,39.8576902534424));
#168971=CARTESIAN_POINT('Ctrl Pts',(6.56531752495282,-62.6108711573006,
40.1599502534424));
#168972=CARTESIAN_POINT('Ctrl Pts',(6.56151674480723,-62.611269698121,40.1599502447857));
#168973=CARTESIAN_POINT('Ctrl Pts',(6.55772139932922,-62.6116196762807,
40.1598744685927));
#168974=CARTESIAN_POINT('Ctrl Pts',(6.55393352450261,-62.6119220062409,
40.1597246934279));
#168975=CARTESIAN_POINT('Ctrl Pts',(6.53204428085673,-62.6136691004464,
40.1588591777435));
#168976=CARTESIAN_POINT('Ctrl Pts',(6.51040190952292,-62.6138271176315,
40.1555254706019));
#168977=CARTESIAN_POINT('Ctrl Pts',(6.48940618066564,-62.612570915664,40.1500631826377));
#168978=CARTESIAN_POINT('Ctrl Pts',(6.48093812023387,-62.612064260513,40.1478601162478));
#168979=CARTESIAN_POINT('Ctrl Pts',(6.4725748990096,-62.6113278644156,40.1453112228305));
#168980=CARTESIAN_POINT('Ctrl Pts',(6.46434122354013,-62.610374252484,40.1424401896328));
#168981=CARTESIAN_POINT('Ctrl Pts',(6.46130349717921,-62.6100224275775,
40.1413809526906));
#168982=CARTESIAN_POINT('Ctrl Pts',(6.45828351400566,-62.6096409597322,
40.1402777640512));
#168983=CARTESIAN_POINT('Ctrl Pts',(6.45528256968506,-62.6092304414384,
40.1391317641987));
#168984=CARTESIAN_POINT('Ctrl Pts',(6.44965579908394,-62.6084607196375,
40.1369830144753));
#168985=CARTESIAN_POINT('Ctrl Pts',(6.44409596194954,-62.6075888673476,
40.1346837565849));
#168986=CARTESIAN_POINT('Ctrl Pts',(6.43861159905749,-62.6066187902474,
40.1322415082996));
#168987=CARTESIAN_POINT('Ctrl Pts',(6.41941632893531,-62.6032235203971,
40.1236936393009));
#168988=CARTESIAN_POINT('Ctrl Pts',(6.40114561781732,-62.5986249921653,
40.113394140767));
#168989=CARTESIAN_POINT('Ctrl Pts',(6.38416565413474,-62.5929906867159,
40.101665321223));
#168990=CARTESIAN_POINT('Ctrl Pts',(6.37567567229345,-62.5901735339912,
40.095800911451));
#168991=CARTESIAN_POINT('Ctrl Pts',(6.36750837741685,-62.5870974379668,
40.0895791707949));
#168992=CARTESIAN_POINT('Ctrl Pts',(6.35970954393957,-62.5837833426318,
40.0830403822906));
#168993=CARTESIAN_POINT('Ctrl Pts',(6.35581012720093,-62.5821262949642,
40.0797709880385));
#168994=CARTESIAN_POINT('Ctrl Pts',(6.35200282582339,-62.5804097475859,
40.0764223317514));
#168995=CARTESIAN_POINT('Ctrl Pts',(6.34829336166144,-62.5786363190253,
40.0729994484778));
#168996=CARTESIAN_POINT('Ctrl Pts',(6.34458389749948,-62.5768628904647,
40.0695765652042));
#168997=CARTESIAN_POINT('Ctrl Pts',(6.3409723839406,-62.5750325180135,40.0660793733488));
#168998=CARTESIAN_POINT('Ctrl Pts',(6.33746431138575,-62.5731479498682,
40.0625130768817));
#168999=CARTESIAN_POINT('Ctrl Pts',(6.3374343948739,-62.5731318784488,40.0624826638418));
#169000=CARTESIAN_POINT('Ctrl Pts',(6.33740448593562,-62.5731158032179,
40.0624522459912));
#169001=CARTESIAN_POINT('Ctrl Pts',(6.33737458457357,-62.5730997241771,
40.0624218233329));
#169002=CARTESIAN_POINT('Ctrl Pts',(6.32210352242537,-62.5648879232825,
40.0468845275917));
#169003=CARTESIAN_POINT('Ctrl Pts',(6.30871688796422,-62.5557775512971,
40.0302263329276));
#169004=CARTESIAN_POINT('Ctrl Pts',(6.29717744164146,-62.5459655399053,
40.0127515884805));
#169005=CARTESIAN_POINT('Ctrl Pts',(6.28524773890653,-62.5358216928038,
39.9946858597798));
#169006=CARTESIAN_POINT('Ctrl Pts',(6.27529192173438,-62.524927122624,39.9757460620596));
#169007=CARTESIAN_POINT('Ctrl Pts',(6.26731706752152,-62.5134793937786,
39.9562444559258));
#169008=CARTESIAN_POINT('Ctrl Pts',(6.25949391181652,-62.5022494248242,
39.9371138113761));
#169009=CARTESIAN_POINT('Ctrl Pts',(6.25357708651871,-62.4904862126997,
39.9174410654523));
#169010=CARTESIAN_POINT('Ctrl Pts',(6.24962081353557,-62.4783706704748,
39.8975196504334));
#169011=CARTESIAN_POINT('Ctrl Pts',(6.2469999213836,-62.4703445484985,39.8843224113901));
#169012=CARTESIAN_POINT('Ctrl Pts',(6.24524040122982,-62.4621637089605,
39.8710160447195));
#169013=CARTESIAN_POINT('Ctrl Pts',(6.2443699078804,-62.4538823482276,39.8576902534424));
#169014=CARTESIAN_POINT('',(6.20712349654444,-62.0995362748659,39.2875012672119));
#169015=CARTESIAN_POINT('',(6.24436990788039,-62.4538823482276,39.8576902534424));
#169016=CARTESIAN_POINT('',(0.318048871876918,-62.4081695979768,39.2875012672119));
#169017=CARTESIAN_POINT('Origin',(5.53234440788222E-15,0.,39.2875012672119));
#169018=CARTESIAN_POINT('',(0.318045750792831,-62.7644678366119,39.8576902534424));
#169019=CARTESIAN_POINT('',(0.318048871876917,-62.4081695979768,39.2875012672119));
#169020=CARTESIAN_POINT('',(0.0152661173106527,-62.9541448057648,40.1599502534424));
#169021=CARTESIAN_POINT('Ctrl Pts',(0.318045750792832,-62.7644678366119,
39.8576902534424));
#169022=CARTESIAN_POINT('Ctrl Pts',(0.318045618797918,-62.77677377149,39.8773836120337));
#169023=CARTESIAN_POINT('Ctrl Pts',(0.316095234070707,-62.7890393354348,
39.8969946442078));
#169024=CARTESIAN_POINT('Ctrl Pts',(0.312273660578351,-62.8010929413131,
39.9162525288161));
#169025=CARTESIAN_POINT('Ctrl Pts',(0.3083752967776,-62.8133887511198,39.9358973793957));
#169026=CARTESIAN_POINT('Ctrl Pts',(0.302529834048607,-62.825464927455,
39.9551762199608));
#169027=CARTESIAN_POINT('Ctrl Pts',(0.294768478454255,-62.83714821357,39.9738152034088));
#169028=CARTESIAN_POINT('Ctrl Pts',(0.287308644488887,-62.8483776146106,
39.9917300792465));
#169029=CARTESIAN_POINT('Ctrl Pts',(0.278078518365733,-62.8592448608849,
40.009055115792));
#169030=CARTESIAN_POINT('Ctrl Pts',(0.267060783356072,-62.8695915013792,
40.0255394551315));
#169031=CARTESIAN_POINT('Ctrl Pts',(0.258597341640148,-62.8775394315757,
40.0382021526009));
#169032=CARTESIAN_POINT('Ctrl Pts',(0.249078184949622,-62.8851801717828,
40.0503687782056));
#169033=CARTESIAN_POINT('Ctrl Pts',(0.238478017627655,-62.8924356323738,
40.0619155352442));
#169034=CARTESIAN_POINT('Ctrl Pts',(0.238450236479546,-62.892454647642,
40.0619457972351));
#169035=CARTESIAN_POINT('Ctrl Pts',(0.238422447083121,-62.8924736601095,
40.0619760547305));
#169036=CARTESIAN_POINT('Ctrl Pts',(0.238394649440958,-62.8924926697742,
40.0620063077269));
#169037=CARTESIAN_POINT('Ctrl Pts',(0.235414176912292,-62.8945308924032,
40.06525004417));
#169038=CARTESIAN_POINT('Ctrl Pts',(0.232339728999104,-62.8965351787718,
40.0684393223556));
#169039=CARTESIAN_POINT('Ctrl Pts',(0.229175397308911,-62.8985027695519,
40.0715697951759));
#169040=CARTESIAN_POINT('Ctrl Pts',(0.211566610930123,-62.9094519648699,
40.0889901646418));
#169041=CARTESIAN_POINT('Ctrl Pts',(0.191177078584712,-62.9192690206957,
40.1045963098239));
#169042=CARTESIAN_POINT('Ctrl Pts',(0.168765047542055,-62.9274935913893,
40.1176634650721));
#169043=CARTESIAN_POINT('Ctrl Pts',(0.158706217640471,-62.9311848926133,
40.123528185306));
#169044=CARTESIAN_POINT('Ctrl Pts',(0.148239886921569,-62.9345557609575,
40.1288820140919));
#169045=CARTESIAN_POINT('Ctrl Pts',(0.137433186922152,-62.9375663198809,
40.1336621774101));
#169046=CARTESIAN_POINT('Ctrl Pts',(0.132736741273405,-62.9388746680683,
40.1357395717319));
#169047=CARTESIAN_POINT('Ctrl Pts',(0.127976140237891,-62.9401148076313,
40.1377083672884));
#169048=CARTESIAN_POINT('Ctrl Pts',(0.123156980417351,-62.9412833674838,
40.1395632548792));
#169049=CARTESIAN_POINT('Ctrl Pts',(0.10628992104546,-62.9453733269673,
40.146055361447));
#169050=CARTESIAN_POINT('Ctrl Pts',(0.0887055165508424,-62.9485864317704,
40.151152097463));
#169051=CARTESIAN_POINT('Ctrl Pts',(0.0706437212499514,-62.9507781643242,
40.1546258197409));
#169052=CARTESIAN_POINT('Ctrl Pts',(0.061612823599506,-62.9518740306011,
40.1563626808798));
#169053=CARTESIAN_POINT('Ctrl Pts',(0.052462578249927,-62.9527145544237,
40.1576937882008));
#169054=CARTESIAN_POINT('Ctrl Pts',(0.0432229794973055,-62.9532816790167,
40.1585906813668));
#169055=CARTESIAN_POINT('Ctrl Pts',(0.0386031801209948,-62.9535652413132,
40.1590391279498));
#169056=CARTESIAN_POINT('Ctrl Pts',(0.0339610423938992,-62.9537804539255,
40.1593790209175));
#169057=CARTESIAN_POINT('Ctrl Pts',(0.0293003156013867,-62.9539250604562,
40.1596068022931));
#169058=CARTESIAN_POINT('Ctrl Pts',(0.024639588808874,-62.9540696669868,
40.1598345836687));
#169059=CARTESIAN_POINT('Ctrl Pts',(0.0199602729505794,-62.9541436657296,
40.1599502506865));
#169060=CARTESIAN_POINT('Ctrl Pts',(0.0152661173106527,-62.9541448057648,
40.1599502534424));
#169061=CARTESIAN_POINT('',(-0.015266117311081,-62.9541448057648,40.1599502534424));
#169062=CARTESIAN_POINT('Origin',(-3.96846087890508E-17,1.55412650666996E-16,
40.1599502534424));
#169063=CARTESIAN_POINT('',(-0.318045750793257,-62.7644678366119,39.8576902534424));
#169064=CARTESIAN_POINT('Ctrl Pts',(-0.015266117311081,-62.9541448057648,
40.1599502534424));
#169065=CARTESIAN_POINT('Ctrl Pts',(-0.0190877352448612,-62.9541438736292,
40.1599502447858));
#169066=CARTESIAN_POINT('Ctrl Pts',(-0.022898872102436,-62.9540952129414,
40.1598744685927));
#169067=CARTESIAN_POINT('Ctrl Pts',(-0.0266975986405572,-62.9539999459718,
40.1597246934279));
#169068=CARTESIAN_POINT('Ctrl Pts',(-0.0486495517941837,-62.953449420412,
40.1588591777434));
#169069=CARTESIAN_POINT('Ctrl Pts',(-0.070189881249066,-62.9513443281451,
40.1555254706012));
#169070=CARTESIAN_POINT('Ctrl Pts',(-0.0909392844476108,-62.9479003565101,
40.150063182636));
#169071=CARTESIAN_POINT('Ctrl Pts',(-0.0993079960717487,-62.9465113235254,
40.1478601162465));
#169072=CARTESIAN_POINT('Ctrl Pts',(-0.107548428340522,-62.9449047668208,
40.1453112228298));
#169073=CARTESIAN_POINT('Ctrl Pts',(-0.115637319282431,-62.9430957254317,
40.1424401896328));
#169074=CARTESIAN_POINT('Ctrl Pts',(-0.118621628943688,-62.9424282989905,
40.1413809526905));
#169075=CARTESIAN_POINT('Ctrl Pts',(-0.121585194085774,-62.9417332466658,
40.1402777640512));
#169076=CARTESIAN_POINT('Ctrl Pts',(-0.124526788072995,-62.941011293136,
40.1391317641987));
#169077=CARTESIAN_POINT('Ctrl Pts',(-0.130042276799036,-62.9396576302675,
40.1369830144753));
#169078=CARTESIAN_POINT('Ctrl Pts',(-0.135480523183809,-62.938209392844,
40.134683756585));
#169079=CARTESIAN_POINT('Ctrl Pts',(-0.140833441493576,-62.9366713579026,
40.1322415082996));
#169080=CARTESIAN_POINT('Ctrl Pts',(-0.159568655577758,-62.9312882356078,
40.1236936393009));
#169081=CARTESIAN_POINT('Ctrl Pts',(-0.177258600739179,-62.9248050892389,
40.113394140767));
#169082=CARTESIAN_POINT('Ctrl Pts',(-0.193556601113859,-62.9174267595942,
40.101665321223));
#169083=CARTESIAN_POINT('Ctrl Pts',(-0.201705601301199,-62.9137375947718,
40.095800911451));
#169084=CARTESIAN_POINT('Ctrl Pts',(-0.209506615291615,-62.9098246351408,
40.0895791707949));
#169085=CARTESIAN_POINT('Ctrl Pts',(-0.216916308650606,-62.9057134946881,
40.0830403822906));
#169086=CARTESIAN_POINT('Ctrl Pts',(-0.220621155330102,-62.9036579244618,
40.0797709880385));
#169087=CARTESIAN_POINT('Ctrl Pts',(-0.224228171852759,-62.9015528091474,
40.0764223317514));
#169088=CARTESIAN_POINT('Ctrl Pts',(-0.227731941419747,-62.8994013510256,
40.0729994484778));
#169089=CARTESIAN_POINT('Ctrl Pts',(-0.231235710986736,-62.8972498929038,
40.0695765652042));
#169090=CARTESIAN_POINT('Ctrl Pts',(-0.23463611427696,-62.8950520414621,
40.0660793733488));
#169091=CARTESIAN_POINT('Ctrl Pts',(-0.237927978231146,-62.892811103745,
40.0625130768817));
#169092=CARTESIAN_POINT('Ctrl Pts',(-0.237956050936441,-62.8927919932396,
40.0624826638418));
#169093=CARTESIAN_POINT('Ctrl Pts',(-0.237984115711232,-62.8927728797351,
40.0624522459912));
#169094=CARTESIAN_POINT('Ctrl Pts',(-0.238012172553065,-62.8927537632335,
40.0624218233329));
#169095=CARTESIAN_POINT('Ctrl Pts',(-0.252341211296384,-62.8829906867849,
40.0468845275921));
#169096=CARTESIAN_POINT('Ctrl Pts',(-0.264702219189541,-62.8725309380422,
40.0302263329286));
#169097=CARTESIAN_POINT('Ctrl Pts',(-0.275152816745417,-62.8615664772848,
40.012751588482));
#169098=CARTESIAN_POINT('Ctrl Pts',(-0.285956846571237,-62.8502312057453,
39.9946858597818));
#169099=CARTESIAN_POINT('Ctrl Pts',(-0.294719332056317,-62.8383556508916,
39.9757460620621));
#169100=CARTESIAN_POINT('Ctrl Pts',(-0.301453885679313,-62.8261370346473,
39.9562444559289));
#169101=CARTESIAN_POINT('Ctrl Pts',(-0.308060333921541,-62.8141508421944,
39.9371138113796));
#169102=CARTESIAN_POINT('Ctrl Pts',(-0.312715155744977,-62.8018335935212,
39.9174410654562));
#169103=CARTESIAN_POINT('Ctrl Pts',(-0.315383336840583,-62.7893708783693,
39.8975196504379));
#169104=CARTESIAN_POINT('Ctrl Pts',(-0.317150913275331,-62.7811147664991,
39.8843224113931));
#169105=CARTESIAN_POINT('Ctrl Pts',(-0.318045664008668,-62.7727948225173,
39.871016044721));
#169106=CARTESIAN_POINT('Ctrl Pts',(-0.318045750793257,-62.7644678366119,
39.8576902534424));
#169107=CARTESIAN_POINT('',(-0.318048871877343,-62.4081695979768,39.2875012672119));
#169108=CARTESIAN_POINT('',(-0.318045750793259,-62.7644678366119,39.8576902534424));
#169109=CARTESIAN_POINT('',(-6.20712349654485,-62.0995362748658,39.2875012672119));
#169110=CARTESIAN_POINT('Origin',(5.53234440788222E-15,0.,39.2875012672119));
#169111=CARTESIAN_POINT('',(-6.24436990788081,-62.4538823482275,39.8576902534424));
#169112=CARTESIAN_POINT('',(-6.20712349654485,-62.0995362748658,39.2875012672119));
#169113=CARTESIAN_POINT('',(-6.56531752495323,-62.6108711573005,40.1599502534424));
#169114=CARTESIAN_POINT('Ctrl Pts',(-6.2443699078808,-62.4538823482275,
39.8576902534424));
#169115=CARTESIAN_POINT('Ctrl Pts',(-6.24565635961484,-62.4661208561118,
39.8773836120374));
#169116=CARTESIAN_POINT('Ctrl Pts',(-6.24887816048168,-62.4781153572978,
39.8969946442152));
#169117=CARTESIAN_POINT('Ctrl Pts',(-6.25393874389551,-62.4897034690595,
39.916252528827));
#169118=CARTESIAN_POINT('Ctrl Pts',(-6.25910101415687,-62.5015244311583,
39.9358973794102));
#169119=CARTESIAN_POINT('Ctrl Pts',(-6.26617675898623,-62.5129234357018,
39.9551762199786));
#169120=CARTESIAN_POINT('Ctrl Pts',(-6.27511683300914,-62.5237314369814,
39.9738152034297));
#169121=CARTESIAN_POINT('Ctrl Pts',(-6.28370959326059,-62.534119557209,
39.9917300792702));
#169122=CARTESIAN_POINT('Ctrl Pts',(-6.2940250923436,-62.543962460673,40.0090551158182));
#169123=CARTESIAN_POINT('Ctrl Pts',(-6.30606398948311,-62.5531007542797,
40.0255394551598));
#169124=CARTESIAN_POINT('Ctrl Pts',(-6.315311852504,-62.5601204743206,40.038202152619));
#169125=CARTESIAN_POINT('Ctrl Pts',(-6.32557753708339,-62.5667243349277,
40.0503687782142));
#169126=CARTESIAN_POINT('Ctrl Pts',(-6.33687803771711,-62.5728320301412,
40.0619155352442));
#169127=CARTESIAN_POINT('Ctrl Pts',(-6.33690765431396,-62.5728480373211,
40.0619457972351));
#169128=CARTESIAN_POINT('Ctrl Pts',(-6.33693727882117,-62.5728640408534,
40.0619760547304));
#169129=CARTESIAN_POINT('Ctrl Pts',(-6.33696691123597,-62.5728800407363,
40.0620063077269));
#169130=CARTESIAN_POINT('Ctrl Pts',(-6.34014410870348,-62.5745955535553,
40.06525004417));
#169131=CARTESIAN_POINT('Ctrl Pts',(-6.34341121944339,-62.5762674929177,
40.0684393223556));
#169132=CARTESIAN_POINT('Ctrl Pts',(-6.34676388583407,-62.5778935423007,
40.0715697951758));
#169133=CARTESIAN_POINT('Ctrl Pts',(-6.36542071199911,-62.586942137401,
40.0889901646417));
#169134=CARTESIAN_POINT('Ctrl Pts',(-6.38672471011203,-62.5945741278849,
40.1045963098237));
#169135=CARTESIAN_POINT('Ctrl Pts',(-6.40987366743906,-62.6004109483561,
40.1176634650718));
#169136=CARTESIAN_POINT('Ctrl Pts',(-6.42026324006253,-62.6030305942139,
40.1235281853058));
#169137=CARTESIAN_POINT('Ctrl Pts',(-6.43102458681472,-62.6052889671226,
40.1288820140918));
#169138=CARTESIAN_POINT('Ctrl Pts',(-6.44208677567884,-62.6071534261453,
40.1336621774101));
#169139=CARTESIAN_POINT('Ctrl Pts',(-6.44689425333237,-62.6079636948179,
40.1357395717319));
#169140=CARTESIAN_POINT('Ctrl Pts',(-6.45175840518007,-62.6086994224562,
40.1377083672884));
#169141=CARTESIAN_POINT('Ctrl Pts',(-6.45667331290448,-62.6093578414452,
40.1395632548792));
#169142=CARTESIAN_POINT('Ctrl Pts',(-6.47387548993995,-62.6116623079068,
40.146055361447));
#169143=CARTESIAN_POINT('Ctrl Pts',(-6.49169942613425,-62.6130197402063,
40.1511520974629));
#169144=CARTESIAN_POINT('Ctrl Pts',(-6.50989137546639,-62.6133114945132,
40.1546258197408));
#169145=CARTESIAN_POINT('Ctrl Pts',(-6.51898735013247,-62.6134573716666,
40.1563626808798));
#169146=CARTESIAN_POINT('Ctrl Pts',(-6.52817532814414,-62.6133368299269,
40.1576937882008));
#169147=CARTESIAN_POINT('Ctrl Pts',(-6.53742359207022,-62.6129350466932,
40.1585906813668));
#169148=CARTESIAN_POINT('Ctrl Pts',(-6.54204772403327,-62.6127341550763,
40.1590391279498));
#169149=CARTESIAN_POINT('Ctrl Pts',(-6.54668692748782,-62.6124629532086,
40.1593790209175));
#169150=CARTESIAN_POINT('Ctrl Pts',(-6.55133723782973,-62.6121195889602,
40.1596068022931));
#169151=CARTESIAN_POINT('Ctrl Pts',(-6.55598754817164,-62.6117762247118,
40.1598345836687));
#169152=CARTESIAN_POINT('Ctrl Pts',(-6.56064896522293,-62.6113606963859,
40.1599502506865));
#169153=CARTESIAN_POINT('Ctrl Pts',(-6.56531752495323,-62.6108711573005,
40.1599502534424));
#169154=CARTESIAN_POINT('',(-6.59568250079906,-62.6076796697354,40.1599502534424));
#169155=CARTESIAN_POINT('Origin',(-2.34395632424774E-17,1.54561283905546E-16,
40.1599502534424));
#169156=CARTESIAN_POINT('',(-6.87697683366585,-62.3873926810691,39.8576902534424));
#169157=CARTESIAN_POINT('Ctrl Pts',(-6.59568250079906,-62.6076796697354,
40.1599502534424));
#169158=CARTESIAN_POINT('Ctrl Pts',(-6.59948308607524,-62.6072792748563,
40.1599502447858));
#169159=CARTESIAN_POINT('Ctrl Pts',(-6.60326825869943,-62.6068325084578,
40.1598744685927));
#169160=CARTESIAN_POINT('Ctrl Pts',(-6.60703621730617,-62.6063406883232,
40.1597246934279));
#169161=CARTESIAN_POINT('Ctrl Pts',(-6.62881036976783,-62.6034985746718,
40.1588591777436));
#169162=CARTESIAN_POINT('Ctrl Pts',(-6.65001265697977,-62.5991534367857,
40.1555254706027));
#169163=CARTESIAN_POINT('Ctrl Pts',(-6.6702883997098,-62.5935594283595,
40.1500631826398));
#169164=CARTESIAN_POINT('Ctrl Pts',(-6.67846607317752,-62.5913032360762,
40.1478601162494));
#169165=CARTESIAN_POINT('Ctrl Pts',(-6.68649343259726,-62.5888441205342,
40.1453112228314));
#169166=CARTESIAN_POINT('Ctrl Pts',(-6.69434891543631,-62.586199469922,
40.1424401896328));
#169167=CARTESIAN_POINT('Ctrl Pts',(-6.69724711167674,-62.5852237544099,
40.1413809526905));
#169168=CARTESIAN_POINT('Ctrl Pts',(-6.7001217893475,-62.5842227327444,
40.1402777640511));
#169169=CARTESIAN_POINT('Ctrl Pts',(-6.70297180428205,-62.5831972538525,
40.1391317641987));
#169170=CARTESIAN_POINT('Ctrl Pts',(-6.70831558228433,-62.5812744809302,
40.1369830144753));
#169171=CARTESIAN_POINT('Ctrl Pts',(-6.71357265535406,-62.5792657255653,
40.1346837565849));
#169172=CARTESIAN_POINT('Ctrl Pts',(-6.71873548138837,-62.5771765838154,
40.1322415082996));
#169173=CARTESIAN_POINT('Ctrl Pts',(-6.73680537250844,-62.5698645876906,
40.1236936393008));
#169174=CARTESIAN_POINT('Ctrl Pts',(-6.75372073697224,-62.5615678538928,
40.113394140767));
#169175=CARTESIAN_POINT('Ctrl Pts',(-6.76915820973634,-62.5525263385764,
40.101665321223));
#169176=CARTESIAN_POINT('Ctrl Pts',(-6.77687694611839,-62.5480055809182,
40.095800911451));
#169177=CARTESIAN_POINT('Ctrl Pts',(-6.78422620968087,-62.5432986288851,
40.0895791707949));
#169178=CARTESIAN_POINT('Ctrl Pts',(-6.79116558077055,-62.5384354858298,
40.0830403822906));
#169179=CARTESIAN_POINT('Ctrl Pts',(-6.79463526631539,-62.5360039143022,
40.0797709880385));
#169180=CARTESIAN_POINT('Ctrl Pts',(-6.79800247875532,-62.5335332951358,
40.0764223317514));
#169181=CARTESIAN_POINT('Ctrl Pts',(-6.80126216569475,-62.5310273792782,
40.0729994484778));
#169182=CARTESIAN_POINT('Ctrl Pts',(-6.80452185263419,-62.5285214634206,
40.0695765652042));
#169183=CARTESIAN_POINT('Ctrl Pts',(-6.80767389012569,-62.5259802131086,
40.0660793733488));
#169184=CARTESIAN_POINT('Ctrl Pts',(-6.81071347912887,-62.5234074580024,
40.0625130768816));
#169185=CARTESIAN_POINT('Ctrl Pts',(-6.81073940045717,-62.5233855177896,
40.0624826638418));
#169186=CARTESIAN_POINT('Ctrl Pts',(-6.81076531358494,-62.5233635754231,
40.0624522459912));
#169187=CARTESIAN_POINT('Ctrl Pts',(-6.81079121850992,-62.5233416309051,
40.0624218233329));
#169188=CARTESIAN_POINT('Ctrl Pts',(-6.82402124190344,-62.5121342452095,
40.0468845275902));
#169189=CARTESIAN_POINT('Ctrl Pts',(-6.83522119344092,-62.5004397189038,
40.0302263329245));
#169190=CARTESIAN_POINT('Ctrl Pts',(-6.84446844329707,-62.4884429377054,
40.0127515884755));
#169191=CARTESIAN_POINT('Ctrl Pts',(-6.85402842900294,-62.476040433333,
39.994685859773));
#169192=CARTESIAN_POINT('Ctrl Pts',(-6.86150157917654,-62.4633140048676,
39.9757460620508));
#169193=CARTESIAN_POINT('Ctrl Pts',(-6.86692204703053,-62.450458370939,
39.9562444559149));
#169194=CARTESIAN_POINT('Ctrl Pts',(-6.8722394061801,-62.4378472782187,
39.9371138113634));
#169195=CARTESIAN_POINT('Ctrl Pts',(-6.87558122532622,-62.4251109433491,
39.9174410654378));
#169196=CARTESIAN_POINT('Ctrl Pts',(-6.87693208138238,-62.4124375993839,
39.8975196504171));
#169197=CARTESIAN_POINT('Ctrl Pts',(-6.87782697616072,-62.4040419533144,
39.8843224113792));
#169198=CARTESIAN_POINT('Ctrl Pts',(-6.87784715439656,-62.3956740599416,
39.871016044714));
#169199=CARTESIAN_POINT('Ctrl Pts',(-6.87697683366585,-62.3873926810691,
39.8576902534424));
#169200=CARTESIAN_POINT('',(-6.83973663030281,-62.0330459552232,39.2875012672119));
#169201=CARTESIAN_POINT('',(-6.87697683366585,-62.3873926810691,39.8576902534424));
#169202=CARTESIAN_POINT('',(-12.6642893210144,-61.1105274371641,39.2875012672119));
#169203=CARTESIAN_POINT('Origin',(5.53234440788222E-15,0.,39.2875012672119));
#169204=CARTESIAN_POINT('',(-12.7383709431253,-61.4590390555208,39.8576902534424));
#169205=CARTESIAN_POINT('',(-12.6642893210144,-61.1105274371641,39.2875012672119));
#169206=CARTESIAN_POINT('',(-13.0739701745327,-61.5816197022697,40.1599502534424));
#169207=CARTESIAN_POINT('Ctrl Pts',(-12.7383709431253,-61.4590390555208,
39.8576902534424));
#169208=CARTESIAN_POINT('Ctrl Pts',(-12.7409296199637,-61.4710760487551,
39.8773836120367));
#169209=CARTESIAN_POINT('Ctrl Pts',(-12.7453875382446,-61.4826680729147,
39.8969946442138));
#169210=CARTESIAN_POINT('Ctrl Pts',(-12.7516316867672,-61.4936637287798,
39.9162525288249));
#169211=CARTESIAN_POINT('Ctrl Pts',(-12.7580013045741,-61.5048803302338,
39.9358973794074));
#169212=CARTESIAN_POINT('Ctrl Pts',(-12.7662298081603,-61.5154772731038,
39.9551762199754));
#169213=CARTESIAN_POINT('Ctrl Pts',(-12.7762506512866,-61.5252915748223,
39.973815203426));
#169214=CARTESIAN_POINT('Ctrl Pts',(-12.7858821937415,-61.534724599816,
39.9917300792663));
#169215=CARTESIAN_POINT('Ctrl Pts',(-12.797170047014,-61.5434353195579,
40.0090551158141));
#169216=CARTESIAN_POINT('Ctrl Pts',(-12.8100982056025,-61.5512651452187,
40.0255394551555));
#169217=CARTESIAN_POINT('Ctrl Pts',(-12.8200291684115,-61.5572797455894,
40.0382021526163));
#169218=CARTESIAN_POINT('Ctrl Pts',(-12.8309289078987,-61.5627743733243,
40.0503687782129));
#169219=CARTESIAN_POINT('Ctrl Pts',(-12.8428059312037,-61.5676673859795,
40.0619155352442));
#169220=CARTESIAN_POINT('Ctrl Pts',(-12.8428370587636,-61.5676802096931,
40.0619457972351));
#169221=CARTESIAN_POINT('Ctrl Pts',(-12.8428681938093,-61.5676930289522,
40.0619760547305));
#169222=CARTESIAN_POINT('Ctrl Pts',(-12.8428993363378,-61.5677058437553,
40.0620063077269));
#169223=CARTESIAN_POINT('Ctrl Pts',(-12.8462384487039,-61.5690798512467,
40.06525004417));
#169224=CARTESIAN_POINT('Ctrl Pts',(-12.8496624271215,-61.5704011254854,
40.0684393223557));
#169225=CARTESIAN_POINT('Ctrl Pts',(-12.8531666956981,-61.5716678181341,
40.0715697951759));
#169226=CARTESIAN_POINT('Ctrl Pts',(-12.8726671535588,-61.5787166747155,
40.0889901646425));
#169227=CARTESIAN_POINT('Ctrl Pts',(-12.8946522063791,-61.5840799821729,
40.1045963098251));
#169228=CARTESIAN_POINT('Ctrl Pts',(-12.9182844651712,-61.5874651029952,
40.1176634650736));
#169229=CARTESIAN_POINT('Ctrl Pts',(-12.9288909501836,-61.5889843920983,
40.1235281853069));
#169230=CARTESIAN_POINT('Ctrl Pts',(-12.9398294094008,-61.5901055263651,
40.1288820140923));
#169231=CARTESIAN_POINT('Ctrl Pts',(-12.9510258874722,-61.5908034580837,
40.1336621774101));
#169232=CARTESIAN_POINT('Ctrl Pts',(-12.9558917253993,-61.5911067697685,
40.1357395717319));
#169233=CARTESIAN_POINT('Ctrl Pts',(-12.9608061353937,-61.591330024696,
40.1377083672884));
#169234=CARTESIAN_POINT('Ctrl Pts',(-12.9657629422644,-61.5914710890454,
40.1395632548792));
#169235=CARTESIAN_POINT('Ctrl Pts',(-12.9831117663121,-61.5919648142682,
40.146055361447));
#169236=CARTESIAN_POINT('Ctrl Pts',(-13.0009799514312,-61.5914517017517,
40.1511520974629));
#169237=CARTESIAN_POINT('Ctrl Pts',(-13.0191027399908,-61.5898402812905,
40.1546258197408));
#169238=CARTESIAN_POINT('Ctrl Pts',(-13.0281641342706,-61.5890345710599,
40.1563626808798));
#169239=CARTESIAN_POINT('Ctrl Pts',(-13.0372891795346,-61.5879542844383,
40.1576937882008));
#169240=CARTESIAN_POINT('Ctrl Pts',(-13.0464447827192,-61.5865879953991,
40.1585906813668));
#169241=CARTESIAN_POINT('Ctrl Pts',(-13.0510225843115,-61.5859048508795,
40.1590391279498));
#169242=CARTESIAN_POINT('Ctrl Pts',(-13.0556080254097,-61.585150205876,
40.1593790209175));
#169243=CARTESIAN_POINT('Ctrl Pts',(-13.0601969695277,-61.5843226328192,
40.1596068022931));
#169244=CARTESIAN_POINT('Ctrl Pts',(-13.0647859136458,-61.5834950597623,
40.1598345836687));
#169245=CARTESIAN_POINT('Ctrl Pts',(-13.0693783604294,-61.582594556983,
40.1599502506865));
#169246=CARTESIAN_POINT('Ctrl Pts',(-13.0739701745327,-61.5816197022697,
40.1599502534424));
#169247=CARTESIAN_POINT('',(-13.103835206573,-61.5752716937451,40.1599502534424));
#169248=CARTESIAN_POINT('Origin',(-7.37250181440781E-18,1.52016511373602E-16,
40.1599502534424));
#169249=CARTESIAN_POINT('',(-13.3605623192489,-61.3267881959112,39.8576902534424));
#169250=CARTESIAN_POINT('Ctrl Pts',(-13.103835206573,-61.5752716937451,
40.1599502534424));
#169251=CARTESIAN_POINT('Ctrl Pts',(-13.107573119184,-61.5744762229326,
40.1599502447859));
#169252=CARTESIAN_POINT('Ctrl Pts',(-13.1112908564314,-61.5736362456895,
40.1598744685927));
#169253=CARTESIAN_POINT('Ctrl Pts',(-13.1149867645638,-61.5727532608743,
40.1597246934279));
#169254=CARTESIAN_POINT('Ctrl Pts',(-13.1363445541706,-61.5676506979223,
40.1588591777434));
#169255=CARTESIAN_POINT('Ctrl Pts',(-13.1569765024517,-61.5611131206551,
40.1555254706018));
#169256=CARTESIAN_POINT('Ctrl Pts',(-13.1765564394397,-61.5534303645618,
40.1500631826374));
#169257=CARTESIAN_POINT('Ctrl Pts',(-13.1844534784414,-61.5503317322961,
40.1478601162476));
#169258=CARTESIAN_POINT('Ctrl Pts',(-13.192179815575,-61.5470470005032,
40.1453112228304));
#169259=CARTESIAN_POINT('Ctrl Pts',(-13.1997158239901,-61.5435957160156,
40.1424401896328));
#169260=CARTESIAN_POINT('Ctrl Pts',(-13.2024961535652,-61.5423224015759,
40.1413809526906));
#169261=CARTESIAN_POINT('Ctrl Pts',(-13.2052504481945,-61.5410263779725,
40.1402777640511));
#169262=CARTESIAN_POINT('Ctrl Pts',(-13.2079776587163,-61.5397086090799,
40.1391317641987));
#169263=CARTESIAN_POINT('Ctrl Pts',(-13.2130911784448,-61.5372377924062,
40.1369830144753));
#169264=CARTESIAN_POINT('Ctrl Pts',(-13.2181094806068,-61.5346905274442,
40.1346837565849));
#169265=CARTESIAN_POINT('Ctrl Pts',(-13.2230256493633,-61.5320731679598,
40.1322415082996));
#169266=CARTESIAN_POINT('Ctrl Pts',(-13.2402322400107,-61.5229124097647,
40.1236936393008));
#169267=CARTESIAN_POINT('Ctrl Pts',(-13.2561876955041,-61.5128929892897,
40.113394140767));
#169268=CARTESIAN_POINT('Ctrl Pts',(-13.2705955044755,-61.5022873490354,
40.101665321223));
#169269=CARTESIAN_POINT('Ctrl Pts',(-13.2777994089612,-61.4969845289083,
40.095800911451));
#169270=CARTESIAN_POINT('Ctrl Pts',(-13.2846164020262,-61.4915351548247,
40.0895791707949));
#169271=CARTESIAN_POINT('Ctrl Pts',(-13.2910094216448,-61.4859732907799,
40.0830403822906));
#169272=CARTESIAN_POINT('Ctrl Pts',(-13.2942059314541,-61.4831923587575,
40.0797709880385));
#169273=CARTESIAN_POINT('Ctrl Pts',(-13.2972964479272,-61.4803833043594,
40.0764223317514));
#169274=CARTESIAN_POINT('Ctrl Pts',(-13.3002763384268,-61.4775503861046,
40.0729994484778));
#169275=CARTESIAN_POINT('Ctrl Pts',(-13.3032562289264,-61.4747174678498,
40.0695765652042));
#169276=CARTESIAN_POINT('Ctrl Pts',(-13.3061253662369,-61.4718606611377,
40.0660793733488));
#169277=CARTESIAN_POINT('Ctrl Pts',(-13.3088793779158,-61.4689842762858,
40.0625130768817));
#169278=CARTESIAN_POINT('Ctrl Pts',(-13.3089028638677,-61.4689597467471,
40.0624826638418));
#169279=CARTESIAN_POINT('Ctrl Pts',(-13.3089263414387,-61.4689352159237,
40.0624522459912));
#169280=CARTESIAN_POINT('Ctrl Pts',(-13.3089498106271,-61.4689106838182,
40.0624218233329));
#169281=CARTESIAN_POINT('Ctrl Pts',(-13.3209358677635,-61.4563817793404,
40.046884527591));
#169282=CARTESIAN_POINT('Ctrl Pts',(-13.3308520539308,-61.4435806031513,
40.0302263329263));
#169283=CARTESIAN_POINT('Ctrl Pts',(-13.3387946412816,-61.4306829407593,
40.0127515884783));
#169284=CARTESIAN_POINT('Ctrl Pts',(-13.3470058416626,-61.4173490879895,
39.9946858597768));
#169285=CARTESIAN_POINT('Ctrl Pts',(-13.3531077791272,-61.4039112193281,
39.9757460620557));
#169286=CARTESIAN_POINT('Ctrl Pts',(-13.3571547734325,-61.390559416733,
39.956244455921));
#169287=CARTESIAN_POINT('Ctrl Pts',(-13.3611247853904,-61.3774615935182,
39.9371138113704));
#169288=CARTESIAN_POINT('Ctrl Pts',(-13.3631169881904,-61.3644457144043,
39.9174410654458));
#169289=CARTESIAN_POINT('Ctrl Pts',(-13.3631357189472,-61.3517005934362,
39.8975196504261));
#169290=CARTESIAN_POINT('Ctrl Pts',(-13.3631481274169,-61.3432573976163,
39.8843224113852));
#169291=CARTESIAN_POINT('Ctrl Pts',(-13.3622935120792,-61.3349332352371,
39.871016044717));
#169292=CARTESIAN_POINT('Ctrl Pts',(-13.3605623192489,-61.3267881959112,
39.8576902534424));
#169293=CARTESIAN_POINT('',(-13.2864868028998,-60.9782752797347,39.2875012672119));
#169294=CARTESIAN_POINT('',(-13.3605623192489,-61.3267881959112,39.8576902534424));
#169295=CARTESIAN_POINT('',(-18.9827025415099,-59.4519788726607,39.2875012672119));
#169296=CARTESIAN_POINT('Origin',(5.53234440788222E-15,0.,39.2875012672119));
#169297=CARTESIAN_POINT('',(-19.0928077206414,-59.7908376697911,39.8576902534424));
#169298=CARTESIAN_POINT('',(-18.9827025415099,-59.4519788726607,39.2875012672119));
#169299=CARTESIAN_POINT('',(-19.4393816709759,-59.8776671349984,40.1599502534424));
#169300=CARTESIAN_POINT('Ctrl Pts',(-19.0928077206414,-59.7908376697911,
39.8576902534424));
#169301=CARTESIAN_POINT('Ctrl Pts',(-19.0966105891856,-59.8025412685591,
39.8773836120369));
#169302=CARTESIAN_POINT('Ctrl Pts',(-19.1022557829954,-59.8136038110503,
39.8969946442141));
#169303=CARTESIAN_POINT('Ctrl Pts',(-19.1096150844294,-59.8238865403127,
39.9162525288254));
#169304=CARTESIAN_POINT('Ctrl Pts',(-19.1171222629167,-59.8343758896894,
39.9358973794081));
#169305=CARTESIAN_POINT('Ctrl Pts',(-19.1264133720529,-59.8440546685628,
39.9551762199762));
#169306=CARTESIAN_POINT('Ctrl Pts',(-19.1374051938288,-59.852767743177,
39.9738152034268));
#169307=CARTESIAN_POINT('Ctrl Pts',(-19.1479699932931,-59.8611423227411,
39.9917300792672));
#169308=CARTESIAN_POINT('Ctrl Pts',(-19.1601065286729,-59.8686254222926,
40.0090551158152));
#169309=CARTESIAN_POINT('Ctrl Pts',(-19.1737823051001,-59.875060994799,
40.0255394551566));
#169310=CARTESIAN_POINT('Ctrl Pts',(-19.1842875619894,-59.8800045782782,
40.038202152617));
#169311=CARTESIAN_POINT('Ctrl Pts',(-19.1957019365562,-59.8843297728487,
40.0503687782133));
#169312=CARTESIAN_POINT('Ctrl Pts',(-19.2080253553781,-59.8879544940744,
40.0619155352442));
#169313=CARTESIAN_POINT('Ctrl Pts',(-19.2080576528611,-59.8879639938223,
40.0619457972351));
#169314=CARTESIAN_POINT('Ctrl Pts',(-19.2080899573232,-59.8879734883576,
40.0619760547305));
#169315=CARTESIAN_POINT('Ctrl Pts',(-19.2081222687613,-59.8879829776792,
40.0620063077269));
#169316=CARTESIAN_POINT('Ctrl Pts',(-19.211586712012,-59.8890004259295,
40.06525004417));
#169317=CARTESIAN_POINT('Ctrl Pts',(-19.2151300442834,-59.8899565588874,
40.0684393223556));
#169318=CARTESIAN_POINT('Ctrl Pts',(-19.2187475215461,-59.8908500166521,
40.0715697951759));
#169319=CARTESIAN_POINT('Ctrl Pts',(-19.2388779600016,-59.8958219059657,
40.08899016464));
#169320=CARTESIAN_POINT('Ctrl Pts',(-19.2613031946851,-59.8988577688774,
40.1045963098206));
#169321=CARTESIAN_POINT('Ctrl Pts',(-19.2851598349646,-59.899754101959,
40.1176634650679));
#169322=CARTESIAN_POINT('Ctrl Pts',(-19.2958670255008,-59.9001563886589,
40.1235281853035));
#169323=CARTESIAN_POINT('Ctrl Pts',(-19.3068627531394,-59.9001280009024,
40.1288820140908));
#169324=CARTESIAN_POINT('Ctrl Pts',(-19.318070849466,-59.8996517586311,
40.1336621774101));
#169325=CARTESIAN_POINT('Ctrl Pts',(-19.3229417365282,-59.8994447901817,
40.1357395717319));
#169326=CARTESIAN_POINT('Ctrl Pts',(-19.3278525613648,-59.8991531263709,
40.1377083672884));
#169327=CARTESIAN_POINT('Ctrl Pts',(-19.3327969595686,-59.8987752905501,
40.1395632548792));
#169328=CARTESIAN_POINT('Ctrl Pts',(-19.3501023532817,-59.8974528651772,
40.146055361447));
#169329=CARTESIAN_POINT('Ctrl Pts',(-19.3678190197503,-59.8950748296129,
40.151152097463));
#169330=CARTESIAN_POINT('Ctrl Pts',(-19.3856740904735,-59.8915778894433,
40.1546258197409));
#169331=CARTESIAN_POINT('Ctrl Pts',(-19.3946016258351,-59.8898294193585,
40.1563626808798));
#169332=CARTESIAN_POINT('Ctrl Pts',(-19.4035637624458,-59.8878012237014,
40.1576937882008));
#169333=CARTESIAN_POINT('Ctrl Pts',(-19.4125263941846,-59.8854853982053,
40.1585906813668));
#169334=CARTESIAN_POINT('Ctrl Pts',(-19.417007710054,-59.8843274854573,
40.1590391279498));
#169335=CARTESIAN_POINT('Ctrl Pts',(-19.4214891497435,-59.8830976653667,
40.1593790209175));
#169336=CARTESIAN_POINT('Ctrl Pts',(-19.4259664502057,-59.881794950565,
40.1596068022931));
#169337=CARTESIAN_POINT('Ctrl Pts',(-19.4304437506678,-59.8804922357632,
40.1598345836687));
#169338=CARTESIAN_POINT('Ctrl Pts',(-19.4349169113758,-59.8791166246275,
40.1599502506865));
#169339=CARTESIAN_POINT('Ctrl Pts',(-19.4393816709759,-59.8776671349984,
40.1599502534424));
#169340=CARTESIAN_POINT('',(-19.4684195516699,-59.8682321556241,40.1599502534424));
#169341=CARTESIAN_POINT('Origin',(8.34054140790947E-18,1.4780621413155E-16,
40.1599502534424));
#169342=CARTESIAN_POINT('',(-19.6977666881848,-59.5942745858235,39.8576902534424));
#169343=CARTESIAN_POINT('Ctrl Pts',(-19.4684195516699,-59.8682321556241,
40.1599502534424));
#169344=CARTESIAN_POINT('Ctrl Pts',(-19.4720538382629,-59.8670503242229,
40.1599502447858));
#169345=CARTESIAN_POINT('Ctrl Pts',(-19.4756634078263,-59.8658263391018,
40.1598744685927));
#169346=CARTESIAN_POINT('Ctrl Pts',(-19.4792467723414,-59.8645618637723,
40.1597246934279));
#169347=CARTESIAN_POINT('Ctrl Pts',(-19.4999541986752,-59.8572547562686,
40.1588591777435));
#169348=CARTESIAN_POINT('Ctrl Pts',(-19.5197897600771,-59.848596366687,
40.1555254706027));
#169349=CARTESIAN_POINT('Ctrl Pts',(-19.5384593694314,-59.8389090368127,
40.1500631826396));
#169350=CARTESIAN_POINT('Ctrl Pts',(-19.5459892523608,-59.8350019138265,
40.1478601162493));
#169351=CARTESIAN_POINT('Ctrl Pts',(-19.553329915847,-59.8309275539895,
40.1453112228313));
#169352=CARTESIAN_POINT('Ctrl Pts',(-19.560463883758,-59.8267074486192,
40.1424401896328));
#169353=CARTESIAN_POINT('Ctrl Pts',(-19.5630958847952,-59.8251504859513,
40.1413809526906));
#169354=CARTESIAN_POINT('Ctrl Pts',(-19.5656996197547,-59.8235736599159,
40.1402777640511));
#169355=CARTESIAN_POINT('Ctrl Pts',(-19.5682741459747,-59.8219780387743,
40.1391317641987));
#169356=CARTESIAN_POINT('Ctrl Pts',(-19.5731013826371,-59.8189862491338,
40.1369830144753));
#169357=CARTESIAN_POINT('Ctrl Pts',(-19.5778259323228,-59.8159283829425,
40.134683756585));
#169358=CARTESIAN_POINT('Ctrl Pts',(-19.5824415812277,-59.812811482062,
40.1322415082996));
#169359=CARTESIAN_POINT('Ctrl Pts',(-19.5985963523948,-59.8019023289803,
40.1236936393009));
#169360=CARTESIAN_POINT('Ctrl Pts',(-19.6134170876084,-59.7902699966955,
40.113394140767));
#169361=CARTESIAN_POINT('Ctrl Pts',(-19.626637377817,-59.7782164291175,
40.101665321223));
#169362=CARTESIAN_POINT('Ctrl Pts',(-19.6332475229213,-59.7721896453284,
40.095800911451));
#169363=CARTESIAN_POINT('Ctrl Pts',(-19.6394575570863,-59.766057553677,
40.0895791707949));
#169364=CARTESIAN_POINT('Ctrl Pts',(-19.645234181973,-59.759857905589,40.0830403822906));
#169365=CARTESIAN_POINT('Ctrl Pts',(-19.6481224944163,-59.756758081545,
40.0797709880385));
#169366=CARTESIAN_POINT('Ctrl Pts',(-19.6509024545773,-59.7536413685032,
40.0764223317514));
#169367=CARTESIAN_POINT('Ctrl Pts',(-19.6535699003333,-59.7505124858964,
40.0729994484778));
#169368=CARTESIAN_POINT('Ctrl Pts',(-19.6562373460892,-59.7473836032895,
40.0695765652042));
#169369=CARTESIAN_POINT('Ctrl Pts',(-19.6587921483498,-59.7442425399496,
40.0660793733488));
#169370=CARTESIAN_POINT('Ctrl Pts',(-19.6612304091763,-59.7410940396262,
40.0625130768817));
#169371=CARTESIAN_POINT('Ctrl Pts',(-19.6612512024346,-59.7410671895124,
40.0624826638418));
#169372=CARTESIAN_POINT('Ctrl Pts',(-19.6612719872239,-59.7410403389971,
40.0624522459912));
#169373=CARTESIAN_POINT('Ctrl Pts',(-19.6612927635423,-59.7410134880828,
40.0624218233329));
#169374=CARTESIAN_POINT('Ctrl Pts',(-19.6719035326728,-59.7273003341207,
40.04688452759));
#169375=CARTESIAN_POINT('Ctrl Pts',(-19.6804273096601,-59.7135327604116,
40.0302263329241));
#169376=CARTESIAN_POINT('Ctrl Pts',(-19.686978213857,-59.6998755263127,
40.0127515884749));
#169377=CARTESIAN_POINT('Ctrl Pts',(-19.6937506652838,-59.6857564136253,
39.9946858597722));
#169378=CARTESIAN_POINT('Ctrl Pts',(-19.6984145359357,-59.6717543328675,
39.9757460620498));
#169379=CARTESIAN_POINT('Ctrl Pts',(-19.7010437169752,-59.6580526467476,
39.9562444559137));
#169380=CARTESIAN_POINT('Ctrl Pts',(-19.703622885459,-59.6446115955291,
39.937113811362));
#169381=CARTESIAN_POINT('Ctrl Pts',(-19.7042436449212,-59.6314587768652,
39.9174410654362));
#169382=CARTESIAN_POINT('Ctrl Pts',(-19.7029300451593,-59.6187815171056,
39.8975196504155));
#169383=CARTESIAN_POINT('Ctrl Pts',(-19.7020598313697,-59.6103832769599,
39.8843224113781));
#169384=CARTESIAN_POINT('Ctrl Pts',(-19.700339785803,-59.6021940468434,
39.8710160447134));
#169385=CARTESIAN_POINT('Ctrl Pts',(-19.6977666881848,-59.5942745858235,
39.8576902534424));
#169386=CARTESIAN_POINT('',(-19.5876674457081,-59.255413859757,39.2875012672119));
#169387=CARTESIAN_POINT('',(-19.6977666881848,-59.5942745858235,39.8576902534424));
#169388=CARTESIAN_POINT('',(-25.0931373005748,-57.142061986502,39.2875012672119));
#169389=CARTESIAN_POINT('Origin',(5.53234440788222E-15,0.,39.2875012672119));
#169390=CARTESIAN_POINT('',(-25.2380597013433,-57.4675553545139,39.8576902534424));
#169391=CARTESIAN_POINT('',(-25.0931373005748,-57.142061986502,39.2875012672119));
#169392=CARTESIAN_POINT('',(-25.5918112338797,-57.5176823163887,40.1599502534424));
#169393=CARTESIAN_POINT('Ctrl Pts',(-25.2380597013433,-57.4675553545139,
39.8576902534424));
#169394=CARTESIAN_POINT('Ctrl Pts',(-25.2430650965695,-57.478797331738,
39.8773836120361));
#169395=CARTESIAN_POINT('Ctrl Pts',(-25.2498357159831,-57.4892091890297,
39.8969946442126));
#169396=CARTESIAN_POINT('Ctrl Pts',(-25.2582295402814,-57.4986663319553,
39.9162525288231));
#169397=CARTESIAN_POINT('Ctrl Pts',(-25.2667920292299,-57.5083135057475,
39.9358973794049));
#169398=CARTESIAN_POINT('Ctrl Pts',(-25.2770439485794,-57.5169680778972,
39.9551762199722));
#169399=CARTESIAN_POINT('Ctrl Pts',(-25.2888863203044,-57.5244844631381,
39.9738152034221));
#169400=CARTESIAN_POINT('Ctrl Pts',(-25.3002686266233,-57.5317088436262,
39.9917300792616));
#169401=CARTESIAN_POINT('Ctrl Pts',(-25.313120873688,-57.5378823365827,
40.0090551158087));
#169402=CARTESIAN_POINT('Ctrl Pts',(-25.327394433284,-57.5428531464557,
40.0255394551494));
#169403=CARTESIAN_POINT('Ctrl Pts',(-25.3383588864627,-57.5466715501095,
40.0382021526124));
#169404=CARTESIAN_POINT('Ctrl Pts',(-25.3501628378352,-57.5497799237797,
40.0503687782111));
#169405=CARTESIAN_POINT('Ctrl Pts',(-25.3627976342212,-57.5520966403719,
40.0619155352442));
#169406=CARTESIAN_POINT('Ctrl Pts',(-25.3628307477693,-57.552102712073,
40.0619457972351));
#169407=CARTESIAN_POINT('Ctrl Pts',(-25.3628638677133,-57.5521087778605,
40.0619760547305));
#169408=CARTESIAN_POINT('Ctrl Pts',(-25.3628969940503,-57.5521148377336,
40.0620063077269));
#169409=CARTESIAN_POINT('Ctrl Pts',(-25.3664488110204,-57.5527645793669,
40.06525004417));
#169410=CARTESIAN_POINT('Ctrl Pts',(-25.3700726756556,-57.5533450954512,
40.0684393223557));
#169411=CARTESIAN_POINT('Ctrl Pts',(-25.3737637277665,-57.5538555294216,
40.0715697951759));
#169412=CARTESIAN_POINT('Ctrl Pts',(-25.3943035935255,-57.5566959784089,
40.0889901646418));
#169413=CARTESIAN_POINT('Ctrl Pts',(-25.4169233145145,-57.5573711352259,
40.1045963098239));
#169414=CARTESIAN_POINT('Ctrl Pts',(-25.4407429579447,-57.5557688601533,
40.1176634650721));
#169415=CARTESIAN_POINT('Ctrl Pts',(-25.451433543779,-57.5550497369119,
40.123528185306));
#169416=CARTESIAN_POINT('Ctrl Pts',(-25.46236606834,-57.5538721381541,40.1288820140919));
#169417=CARTESIAN_POINT('Ctrl Pts',(-25.4734629846668,-57.552226939703,
40.1336621774101));
#169418=CARTESIAN_POINT('Ctrl Pts',(-25.478285554406,-57.5515119587091,
40.1357395717319));
#169419=CARTESIAN_POINT('Ctrl Pts',(-25.4831389900605,-57.5507085716896,
40.1377083672884));
#169420=CARTESIAN_POINT('Ctrl Pts',(-25.4880168077358,-57.5498159753469,
40.1395632548792));
#169421=CARTESIAN_POINT('Ctrl Pts',(-25.5050891695995,-57.5466918881475,
40.146055361447));
#169422=CARTESIAN_POINT('Ctrl Pts',(-25.5224602099123,-57.5424749837906,
40.151152097463));
#169423=CARTESIAN_POINT('Ctrl Pts',(-25.5398519389078,-57.537130837121,
40.1546258197409));
#169424=CARTESIAN_POINT('Ctrl Pts',(-25.5485478034055,-57.5344587637861,
40.1563626808798));
#169425=CARTESIAN_POINT('Ctrl Pts',(-25.557248840319,-57.5315048804295,
40.1576937882008));
#169426=CARTESIAN_POINT('Ctrl Pts',(-25.565920304143,-57.5282648911454,
40.1585906813668));
#169427=CARTESIAN_POINT('Ctrl Pts',(-25.5702560360551,-57.5266448965033,
40.1590391279498));
#169428=CARTESIAN_POINT('Ctrl Pts',(-25.5745843747449,-57.5249533754918,
40.1593790209175));
#169429=CARTESIAN_POINT('Ctrl Pts',(-25.5789009773103,-57.5231897917612,
40.1596068022931));
#169430=CARTESIAN_POINT('Ctrl Pts',(-25.5832175798758,-57.5214262080305,
40.1598345836687));
#169431=CARTESIAN_POINT('Ctrl Pts',(-25.5875224456232,-57.5195905600218,
40.1599502506865));
#169432=CARTESIAN_POINT('Ctrl Pts',(-25.5918112338797,-57.5176823163887,
40.1599502534424));
#169433=CARTESIAN_POINT('',(-25.61970381813,-57.5052637377731,40.1599502534424));
#169434=CARTESIAN_POINT('Origin',(2.35274110347535E-17,1.4197652107703E-16,
40.1599502534424));
#169435=CARTESIAN_POINT('',(-25.8191582032623,-57.2088336324698,39.8576902534424));
#169436=CARTESIAN_POINT('Ctrl Pts',(-25.61970381813,-57.5052637377731,40.1599502534424));
#169437=CARTESIAN_POINT('Ctrl Pts',(-25.6231946607006,-57.5037084941753,
40.1599502447858));
#169438=CARTESIAN_POINT('Ctrl Pts',(-25.6266565153805,-57.5021139114132,
40.1598744685927));
#169439=CARTESIAN_POINT('Ctrl Pts',(-25.6300880761868,-57.5004817994258,
40.1597246934279));
#169440=CARTESIAN_POINT('Ctrl Pts',(-25.6499182643581,-57.4910502055668,
40.1588591777434));
#169441=CARTESIAN_POINT('Ctrl Pts',(-25.6687401163254,-57.4803658667955,
40.1555254706014));
#169442=CARTESIAN_POINT('Ctrl Pts',(-25.6862948499043,-57.4687800995496,
40.1500631826363));
#169443=CARTESIAN_POINT('Ctrl Pts',(-25.6933750777819,-57.4641072931028,
40.1478601162468));
#169444=CARTESIAN_POINT('Ctrl Pts',(-25.7002496417694,-57.4592879447641,
40.1453112228299));
#169445=CARTESIAN_POINT('Ctrl Pts',(-25.7069034079254,-57.4543452548723,
40.1424401896328));
#169446=CARTESIAN_POINT('Ctrl Pts',(-25.7093582436704,-57.4525217023851,
40.1413809526905));
#169447=CARTESIAN_POINT('Ctrl Pts',(-25.7117828918951,-57.4506813499536,
40.1402777640511));
#169448=CARTESIAN_POINT('Ctrl Pts',(-25.7141765267651,-57.4488253585221,
40.1391317641987));
#169449=CARTESIAN_POINT('Ctrl Pts',(-25.7186645921465,-57.4453453745882,
40.1369830144753));
#169450=CARTESIAN_POINT('Ctrl Pts',(-25.7230436262008,-57.4418104097895,
40.1346837565849));
#169451=CARTESIAN_POINT('Ctrl Pts',(-25.7273081852389,-57.4382281169312,
40.1322415082996));
#169452=CARTESIAN_POINT('Ctrl Pts',(-25.742234141872,-57.4256900919269,
40.1236936393009));
#169453=CARTESIAN_POINT('Ctrl Pts',(-25.7557577777295,-57.4125722940992,
40.113394140767));
#169454=CARTESIAN_POINT('Ctrl Pts',(-25.7676457049092,-57.399202860606,
40.101665321223));
#169455=CARTESIAN_POINT('Ctrl Pts',(-25.7735896684991,-57.3925181438595,
40.095800911451));
#169456=CARTESIAN_POINT('Ctrl Pts',(-25.7791247053302,-57.3857705191196,
40.0895791707949));
#169457=CARTESIAN_POINT('Ctrl Pts',(-25.7842216455739,-57.3790010116302,
40.0830403822906));
#169458=CARTESIAN_POINT('Ctrl Pts',(-25.7867701156958,-57.3756162578856,
40.0797709880385));
#169459=CARTESIAN_POINT('Ctrl Pts',(-25.7892090617194,-57.3722260335604,
40.0764223317514));
#169460=CARTESIAN_POINT('Ctrl Pts',(-25.7915348376378,-57.3688354672941,
40.0729994484778));
#169461=CARTESIAN_POINT('Ctrl Pts',(-25.7938606135562,-57.3654449010278,
40.0695765652042));
#169462=CARTESIAN_POINT('Ctrl Pts',(-25.7960730898187,-57.3620539952073,
40.0660793733488));
#169463=CARTESIAN_POINT('Ctrl Pts',(-25.7981688856969,-57.3586678750409,
40.0625130768817));
#169464=CARTESIAN_POINT('Ctrl Pts',(-25.7981867584464,-57.3586389985275,
40.0624826638418));
#169465=CARTESIAN_POINT('Ctrl Pts',(-25.7982046227313,-57.3586101225,40.0624522459912));
#169466=CARTESIAN_POINT('Ctrl Pts',(-25.7982224785501,-57.3585812469612,
40.0624218233329));
#169467=CARTESIAN_POINT('Ctrl Pts',(-25.8073417058667,-57.3438340877002,
40.0468845275903));
#169468=CARTESIAN_POINT('Ctrl Pts',(-25.8143796853889,-57.3292509568911,
40.0302263329247));
#169469=CARTESIAN_POINT('Ctrl Pts',(-25.8194671333544,-57.314983782601,
40.0127515884759));
#169470=CARTESIAN_POINT('Ctrl Pts',(-25.8247266354318,-57.3002341019502,
39.9946858597735));
#169471=CARTESIAN_POINT('Ctrl Pts',(-25.8279013409282,-57.2858212188239,
39.9757460620513));
#169472=CARTESIAN_POINT('Ctrl Pts',(-25.8290839028447,-57.2719197677207,
39.9562444559156));
#169473=CARTESIAN_POINT('Ctrl Pts',(-25.8302439699452,-57.2582827514691,
39.9371138113642));
#169474=CARTESIAN_POINT('Ctrl Pts',(-25.8294864848998,-57.2451370982896,
39.9174410654388));
#169475=CARTESIAN_POINT('Ctrl Pts',(-25.8268549466938,-57.23266659445,39.8975196504183));
#169476=CARTESIAN_POINT('Ctrl Pts',(-25.8251116448899,-57.2244053228521,
39.88432241138));
#169477=CARTESIAN_POINT('Ctrl Pts',(-25.8225450142732,-57.2164407479142,
39.8710160447144));
#169478=CARTESIAN_POINT('Ctrl Pts',(-25.8191582032623,-57.2088336324698,
39.8576902534424));
#169479=CARTESIAN_POINT('',(-25.6742415049982,-56.8833377255393,39.2875012672119));
#169480=CARTESIAN_POINT('',(-25.8191582032623,-57.2088336324698,39.8576902534424));
#169481=CARTESIAN_POINT('',(-30.9286463962981,-54.206084711474,39.2875012672119));
#169482=CARTESIAN_POINT('Origin',(5.53234440788222E-15,0.,39.2875012672119));
#169483=CARTESIAN_POINT('',(-31.1067982185537,-54.5146464769136,39.8576902534424));
#169484=CARTESIAN_POINT('',(-30.9286463962981,-54.206084711474,39.2875012672119));
#169485=CARTESIAN_POINT('',(-31.4638515574743,-54.5275217339718,40.1599502534424));
#169486=CARTESIAN_POINT('Ctrl Pts',(-31.1067982185537,-54.5146464769136,
39.8576902534424));
#169487=CARTESIAN_POINT('Ctrl Pts',(-31.1129513003034,-54.5253036631377,
39.8773836120333));
#169488=CARTESIAN_POINT('Ctrl Pts',(-31.1207731649965,-54.5349507607419,
39.896994644207));
#169489=CARTESIAN_POINT('Ctrl Pts',(-31.1301095476621,-54.5434787028934,
39.9162525288149));
#169490=CARTESIAN_POINT('Ctrl Pts',(-31.1396335346499,-54.5521780046457,
39.9358973793941));
#169491=CARTESIAN_POINT('Ctrl Pts',(-31.1507339420374,-54.559713548768,
39.9551762199589));
#169492=CARTESIAN_POINT('Ctrl Pts',(-31.1632971162072,-54.565950893546,
39.9738152034066));
#169493=CARTESIAN_POINT('Ctrl Pts',(-31.1753722224493,-54.5719459231339,
39.9917300792442));
#169494=CARTESIAN_POINT('Ctrl Pts',(-31.1887993692891,-54.576742171415,
40.0090551157898));
#169495=CARTESIAN_POINT('Ctrl Pts',(-31.2035143279466,-54.5801937574222,
40.0255394551292));
#169496=CARTESIAN_POINT('Ctrl Pts',(-31.2148178485749,-54.5828451460221,
40.0382021525994));
#169497=CARTESIAN_POINT('Ctrl Pts',(-31.2268820501958,-54.5847026428001,
40.050368778205));
#169498=CARTESIAN_POINT('Ctrl Pts',(-31.2396897946772,-54.5856859723271,
40.0619155352442));
#169499=CARTESIAN_POINT('Ctrl Pts',(-31.2397233614914,-54.5856885494584,
40.0619457972351));
#169500=CARTESIAN_POINT('Ctrl Pts',(-31.2397569340484,-54.58569112004,40.0619760547305));
#169501=CARTESIAN_POINT('Ctrl Pts',(-31.239790512345,-54.5856936840715,
40.0620063077269));
#169502=CARTESIAN_POINT('Ctrl Pts',(-31.2433907885846,-54.5859686003824,
40.06525004417));
#169503=CARTESIAN_POINT('Ctrl Pts',(-31.2470554817643,-54.5861671393375,
40.0684393223556));
#169504=CARTESIAN_POINT('Ctrl Pts',(-31.2507796687841,-54.5862889570922,
40.0715697951759));
#169505=CARTESIAN_POINT('Ctrl Pts',(-31.2715039227789,-54.5869668451993,
40.0889901646435));
#169506=CARTESIAN_POINT('Ctrl Pts',(-31.2940703036764,-54.5852738987617,
40.1045963098268));
#169507=CARTESIAN_POINT('Ctrl Pts',(-31.317591977259,-54.5811905703954,
40.1176634650757));
#169508=CARTESIAN_POINT('Ctrl Pts',(-31.328148830096,-54.5793579160778,
40.1235281853082));
#169509=CARTESIAN_POINT('Ctrl Pts',(-31.3388983725528,-54.5770440083377,
40.1288820140929));
#169510=CARTESIAN_POINT('Ctrl Pts',(-31.3497625287428,-54.5742478788458,
40.1336621774101));
#169511=CARTESIAN_POINT('Ctrl Pts',(-31.3544839440758,-54.5730327187887,
40.1357395717319));
#169512=CARTESIAN_POINT('Ctrl Pts',(-31.3592268152914,-54.5717264106368,
40.1377083672884));
#169513=CARTESIAN_POINT('Ctrl Pts',(-31.3639846100471,-54.5703288332446,
40.1395632548792));
#169514=CARTESIAN_POINT('Ctrl Pts',(-31.380636891692,-54.5654373123718,
40.146055361447));
#169515=CARTESIAN_POINT('Ctrl Pts',(-31.3974719850963,-54.559427740509,
40.1511520974629));
#169516=CARTESIAN_POINT('Ctrl Pts',(-31.4142098249418,-54.5522949389284,
40.1546258197409));
#169517=CARTESIAN_POINT('Ctrl Pts',(-31.4225787448645,-54.5487285381382,
40.1563626808798));
#169518=CARTESIAN_POINT('Ctrl Pts',(-31.4309233516994,-54.5448813304463,
40.1576937882008));
#169519=CARTESIAN_POINT('Ctrl Pts',(-31.4392086412365,-54.5407526753746,
40.1585906813668));
#169520=CARTESIAN_POINT('Ctrl Pts',(-31.443351286005,-54.5386883478388,
40.1590391279498));
#169521=CARTESIAN_POINT('Ctrl Pts',(-31.4474791015107,-54.5365536585646,
40.1593790209175));
#169522=CARTESIAN_POINT('Ctrl Pts',(-31.4515877125784,-54.5343485280975,
40.1596068022931));
#169523=CARTESIAN_POINT('Ctrl Pts',(-31.4556963236462,-54.5321433976303,
40.1598345836687));
#169524=CARTESIAN_POINT('Ctrl Pts',(-31.4597857294232,-54.5298678244923,
40.1599502506865));
#169525=CARTESIAN_POINT('Ctrl Pts',(-31.4638515574743,-54.5275217339718,
40.1599502534424));
#169526=CARTESIAN_POINT('',(-31.490293248291,-54.5122556166609,40.1599502534424));
#169527=CARTESIAN_POINT('Origin',(3.80217165444497E-17,1.34591303547096E-16,
40.1599502534424));
#169528=CARTESIAN_POINT('',(-31.6576696180587,-54.1966007261206,39.8576902534424));
#169529=CARTESIAN_POINT('Ctrl Pts',(-31.490293248291,-54.5122556166609,
40.1599502534424));
#169530=CARTESIAN_POINT('Ctrl Pts',(-31.4936024004374,-54.5103440004409,
40.1599502447858));
#169531=CARTESIAN_POINT('Ctrl Pts',(-31.4968786114295,-54.5083962906203,
40.1598744685927));
#169532=CARTESIAN_POINT('Ctrl Pts',(-31.5001207716287,-54.5064144237354,
40.1597246934279));
#169533=CARTESIAN_POINT('Ctrl Pts',(-31.5188564579439,-54.4949616780375,
40.1588591777433));
#169534=CARTESIAN_POINT('Ctrl Pts',(-31.5364583843255,-54.4823684499286,
40.1555254706007));
#169535=CARTESIAN_POINT('Ctrl Pts',(-31.5527059087924,-54.4690111814025,
40.1500631826348));
#169536=CARTESIAN_POINT('Ctrl Pts',(-31.5592589091622,-54.4636238877399,
40.1478601162456));
#169537=CARTESIAN_POINT('Ctrl Pts',(-31.5655920544915,-54.4581123526876,
40.1453112228293));
#169538=CARTESIAN_POINT('Ctrl Pts',(-31.57169271884,-54.4525012314183,40.1424401896328));
#169539=CARTESIAN_POINT('Ctrl Pts',(-31.5739434935988,-54.4504310683344,
40.1413809526906));
#169540=CARTESIAN_POINT('Ctrl Pts',(-31.5761624901353,-54.4483473527932,
40.1402777640512));
#169541=CARTESIAN_POINT('Ctrl Pts',(-31.5783490084909,-54.4462513257025,
40.1391317641987));
#169542=CARTESIAN_POINT('Ctrl Pts',(-31.5824487304078,-54.4423212749072,
40.1369830144753));
#169543=CARTESIAN_POINT('Ctrl Pts',(-31.5864342712172,-54.4383479413153,
40.134683756585));
#169544=CARTESIAN_POINT('Ctrl Pts',(-31.5903010169872,-54.4343395048293,
40.1322415082996));
#169545=CARTESIAN_POINT('Ctrl Pts',(-31.6038346271821,-54.4203099771282,
40.1236936393009));
#169546=CARTESIAN_POINT('Ctrl Pts',(-31.6159129958989,-54.4058504350956,
40.113394140767));
#169547=CARTESIAN_POINT('Ctrl Pts',(-31.6263383134319,-54.3913116139984,
40.101665321223));
#169548=CARTESIAN_POINT('Ctrl Pts',(-31.6315509721984,-54.3840422034499,
40.095800911451));
#169549=CARTESIAN_POINT('Ctrl Pts',(-31.6363503686739,-54.3767529740102,
40.0895791707949));
#169550=CARTESIAN_POINT('Ctrl Pts',(-31.6407117811307,-54.3694877752602,
40.0830403822906));
#169551=CARTESIAN_POINT('Ctrl Pts',(-31.6428924873591,-54.3658551758851,
40.0797709880385));
#169552=CARTESIAN_POINT('Ctrl Pts',(-31.6449636976424,-54.3622285842837,
40.0764223317514));
#169553=CARTESIAN_POINT('Ctrl Pts',(-31.6469223220355,-54.3586134821115,
40.0729994484778));
#169554=CARTESIAN_POINT('Ctrl Pts',(-31.6488809464287,-54.3549983799394,
40.0695765652042));
#169555=CARTESIAN_POINT('Ctrl Pts',(-31.6507268563402,-54.3513947831119,
40.0660793733488));
#169556=CARTESIAN_POINT('Ctrl Pts',(-31.6524572252919,-54.3478081421436,
40.0625130768817));
#169557=CARTESIAN_POINT('Ctrl Pts',(-31.6524719817151,-54.3477775556078,
40.0624826638418));
#169558=CARTESIAN_POINT('Ctrl Pts',(-31.6524867297707,-54.3477469704399,
40.0624522459912));
#169559=CARTESIAN_POINT('Ctrl Pts',(-31.6525014694577,-54.347716386643,
40.0624218233329));
#169560=CARTESIAN_POINT('Ctrl Pts',(-31.6600292427982,-54.3320967950452,
40.0468845275896));
#169561=CARTESIAN_POINT('Ctrl Pts',(-31.6655043152793,-54.3168578829677,
40.0302263329231));
#169562=CARTESIAN_POINT('Ctrl Pts',(-31.6690725678687,-54.3021370826328,
40.0127515884733));
#169563=CARTESIAN_POINT('Ctrl Pts',(-31.6727614963913,-54.2869184346054,
39.9946858597698));
#169564=CARTESIAN_POINT('Ctrl Pts',(-31.6744122539941,-54.2722526596734,
39.9757460620465));
#169565=CARTESIAN_POINT('Ctrl Pts',(-31.6741352403913,-54.2583037507934,
39.9562444559096));
#169566=CARTESIAN_POINT('Ctrl Pts',(-31.6738634961701,-54.2446201795118,
39.9371138113571));
#169567=CARTESIAN_POINT('Ctrl Pts',(-31.6717360657809,-54.2316257183431,
39.9174410654305));
#169568=CARTESIAN_POINT('Ctrl Pts',(-31.6678154208133,-54.2194985998727,
39.8975196504089));
#169569=CARTESIAN_POINT('Ctrl Pts',(-31.6652181309745,-54.2114648090456,
39.8843224113736));
#169570=CARTESIAN_POINT('Ctrl Pts',(-31.6618330358507,-54.2038121508387,
39.8710160447113));
#169571=CARTESIAN_POINT('Ctrl Pts',(-31.6576696180587,-54.1966007261206,
39.8576902534424));
#169572=CARTESIAN_POINT('',(-31.4795232016792,-53.8880358395969,39.2875012672119));
#169573=CARTESIAN_POINT('',(-31.6576696180587,-54.1966007261206,39.8576902534424));
#169574=CARTESIAN_POINT('',(-36.4252947698681,-50.6762142289946,39.2875012672119));
#169575=CARTESIAN_POINT('Origin',(5.53234440788222E-15,0.,39.2875012672119));
#169576=CARTESIAN_POINT('',(-36.6347241449657,-50.9644637245891,39.8576902534424));
#169577=CARTESIAN_POINT('',(-36.4252947698681,-50.6762142289946,39.2875012672119));
#169578=CARTESIAN_POINT('',(-36.991167339171,-50.93994621282,40.1599502534424));
#169579=CARTESIAN_POINT('Ctrl Pts',(-36.6347241449657,-50.9644637245891,
39.8576902534424));
#169580=CARTESIAN_POINT('Ctrl Pts',(-36.641957498789,-50.9744193574523,
39.8773836120336));
#169581=CARTESIAN_POINT('Ctrl Pts',(-36.6507449107767,-50.9831959997502,
39.8969946442077));
#169582=CARTESIAN_POINT('Ctrl Pts',(-36.6609215604495,-50.9907013072098,
39.9162525288159));
#169583=CARTESIAN_POINT('Ctrl Pts',(-36.6713026986838,-50.9983574255528,
39.9358973793952));
#169584=CARTESIAN_POINT('Ctrl Pts',(-36.6831299757253,-51.0046913806501,
39.9551762199601));
#169585=CARTESIAN_POINT('Ctrl Pts',(-36.6962763075769,-51.0095813473111,
39.9738152034078));
#169586=CARTESIAN_POINT('Ctrl Pts',(-36.7089119163533,-51.0142813432002,
39.9917300792449));
#169587=CARTESIAN_POINT('Ctrl Pts',(-36.7227668523395,-51.0176477981061,
40.0090551157899));
#169588=CARTESIAN_POINT('Ctrl Pts',(-36.7377619898945,-51.0195423439486,
40.0255394551289));
#169589=CARTESIAN_POINT('Ctrl Pts',(-36.74928073423,-51.0209976683236,40.0382021525992));
#169590=CARTESIAN_POINT('Ctrl Pts',(-36.7614730081759,-51.0215839370839,
40.0503687782048));
#169591=CARTESIAN_POINT('Ctrl Pts',(-36.7743133764174,-51.0212231059803,
40.0619155352442));
#169592=CARTESIAN_POINT('Ctrl Pts',(-36.7743470287326,-51.0212221603063,
40.0619457972351));
#169593=CARTESIAN_POINT('Ctrl Pts',(-36.7743806860745,-51.0212212075182,
40.0619760547305));
#169594=CARTESIAN_POINT('Ctrl Pts',(-36.77441434844,-51.0212202476159,40.0620063077269));
#169595=CARTESIAN_POINT('Ctrl Pts',(-36.7780236385692,-51.0211173265639,
40.06525004417));
#169596=CARTESIAN_POINT('Ctrl Pts',(-36.7816890091481,-51.0209317131554,
40.0684393223557));
#169597=CARTESIAN_POINT('Ctrl Pts',(-36.7854055281044,-51.0206635800336,
40.0715697951759));
#169598=CARTESIAN_POINT('Ctrl Pts',(-36.8060871110681,-51.0191714801764,
40.0889901646423));
#169599=CARTESIAN_POINT('Ctrl Pts',(-36.8283529098788,-51.0151289787601,
40.1045963098247));
#169600=CARTESIAN_POINT('Ctrl Pts',(-36.8513189052316,-51.0086093349016,
40.1176634650731));
#169601=CARTESIAN_POINT('Ctrl Pts',(-36.8616263619861,-51.0056832284519,
40.1235281853066));
#169602=CARTESIAN_POINT('Ctrl Pts',(-36.872075148106,-51.0022583633861,
40.1288820140922));
#169603=CARTESIAN_POINT('Ctrl Pts',(-36.8825875141943,-50.9983419378323,
40.1336621774101));
#169604=CARTESIAN_POINT('Ctrl Pts',(-36.8871560463067,-50.9966399122599,
40.1357395717319));
#169605=CARTESIAN_POINT('Ctrl Pts',(-36.8917363891939,-50.9948449951611,
40.1377083672884));
#169606=CARTESIAN_POINT('Ctrl Pts',(-36.896322033635,-50.9929577488697,
40.1395632548792));
#169607=CARTESIAN_POINT('Ctrl Pts',(-36.9123717891789,-50.9863523868499,
40.146055361447));
#169608=CARTESIAN_POINT('Ctrl Pts',(-36.9284864868683,-50.978615989608,
40.1511520974629));
#169609=CARTESIAN_POINT('Ctrl Pts',(-36.9443870542877,-50.9697726815834,
40.1546258197408));
#169610=CARTESIAN_POINT('Ctrl Pts',(-36.9523373379975,-50.9653510275711,
40.1563626808798));
#169611=CARTESIAN_POINT('Ctrl Pts',(-36.9602340894951,-50.9606526463564,
40.1576937882008));
#169612=CARTESIAN_POINT('Ctrl Pts',(-36.9680424293792,-50.9556805599062,
40.1585906813668));
#169613=CARTESIAN_POINT('Ctrl Pts',(-36.9719465993212,-50.953194516681,
40.1590391279498));
#169614=CARTESIAN_POINT('Ctrl Pts',(-36.9758286664323,-50.9506400472467,
40.1593790209175));
#169615=CARTESIAN_POINT('Ctrl Pts',(-36.9796842711996,-50.9480175299139,
40.1596068022931));
#169616=CARTESIAN_POINT('Ctrl Pts',(-36.983539875967,-50.9453950125811,
40.1598345836687));
#169617=CARTESIAN_POINT('Ctrl Pts',(-36.9873690173881,-50.9427044459692,
40.1599502506865));
#169618=CARTESIAN_POINT('Ctrl Pts',(-36.991167339171,-50.93994621282,40.1599502534424));
#169619=CARTESIAN_POINT('',(-37.0158684358562,-50.9219998155898,40.1599502534424));
#169620=CARTESIAN_POINT('Origin',(5.16646552926933E-17,1.25731475530457E-16,
40.1599502534424));
#169621=CARTESIAN_POINT('',(-37.1493329797263,-50.5905785208482,39.8576902534424));
#169622=CARTESIAN_POINT('Ctrl Pts',(-37.0158684358562,-50.9219998155898,
40.1599502534424));
#169623=CARTESIAN_POINT('Ctrl Pts',(-37.0189596418151,-50.9197527708149,
40.1599502447858));
#169624=CARTESIAN_POINT('Ctrl Pts',(-37.0220143142661,-50.9174732734521,
40.1598744685927));
#169625=CARTESIAN_POINT('Ctrl Pts',(-37.0250315520727,-50.9151633654181,
40.1597246934279));
#169626=CARTESIAN_POINT('Ctrl Pts',(-37.0424674644255,-50.9018149465641,
40.1588591777435));
#169627=CARTESIAN_POINT('Ctrl Pts',(-37.0586566148271,-50.8874508031651,
40.1555254706024));
#169628=CARTESIAN_POINT('Ctrl Pts',(-37.0734189188993,-50.8724683783931,
40.150063182639));
#169629=CARTESIAN_POINT('Ctrl Pts',(-37.0793728957238,-50.8664256218268,
40.1478601162488));
#169630=CARTESIAN_POINT('Ctrl Pts',(-37.0850952351349,-50.8602822855875,
40.145311222831));
#169631=CARTESIAN_POINT('Ctrl Pts',(-37.0905759575257,-50.8540642095544,
40.1424401896328));
#169632=CARTESIAN_POINT('Ctrl Pts',(-37.092598011339,-50.8517701170138,
40.1413809526905));
#169633=CARTESIAN_POINT('Ctrl Pts',(-37.0945870443968,-50.8494658679864,
40.1402777640511));
#169634=CARTESIAN_POINT('Ctrl Pts',(-37.0965424902854,-50.8471527697477,
40.1391317641987));
#169635=CARTESIAN_POINT('Ctrl Pts',(-37.1002089513264,-50.8428157105502,
40.1369830144753));
#169636=CARTESIAN_POINT('Ctrl Pts',(-37.1037573324719,-50.8384475408393,
40.1346837565849));
#169637=CARTESIAN_POINT('Ctrl Pts',(-37.107183900098,-50.8340568779946,
40.1322415082996));
#169638=CARTESIAN_POINT('Ctrl Pts',(-37.1191768867892,-50.8186895580381,
40.1236936393009));
#169639=CARTESIAN_POINT('Ctrl Pts',(-37.1296776552302,-50.8030466935689,
40.113394140767));
#169640=CARTESIAN_POINT('Ctrl Pts',(-37.1385261411559,-50.7874977752341,
40.101665321223));
#169641=CARTESIAN_POINT('Ctrl Pts',(-37.1429503841188,-50.7797233160668,
40.095800911451));
#169642=CARTESIAN_POINT('Ctrl Pts',(-37.1469615570465,-50.7719723442505,
40.0895791707949));
#169643=CARTESIAN_POINT('Ctrl Pts',(-37.1505396571688,-50.7642910532776,
40.0830403822906));
#169644=CARTESIAN_POINT('Ctrl Pts',(-37.1523287072299,-50.7604504077911,
40.0797709880385));
#169645=CARTESIAN_POINT('Ctrl Pts',(-37.1540094891596,-50.7566271826099,
40.0764223317514));
#169646=CARTESIAN_POINT('Ctrl Pts',(-37.1555795029288,-50.7528271523478,
40.0729994484778));
#169647=CARTESIAN_POINT('Ctrl Pts',(-37.1571495166979,-50.7490271220856,
40.0695765652042));
#169648=CARTESIAN_POINT('Ctrl Pts',(-37.1586086360832,-50.7452503160123,
40.0660793733488));
#169649=CARTESIAN_POINT('Ctrl Pts',(-37.159954619824,-50.7415024502311,
40.0625130768817));
#169650=CARTESIAN_POINT('Ctrl Pts',(-37.1599660982464,-50.7414704887852,
40.0624826638418));
#169651=CARTESIAN_POINT('Ctrl Pts',(-37.15997756849,-50.7414385295745,40.0624522459912));
#169652=CARTESIAN_POINT('Ctrl Pts',(-37.1599890305542,-50.741406572602,
40.0624218233329));
#169653=CARTESIAN_POINT('Ctrl Pts',(-37.1658428740573,-50.7250856801843,
40.0468845275916));
#169654=CARTESIAN_POINT('Ctrl Pts',(-37.1696950534569,-50.709357947551,
40.0302263329275));
#169655=CARTESIAN_POINT('Ctrl Pts',(-37.1717050161484,-50.6943448053427,
40.0127515884803));
#169656=CARTESIAN_POINT('Ctrl Pts',(-37.1737829544435,-50.6788239286339,
39.9946858597795));
#169657=CARTESIAN_POINT('Ctrl Pts',(-37.1738916781079,-50.6640659431977,
39.9757460620591));
#169658=CARTESIAN_POINT('Ctrl Pts',(-37.1721581240063,-50.6502224037077,
39.9562444559252));
#169659=CARTESIAN_POINT('Ctrl Pts',(-37.1704575457515,-50.6366421974684,
39.9371138113754));
#169660=CARTESIAN_POINT('Ctrl Pts',(-37.1669834785932,-50.6239412983478,
39.9174410654515));
#169661=CARTESIAN_POINT('Ctrl Pts',(-37.1618166822734,-50.6122904324954,
39.8975196504326));
#169662=CARTESIAN_POINT('Ctrl Pts',(-37.1583938608496,-50.6045721423254,
39.8843224113896));
#169663=CARTESIAN_POINT('Ctrl Pts',(-37.1542273890267,-50.5973152449674,
39.8710160447192));
#169664=CARTESIAN_POINT('Ctrl Pts',(-37.1493329797263,-50.5905785208482,
39.8576902534424));
#169665=CARTESIAN_POINT('',(-36.9399086546489,-50.3023253561993,39.2875012672119));
#169666=CARTESIAN_POINT('',(-37.1493329797263,-50.5905785208482,39.8576902534424));
#169667=CARTESIAN_POINT('',(-41.5228599914565,-46.5911245387428,39.2875012672119));
#169668=CARTESIAN_POINT('Origin',(5.53234440788222E-15,0.,39.2875012672119));
#169669=CARTESIAN_POINT('',(-41.7612723673365,-46.8559036426983,39.8576902534424));
#169670=CARTESIAN_POINT('',(-41.5228599914565,-46.5911245387428,39.2875012672119));
#169671=CARTESIAN_POINT('',(-42.1132001506003,-46.7942619810915,40.1599502534424));
#169672=CARTESIAN_POINT('Ctrl Pts',(-41.7612723673365,-46.8559036426983,
39.8576902534424));
#169673=CARTESIAN_POINT('Ctrl Pts',(-41.7695067430955,-46.8650486462049,
39.8773836120361));
#169674=CARTESIAN_POINT('Ctrl Pts',(-41.7791634256543,-46.8728586744677,
39.8969946442126));
#169675=CARTESIAN_POINT('Ctrl Pts',(-41.7900688448321,-46.8792591175168,
39.9162525288231));
#169676=CARTESIAN_POINT('Ctrl Pts',(-41.8011933963918,-46.8857881704164,
39.9358973794051));
#169677=CARTESIAN_POINT('Ctrl Pts',(-41.813617960967,-46.8908511403512,
39.9551762199724));
#169678=CARTESIAN_POINT('Ctrl Pts',(-41.8272034165403,-46.8943401533968,
39.9738152034225));
#169679=CARTESIAN_POINT('Ctrl Pts',(-41.8402610894803,-46.8976936214485,
39.9917300792623));
#169680=CARTESIAN_POINT('Ctrl Pts',(-41.8543920170388,-46.8995933993941,
40.0090551158097));
#169681=CARTESIAN_POINT('Ctrl Pts',(-41.8695030436303,-46.8999101480296,
40.0255394551508));
#169682=CARTESIAN_POINT('Ctrl Pts',(-41.8811108098936,-46.90015346334,40.0382021526132));
#169683=CARTESIAN_POINT('Ctrl Pts',(-41.893297575053,-46.8994620807992,
40.0503687782115));
#169684=CARTESIAN_POINT('Ctrl Pts',(-41.9060298852857,-46.897761042407,
40.0619155352442));
#169685=CARTESIAN_POINT('Ctrl Pts',(-41.9060632544001,-46.8977565842888,
40.0619457972351));
#169686=CARTESIAN_POINT('Ctrl Pts',(-41.9060966277702,-46.8977521185699,
40.0619760547305));
#169687=CARTESIAN_POINT('Ctrl Pts',(-41.9061300053926,-46.8977476452507,
40.0620063077269));
#169688=CARTESIAN_POINT('Ctrl Pts',(-41.9097087652733,-46.8972680144603,
40.06525004417));
#169689=CARTESIAN_POINT('Ctrl Pts',(-41.9133346546844,-46.8967002823075,
40.0684393223556));
#169690=CARTESIAN_POINT('Ctrl Pts',(-41.9170027866178,-46.8960451360318,
40.0715697951759));
#169691=CARTESIAN_POINT('Ctrl Pts',(-41.9374151067974,-46.8923993959692,
40.0889901646392));
#169692=CARTESIAN_POINT('Ctrl Pts',(-41.9591363747676,-46.8860516300672,
40.1045963098192));
#169693=CARTESIAN_POINT('Ctrl Pts',(-41.9812950716372,-46.8771671013007,
40.1176634650662));
#169694=CARTESIAN_POINT('Ctrl Pts',(-41.9912402016585,-46.8731796017523,
40.1235281853024));
#169695=CARTESIAN_POINT('Ctrl Pts',(-42.0012737523565,-46.8686813028981,
40.1288820140903));
#169696=CARTESIAN_POINT('Ctrl Pts',(-42.0113191526628,-46.8636874904588,
40.1336621774101));
#169697=CARTESIAN_POINT('Ctrl Pts',(-42.0156847477608,-46.8615172471195,
40.1357395717319));
#169698=CARTESIAN_POINT('Ctrl Pts',(-42.0200523791243,-46.8592533865611,
40.1377083672884));
#169699=CARTESIAN_POINT('Ctrl Pts',(-42.0244156319707,-46.8568971484358,
40.1395632548792));
#169700=CARTESIAN_POINT('Ctrl Pts',(-42.0396870169331,-46.8486503149974,
40.146055361447));
#169701=CARTESIAN_POINT('Ctrl Pts',(-42.0549047629075,-46.8392718539636,
40.151152097463));
#169702=CARTESIAN_POINT('Ctrl Pts',(-42.069793847957,-46.8288149286282,
40.1546258197409));
#169703=CARTESIAN_POINT('Ctrl Pts',(-42.0772383904817,-46.8235864659605,
40.1563626808798));
#169704=CARTESIAN_POINT('Ctrl Pts',(-42.0846007681801,-46.8180883876709,
40.1576937882008));
#169705=CARTESIAN_POINT('Ctrl Pts',(-42.0918466086054,-46.8123273450617,
40.1585906813668));
#169706=CARTESIAN_POINT('Ctrl Pts',(-42.095469528818,-46.8094468237571,
40.1590391279498));
#169707=CARTESIAN_POINT('Ctrl Pts',(-42.0990633147948,-46.8065005614642,
40.1593790209175));
#169708=CARTESIAN_POINT('Ctrl Pts',(-42.1026236704492,-46.8034893901144,
40.1596068022931));
#169709=CARTESIAN_POINT('Ctrl Pts',(-42.1061840261036,-46.8004782187647,
40.1598345836687));
#169710=CARTESIAN_POINT('Ctrl Pts',(-42.1097109502941,-46.7974021370899,
40.1599502506865));
#169711=CARTESIAN_POINT('Ctrl Pts',(-42.1132001506003,-46.7942619810915,
40.1599502534424));
#169712=CARTESIAN_POINT('',(-42.1358900227697,-46.7738319284255,40.1599502534424));
#169713=CARTESIAN_POINT('Origin',(6.43067523875937E-17,1.15494107156903E-16,
40.1599502534424));
#169714=CARTESIAN_POINT('',(-42.2339804752703,-46.4302753505423,39.8576902534424));
#169715=CARTESIAN_POINT('Ctrl Pts',(-42.1358900227697,-46.7738319284255,
40.1599502534424));
#169716=CARTESIAN_POINT('Ctrl Pts',(-42.1387294146417,-46.7712740741885,
40.1599502447858));
#169717=CARTESIAN_POINT('Ctrl Pts',(-42.141529080921,-46.7686877639337,
40.1598744685927));
#169718=CARTESIAN_POINT('Ctrl Pts',(-42.1442883388461,-46.7660751225864,
40.1597246934279));
#169719=CARTESIAN_POINT('Ctrl Pts',(-42.1602334457364,-46.750977278644,
40.1588591777436));
#169720=CARTESIAN_POINT('Ctrl Pts',(-42.1748324484421,-46.7349995965129,
40.1555254706026));
#169721=CARTESIAN_POINT('Ctrl Pts',(-42.1879477932303,-46.718556166073,
40.1500631826395));
#169722=CARTESIAN_POINT('Ctrl Pts',(-42.1932375134894,-46.7119241523112,
40.1478601162492));
#169723=CARTESIAN_POINT('Ctrl Pts',(-42.1982863518304,-46.7052163225652,
40.1453112228313));
#169724=CARTESIAN_POINT('Ctrl Pts',(-42.2030870843187,-46.6984594183137,
40.1424401896328));
#169725=CARTESIAN_POINT('Ctrl Pts',(-42.2048582631417,-46.6959665308743,
40.1413809526906));
#169726=CARTESIAN_POINT('Ctrl Pts',(-42.2065955404585,-46.6934669941952,
40.1402777640512));
#169727=CARTESIAN_POINT('Ctrl Pts',(-42.2082984896056,-46.690962167597,
40.1391317641987));
#169728=CARTESIAN_POINT('Ctrl Pts',(-42.2114915192564,-46.6862656177252,
40.1369830144753));
#169729=CARTESIAN_POINT('Ctrl Pts',(-42.2145638639316,-46.6815504704769,
40.134683756585));
#169730=CARTESIAN_POINT('Ctrl Pts',(-42.2175127112217,-46.6768256862944,
40.1322415082996));
#169731=CARTESIAN_POINT('Ctrl Pts',(-42.2278336767374,-46.6602889416557,
40.1236936393009));
#169732=CARTESIAN_POINT('Ctrl Pts',(-42.2366417962861,-46.6436341412465,
40.113394140767));
#169733=CARTESIAN_POINT('Ctrl Pts',(-42.2438165047411,-46.6272454828772,
40.101665321223));
#169734=CARTESIAN_POINT('Ctrl Pts',(-42.2474038589686,-46.6190511536926,
40.095800911451));
#169735=CARTESIAN_POINT('Ctrl Pts',(-42.2505828610986,-46.6109233607689,
40.0895791707949));
#169736=CARTESIAN_POINT('Ctrl Pts',(-42.2533384464727,-46.6029101354044,
40.0830403822907));
#169737=CARTESIAN_POINT('Ctrl Pts',(-42.2547162391598,-46.5989035227222,
40.0797709880385));
#169738=CARTESIAN_POINT('Ctrl Pts',(-42.2559881777373,-46.5949255520163,
40.0764223317514));
#169739=CARTESIAN_POINT('Ctrl Pts',(-42.2571523794831,-46.590982227591,
40.0729994484778));
#169740=CARTESIAN_POINT('Ctrl Pts',(-42.2583165812288,-46.5870389031656,
40.0695765652042));
#169741=CARTESIAN_POINT('Ctrl Pts',(-42.2593729236706,-46.5831302673241,
40.0660793733488));
#169742=CARTESIAN_POINT('Ctrl Pts',(-42.2603197753209,-46.5792622391317,
40.0625130768817));
#169743=CARTESIAN_POINT('Ctrl Pts',(-42.2603278499825,-46.5792292529522,
40.0624826638418));
#169744=CARTESIAN_POINT('Ctrl Pts',(-42.2603359167438,-46.5791962698504,
40.0624522459912));
#169745=CARTESIAN_POINT('Ctrl Pts',(-42.2603439756043,-46.5791632898296,
40.0624218233329));
#169746=CARTESIAN_POINT('Ctrl Pts',(-42.2644597533373,-46.5623199117001,
40.0468845275892));
#169747=CARTESIAN_POINT('Ctrl Pts',(-42.2666468343722,-46.5462756748365,
40.0302263329223));
#169748=CARTESIAN_POINT('Ctrl Pts',(-42.2670764855933,-46.5311346778787,
40.0127515884721));
#169749=CARTESIAN_POINT('Ctrl Pts',(-42.2675206673335,-46.5154816224575,
39.9946858597679));
#169750=CARTESIAN_POINT('Ctrl Pts',(-42.2660861658585,-46.5007931180901,
39.9757460620439));
#169751=CARTESIAN_POINT('Ctrl Pts',(-42.2629150644368,-46.4872066207025,
39.9562444559062));
#169752=CARTESIAN_POINT('Ctrl Pts',(-42.2598042840369,-46.4738785670839,
39.9371138113525));
#169753=CARTESIAN_POINT('Ctrl Pts',(-42.2550216427124,-46.4616103837176,
39.9174410654245));
#169754=CARTESIAN_POINT('Ctrl Pts',(-42.2486653035375,-46.4505634198058,
39.8975196504016));
#169755=CARTESIAN_POINT('Ctrl Pts',(-42.2444544516793,-46.4432451935069,
39.8843224113688));
#169756=CARTESIAN_POINT('Ctrl Pts',(-42.2395522518995,-46.4364635650945,
39.8710160447088));
#169757=CARTESIAN_POINT('Ctrl Pts',(-42.2339804752703,-46.4302753505423,
39.8576902534424));
#169758=CARTESIAN_POINT('',(-41.9955727382253,-46.165492069761,39.2875012672119));
#169759=CARTESIAN_POINT('',(-42.2339804752703,-46.4302753505423,39.8576902534424));
#169760=CARTESIAN_POINT('',(-46.1654920697614,-41.9955727382249,39.2875012672119));
#169761=CARTESIAN_POINT('Origin',(5.53234440788222E-15,0.,39.2875012672119));
#169762=CARTESIAN_POINT('',(-46.4302753505427,-42.2339804752699,39.8576902534424));
#169763=CARTESIAN_POINT('',(-46.1654920697614,-41.9955727382249,39.2875012672119));
#169764=CARTESIAN_POINT('',(-46.7738319284259,-42.1358900227692,40.1599502534424));
#169765=CARTESIAN_POINT('Ctrl Pts',(-46.4302753505427,-42.2339804752699,
39.8576902534424));
#169766=CARTESIAN_POINT('Ctrl Pts',(-46.4394205306938,-42.2422146548471,
39.8773836120379));
#169767=CARTESIAN_POINT('Ctrl Pts',(-46.4498406831885,-42.2489725007703,
39.8969946442163));
#169768=CARTESIAN_POINT('Ctrl Pts',(-46.4613553898164,-42.2541979548149,
39.9162525288286));
#169769=CARTESIAN_POINT('Ctrl Pts',(-46.4731014717862,-42.2595284086007,
39.9358973794123));
#169770=CARTESIAN_POINT('Ctrl Pts',(-46.4859871977651,-42.2632649224146,
39.9551762199814));
#169771=CARTESIAN_POINT('Ctrl Pts',(-46.499862931965,-42.2653147554874,
39.9738152034329));
#169772=CARTESIAN_POINT('Ctrl Pts',(-46.5131996064699,-42.2672849544035,
39.9917300792741));
#169773=CARTESIAN_POINT('Ctrl Pts',(-46.5274517041996,-42.2676972410238,
40.0090551158227));
#169774=CARTESIAN_POINT('Ctrl Pts',(-46.5425130602562,-42.2664327220881,
40.0255394551647));
#169775=CARTESIAN_POINT('Ctrl Pts',(-46.5540826713329,-42.2654613625219,
40.0382021526222));
#169776=CARTESIAN_POINT('Ctrl Pts',(-46.5661304069589,-42.263499903613,
40.0503687782157));
#169777=CARTESIAN_POINT('Ctrl Pts',(-46.5786151613303,-42.2604772948658,
40.0619155352442));
#169778=CARTESIAN_POINT('Ctrl Pts',(-46.578647881645,-42.2604693731473,
40.0619457972352));
#169779=CARTESIAN_POINT('Ctrl Pts',(-46.5786806053975,-42.260461443425,
40.0619760547305));
#169780=CARTESIAN_POINT('Ctrl Pts',(-46.5787133325846,-42.2604535056995,
40.062006307727));
#169781=CARTESIAN_POINT('Ctrl Pts',(-46.5822223525748,-42.259602420106,
40.06525004417));
#169782=CARTESIAN_POINT('Ctrl Pts',(-46.5857690348148,-42.2586587894012,
40.0684393223556));
#169783=CARTESIAN_POINT('Ctrl Pts',(-46.5893485909042,-42.2576238078913,
40.0715697951759));
#169784=CARTESIAN_POINT('Ctrl Pts',(-46.609268006654,-42.2518643711135,
40.0889901646411));
#169785=CARTESIAN_POINT('Ctrl Pts',(-46.6302067610331,-42.243280888175,
40.1045963098226));
#169786=CARTESIAN_POINT('Ctrl Pts',(-46.6513153841062,-42.2321288152531,
40.1176634650704));
#169787=CARTESIAN_POINT('Ctrl Pts',(-46.6607892264623,-42.2271236104873,
40.123528185305));
#169788=CARTESIAN_POINT('Ctrl Pts',(-46.6702976120509,-42.2216011621505,
40.1288820140914));
#169789=CARTESIAN_POINT('Ctrl Pts',(-46.6797659870608,-42.2155846760827,
40.1336621774101));
#169790=CARTESIAN_POINT('Ctrl Pts',(-46.6838808147709,-42.2129699926167,
40.1357395717319));
#169791=CARTESIAN_POINT('Ctrl Pts',(-46.6879878819276,-42.2102619919288,
40.1377083672884));
#169792=CARTESIAN_POINT('Ctrl Pts',(-46.692080938468,-42.2074625774076,
40.1395632548792));
#169793=CARTESIAN_POINT('Ctrl Pts',(-46.7064066363596,-42.1976646265836,
40.146055361447));
#169794=CARTESIAN_POINT('Ctrl Pts',(-46.7205607018097,-42.1867468541395,
40.151152097463));
#169795=CARTESIAN_POINT('Ctrl Pts',(-46.7342751765575,-42.1747908797555,
40.1546258197409));
#169796=CARTESIAN_POINT('Ctrl Pts',(-46.7411324139314,-42.1688128925635,
40.1563626808798));
#169797=CARTESIAN_POINT('Ctrl Pts',(-46.74787975408,-42.1625753552952,40.1576937882008));
#169798=CARTESIAN_POINT('Ctrl Pts',(-46.7544837081025,-42.1560884757155,
40.1585906813668));
#169799=CARTESIAN_POINT('Ctrl Pts',(-46.7577856851138,-42.1528450359257,
40.1590391279498));
#169800=CARTESIAN_POINT('Ctrl Pts',(-46.7610518156851,-42.1495392606404,
40.1593790209175));
#169801=CARTESIAN_POINT('Ctrl Pts',(-46.7642779142249,-42.1461724262971,
40.1596068022931));
#169802=CARTESIAN_POINT('Ctrl Pts',(-46.7675040127646,-42.1428055919538,
40.1598345836687));
#169803=CARTESIAN_POINT('Ctrl Pts',(-46.770690078005,-42.1393776974106,
40.1599502506865));
#169804=CARTESIAN_POINT('Ctrl Pts',(-46.773831928426,-42.1358900227693,
40.1599502534424));
#169805=CARTESIAN_POINT('',(-46.7942619810919,-42.1132001505999,40.1599502534424));
#169806=CARTESIAN_POINT('Origin',(7.58094983678529E-17,1.03991361176644E-16,
40.1599502534424));
#169807=CARTESIAN_POINT('',(-46.8559036426987,-41.761272367336,39.8576902534424));
#169808=CARTESIAN_POINT('Ctrl Pts',(-46.7942619810919,-42.1132001505999,
40.1599502534424));
#169809=CARTESIAN_POINT('Ctrl Pts',(-46.7968184499054,-42.1103595112869,
40.1599502447858));
#169810=CARTESIAN_POINT('Ctrl Pts',(-46.7993324362835,-42.1074947242965,
40.1598744685927));
#169811=CARTESIAN_POINT('Ctrl Pts',(-46.8018034833199,-42.1046079742812,
40.1597246934279));
#169812=CARTESIAN_POINT('Ctrl Pts',(-46.8160830868189,-42.0879261203894,
40.1588591777436));
#169813=CARTESIAN_POINT('Ctrl Pts',(-46.8289319920994,-42.0705099543564,
40.1555254706033));
#169814=CARTESIAN_POINT('Ctrl Pts',(-46.8402566831411,-42.0527856759149,
40.150063182641));
#169815=CARTESIAN_POINT('Ctrl Pts',(-46.8448241915534,-42.0456370666869,
40.1478601162504));
#169816=CARTESIAN_POINT('Ctrl Pts',(-46.8491442126956,-42.0384382358192,
40.1453112228319));
#169817=CARTESIAN_POINT('Ctrl Pts',(-46.8532123574521,-42.0312165334048,
40.1424401896328));
#169818=CARTESIAN_POINT('Ctrl Pts',(-46.8547132558792,-42.0285521636631,
40.1413809526905));
#169819=CARTESIAN_POINT('Ctrl Pts',(-46.8561797434811,-42.0258847247793,
40.1402777640511));
#169820=CARTESIAN_POINT('Ctrl Pts',(-46.8576115380195,-42.0232156132259,
40.1391317641987));
#169821=CARTESIAN_POINT('Ctrl Pts',(-46.860296152779,-42.0182110290632,
40.1369830144753));
#169822=CARTESIAN_POINT('Ctrl Pts',(-46.8628587997326,-42.0132005644173,
40.1346837565849));
#169823=CARTESIAN_POINT('Ctrl Pts',(-46.8652976184989,-42.0081934246213,
40.1322415082996));
#169824=CARTESIAN_POINT('Ctrl Pts',(-46.8738334841811,-41.9906684353352,
40.1236936393008));
#169825=CARTESIAN_POINT('Ctrl Pts',(-46.8808524512365,-41.9731841724646,
40.113394140767));
#169826=CARTESIAN_POINT('Ctrl Pts',(-46.8862747746135,-41.9561353316315,
40.101665321223));
#169827=CARTESIAN_POINT('Ctrl Pts',(-46.888985936302,-41.9476109112149,
40.095800911451));
#169828=CARTESIAN_POINT('Ctrl Pts',(-46.8912979378216,-41.9391953469839,
40.0895791707949));
#169829=CARTESIAN_POINT('Ctrl Pts',(-46.8932008176776,-41.9309379818018,
40.0830403822906));
#169830=CARTESIAN_POINT('Ctrl Pts',(-46.8941522576055,-41.9268092992108,
40.0797709880385));
#169831=CARTESIAN_POINT('Ctrl Pts',(-46.8950014172056,-41.9227201664598,
40.0764223317514));
#169832=CARTESIAN_POINT('Ctrl Pts',(-46.8957470516901,-41.9186767517589,
40.0729994484778));
#169833=CARTESIAN_POINT('Ctrl Pts',(-46.8964926861745,-41.9146333370579,
40.0695765652042));
#169834=CARTESIAN_POINT('Ctrl Pts',(-46.8971346781638,-41.9106356952803,
40.0660793733488));
#169835=CARTESIAN_POINT('Ctrl Pts',(-46.8976720238189,-41.9066898836032,
40.0625130768817));
#169836=CARTESIAN_POINT('Ctrl Pts',(-46.897676606252,-41.9066562340934,
40.0624826638418));
#169837=CARTESIAN_POINT('Ctrl Pts',(-46.8976811811498,-41.9066225884704,
40.0624522459912));
#169838=CARTESIAN_POINT('Ctrl Pts',(-46.8976857485122,-41.9065889467373,
40.0624218233329));
#169839=CARTESIAN_POINT('Ctrl Pts',(-46.9000183671518,-41.8894076224754,
40.0468845275905));
#169840=CARTESIAN_POINT('Ctrl Pts',(-46.9005163877045,-41.8732226654017,
40.0302263329251));
#169841=CARTESIAN_POINT('Ctrl Pts',(-46.8993610201074,-41.8581197016285,
40.0127515884765));
#169842=CARTESIAN_POINT('Ctrl Pts',(-46.8981665787455,-41.8425059656494,
39.9946858597745));
#169843=CARTESIAN_POINT('Ctrl Pts',(-46.8952045688313,-41.8280478726817,
39.9757460620529));
#169844=CARTESIAN_POINT('Ctrl Pts',(-46.8906306633432,-41.8148672739078,
39.9562444559176));
#169845=CARTESIAN_POINT('Ctrl Pts',(-46.886143763162,-41.8019373978574,
39.9371138113668));
#169846=CARTESIAN_POINT('Ctrl Pts',(-46.8801049472944,-41.7902363430322,
39.9174410654419));
#169847=CARTESIAN_POINT('Ctrl Pts',(-46.872628706651,-41.7799143139112,
39.897519650422));
#169848=CARTESIAN_POINT('Ctrl Pts',(-46.8676759593291,-41.7730763314914,
39.8843224113824));
#169849=CARTESIAN_POINT('Ctrl Pts',(-46.8620917411135,-41.7668442729553,
39.8710160447157));
#169850=CARTESIAN_POINT('Ctrl Pts',(-46.8559036426987,-41.761272367336,
39.8576902534424));
#169851=CARTESIAN_POINT('',(-46.5911245387432,-41.522859991456,39.2875012672119));
#169852=CARTESIAN_POINT('',(-46.8559036426987,-41.761272367336,39.8576902534424));
#169853=CARTESIAN_POINT('',(-50.3023253561997,-36.9399086546484,39.2875012672119));
#169854=CARTESIAN_POINT('Origin',(5.53234440788222E-15,0.,39.2875012672119));
#169855=CARTESIAN_POINT('',(-50.5905785208486,-37.1493329797258,39.8576902534424));
#169856=CARTESIAN_POINT('',(-50.3023253561997,-36.9399086546484,39.2875012672119));
#169857=CARTESIAN_POINT('',(-50.9219998155902,-37.0158684358557,40.1599502534424));
#169858=CARTESIAN_POINT('Ctrl Pts',(-50.5905785208486,-37.1493329797258,
39.8576902534424));
#169859=CARTESIAN_POINT('Ctrl Pts',(-50.6005343088827,-37.1565661199776,
39.8773836120365));
#169860=CARTESIAN_POINT('Ctrl Pts',(-50.6116037659404,-37.1621977431861,
39.8969946442134));
#169861=CARTESIAN_POINT('Ctrl Pts',(-50.6236016024807,-37.1661909570579,
39.9162525288243));
#169862=CARTESIAN_POINT('Ctrl Pts',(-50.6358405223261,-37.1702644101623,
39.9358973794066));
#169863=CARTESIAN_POINT('Ctrl Pts',(-50.6490462309955,-37.1726335298281,
39.9551762199742));
#169864=CARTESIAN_POINT('Ctrl Pts',(-50.6630602183712,-37.1732217245287,
39.9738152034244));
#169865=CARTESIAN_POINT('Ctrl Pts',(-50.6765297750414,-37.1737870683984,
39.9917300792642));
#169866=CARTESIAN_POINT('Ctrl Pts',(-50.6907468939737,-37.1727073465962,
40.0090551158116));
#169867=CARTESIAN_POINT('Ctrl Pts',(-50.7055935641233,-37.1698754144254,
40.0255394551526));
#169868=CARTESIAN_POINT('Ctrl Pts',(-50.7169982609406,-37.1677000224021,
40.0382021526144));
#169869=CARTESIAN_POINT('Ctrl Pts',(-50.7287749695284,-37.1644899772788,
40.0503687782121));
#169870=CARTESIAN_POINT('Ctrl Pts',(-50.7408753824655,-37.1601789145085,
40.0619155352442));
#169871=CARTESIAN_POINT('Ctrl Pts',(-50.7409070954898,-37.1601676159818,
40.0619457972351));
#169872=CARTESIAN_POINT('Ctrl Pts',(-50.7409388110965,-37.1601563091358,
40.0619760547305));
#169873=CARTESIAN_POINT('Ctrl Pts',(-50.7409705292823,-37.1601449939714,
40.0620063077269));
#169874=CARTESIAN_POINT('Ctrl Pts',(-50.7443713638247,-37.1589317782467,
40.06525004417));
#169875=CARTESIAN_POINT('Ctrl Pts',(-50.7477999807009,-37.1576225876054,
40.0684393223556));
#169876=CARTESIAN_POINT('Ctrl Pts',(-50.7512517425808,-37.1562191103353,
40.0715697951759));
#169877=CARTESIAN_POINT('Ctrl Pts',(-50.7704600126119,-37.148409078437,
40.0889901646418));
#169878=CARTESIAN_POINT('Ctrl Pts',(-50.7903868440233,-37.1376839208976,
40.1045963098238));
#169879=CARTESIAN_POINT('Ctrl Pts',(-50.8102141228066,-37.1243864882659,
40.1176634650719));
#169880=CARTESIAN_POINT('Ctrl Pts',(-50.8191128800998,-37.1184184163531,
40.1235281853059));
#169881=CARTESIAN_POINT('Ctrl Pts',(-50.8279919247184,-37.1119323236329,
40.1288820140919));
#169882=CARTESIAN_POINT('Ctrl Pts',(-50.8367795369357,-37.1049590818164,
40.1336621774102));
#169883=CARTESIAN_POINT('Ctrl Pts',(-50.8405985143444,-37.1019286052429,
40.135739571732));
#169884=CARTESIAN_POINT('Ctrl Pts',(-50.844400019407,-37.0988061338476,
40.1377083672884));
#169885=CARTESIAN_POINT('Ctrl Pts',(-50.8481780352575,-37.0955942139019,
40.1395632548792));
#169886=CARTESIAN_POINT('Ctrl Pts',(-50.8614010907343,-37.0843524940918,
40.146055361447));
#169887=CARTESIAN_POINT('Ctrl Pts',(-50.874336400757,-37.072015027637,40.151152097463));
#169888=CARTESIAN_POINT('Ctrl Pts',(-50.8867260065479,-37.0586909963618,
40.1546258197409));
#169889=CARTESIAN_POINT('Ctrl Pts',(-50.8929208094434,-37.0520289807242,
40.1563626808798));
#169890=CARTESIAN_POINT('Ctrl Pts',(-50.8989791867715,-37.0451203242408,
40.1576937882008));
#169891=CARTESIAN_POINT('Ctrl Pts',(-50.904868900089,-37.0379786793007,
40.1585906813668));
#169892=CARTESIAN_POINT('Ctrl Pts',(-50.9078137567478,-37.0344078568306,
40.1590391279498));
#169893=CARTESIAN_POINT('Ctrl Pts',(-50.9107164475036,-37.0307787873188,
40.1593790209175));
#169894=CARTESIAN_POINT('Ctrl Pts',(-50.913572943118,-37.0270931777236,
40.1596068022931));
#169895=CARTESIAN_POINT('Ctrl Pts',(-50.9164294387324,-37.0234075681284,
40.1598345836687));
#169896=CARTESIAN_POINT('Ctrl Pts',(-50.9192397378252,-37.0196654174467,
40.1599502506864));
#169897=CARTESIAN_POINT('Ctrl Pts',(-50.9219998155902,-37.0158684358557,
40.1599502534424));
#169898=CARTESIAN_POINT('',(-50.9399462128204,-36.9911673391705,40.1599502534424));
#169899=CARTESIAN_POINT('Origin',(8.60468667414046E-17,9.13492640817417E-17,
40.1599502534424));
#169900=CARTESIAN_POINT('',(-50.9644637245895,-36.6347241449652,39.8576902534424));
#169901=CARTESIAN_POINT('Ctrl Pts',(-50.9399462128204,-36.9911673391705,
40.1599502534424));
#169902=CARTESIAN_POINT('Ctrl Pts',(-50.9421917493682,-36.9880750374205,
40.1599502447858));
#169903=CARTESIAN_POINT('Ctrl Pts',(-50.9443925120841,-36.9849631609002,
40.1598744685927));
#169904=CARTESIAN_POINT('Ctrl Pts',(-50.9465482749233,-36.9818339300541,
40.1597246934279));
#169905=CARTESIAN_POINT('Ctrl Pts',(-50.9590059247108,-36.9637508360902,
40.1588591777435));
#169906=CARTESIAN_POINT('Ctrl Pts',(-50.969963957274,-36.94508700131,40.1555254706021));
#169907=CARTESIAN_POINT('Ctrl Pts',(-50.9793739188864,-36.9262760657652,
40.1500631826381));
#169908=CARTESIAN_POINT('Ctrl Pts',(-50.9831691728707,-36.9186891827346,
40.1478601162481));
#169909=CARTESIAN_POINT('Ctrl Pts',(-50.9867130457555,-36.9110782226479,
40.1453112228307));
#169910=CARTESIAN_POINT('Ctrl Pts',(-50.9900040313323,-36.9034708445586,
40.1424401896328));
#169911=CARTESIAN_POINT('Ctrl Pts',(-50.991218205206,-36.900664183907,40.1413809526906));
#169912=CARTESIAN_POINT('Ctrl Pts',(-50.9923978359481,-36.8978580678371,
40.1402777640512));
#169913=CARTESIAN_POINT('Ctrl Pts',(-50.9935427888372,-36.8950539146732,
40.1391317641987));
#169914=CARTESIAN_POINT('Ctrl Pts',(-50.9956895755044,-36.8897961274909,
40.1369830144753));
#169915=CARTESIAN_POINT('Ctrl Pts',(-50.9977144478401,-36.8845452411467,
40.1346837565849));
#169916=CARTESIAN_POINT('Ctrl Pts',(-50.9996165178738,-36.8793106050085,
40.1322415082996));
#169917=CARTESIAN_POINT('Ctrl Pts',(-51.0062737629917,-36.860989378525,
40.1236936393008));
#169918=CARTESIAN_POINT('Ctrl Pts',(-51.011426676282,-36.8428672144357,
40.113394140767));
#169919=CARTESIAN_POINT('Ctrl Pts',(-51.0150372064714,-36.8253449818066,
40.101665321223));
#169920=CARTESIAN_POINT('Ctrl Pts',(-51.0168424715662,-36.816583865492,
40.095800911451));
#169921=CARTESIAN_POINT('Ctrl Pts',(-51.0182621417029,-36.8079727326365,
40.0895791707949));
#169922=CARTESIAN_POINT('Ctrl Pts',(-51.0192914676908,-36.7995616970578,
40.0830403822907));
#169923=CARTESIAN_POINT('Ctrl Pts',(-51.0198061306847,-36.7953561792684,
40.0797709880385));
#169924=CARTESIAN_POINT('Ctrl Pts',(-51.0202232077371,-36.7912006858664,
40.0764223317514));
#169925=CARTESIAN_POINT('Ctrl Pts',(-51.0205421056328,-36.7871014813874,
40.0729994484778));
#169926=CARTESIAN_POINT('Ctrl Pts',(-51.0208610035285,-36.7830022769085,
40.0695765652043));
#169927=CARTESIAN_POINT('Ctrl Pts',(-51.0210816112668,-36.7789594281948,
40.0660793733488));
#169928=CARTESIAN_POINT('Ctrl Pts',(-51.0212035636552,-36.7749790641713,
40.0625130768817));
#169929=CARTESIAN_POINT('Ctrl Pts',(-51.0212046036537,-36.7749451200024,
40.0624826638418));
#169930=CARTESIAN_POINT('Ctrl Pts',(-51.0212056365645,-36.7749111804865,
40.0624522459912));
#169931=CARTESIAN_POINT('Ctrl Pts',(-51.0212066623877,-36.774877245627,
40.0624218233329));
#169932=CARTESIAN_POINT('Ctrl Pts',(-51.0217305652762,-36.7575462174171,
40.0468845275921));
#169933=CARTESIAN_POINT('Ctrl Pts',(-51.0205340689296,-36.7413978659102,
40.0302263329286));
#169934=CARTESIAN_POINT('Ctrl Pts',(-51.0178063409637,-36.7264984065536,
40.012751588482));
#169935=CARTESIAN_POINT('Ctrl Pts',(-51.0149863630493,-36.7110950573751,
39.9946858597819));
#169936=CARTESIAN_POINT('Ctrl Pts',(-51.0105292970966,-36.697025781699,
39.9757460620623));
#169937=CARTESIAN_POINT('Ctrl Pts',(-51.0046027002077,-36.6843954909367,
39.9562444559292));
#169938=CARTESIAN_POINT('Ctrl Pts',(-50.9987888396623,-36.6720054548815,
39.9371138113801));
#169939=CARTESIAN_POINT('Ctrl Pts',(-50.9915600117817,-36.6609997278017,
39.917441065457));
#169940=CARTESIAN_POINT('Ctrl Pts',(-50.9830457809264,-36.6515157237815,
39.8975196504388));
#169941=CARTESIAN_POINT('Ctrl Pts',(-50.9774054014764,-36.6452329036082,
39.8843224113937));
#169942=CARTESIAN_POINT('Ctrl Pts',(-50.9712003466883,-36.6396186946867,
39.8710160447213));
#169943=CARTESIAN_POINT('Ctrl Pts',(-50.9644637245895,-36.6347241449652,
39.8576902534424));
#169944=CARTESIAN_POINT('',(-50.676214228995,-36.4252947698676,39.2875012672119));
#169945=CARTESIAN_POINT('',(-50.9644637245895,-36.6347241449652,39.8576902534424));
#169946=CARTESIAN_POINT('',(-53.8880358395972,-31.4795232016787,39.2875012672119));
#169947=CARTESIAN_POINT('Origin',(5.53234440788222E-15,0.,39.2875012672119));
#169948=CARTESIAN_POINT('',(-54.1966007261209,-31.6576696180581,39.8576902534424));
#169949=CARTESIAN_POINT('',(-53.8880358395972,-31.4795232016787,39.2875012672119));
#169950=CARTESIAN_POINT('',(-54.5122556166612,-31.4902932482905,40.1599502534424));
#169951=CARTESIAN_POINT('Ctrl Pts',(-54.1966007261209,-31.6576696180581,
39.8576902534424));
#169952=CARTESIAN_POINT('Ctrl Pts',(-54.2072580443417,-31.6638224711871,
39.8773836120366));
#169953=CARTESIAN_POINT('Ctrl Pts',(-54.2188555266751,-31.668266170439,
39.8969946442136));
#169954=CARTESIAN_POINT('Ctrl Pts',(-54.2312050423211,-31.6709833936512,
39.9162525288247));
#169955=CARTESIAN_POINT('Ctrl Pts',(-54.2438027078763,-31.6737552164699,
39.9358973794071));
#169956=CARTESIAN_POINT('Ctrl Pts',(-54.25718371473,-31.6747309854166,39.9551762199749));
#169957=CARTESIAN_POINT('Ctrl Pts',(-54.2711824151049,-31.6738510973604,
39.9738152034253));
#169958=CARTESIAN_POINT('Ctrl Pts',(-54.2846372786604,-31.6730053921575,
39.9917300792653));
#169959=CARTESIAN_POINT('Ctrl Pts',(-54.2986636530671,-31.6704454915902,
40.0090551158128));
#169960=CARTESIAN_POINT('Ctrl Pts',(-54.3131329740864,-31.6660771734245,
40.025539455154));
#169961=CARTESIAN_POINT('Ctrl Pts',(-54.3242478043957,-31.662721582994,
40.0382021526153));
#169962=CARTESIAN_POINT('Ctrl Pts',(-54.3356244578575,-31.6582981215829,
40.0503687782125));
#169963=CARTESIAN_POINT('Ctrl Pts',(-54.3472079546995,-31.6527458376965,
40.0619155352442));
#169964=CARTESIAN_POINT('Ctrl Pts',(-54.347238312979,-31.6527312861506,
40.0619457972351));
#169965=CARTESIAN_POINT('Ctrl Pts',(-54.347268672957,-31.6527167260611,
40.0619760547305));
#169966=CARTESIAN_POINT('Ctrl Pts',(-54.3472990346306,-31.6527021574291,
40.0620063077269));
#169967=CARTESIAN_POINT('Ctrl Pts',(-54.3505544234702,-31.6511401038185,
40.06525004417));
#169968=CARTESIAN_POINT('Ctrl Pts',(-54.3538274103385,-31.6494796970074,
40.0684393223557));
#169969=CARTESIAN_POINT('Ctrl Pts',(-54.3571135597834,-31.6477231007677,
40.0715697951759));
#169970=CARTESIAN_POINT('Ctrl Pts',(-54.3754002342689,-31.6379480420931,
40.0889901646415));
#169971=CARTESIAN_POINT('Ctrl Pts',(-54.3940968201766,-31.6251987170239,
40.1045963098233));
#169972=CARTESIAN_POINT('Ctrl Pts',(-54.4124255228535,-31.6099016141378,
40.1176634650713));
#169973=CARTESIAN_POINT('Ctrl Pts',(-54.4206516984377,-31.6030360625224,
40.1235281853055));
#169974=CARTESIAN_POINT('Ctrl Pts',(-54.4288041214164,-31.5956573884072,
40.1288820140917));
#169975=CARTESIAN_POINT('Ctrl Pts',(-54.4368146919238,-31.5878037911379,
40.1336621774101));
#169976=CARTESIAN_POINT('Ctrl Pts',(-54.4402959775154,-31.5843907239923,
40.1357395717319));
#169977=CARTESIAN_POINT('Ctrl Pts',(-54.443750270399,-31.5808879923398,
40.1377083672884));
#169978=CARTESIAN_POINT('Ctrl Pts',(-54.4471718528273,-31.5772987574365,
40.1395632548792));
#169979=CARTESIAN_POINT('Ctrl Pts',(-54.4591473913264,-31.5647364352751,
40.146055361447));
#169980=CARTESIAN_POINT('Ctrl Pts',(-54.4707222239582,-31.5511144466739,
40.151152097463));
#169981=CARTESIAN_POINT('Ctrl Pts',(-54.4816512176786,-31.5365683393823,
40.1546258197409));
#169982=CARTESIAN_POINT('Ctrl Pts',(-54.4871157145388,-31.5292952857365,
40.1563626808798));
#169983=CARTESIAN_POINT('Ctrl Pts',(-54.4924187521965,-31.5217912027242,
40.1576937882008));
#169984=CARTESIAN_POINT('Ctrl Pts',(-54.4975296958774,-31.5140730377801,
40.1585906813668));
#169985=CARTESIAN_POINT('Ctrl Pts',(-54.5000851677179,-31.5102139553081,
40.1590391279498));
#169986=CARTESIAN_POINT('Ctrl Pts',(-54.5025926161709,-31.5063013524147,
40.1593790209175));
#169987=CARTESIAN_POINT('Ctrl Pts',(-54.5050482124962,-31.5023373478776,
40.1596068022931));
#169988=CARTESIAN_POINT('Ctrl Pts',(-54.5075038088216,-31.4983733433406,
40.1598345836687));
#169989=CARTESIAN_POINT('Ctrl Pts',(-54.5099075515418,-31.4943579363063,
40.1599502506865));
#169990=CARTESIAN_POINT('Ctrl Pts',(-54.5122556166612,-31.4902932482905,
40.1599502534424));
#169991=CARTESIAN_POINT('',(-54.5275217339721,-31.4638515574737,40.1599502534424));
#169992=CARTESIAN_POINT('Origin',(9.49066947580433E-17,7.77063253334978E-17,
40.1599502534424));
#169993=CARTESIAN_POINT('',(-54.514646476914,-31.1067982185532,39.8576902534424));
#169994=CARTESIAN_POINT('Ctrl Pts',(-54.5275217339721,-31.4638515574737,
40.1599502534424));
#169995=CARTESIAN_POINT('Ctrl Pts',(-54.5294317356859,-31.4605414731917,
40.1599502447858));
#169996=CARTESIAN_POINT('Ctrl Pts',(-54.5312951627229,-31.4572166015119,
40.1598744685927));
#169997=CARTESIAN_POINT('Ctrl Pts',(-54.5331120223761,-31.453879174343,
40.1597246934279));
#169998=CARTESIAN_POINT('Ctrl Pts',(-54.5436112298343,-31.4345929624664,
40.1588591777432));
#169999=CARTESIAN_POINT('Ctrl Pts',(-54.5525583311825,-31.414885943816,
40.1555254706002));
#170000=CARTESIAN_POINT('Ctrl Pts',(-54.5599504658566,-31.3951944477122,
40.1500631826335));
#170001=CARTESIAN_POINT('Ctrl Pts',(-54.5629318838159,-31.3872524143595,
40.1478601162446));
#170002=CARTESIAN_POINT('Ctrl Pts',(-54.5656607810303,-31.3793127123272,
40.1453112228287));
#170003=CARTESIAN_POINT('Ctrl Pts',(-54.5681385507009,-31.3714030065916,
40.1424401896328));
#170004=CARTESIAN_POINT('Ctrl Pts',(-54.5690526972783,-31.3684848053916,
40.1413809526906));
#170005=CARTESIAN_POINT('Ctrl Pts',(-54.5699325468791,-31.3655707565304,
40.1402777640511));
#170006=CARTESIAN_POINT('Ctrl Pts',(-54.5707781137755,-31.3626622846449,
40.1391317641987));
#170007=CARTESIAN_POINT('Ctrl Pts',(-54.5723635517064,-31.3572088998597,
40.1369830144753));
#170008=CARTESIAN_POINT('Ctrl Pts',(-54.5738284644993,-31.3517751216267,
40.134683756585));
#170009=CARTESIAN_POINT('Ctrl Pts',(-54.575172946323,-31.3463703409153,
40.1322415082996));
#170010=CARTESIAN_POINT('Ctrl Pts',(-54.5798786327061,-31.3274536084257,
40.1236936393009));
#170011=CARTESIAN_POINT('Ctrl Pts',(-54.5831090358349,-31.3088920933399,
40.113394140767));
#170012=CARTESIAN_POINT('Ctrl Pts',(-54.5848682151124,-31.2910884461622,
40.101665321223));
#170013=CARTESIAN_POINT('Ctrl Pts',(-54.5857478047512,-31.2821866225733,
40.095800911451));
#170014=CARTESIAN_POINT('Ctrl Pts',(-54.5862595893019,-31.2734742664669,
40.0895791707949));
#170015=CARTESIAN_POINT('Ctrl Pts',(-54.5864040839109,-31.2650017135574,
40.0830403822906));
#170016=CARTESIAN_POINT('Ctrl Pts',(-54.5864763312153,-31.2607654371026,
40.0797709880385));
#170017=CARTESIAN_POINT('Ctrl Pts',(-54.5864567561365,-31.256589111505,
40.0764223317514));
#170018=CARTESIAN_POINT('Ctrl Pts',(-54.5863454235314,-31.25247902899,40.0729994484778));
#170019=CARTESIAN_POINT('Ctrl Pts',(-54.5862340909262,-31.2483689464751,
40.0695765652042));
#170020=CARTESIAN_POINT('Ctrl Pts',(-54.586030897389,-31.2443251851218,
40.0660793733488));
#170021=CARTESIAN_POINT('Ctrl Pts',(-54.5857361203749,-31.2403538784532,
40.0625130768817));
#170022=CARTESIAN_POINT('Ctrl Pts',(-54.5857336065443,-31.2403200115245,
40.0624826638418));
#170023=CARTESIAN_POINT('Ctrl Pts',(-54.5857310861513,-31.2402861499643,
40.0624522459912));
#170024=CARTESIAN_POINT('Ctrl Pts',(-54.5857285591962,-31.2402522937758,
40.0624218233329));
#170025=CARTESIAN_POINT('Ctrl Pts',(-54.5844380063442,-31.2229614439868,
40.0468845275911));
#170026=CARTESIAN_POINT('Ctrl Pts',(-54.5815601021621,-31.2070266227626,
40.0302263329264));
#170027=CARTESIAN_POINT('Ctrl Pts',(-54.5772898993848,-31.1924939094151,
40.0127515884786));
#170028=CARTESIAN_POINT('Ctrl Pts',(-54.5728752811851,-31.177469709352,
39.9946858597769));
#170029=CARTESIAN_POINT('Ctrl Pts',(-54.5669719917396,-31.1639433968941,
39.9757460620557));
#170030=CARTESIAN_POINT('Ctrl Pts',(-54.5597576364835,-31.1520017942509,
39.9562444559208));
#170031=CARTESIAN_POINT('Ctrl Pts',(-54.5526805134449,-31.1402873460175,
39.9371138113699));
#170032=CARTESIAN_POINT('Ctrl Pts',(-54.5443408740998,-31.1300975277315,
39.917441065445));
#170033=CARTESIAN_POINT('Ctrl Pts',(-54.5348819367248,-31.1215554575449,
39.897519650425));
#170034=CARTESIAN_POINT('Ctrl Pts',(-54.5286157223278,-31.1158966355165,
39.8843224113845));
#170035=CARTESIAN_POINT('Ctrl Pts',(-54.5218578148503,-31.1109617866623,
39.8710160447167));
#170036=CARTESIAN_POINT('Ctrl Pts',(-54.514646476914,-31.1067982185532,
39.8576902534424));
#170037=CARTESIAN_POINT('',(-54.2060847114743,-30.9286463962975,39.2875012672119));
#170038=CARTESIAN_POINT('',(-54.514646476914,-31.1067982185532,39.8576902534424));
#170039=CARTESIAN_POINT('',(-56.8833377255396,-25.6742415049977,39.2875012672119));
#170040=CARTESIAN_POINT('Origin',(5.53234440788222E-15,0.,39.2875012672119));
#170041=CARTESIAN_POINT('',(-57.20883363247,-25.8191582032617,39.8576902534424));
#170042=CARTESIAN_POINT('',(-56.8833377255396,-25.6742415049977,39.2875012672119));
#170043=CARTESIAN_POINT('',(-57.5052637377733,-25.6197038181295,40.1599502534424));
#170044=CARTESIAN_POINT('Ctrl Pts',(-57.20883363247,-25.8191582032617,39.8576902534424));
#170045=CARTESIAN_POINT('Ctrl Pts',(-57.2200757170687,-25.8241633573214,
39.8773836120366));
#170046=CARTESIAN_POINT('Ctrl Pts',(-57.2320741602344,-25.8273704465178,
39.8969946442136));
#170047=CARTESIAN_POINT('Ctrl Pts',(-57.2446400511083,-25.8287819086044,
39.9162525288247));
#170048=CARTESIAN_POINT('Ctrl Pts',(-57.2574584397132,-25.8302217324664,
39.9358973794071));
#170049=CARTESIAN_POINT('Ctrl Pts',(-57.2708681396398,-25.8297934599654,
39.9551762199749));
#170050=CARTESIAN_POINT('Ctrl Pts',(-57.284698180323,-25.82745512939,39.9738152034254));
#170051=CARTESIAN_POINT('Ctrl Pts',(-57.2979909364631,-25.8252076408377,
39.9917300792656));
#170052=CARTESIAN_POINT('Ctrl Pts',(-57.311672890451,-25.8211956083115,
40.0090551158133));
#170053=CARTESIAN_POINT('Ctrl Pts',(-57.325606333431,-25.815338764359,40.0255394551547));
#170054=CARTESIAN_POINT('Ctrl Pts',(-57.3363095208257,-25.8108397400723,
40.0382021526157));
#170055=CARTESIAN_POINT('Ctrl Pts',(-57.3471614741657,-25.8052513267422,
40.0503687782127));
#170056=CARTESIAN_POINT('Ctrl Pts',(-57.3581011436975,-25.7985186537238,
40.0619155352442));
#170057=CARTESIAN_POINT('Ctrl Pts',(-57.3581298146204,-25.7985010085885,
40.0619457972351));
#170058=CARTESIAN_POINT('Ctrl Pts',(-57.3581584863395,-25.7984833547788,
40.0619760547305));
#170059=CARTESIAN_POINT('Ctrl Pts',(-57.358187158852,-25.7984656922963,
40.0620063077269));
#170060=CARTESIAN_POINT('Ctrl Pts',(-57.3612614352675,-25.796571914986,
40.06525004417));
#170061=CARTESIAN_POINT('Ctrl Pts',(-57.3643429325988,-25.7945784837695,
40.0684393223557));
#170062=CARTESIAN_POINT('Ctrl Pts',(-57.3674274658677,-25.7924880141963,
40.0715697951759));
#170063=CARTESIAN_POINT('Ctrl Pts',(-57.3845921921726,-25.7808550263355,
40.0889901646387));
#170064=CARTESIAN_POINT('Ctrl Pts',(-57.4018536888665,-25.7662212180126,
40.1045963098182));
#170065=CARTESIAN_POINT('Ctrl Pts',(-57.4184830023326,-25.7490920431358,
40.1176634650649));
#170066=CARTESIAN_POINT('Ctrl Pts',(-57.4259464685093,-25.7414042322357,
40.1235281853016));
#170067=CARTESIAN_POINT('Ctrl Pts',(-57.4332829501985,-25.7332138190206,
40.1288820140899));
#170068=CARTESIAN_POINT('Ctrl Pts',(-57.4404287135113,-25.7245659119508,
40.1336621774101));
#170069=CARTESIAN_POINT('Ctrl Pts',(-57.4435341655924,-25.720807648511,
40.1357395717319));
#170070=CARTESIAN_POINT('Ctrl Pts',(-57.4466034003413,-25.7169630332622,
40.1377083672884));
#170071=CARTESIAN_POINT('Ctrl Pts',(-57.4496310617744,-25.7130358078101,
40.1395632548792));
#170072=CARTESIAN_POINT('Ctrl Pts',(-57.46022787679,-25.6992905187278,40.146055361447));
#170073=CARTESIAN_POINT('Ctrl Pts',(-57.4703154157424,-25.6845332533378,
40.151152097463));
#170074=CARTESIAN_POINT('Ctrl Pts',(-57.4796640570499,-25.6689244402253,
40.1546258197409));
#170075=CARTESIAN_POINT('Ctrl Pts',(-57.4843383777036,-25.661120033669,
40.1563626808798));
#170076=CARTESIAN_POINT('Ctrl Pts',(-57.4888279745007,-25.6531027404317,
40.1576937882008));
#170077=CARTESIAN_POINT('Ctrl Pts',(-57.4931041519765,-25.6448926173139,
40.1585906813668));
#170078=CARTESIAN_POINT('Ctrl Pts',(-57.4952422407144,-25.6407875557551,
40.1590391279498));
#170079=CARTESIAN_POINT('Ctrl Pts',(-57.4973269747346,-25.6366342867762,
40.1593790209175));
#170080=CARTESIAN_POINT('Ctrl Pts',(-57.4993547677437,-25.6324353177604,
40.1596068022931));
#170081=CARTESIAN_POINT('Ctrl Pts',(-57.5013825607528,-25.6282363487447,
40.1598345836687));
#170082=CARTESIAN_POINT('Ctrl Pts',(-57.5033534111923,-25.6239916789977,
40.1599502506865));
#170083=CARTESIAN_POINT('Ctrl Pts',(-57.5052637377733,-25.6197038181295,
40.1599502534424));
#170084=CARTESIAN_POINT('',(-57.517682316389,-25.5918112338791,40.1599502534424));
#170085=CARTESIAN_POINT('Origin',(1.02291912287982E-16,6.3212019823805E-17,
40.1599502534424));
#170086=CARTESIAN_POINT('',(-57.4675553545142,-25.2380597013427,39.8576902534424));
#170087=CARTESIAN_POINT('Ctrl Pts',(-57.517682316389,-25.5918112338791,
40.1599502534424));
#170088=CARTESIAN_POINT('Ctrl Pts',(-57.5192358568902,-25.5883196330411,
40.1599502447858));
#170089=CARTESIAN_POINT('Ctrl Pts',(-57.5207415321516,-25.5848181941916,
40.1598744685927));
#170090=CARTESIAN_POINT('Ctrl Pts',(-57.5221995827244,-25.5813091362505,
40.1597246934279));
#170091=CARTESIAN_POINT('Ctrl Pts',(-57.5306253163328,-25.5610311102466,
40.1588591777435));
#170092=CARTESIAN_POINT('Ctrl Pts',(-57.5374634601467,-25.5404968219592,
40.1555254706026));
#170093=CARTESIAN_POINT('Ctrl Pts',(-57.5427567781056,-25.5201405094608,
40.1500631826394));
#170094=CARTESIAN_POINT('Ctrl Pts',(-57.5448916950062,-25.5119303403528,
40.1478601162491));
#170095=CARTESIAN_POINT('Ctrl Pts',(-57.5467757181857,-25.5037488853995,
40.1453112228312));
#170096=CARTESIAN_POINT('Ctrl Pts',(-57.5484131249909,-25.4956235123963,
40.1424401896328));
#170097=CARTESIAN_POINT('Ctrl Pts',(-57.5490172286907,-25.4926257430708,
40.1413809526906));
#170098=CARTESIAN_POINT('Ctrl Pts',(-57.549587657334,-25.4896356883475,
40.1402777640512));
#170099=CARTESIAN_POINT('Ctrl Pts',(-57.5501245740299,-25.4866547635671,
40.1391317641987));
#170100=CARTESIAN_POINT('Ctrl Pts',(-57.5511312928346,-25.4810655296038,
40.1369830144753));
#170101=CARTESIAN_POINT('Ctrl Pts',(-57.5520201961935,-25.4755083930934,
40.134683756585));
#170102=CARTESIAN_POINT('Ctrl Pts',(-57.5527923593831,-25.4699926837174,
40.1322415082996));
#170103=CARTESIAN_POINT('Ctrl Pts',(-57.5554949305467,-25.4506877009014,
40.1236936393009));
#170104=CARTESIAN_POINT('Ctrl Pts',(-57.5567674305412,-25.4318901986625,
40.113394140767));
#170105=CARTESIAN_POINT('Ctrl Pts',(-57.5566559849706,-25.4140001974204,
40.101665321223));
#170106=CARTESIAN_POINT('Ctrl Pts',(-57.5566002621852,-25.4050551967993,
40.095800911451));
#170107=CARTESIAN_POINT('Ctrl Pts',(-57.5561985539314,-25.3963370718386,
40.0895791707949));
#170108=CARTESIAN_POINT('Ctrl Pts',(-57.5554566340482,-25.387895828661,
40.0830403822906));
#170109=CARTESIAN_POINT('Ctrl Pts',(-57.5550856741066,-25.3836752070722,
40.0797709880385));
#170110=CARTESIAN_POINT('Ctrl Pts',(-57.5546296613653,-25.379523805976,
40.0764223317514));
#170111=CARTESIAN_POINT('Ctrl Pts',(-57.5540893180426,-25.3754478763493,
40.0729994484778));
#170112=CARTESIAN_POINT('Ctrl Pts',(-57.5535489747199,-25.3713719467226,
40.0695765652042));
#170113=CARTESIAN_POINT('Ctrl Pts',(-57.5529242061381,-25.3673715770253,
40.0660793733488));
#170114=CARTESIAN_POINT('Ctrl Pts',(-57.55221592936,-25.3634528381784,40.0625130768817));
#170115=CARTESIAN_POINT('Ctrl Pts',(-57.5522098892425,-25.3634194195431,
40.0624826638418));
#170116=CARTESIAN_POINT('Ctrl Pts',(-57.5522038431596,-25.3633860069329,
40.0624522459912));
#170117=CARTESIAN_POINT('Ctrl Pts',(-57.552197791112,-25.3633526003509,
40.0624218233329));
#170118=CARTESIAN_POINT('Ctrl Pts',(-57.5491069220861,-25.34629137115,40.0468845275888));
#170119=CARTESIAN_POINT('Ctrl Pts',(-57.5445791409883,-25.3307446654432,
40.0302263329214));
#170120=CARTESIAN_POINT('Ctrl Pts',(-57.5388132486341,-25.3167379215524,
40.0127515884706));
#170121=CARTESIAN_POINT('Ctrl Pts',(-57.5328523576292,-25.3022574788841,
39.9946858597662));
#170122=CARTESIAN_POINT('Ctrl Pts',(-57.5255675223644,-25.289422326754,
39.9757460620419));
#170123=CARTESIAN_POINT('Ctrl Pts',(-57.5171444507262,-25.2783002469273,
39.956244455904));
#170124=CARTESIAN_POINT('Ctrl Pts',(-57.5088816036346,-25.2673897324622,
39.9371138113505));
#170125=CARTESIAN_POINT('Ctrl Pts',(-57.4995225236582,-25.258127464752,
39.9174410654228));
#170126=CARTESIAN_POINT('Ctrl Pts',(-57.48922251386,-25.2506209171082,39.8975196504002));
#170127=CARTESIAN_POINT('Ctrl Pts',(-57.4823991184743,-25.2456480924645,
39.8843224113678));
#170128=CARTESIAN_POINT('Ctrl Pts',(-57.4751623993582,-25.2414466709153,
39.8710160447083));
#170129=CARTESIAN_POINT('Ctrl Pts',(-57.4675553545142,-25.2380597013427,
39.8576902534424));
#170130=CARTESIAN_POINT('',(-57.1420619865023,-25.0931373005743,39.2875012672119));
#170131=CARTESIAN_POINT('',(-57.4675553545142,-25.2380597013427,39.8576902534424));
#170132=CARTESIAN_POINT('',(-59.2554138597572,-19.5876674457075,39.2875012672119));
#170133=CARTESIAN_POINT('Origin',(5.53234440788222E-15,0.,39.2875012672119));
#170134=CARTESIAN_POINT('',(-59.5942745858237,-19.6977666881842,39.8576902534424));
#170135=CARTESIAN_POINT('',(-59.2554138597572,-19.5876674457075,39.2875012672119));
#170136=CARTESIAN_POINT('',(-59.8682321556243,-19.4684195516693,40.1599502534424));
#170137=CARTESIAN_POINT('Ctrl Pts',(-59.5942745858237,-19.6977666881842,
39.8576902534424));
#170138=CARTESIAN_POINT('Ctrl Pts',(-59.6059782661684,-19.7015693056588,
39.8773836120357));
#170139=CARTESIAN_POINT('Ctrl Pts',(-59.6182462127118,-19.7035046472592,
39.8969946442118));
#170140=CARTESIAN_POINT('Ctrl Pts',(-59.6308908042829,-19.7035948839463,
39.916252528822));
#170141=CARTESIAN_POINT('Ctrl Pts',(-59.6437894749888,-19.7036869338402,
39.9358973794034));
#170142=CARTESIAN_POINT('Ctrl Pts',(-59.6570809485089,-19.701859312135,
39.9551762199702));
#170143=CARTESIAN_POINT('Ctrl Pts',(-59.6705908046797,-19.6980881582803,
39.9738152034197));
#170144=CARTESIAN_POINT('Ctrl Pts',(-59.6835758151852,-19.6944635103343,
39.9917300792587));
#170145=CARTESIAN_POINT('Ctrl Pts',(-59.696763446402,-19.6890433025181,
40.0090551158054));
#170146=CARTESIAN_POINT('Ctrl Pts',(-59.7100083536245,-19.6817621015882,
40.0255394551458));
#170147=CARTESIAN_POINT('Ctrl Pts',(-59.7201826317462,-19.6761689356961,
40.03820215261));
#170148=CARTESIAN_POINT('Ctrl Pts',(-59.7303909886952,-19.6694767982716,
40.05036877821));
#170149=CARTESIAN_POINT('Ctrl Pts',(-59.7405669736108,-19.6616375006938,
40.0619155352442));
#170150=CARTESIAN_POINT('Ctrl Pts',(-59.7405936430525,-19.6616169552929,
40.0619457972351));
#170151=CARTESIAN_POINT('Ctrl Pts',(-59.7406203123794,-19.6615964011819,
40.0619760547305));
#170152=CARTESIAN_POINT('Ctrl Pts',(-59.7406469815886,-19.6615758383626,
40.0620063077269));
#170153=CARTESIAN_POINT('Ctrl Pts',(-59.7435064631642,-19.6593710859732,
40.06525004417));
#170154=CARTESIAN_POINT('Ctrl Pts',(-59.7463627094291,-19.6570664708009,
40.0684393223557));
#170155=CARTESIAN_POINT('Ctrl Pts',(-59.74921183173,-19.6546650315162,40.0715697951759));
#170156=CARTESIAN_POINT('Ctrl Pts',(-59.7650665495273,-19.6413015679142,
40.0889901646424));
#170157=CARTESIAN_POINT('Ctrl Pts',(-59.7807038364438,-19.6249436073972,
40.1045963098249));
#170158=CARTESIAN_POINT('Ctrl Pts',(-59.7954515664667,-19.6061700313457,
40.1176634650733));
#170159=CARTESIAN_POINT('Ctrl Pts',(-59.8020705519321,-19.5977441904316,
40.1235281853067));
#170160=CARTESIAN_POINT('Ctrl Pts',(-59.8085107122969,-19.5888317740044,
40.1288820140922));
#170161=CARTESIAN_POINT('Ctrl Pts',(-59.8147133779311,-19.5794843054209,
40.1336621774101));
#170162=CARTESIAN_POINT('Ctrl Pts',(-59.8174089725189,-19.5754220220077,
40.1357395717319));
#170163=CARTESIAN_POINT('Ctrl Pts',(-59.8200595219549,-19.5712776455717,
40.1377083672884));
#170164=CARTESIAN_POINT('Ctrl Pts',(-59.8226600907004,-19.5670554570747,
40.1395632548792));
#170165=CARTESIAN_POINT('Ctrl Pts',(-59.8317620813096,-19.552277797335,
40.146055361447));
#170166=CARTESIAN_POINT('Ctrl Pts',(-59.8402518053949,-19.5365469388441,
40.151152097463));
#170167=CARTESIAN_POINT('Ctrl Pts',(-59.8479176686191,-19.5200464333335,
40.1546258197409));
#170168=CARTESIAN_POINT('Ctrl Pts',(-59.8517506002312,-19.5117961805782,
40.1563626808798));
#170169=CARTESIAN_POINT('Ctrl Pts',(-59.8553775672056,-19.5033535162581,
40.1576937882008));
#170170=CARTESIAN_POINT('Ctrl Pts',(-59.858772127781,-19.4947413867936,
40.1585906813668));
#170171=CARTESIAN_POINT('Ctrl Pts',(-59.8604694080688,-19.4904353220614,
40.1590391279498));
#170172=CARTESIAN_POINT('Ctrl Pts',(-59.862108586874,-19.4860868910811,
40.1593790209175));
#170173=CARTESIAN_POINT('Ctrl Pts',(-59.8636863596423,-19.4816989623699,
40.1596068022931));
#170174=CARTESIAN_POINT('Ctrl Pts',(-59.8652641324106,-19.4773110336587,
40.1598345836687));
#170175=CARTESIAN_POINT('Ctrl Pts',(-59.8667804975193,-19.4728836066889,
40.1599502506864));
#170176=CARTESIAN_POINT('Ctrl Pts',(-59.8682321556243,-19.4684195516693,
40.1599502534424));
#170177=CARTESIAN_POINT('',(-59.8776671349986,-19.4393816709753,40.1599502534424));
#170178=CARTESIAN_POINT('Origin',(1.08121605342496E-16,4.80251501969578E-17,
40.1599502534424));
#170179=CARTESIAN_POINT('',(-59.7908376697913,-19.0928077206408,39.8576902534424));
#170180=CARTESIAN_POINT('Ctrl Pts',(-59.8776671349986,-19.4393816709753,
40.1599502534424));
#170181=CARTESIAN_POINT('Ctrl Pts',(-59.8788471933725,-19.4357468082908,
40.1599502447858));
#170182=CARTESIAN_POINT('Ctrl Pts',(-59.8799786203652,-19.4321071647684,
40.1598744685927));
#170183=CARTESIAN_POINT('Ctrl Pts',(-59.8810618871502,-19.4284649220281,
40.159724693428));
#170184=CARTESIAN_POINT('Ctrl Pts',(-59.8873218328122,-19.407417252186,
40.1588591777435));
#170185=CARTESIAN_POINT('Ctrl Pts',(-59.8919760989598,-19.3862806722135,
40.1555254706024));
#170186=CARTESIAN_POINT('Ctrl Pts',(-59.8951126055059,-19.3654825713326,
40.150063182639));
#170187=CARTESIAN_POINT('Ctrl Pts',(-59.8963776307481,-19.3570942188076,
40.1478601162488));
#170188=CARTESIAN_POINT('Ctrl Pts',(-59.897396138138,-19.3487606486732,
40.1453112228311));
#170189=CARTESIAN_POINT('Ctrl Pts',(-59.8981752423038,-19.3405086316968,
40.1424401896328));
#170190=CARTESIAN_POINT('Ctrl Pts',(-59.8984626844395,-19.337464138434,
40.1413809526905));
#170191=CARTESIAN_POINT('Ctrl Pts',(-59.8987174423897,-19.3344308375139,
40.1402777640511));
#170192=CARTESIAN_POINT('Ctrl Pts',(-59.8989398263133,-19.3314101194741,
40.1391317641987));
#170193=CARTESIAN_POINT('Ctrl Pts',(-59.8993567961701,-19.3257462731497,
40.1369830144753));
#170194=CARTESIAN_POINT('Ctrl Pts',(-59.8996599510837,-19.3201266635125,
40.1346837565849));
#170195=CARTESIAN_POINT('Ctrl Pts',(-59.8998513356577,-19.314560456738,
40.1322415082996));
#170196=CARTESIAN_POINT('Ctrl Pts',(-59.9005211816665,-19.2950787330271,
40.1236936393009));
#170197=CARTESIAN_POINT('Ctrl Pts',(-59.8998218367506,-19.2762511930034,
40.113394140767));
#170198=CARTESIAN_POINT('Ctrl Pts',(-59.8978409873528,-19.2584708442942,
40.101665321223));
#170199=CARTESIAN_POINT('Ctrl Pts',(-59.8968505626539,-19.2495806699396,
40.095800911451));
#170200=CARTESIAN_POINT('Ctrl Pts',(-59.8955397627952,-19.240952293726,
40.0895791707949));
#170201=CARTESIAN_POINT('Ctrl Pts',(-59.8939195570493,-19.2326348443071,
40.0830403822907));
#170202=CARTESIAN_POINT('Ctrl Pts',(-59.8931094541763,-19.2284761195976,
40.0797709880385));
#170203=CARTESIAN_POINT('Ctrl Pts',(-59.8922219999436,-19.2243951266221,
40.0764223317514));
#170204=CARTESIAN_POINT('Ctrl Pts',(-59.8912585660179,-19.2203980066215,
40.0729994484778));
#170205=CARTESIAN_POINT('Ctrl Pts',(-59.8902951320921,-19.2164008866209,
40.0695765652042));
#170206=CARTESIAN_POINT('Ctrl Pts',(-59.889255633561,-19.2124877374671,
40.0660793733488));
#170207=CARTESIAN_POINT('Ctrl Pts',(-59.8881416170477,-19.2086645009648,
40.0625130768817));
#170208=CARTESIAN_POINT('Ctrl Pts',(-59.8881321168199,-19.2086318967645,
40.0624826638418));
#170209=CARTESIAN_POINT('Ctrl Pts',(-59.8881226112893,-19.2085992991799,
40.0624522459912));
#170210=CARTESIAN_POINT('Ctrl Pts',(-59.8881131004568,-19.2085667082138,
40.0624218233329));
#170211=CARTESIAN_POINT('Ctrl Pts',(-59.8832557794653,-19.1919220260021,
40.0468845275897));
#170212=CARTESIAN_POINT('Ctrl Pts',(-59.8771277287702,-19.1769337687768,
40.0302263329234));
#170213=CARTESIAN_POINT('Ctrl Pts',(-59.8699293191639,-19.1636064551624,
40.0127515884738));
#170214=CARTESIAN_POINT('Ctrl Pts',(-59.8624874641246,-19.1498284206511,
39.9946858597706));
#170215=CARTESIAN_POINT('Ctrl Pts',(-59.8539008972224,-19.1378250534631,
39.9757460620477));
#170216=CARTESIAN_POINT('Ctrl Pts',(-59.8443613941402,-19.127644352288,
39.9562444559111));
#170217=CARTESIAN_POINT('Ctrl Pts',(-59.8350033524798,-19.1176573094716,
39.9371138113589));
#170218=CARTESIAN_POINT('Ctrl Pts',(-59.8247273719135,-19.1094240716805,
39.9174410654326));
#170219=CARTESIAN_POINT('Ctrl Pts',(-59.8136991387581,-19.1030352898857,
39.8975196504113));
#170220=CARTESIAN_POINT('Ctrl Pts',(-59.8063933209263,-19.098802945928,
39.8843224113753));
#170221=CARTESIAN_POINT('Ctrl Pts',(-59.7987570771745,-19.0953809833328,
39.8710160447121));
#170222=CARTESIAN_POINT('Ctrl Pts',(-59.7908376697913,-19.0928077206408,
39.8576902534424));
#170223=CARTESIAN_POINT('',(-59.4519788726609,-18.9827025415093,39.2875012672119));
#170224=CARTESIAN_POINT('',(-59.7908376697913,-19.0928077206408,39.8576902534424));
#170225=CARTESIAN_POINT('',(-60.9782752797349,-13.2864868028992,39.2875012672119));
#170226=CARTESIAN_POINT('Origin',(5.53234440788222E-15,0.,39.2875012672119));
#170227=CARTESIAN_POINT('',(-61.3267881959114,-13.3605623192483,39.8576902534424));
#170228=CARTESIAN_POINT('',(-60.9782752797349,-13.2864868028992,39.2875012672119));
#170229=CARTESIAN_POINT('',(-61.5752716937452,-13.1038352065724,40.1599502534424));
#170230=CARTESIAN_POINT('Ctrl Pts',(-61.3267881959114,-13.3605623192483,
39.8576902534424));
#170231=CARTESIAN_POINT('Ctrl Pts',(-61.3388252440322,-13.3631207378657,
39.8773836120366));
#170232=CARTESIAN_POINT('Ctrl Pts',(-61.3512282837647,-13.3637631278627,
39.8969946442137));
#170233=CARTESIAN_POINT('Ctrl Pts',(-61.363813039243,-13.3625311504981,
39.9162525288247));
#170234=CARTESIAN_POINT('Ctrl Pts',(-61.3766506715158,-13.3612744179057,
39.9358973794071));
#170235=CARTESIAN_POINT('Ctrl Pts',(-61.3896782944657,-13.3580674708013,
39.9551762199749));
#170236=CARTESIAN_POINT('Ctrl Pts',(-61.4027199493144,-13.3529048112168,
39.9738152034253));
#170237=CARTESIAN_POINT('Ctrl Pts',(-61.4152549476949,-13.3479427162771,
39.9917300792654));
#170238=CARTESIAN_POINT('Ctrl Pts',(-61.4278037696953,-13.3411737181002,
40.0090551158131));
#170239=CARTESIAN_POINT('Ctrl Pts',(-61.4402150271871,-13.3325479345514,
40.0255394551543));
#170240=CARTESIAN_POINT('Ctrl Pts',(-61.449748924511,-13.3259219069513,
40.0382021526155));
#170241=CARTESIAN_POINT('Ctrl Pts',(-61.4592018401694,-13.3181993658929,
40.0503687782126));
#170242=CARTESIAN_POINT('Ctrl Pts',(-61.4685026502439,-13.309339332744,
40.0619155352442));
#170243=CARTESIAN_POINT('Ctrl Pts',(-61.4685270260084,-13.3093161121772,
40.0619457972351));
#170244=CARTESIAN_POINT('Ctrl Pts',(-61.4685514007483,-13.30929288296,40.0619760547305));
#170245=CARTESIAN_POINT('Ctrl Pts',(-61.4685757744609,-13.3092696450946,
40.0620063077269));
#170246=CARTESIAN_POINT('Ctrl Pts',(-61.4711891321181,-13.3067780733547,
40.06525004417));
#170247=CARTESIAN_POINT('Ctrl Pts',(-61.4737888336847,-13.3041875240726,
40.0684393223557));
#170248=CARTESIAN_POINT('Ctrl Pts',(-61.4763713294375,-13.3015014257478,
40.0715697951759));
#170249=CARTESIAN_POINT('Ctrl Pts',(-61.490742331116,-13.2865538993123,
40.0889901646406));
#170250=CARTESIAN_POINT('Ctrl Pts',(-61.5045840828622,-13.2686510078457,
40.1045963098216));
#170251=CARTESIAN_POINT('Ctrl Pts',(-61.5172886502212,-13.2484387178548,
40.1176634650692));
#170252=CARTESIAN_POINT('Ctrl Pts',(-61.5229906359905,-13.2393671621978,
40.1235281853042));
#170253=CARTESIAN_POINT('Ctrl Pts',(-61.5284639152912,-13.2298303888521,
40.1288820140911));
#170254=CARTESIAN_POINT('Ctrl Pts',(-61.5336555255488,-13.2198857715702,
40.1336621774101));
#170255=CARTESIAN_POINT('Ctrl Pts',(-61.5359117291449,-13.2155639754107,
40.1357395717319));
#170256=CARTESIAN_POINT('Ctrl Pts',(-61.5381145532937,-13.2111652444432,
40.1377083672884));
#170257=CARTESIAN_POINT('Ctrl Pts',(-61.5402595369763,-13.2066943520819,
40.1395632548792));
#170258=CARTESIAN_POINT('Ctrl Pts',(-61.5477669798653,-13.1910462288175,
40.146055361447));
#170259=CARTESIAN_POINT('Ctrl Pts',(-61.5545658738899,-13.1745141278031,
40.151152097463));
#170260=CARTESIAN_POINT('Ctrl Pts',(-61.5604649702291,-13.1573027128857,
40.1546258197409));
#170261=CARTESIAN_POINT('Ctrl Pts',(-61.5634145183987,-13.148697005427,
40.1563626808798));
#170262=CARTESIAN_POINT('Ctrl Pts',(-61.5661391177411,-13.1399214696213,
40.1576937882008));
#170263=CARTESIAN_POINT('Ctrl Pts',(-61.5686148699002,-13.1310016901027,
40.1585906813668));
#170264=CARTESIAN_POINT('Ctrl Pts',(-61.5698527459798,-13.1265418003434,
40.1590391279498));
#170265=CARTESIAN_POINT('Ctrl Pts',(-61.571028410384,-13.1220458496815,
40.1593790209175));
#170266=CARTESIAN_POINT('Ctrl Pts',(-61.5721388765028,-13.11751703634,40.1596068022931));
#170267=CARTESIAN_POINT('Ctrl Pts',(-61.5732493426217,-13.1129882229985,
40.1598345836687));
#170268=CARTESIAN_POINT('Ctrl Pts',(-61.5742946087864,-13.1084265466224,
40.1599502506865));
#170269=CARTESIAN_POINT('Ctrl Pts',(-61.5752716937452,-13.1038352065724,
40.1599502534424));
#170270=CARTESIAN_POINT('',(-61.5816197022698,-13.0739701745321,40.1599502534424));
#170271=CARTESIAN_POINT('Origin',(1.12331902584552E-16,3.23121069746441E-17,
40.1599502534424));
#170272=CARTESIAN_POINT('',(-61.4590390555209,-12.7383709431247,39.8576902534424));
#170273=CARTESIAN_POINT('Ctrl Pts',(-61.5816197022698,-13.0739701745321,
40.1599502534424));
#170274=CARTESIAN_POINT('Ctrl Pts',(-61.5824133495499,-13.0702318743173,
40.1599502447858));
#170275=CARTESIAN_POINT('Ctrl Pts',(-61.5831581321229,-13.0664939028182,
40.1598744685927));
#170276=CARTESIAN_POINT('Ctrl Pts',(-61.5838547466226,-13.0627583804523,
40.1597246934279));
#170277=CARTESIAN_POINT('Ctrl Pts',(-61.5878803190634,-13.041171669447,
40.1588591777435));
#170278=CARTESIAN_POINT('Ctrl Pts',(-61.5902997144309,-13.0196643745825,
40.1555254706023));
#170279=CARTESIAN_POINT('Ctrl Pts',(-61.5912450453419,-12.9986523536645,
40.1500631826386));
#170280=CARTESIAN_POINT('Ctrl Pts',(-61.5916263190447,-12.9901777222684,
40.1478601162485));
#170281=CARTESIAN_POINT('Ctrl Pts',(-61.5917681516647,-12.9817833412915,
40.1453112228309));
#170282=CARTESIAN_POINT('Ctrl Pts',(-61.591680417163,-12.973495091167,40.1424401896328));
#170283=CARTESIAN_POINT('Ctrl Pts',(-61.5916480484584,-12.9704372300721,
40.1413809526906));
#170284=CARTESIAN_POINT('Ctrl Pts',(-61.5915843445341,-12.9673939164347,
40.1402777640511));
#170285=CARTESIAN_POINT('Ctrl Pts',(-61.5914897592007,-12.9643665007547,
40.1391317641987));
#170286=CARTESIAN_POINT('Ctrl Pts',(-61.5913124117005,-12.9586900963547,
40.1369830144753));
#170287=CARTESIAN_POINT('Ctrl Pts',(-61.5910264967403,-12.9530695832098,
40.134683756585));
#170288=CARTESIAN_POINT('Ctrl Pts',(-61.5906350058491,-12.9475138635629,
40.1322415082996));
#170289=CARTESIAN_POINT('Ctrl Pts',(-61.5892647877301,-12.9280688447991,
40.1236936393009));
#170290=CARTESIAN_POINT('Ctrl Pts',(-61.5866012600731,-12.9094175454589,
40.113394140767));
#170291=CARTESIAN_POINT('Ctrl Pts',(-61.5827727094485,-12.8919416545039,
40.101665321223));
#170292=CARTESIAN_POINT('Ctrl Pts',(-61.5808584341363,-12.8832037090263,
40.095800911451));
#170293=CARTESIAN_POINT('Ctrl Pts',(-61.5786529040703,-12.8747596158553,
40.0895791707949));
#170294=CARTESIAN_POINT('Ctrl Pts',(-61.5761721637749,-12.8666570879113,
40.0830403822907));
#170295=CARTESIAN_POINT('Ctrl Pts',(-61.5749317936272,-12.8626058239394,
40.0797709880385));
#170296=CARTESIAN_POINT('Ctrl Pts',(-61.5736226210372,-12.8586399512975,
40.0764223317514));
#170297=CARTESIAN_POINT('Ctrl Pts',(-61.5722466520922,-12.8547654342062,
40.0729994484778));
#170298=CARTESIAN_POINT('Ctrl Pts',(-61.5708706831472,-12.8508909171149,
40.0695765652042));
#170299=CARTESIAN_POINT('Ctrl Pts',(-61.5694278436302,-12.8471078617857,
40.0660793733488));
#170300=CARTESIAN_POINT('Ctrl Pts',(-61.5679202927796,-12.8434220158072,
40.0625130768817));
#170301=CARTESIAN_POINT('Ctrl Pts',(-61.5679074365281,-12.8433905832603,
40.0624826638418));
#170302=CARTESIAN_POINT('Ctrl Pts',(-61.5678945756944,-12.8433591578472,
40.0624522459912));
#170303=CARTESIAN_POINT('Ctrl Pts',(-61.5678817102796,-12.8433277395705,
40.0624218233329));
#170304=CARTESIAN_POINT('Ctrl Pts',(-61.5613111551479,-12.8272819669692,
40.0468845275905));
#170305=CARTESIAN_POINT('Ctrl Pts',(-61.5536499750613,-12.8130163727079,
40.0302263329252));
#170306=CARTESIAN_POINT('Ctrl Pts',(-61.545097915485,-12.8005145062065,
40.0127515884766));
#170307=CARTESIAN_POINT('Ctrl Pts',(-61.5362566309325,-12.7875898348815,
39.9946858597744));
#170308=CARTESIAN_POINT('Ctrl Pts',(-61.5264624086167,-12.7765497640383,
39.9757460620526));
#170309=CARTESIAN_POINT('Ctrl Pts',(-61.5159109908824,-12.767421983407,
39.9562444559172));
#170310=CARTESIAN_POINT('Ctrl Pts',(-61.5055602833158,-12.7584678323701,
39.937113811366));
#170311=CARTESIAN_POINT('Ctrl Pts',(-61.4944799879529,-12.7513538295741,
39.9174410654407));
#170312=CARTESIAN_POINT('Ctrl Pts',(-61.4828443590702,-12.7461528104584,
39.8975196504204));
#170313=CARTESIAN_POINT('Ctrl Pts',(-61.4751361628613,-12.7427073176334,
39.8843224113814));
#170314=CARTESIAN_POINT('Ctrl Pts',(-61.4671840587585,-12.7401023057311,
39.8710160447151));
#170315=CARTESIAN_POINT('Ctrl Pts',(-61.4590390555209,-12.7383709431247,
39.8576902534424));
#170316=CARTESIAN_POINT('',(-61.1105274371642,-12.6642893210138,39.2875012672119));
#170317=CARTESIAN_POINT('',(-61.4590390555209,-12.7383709431247,39.8576902534424));
#170318=CARTESIAN_POINT('',(-62.0330459552233,-6.83973663030219,39.2875012672119));
#170319=CARTESIAN_POINT('Origin',(5.53234440788222E-15,0.,39.2875012672119));
#170320=CARTESIAN_POINT('',(-62.3873926810692,-6.87697683366523,39.8576902534424));
#170321=CARTESIAN_POINT('',(-62.0330459552233,-6.83973663030219,39.2875012672119));
#170322=CARTESIAN_POINT('',(-62.6076796697355,-6.59568250079844,40.1599502534424));
#170323=CARTESIAN_POINT('Ctrl Pts',(-62.3873926810692,-6.87697683366523,
39.8576902534424));
#170324=CARTESIAN_POINT('Ctrl Pts',(-62.3996312165479,-6.87826302285553,
39.8773836120375));
#170325=CARTESIAN_POINT('Ctrl Pts',(-62.4120334591708,-6.87760542308973,
39.8969946442154));
#170326=CARTESIAN_POINT('Ctrl Pts',(-62.4244204973417,-6.87506472947493,
39.9162525288273));
#170327=CARTESIAN_POINT('Ctrl Pts',(-62.4370564393957,-6.87247298342148,
39.9358973794106));
#170328=CARTESIAN_POINT('Ctrl Pts',(-62.4496774784119,-6.8679218469014,
39.9551762199793));
#170329=CARTESIAN_POINT('Ctrl Pts',(-62.4621080448386,-6.86142424476579,
39.9738152034304));
#170330=CARTESIAN_POINT('Ctrl Pts',(-62.4740556950283,-6.85517906858289,
39.9917300792713));
#170331=CARTESIAN_POINT('Ctrl Pts',(-62.485828220292,-6.84713544260593,
40.0090551158197));
#170332=CARTESIAN_POINT('Ctrl Pts',(-62.4972698477183,-6.83725958232806,
40.0255394551615));
#170333=CARTESIAN_POINT('Ctrl Pts',(-62.5060589088708,-6.82967328916524,
40.0382021526201));
#170334=CARTESIAN_POINT('Ctrl Pts',(-62.5146528151171,-6.82100495424908,
40.0503687782148));
#170335=CARTESIAN_POINT('Ctrl Pts',(-62.5229765487298,-6.81122125790639,
40.0619155352442));
#170336=CARTESIAN_POINT('Ctrl Pts',(-62.5229983637511,-6.81119561658308,
40.0619457972351));
#170337=CARTESIAN_POINT('Ctrl Pts',(-62.5230201768492,-6.81116996676389,
40.0619760547305));
#170338=CARTESIAN_POINT('Ctrl Pts',(-62.5230419880218,-6.81114430845115,
40.0620063077269));
#170339=CARTESIAN_POINT('Ctrl Pts',(-62.5253805892672,-6.80839321554205,
40.06525004417));
#170340=CARTESIAN_POINT('Ctrl Pts',(-62.5276952632611,-6.80554511475028,
40.0684393223557));
#170341=CARTESIAN_POINT('Ctrl Pts',(-62.5299828381019,-6.80260378684076,
40.0715697951759));
#170342=CARTESIAN_POINT('Ctrl Pts',(-62.5427126719606,-6.78623596579932,
40.0889901646392));
#170343=CARTESIAN_POINT('Ctrl Pts',(-62.5546072354084,-6.76698429120816,
40.1045963098191));
#170344=CARTESIAN_POINT('Ctrl Pts',(-62.5651294462056,-6.74555473735616,
40.1176634650661));
#170345=CARTESIAN_POINT('Ctrl Pts',(-62.569851960129,-6.73593685681868,
40.1235281853023));
#170346=CARTESIAN_POINT('Ctrl Pts',(-62.5742983919715,-6.72588021343918,
40.1288820140902));
#170347=CARTESIAN_POINT('Ctrl Pts',(-62.5784220664834,-6.71544740276736,
40.1336621774101));
#170348=CARTESIAN_POINT('Ctrl Pts',(-62.580214159649,-6.71091344436472,
40.1357395717319));
#170349=CARTESIAN_POINT('Ctrl Pts',(-62.5819451239083,-6.70630855228255,
40.1377083672884));
#170350=CARTESIAN_POINT('Ctrl Pts',(-62.5836110216378,-6.70163794008936,
40.1395632548792));
#170351=CARTESIAN_POINT('Ctrl Pts',(-62.5894416636914,-6.68529079741317,
40.146055361447));
#170352=CARTESIAN_POINT('Ctrl Pts',(-62.5944752375494,-6.66813858303363,
40.151152097463));
#170353=CARTESIAN_POINT('Ctrl Pts',(-62.5985429352697,-6.65040483057297,
40.1546258197409));
#170354=CARTESIAN_POINT('Ctrl Pts',(-62.6005767841298,-6.64153795434265,
40.1563626808798));
#170355=CARTESIAN_POINT('Ctrl Pts',(-62.6023691645599,-6.63252569365801,
40.1576937882008));
#170356=CARTESIAN_POINT('Ctrl Pts',(-62.6038989834438,-6.62339599105629,
40.1585906813668));
#170357=CARTESIAN_POINT('Ctrl Pts',(-62.6046638928858,-6.61883113975543,
40.1590391279498));
#170358=CARTESIAN_POINT('Ctrl Pts',(-62.6053631620638,-6.61423692798816,
40.1593790209175));
#170359=CARTESIAN_POINT('Ctrl Pts',(-62.6059941550341,-6.6096168486431,
40.1596068022931));
#170360=CARTESIAN_POINT('Ctrl Pts',(-62.6066251480043,-6.60499676929804,
40.1598345836687));
#170361=CARTESIAN_POINT('Ctrl Pts',(-62.6071878630701,-6.60035082219649,
40.1599502506865));
#170362=CARTESIAN_POINT('Ctrl Pts',(-62.6076796697355,-6.59568250079845,
40.1599502534424));
#170363=CARTESIAN_POINT('',(-62.6108711573006,-6.56531752495261,40.1599502534424));
#170364=CARTESIAN_POINT('Origin',(1.148766751165E-16,1.62450455465728E-17,
40.1599502534424));
#170365=CARTESIAN_POINT('',(-62.4538823482276,-6.24436990788019,39.8576902534424));
#170366=CARTESIAN_POINT('Ctrl Pts',(-62.6108711573006,-6.56531752495261,
40.1599502534424));
#170367=CARTESIAN_POINT('Ctrl Pts',(-62.6112696981211,-6.56151674480702,
40.1599502447858));
#170368=CARTESIAN_POINT('Ctrl Pts',(-62.6116196762807,-6.557721399329,40.1598744685927));
#170369=CARTESIAN_POINT('Ctrl Pts',(-62.6119220062409,-6.55393352450239,
40.1597246934279));
#170370=CARTESIAN_POINT('Ctrl Pts',(-62.6136691004464,-6.53204428085628,
40.1588591777434));
#170371=CARTESIAN_POINT('Ctrl Pts',(-62.6138271176316,-6.51040190952224,
40.1555254706018));
#170372=CARTESIAN_POINT('Ctrl Pts',(-62.612570915664,-6.48940618066474,
40.1500631826375));
#170373=CARTESIAN_POINT('Ctrl Pts',(-62.6120642605129,-6.4809381202332,
40.1478601162477));
#170374=CARTESIAN_POINT('Ctrl Pts',(-62.6113278644156,-6.47257489900915,
40.1453112228304));
#170375=CARTESIAN_POINT('Ctrl Pts',(-62.610374252484,-6.46434122353989,
40.1424401896328));
#170376=CARTESIAN_POINT('Ctrl Pts',(-62.6100224275775,-6.46130349717896,
40.1413809526905));
#170377=CARTESIAN_POINT('Ctrl Pts',(-62.6096409597322,-6.45828351400542,
40.1402777640511));
#170378=CARTESIAN_POINT('Ctrl Pts',(-62.6092304414384,-6.45528256968482,
40.1391317641987));
#170379=CARTESIAN_POINT('Ctrl Pts',(-62.6084607196375,-6.4496557990837,
40.1369830144753));
#170380=CARTESIAN_POINT('Ctrl Pts',(-62.6075888673476,-6.44409596194931,
40.1346837565849));
#170381=CARTESIAN_POINT('Ctrl Pts',(-62.6066187902475,-6.43861159905725,
40.1322415082996));
#170382=CARTESIAN_POINT('Ctrl Pts',(-62.6032235203971,-6.41941632893507,
40.1236936393008));
#170383=CARTESIAN_POINT('Ctrl Pts',(-62.5986249921653,-6.40114561781709,
40.113394140767));
#170384=CARTESIAN_POINT('Ctrl Pts',(-62.5929906867159,-6.38416565413452,
40.101665321223));
#170385=CARTESIAN_POINT('Ctrl Pts',(-62.5901735339912,-6.37567567229323,
40.095800911451));
#170386=CARTESIAN_POINT('Ctrl Pts',(-62.5870974379668,-6.36750837741663,
40.0895791707949));
#170387=CARTESIAN_POINT('Ctrl Pts',(-62.5837833426318,-6.35970954393935,
40.0830403822907));
#170388=CARTESIAN_POINT('Ctrl Pts',(-62.5821262949642,-6.35581012720071,
40.0797709880385));
#170389=CARTESIAN_POINT('Ctrl Pts',(-62.580409747586,-6.35200282582317,
40.0764223317514));
#170390=CARTESIAN_POINT('Ctrl Pts',(-62.5786363190253,-6.34829336166122,
40.0729994484778));
#170391=CARTESIAN_POINT('Ctrl Pts',(-62.5768628904647,-6.34458389749927,
40.0695765652042));
#170392=CARTESIAN_POINT('Ctrl Pts',(-62.5750325180135,-6.34097238394038,
40.0660793733488));
#170393=CARTESIAN_POINT('Ctrl Pts',(-62.5731479498682,-6.33746431138553,
40.0625130768817));
#170394=CARTESIAN_POINT('Ctrl Pts',(-62.5731318784488,-6.33743439487368,
40.0624826638418));
#170395=CARTESIAN_POINT('Ctrl Pts',(-62.5731158032179,-6.33740448593541,
40.0624522459912));
#170396=CARTESIAN_POINT('Ctrl Pts',(-62.5730997241771,-6.33737458457336,
40.0624218233329));
#170397=CARTESIAN_POINT('Ctrl Pts',(-62.5648879232826,-6.32210352242532,
40.0468845275918));
#170398=CARTESIAN_POINT('Ctrl Pts',(-62.5557775512973,-6.3087168879643,
40.030226332928));
#170399=CARTESIAN_POINT('Ctrl Pts',(-62.5459655399057,-6.29717744164162,
40.012751588481));
#170400=CARTESIAN_POINT('Ctrl Pts',(-62.5358216928042,-6.28524773890675,
39.9946858597805));
#170401=CARTESIAN_POINT('Ctrl Pts',(-62.5249271226245,-6.27529192173462,
39.9757460620605));
#170402=CARTESIAN_POINT('Ctrl Pts',(-62.5134793937792,-6.26731706752176,
39.9562444559268));
#170403=CARTESIAN_POINT('Ctrl Pts',(-62.502249424825,-6.25949391181675,
39.9371138113773));
#170404=CARTESIAN_POINT('Ctrl Pts',(-62.4904862127005,-6.25357708651889,
39.9174410654536));
#170405=CARTESIAN_POINT('Ctrl Pts',(-62.4783706704757,-6.24962081353567,
39.8975196504349));
#170406=CARTESIAN_POINT('Ctrl Pts',(-62.4703445484992,-6.24699992138354,
39.8843224113911));
#170407=CARTESIAN_POINT('Ctrl Pts',(-62.4621637089609,-6.24524040122965,
39.87101604472));
#170408=CARTESIAN_POINT('Ctrl Pts',(-62.4538823482276,-6.24436990788019,
39.8576902534424));
#170409=CARTESIAN_POINT('',(-62.0995362748659,-6.20712349654422,39.2875012672119));
#170410=CARTESIAN_POINT('',(-62.4538823482276,-6.24436990788019,39.8576902534424));
#170411=CARTESIAN_POINT('',(-62.4081695979768,-0.318048871877127,39.2875012672119));
#170412=CARTESIAN_POINT('Origin',(5.53234440788222E-15,0.,39.2875012672119));
#170413=CARTESIAN_POINT('',(-62.7644678366119,-0.318045750793044,39.8576902534424));
#170414=CARTESIAN_POINT('',(-62.4081695979768,-0.318048871877129,39.2875012672119));
#170415=CARTESIAN_POINT('Ctrl Pts',(-62.7644678366119,-0.318045750793045,
39.8576902534424));
#170416=CARTESIAN_POINT('Ctrl Pts',(-62.7767737714912,-0.318045618798132,
39.8773836120357));
#170417=CARTESIAN_POINT('Ctrl Pts',(-62.7890393354372,-0.316095234070559,
39.8969946442117));
#170418=CARTESIAN_POINT('Ctrl Pts',(-62.8010929413166,-0.312273660577473,
39.9162525288219));
#170419=CARTESIAN_POINT('Ctrl Pts',(-62.8133887511246,-0.308375296775969,
39.9358973794033));
#170420=CARTESIAN_POINT('Ctrl Pts',(-62.8254649274609,-0.302529834045832,
39.9551762199702));
#170421=CARTESIAN_POINT('Ctrl Pts',(-62.8371482135769,-0.294768478449938,
39.9738152034198));
#170422=CARTESIAN_POINT('Ctrl Pts',(-62.8483776146185,-0.287308644483076,
39.9917300792591));
#170423=CARTESIAN_POINT('Ctrl Pts',(-62.8592448608937,-0.278078518358053,
40.0090551158061));
#170424=CARTESIAN_POINT('Ctrl Pts',(-62.8695915013888,-0.267060783346145,
40.0255394551467));
#170425=CARTESIAN_POINT('Ctrl Pts',(-62.8775394315818,-0.258597341632753,
40.0382021526107));
#170426=CARTESIAN_POINT('Ctrl Pts',(-62.8851801717857,-0.249078184945598,
40.0503687782103));
#170427=CARTESIAN_POINT('Ctrl Pts',(-62.8924356323738,-0.238478017627878,
40.0619155352442));
#170428=CARTESIAN_POINT('Ctrl Pts',(-62.892454647642,-0.23845023647977,
40.0619457972351));
#170429=CARTESIAN_POINT('Ctrl Pts',(-62.8924736601095,-0.238422447083347,
40.0619760547305));
#170430=CARTESIAN_POINT('Ctrl Pts',(-62.8924926697742,-0.238394649441185,
40.0620063077269));
#170431=CARTESIAN_POINT('Ctrl Pts',(-62.8945308924032,-0.23541417691252,
40.06525004417));
#170432=CARTESIAN_POINT('Ctrl Pts',(-62.8965351787718,-0.232339728999315,
40.0684393223557));
#170433=CARTESIAN_POINT('Ctrl Pts',(-62.8985027695519,-0.229175397309122,
40.0715697951759));
#170434=CARTESIAN_POINT('Ctrl Pts',(-62.9094519648694,-0.211566610931162,
40.088990164641));
#170435=CARTESIAN_POINT('Ctrl Pts',(-62.9192690206947,-0.191177078586841,
40.1045963098225));
#170436=CARTESIAN_POINT('Ctrl Pts',(-62.9274935913881,-0.168765047545427,
40.1176634650702));
#170437=CARTESIAN_POINT('Ctrl Pts',(-62.9311848926126,-0.158706217642862,
40.1235281853049));
#170438=CARTESIAN_POINT('Ctrl Pts',(-62.9345557609572,-0.148239886922884,
40.1288820140914));
#170439=CARTESIAN_POINT('Ctrl Pts',(-62.9375663198809,-0.137433186922322,
40.1336621774101));
#170440=CARTESIAN_POINT('Ctrl Pts',(-62.9388746680683,-0.132736741273575,
40.1357395717319));
#170441=CARTESIAN_POINT('Ctrl Pts',(-62.9401148076313,-0.127976140238065,
40.1377083672884));
#170442=CARTESIAN_POINT('Ctrl Pts',(-62.9412833674838,-0.123156980417526,
40.1395632548792));
#170443=CARTESIAN_POINT('Ctrl Pts',(-62.9453733269673,-0.106289921045641,
40.146055361447));
#170444=CARTESIAN_POINT('Ctrl Pts',(-62.9485864317704,-0.0887055165510291,
40.151152097463));
#170445=CARTESIAN_POINT('Ctrl Pts',(-62.9507781643242,-0.0706437212501446,
40.1546258197409));
#170446=CARTESIAN_POINT('Ctrl Pts',(-62.9518740306011,-0.0616128235997025,
40.1563626808798));
#170447=CARTESIAN_POINT('Ctrl Pts',(-62.9527145544237,-0.0524625782501274,
40.1576937882008));
#170448=CARTESIAN_POINT('Ctrl Pts',(-62.9532816790167,-0.0432229794975093,
40.1585906813668));
#170449=CARTESIAN_POINT('Ctrl Pts',(-62.9535652413132,-0.0386031801212003,
40.1590391279498));
#170450=CARTESIAN_POINT('Ctrl Pts',(-62.9537804539255,-0.0339610423941066,
40.1593790209175));
#170451=CARTESIAN_POINT('Ctrl Pts',(-62.9539250604562,-0.0293003156015957,
40.1596068022931));
#170452=CARTESIAN_POINT('Ctrl Pts',(-62.9540696669868,-0.0246395888090847,
40.1598345836687));
#170453=CARTESIAN_POINT('Ctrl Pts',(-62.9541436657296,-0.0199602729507917,
40.1599502506865));
#170454=CARTESIAN_POINT('Ctrl Pts',(-62.9541448057648,-0.0152661173108669,
40.1599502534424));
#170455=CARTESIAN_POINT('',(-62.2224557307631,-7.62005312457669E-15,38.989));
#170456=CARTESIAN_POINT('',(-62.7644678366119,0.318045750793044,39.8576902534424));
#170457=CARTESIAN_POINT('Ctrl Pts',(-62.9541448057648,0.0152661173108668,
40.1599502534424));
#170458=CARTESIAN_POINT('Ctrl Pts',(-62.9541438736292,0.0190877352446491,
40.1599502447858));
#170459=CARTESIAN_POINT('Ctrl Pts',(-62.9540952129414,0.0228988721022259,
40.1598744685927));
#170460=CARTESIAN_POINT('Ctrl Pts',(-62.9539999459718,0.0266975986403491,
40.1597246934279));
#170461=CARTESIAN_POINT('Ctrl Pts',(-62.953449420412,0.0486495517950492,
40.1588591777433));
#170462=CARTESIAN_POINT('Ctrl Pts',(-62.9513443281449,0.0701898812509633,
40.1555254706009));
#170463=CARTESIAN_POINT('Ctrl Pts',(-62.9479003565096,0.0909392844504461,
40.1500631826352));
#170464=CARTESIAN_POINT('Ctrl Pts',(-62.9465113235251,0.0993079960735539,
40.1478601162459));
#170465=CARTESIAN_POINT('Ctrl Pts',(-62.9449047668205,0.107548428341324,
40.1453112228295));
#170466=CARTESIAN_POINT('Ctrl Pts',(-62.9430957254317,0.115637319282268,
40.1424401896328));
#170467=CARTESIAN_POINT('Ctrl Pts',(-62.9424282989905,0.118621628943523,
40.1413809526906));
#170468=CARTESIAN_POINT('Ctrl Pts',(-62.9417332466658,0.121585194085607,
40.1402777640511));
#170469=CARTESIAN_POINT('Ctrl Pts',(-62.9410112931359,0.124526788072828,
40.1391317641987));
#170470=CARTESIAN_POINT('Ctrl Pts',(-62.9396576302675,0.130042276798866,
40.1369830144753));
#170471=CARTESIAN_POINT('Ctrl Pts',(-62.938209392844,0.135480523183637,
40.134683756585));
#170472=CARTESIAN_POINT('Ctrl Pts',(-62.9366713579026,0.140833441493401,
40.1322415082996));
#170473=CARTESIAN_POINT('Ctrl Pts',(-62.9312882356078,0.159568655577575,
40.1236936393009));
#170474=CARTESIAN_POINT('Ctrl Pts',(-62.9248050892389,0.177258600738988,
40.113394140767));
#170475=CARTESIAN_POINT('Ctrl Pts',(-62.9174267595942,0.193556601113662,
40.101665321223));
#170476=CARTESIAN_POINT('Ctrl Pts',(-62.9137375947718,0.201705601300999,
40.095800911451));
#170477=CARTESIAN_POINT('Ctrl Pts',(-62.9098246351408,0.209506615291412,
40.0895791707949));
#170478=CARTESIAN_POINT('Ctrl Pts',(-62.9057134946881,0.2169163086504,40.0830403822907));
#170479=CARTESIAN_POINT('Ctrl Pts',(-62.9036579244618,0.220621155329894,
40.0797709880385));
#170480=CARTESIAN_POINT('Ctrl Pts',(-62.9015528091474,0.22422817185255,
40.0764223317514));
#170481=CARTESIAN_POINT('Ctrl Pts',(-62.8994013510256,0.227731941419537,
40.0729994484778));
#170482=CARTESIAN_POINT('Ctrl Pts',(-62.8972498929038,0.231235710986524,
40.0695765652043));
#170483=CARTESIAN_POINT('Ctrl Pts',(-62.8950520414621,0.23463611427673,
40.0660793733488));
#170484=CARTESIAN_POINT('Ctrl Pts',(-62.8928111037451,0.237927978230917,
40.0625130768817));
#170485=CARTESIAN_POINT('Ctrl Pts',(-62.8927919932396,0.237956050936214,
40.0624826638418));
#170486=CARTESIAN_POINT('Ctrl Pts',(-62.8927728797351,0.237984115711007,
40.0624522459912));
#170487=CARTESIAN_POINT('Ctrl Pts',(-62.8927537632335,0.238012172552842,
40.0624218233329));
#170488=CARTESIAN_POINT('Ctrl Pts',(-62.8829906867849,0.25234121129618,
40.0468845275921));
#170489=CARTESIAN_POINT('Ctrl Pts',(-62.8725309380422,0.264702219189351,
40.0302263329286));
#170490=CARTESIAN_POINT('Ctrl Pts',(-62.8615664772848,0.275152816745237,
40.012751588482));
#170491=CARTESIAN_POINT('Ctrl Pts',(-62.8502312057452,0.285956846571069,
39.9946858597817));
#170492=CARTESIAN_POINT('Ctrl Pts',(-62.8383556508915,0.294719332056153,
39.975746062062));
#170493=CARTESIAN_POINT('Ctrl Pts',(-62.8261370346472,0.30145388567915,
39.9562444559287));
#170494=CARTESIAN_POINT('Ctrl Pts',(-62.8141508421943,0.308060333921374,
39.9371138113794));
#170495=CARTESIAN_POINT('Ctrl Pts',(-62.8018335935211,0.312715155744803,
39.9174410654561));
#170496=CARTESIAN_POINT('Ctrl Pts',(-62.7893708783692,0.315383336840398,
39.8975196504376));
#170497=CARTESIAN_POINT('Ctrl Pts',(-62.781114766499,0.317150913275127,
39.884322411393));
#170498=CARTESIAN_POINT('Ctrl Pts',(-62.7727948225173,0.318045664008455,
39.8710160447209));
#170499=CARTESIAN_POINT('Ctrl Pts',(-62.7644678366119,0.318045750793045,
39.8576902534424));
#170500=CARTESIAN_POINT('',(-62.4081695979768,0.318048871877127,39.2875012672119));
#170501=CARTESIAN_POINT('',(-62.7644678366119,0.318045750793045,39.8576902534424));
#170502=CARTESIAN_POINT('',(-62.0995362748658,6.20712349654507,39.2875012672119));
#170503=CARTESIAN_POINT('Origin',(5.53234440788222E-15,0.,39.2875012672119));
#170504=CARTESIAN_POINT('',(-62.4538823482275,6.24436990788103,39.8576902534424));
#170505=CARTESIAN_POINT('',(-62.0995362748658,6.20712349654507,39.2875012672119));
#170506=CARTESIAN_POINT('',(-62.6108711573005,6.56531752495345,40.1599502534424));
#170507=CARTESIAN_POINT('Ctrl Pts',(-62.4538823482275,6.24436990788103,
39.8576902534424));
#170508=CARTESIAN_POINT('Ctrl Pts',(-62.4661208561129,6.24565635961515,
39.8773836120393));
#170509=CARTESIAN_POINT('Ctrl Pts',(-62.4781153573,6.24887816048243,39.8969946442189));
#170510=CARTESIAN_POINT('Ctrl Pts',(-62.4897034690628,6.25393874389706,
39.9162525288325));
#170511=CARTESIAN_POINT('Ctrl Pts',(-62.5015244311627,6.25910101415925,
39.9358973794174));
#170512=CARTESIAN_POINT('Ctrl Pts',(-62.5129234357071,6.26617675898984,
39.9551762199877));
#170513=CARTESIAN_POINT('Ctrl Pts',(-62.5237314369876,6.27511683301435,
39.9738152034403));
#170514=CARTESIAN_POINT('Ctrl Pts',(-62.5341195572161,6.28370959326737,
39.9917300792824));
#170515=CARTESIAN_POINT('Ctrl Pts',(-62.5439624606807,6.29402509235232,
40.0090551158319));
#170516=CARTESIAN_POINT('Ctrl Pts',(-62.5531007542879,6.3060639894941,40.0255394551746));
#170517=CARTESIAN_POINT('Ctrl Pts',(-62.5601204743257,6.3153118525122,40.0382021526285));
#170518=CARTESIAN_POINT('Ctrl Pts',(-62.56672433493,6.32557753708801,40.0503687782188));
#170519=CARTESIAN_POINT('Ctrl Pts',(-62.5728320301412,6.33687803771732,
40.0619155352442));
#170520=CARTESIAN_POINT('Ctrl Pts',(-62.5728480373211,6.33690765431417,
40.0619457972352));
#170521=CARTESIAN_POINT('Ctrl Pts',(-62.5728640408534,6.33693727882138,
40.0619760547305));
#170522=CARTESIAN_POINT('Ctrl Pts',(-62.5728800407363,6.33696691123619,
40.062006307727));
#170523=CARTESIAN_POINT('Ctrl Pts',(-62.5745955535553,6.34014410870369,
40.06525004417));
#170524=CARTESIAN_POINT('Ctrl Pts',(-62.5762674929177,6.34341121944362,
40.0684393223557));
#170525=CARTESIAN_POINT('Ctrl Pts',(-62.5778935423007,6.3467638858343,40.0715697951759));
#170526=CARTESIAN_POINT('Ctrl Pts',(-62.586942137401,6.36542071199947,40.0889901646418));
#170527=CARTESIAN_POINT('Ctrl Pts',(-62.594574127885,6.38672471011255,40.1045963098239));
#170528=CARTESIAN_POINT('Ctrl Pts',(-62.6004109483562,6.40987366743977,
40.117663465072));
#170529=CARTESIAN_POINT('Ctrl Pts',(-62.603030594214,6.42026324006312,40.123528185306));
#170530=CARTESIAN_POINT('Ctrl Pts',(-62.6052889671226,6.43102458681517,
40.1288820140919));
#170531=CARTESIAN_POINT('Ctrl Pts',(-62.6071534261453,6.44208677567914,
40.1336621774101));
#170532=CARTESIAN_POINT('Ctrl Pts',(-62.6079636948179,6.44689425333267,
40.1357395717319));
#170533=CARTESIAN_POINT('Ctrl Pts',(-62.6086994224562,6.45175840518036,
40.1377083672884));
#170534=CARTESIAN_POINT('Ctrl Pts',(-62.6093578414452,6.45667331290478,
40.1395632548792));
#170535=CARTESIAN_POINT('Ctrl Pts',(-62.6116623079068,6.47387548994023,
40.146055361447));
#170536=CARTESIAN_POINT('Ctrl Pts',(-62.6130197402062,6.49169942613452,
40.151152097463));
#170537=CARTESIAN_POINT('Ctrl Pts',(-62.6133114945132,6.50989137546665,
40.1546258197409));
#170538=CARTESIAN_POINT('Ctrl Pts',(-62.6134573716666,6.51898735013272,
40.1563626808798));
#170539=CARTESIAN_POINT('Ctrl Pts',(-62.6133368299269,6.52817532814438,
40.1576937882008));
#170540=CARTESIAN_POINT('Ctrl Pts',(-62.6129350466932,6.53742359207046,
40.1585906813668));
#170541=CARTESIAN_POINT('Ctrl Pts',(-62.6127341550763,6.5420477240335,40.1590391279498));
#170542=CARTESIAN_POINT('Ctrl Pts',(-62.6124629532085,6.54668692748805,
40.1593790209175));
#170543=CARTESIAN_POINT('Ctrl Pts',(-62.6121195889601,6.55133723782996,
40.1596068022931));
#170544=CARTESIAN_POINT('Ctrl Pts',(-62.6117762247118,6.55598754817187,
40.1598345836687));
#170545=CARTESIAN_POINT('Ctrl Pts',(-62.6113606963859,6.56064896522315,
40.1599502506865));
#170546=CARTESIAN_POINT('Ctrl Pts',(-62.6108711573005,6.56531752495346,
40.1599502534424));
#170547=CARTESIAN_POINT('',(-62.6076796697354,6.59568250079929,40.1599502534424));
#170548=CARTESIAN_POINT('Origin',(1.14876675116497E-16,-1.62450455465748E-17,
40.1599502534424));
#170549=CARTESIAN_POINT('',(-62.3873926810691,6.87697683366608,39.8576902534424));
#170550=CARTESIAN_POINT('Ctrl Pts',(-62.6076796697354,6.59568250079929,
40.1599502534424));
#170551=CARTESIAN_POINT('Ctrl Pts',(-62.6072792748562,6.59948308607546,
40.1599502447858));
#170552=CARTESIAN_POINT('Ctrl Pts',(-62.6068325084578,6.60326825869965,
40.1598744685927));
#170553=CARTESIAN_POINT('Ctrl Pts',(-62.6063406883232,6.6070362173064,40.1597246934279));
#170554=CARTESIAN_POINT('Ctrl Pts',(-62.6034985746712,6.62881036977223,
40.1588591777434));
#170555=CARTESIAN_POINT('Ctrl Pts',(-62.5991534367841,6.65001265698812,
40.1555254706015));
#170556=CARTESIAN_POINT('Ctrl Pts',(-62.5935594283563,6.67028839972168,
40.1500631826366));
#170557=CARTESIAN_POINT('Ctrl Pts',(-62.5913032360739,6.67846607318537,
40.147860116247));
#170558=CARTESIAN_POINT('Ctrl Pts',(-62.588844120533,6.68649343260121,40.14531122283));
#170559=CARTESIAN_POINT('Ctrl Pts',(-62.586199469922,6.69434891543653,40.1424401896328));
#170560=CARTESIAN_POINT('Ctrl Pts',(-62.5852237544099,6.69724711167696,
40.1413809526905));
#170561=CARTESIAN_POINT('Ctrl Pts',(-62.5842227327444,6.70012178934772,
40.1402777640511));
#170562=CARTESIAN_POINT('Ctrl Pts',(-62.5831972538525,6.70297180428227,
40.1391317641987));
#170563=CARTESIAN_POINT('Ctrl Pts',(-62.5812744809302,6.70831558228455,
40.1369830144753));
#170564=CARTESIAN_POINT('Ctrl Pts',(-62.5792657255653,6.71357265535428,
40.1346837565849));
#170565=CARTESIAN_POINT('Ctrl Pts',(-62.5771765838154,6.71873548138859,
40.1322415082996));
#170566=CARTESIAN_POINT('Ctrl Pts',(-62.5698645876906,6.73680537250866,
40.1236936393008));
#170567=CARTESIAN_POINT('Ctrl Pts',(-62.5615678538927,6.75372073697247,
40.113394140767));
#170568=CARTESIAN_POINT('Ctrl Pts',(-62.5525263385764,6.76915820973656,
40.101665321223));
#170569=CARTESIAN_POINT('Ctrl Pts',(-62.5480055809182,6.77687694611861,
40.095800911451));
#170570=CARTESIAN_POINT('Ctrl Pts',(-62.5432986288851,6.78422620968109,
40.0895791707949));
#170571=CARTESIAN_POINT('Ctrl Pts',(-62.5384354858298,6.79116558077077,
40.0830403822906));
#170572=CARTESIAN_POINT('Ctrl Pts',(-62.5360039143022,6.79463526631561,
40.0797709880385));
#170573=CARTESIAN_POINT('Ctrl Pts',(-62.5335332951357,6.79800247875554,
40.0764223317514));
#170574=CARTESIAN_POINT('Ctrl Pts',(-62.5310273792782,6.80126216569498,
40.0729994484778));
#170575=CARTESIAN_POINT('Ctrl Pts',(-62.5285214634206,6.80452185263442,
40.0695765652042));
#170576=CARTESIAN_POINT('Ctrl Pts',(-62.5259802131085,6.80767389012592,
40.0660793733488));
#170577=CARTESIAN_POINT('Ctrl Pts',(-62.5234074580024,6.8107134791291,40.0625130768817));
#170578=CARTESIAN_POINT('Ctrl Pts',(-62.5233855177895,6.8107394004574,40.0624826638418));
#170579=CARTESIAN_POINT('Ctrl Pts',(-62.523363575423,6.81076531358517,40.0624522459912));
#170580=CARTESIAN_POINT('Ctrl Pts',(-62.5233416309051,6.81079121851015,
40.0624218233329));
#170581=CARTESIAN_POINT('Ctrl Pts',(-62.5121342452096,6.8240212419036,40.0468845275903));
#170582=CARTESIAN_POINT('Ctrl Pts',(-62.5004397189039,6.83522119344104,
40.0302263329247));
#170583=CARTESIAN_POINT('Ctrl Pts',(-62.4884429377056,6.84446844329716,
40.0127515884758));
#170584=CARTESIAN_POINT('Ctrl Pts',(-62.4760404333332,6.85402842900305,
39.9946858597733));
#170585=CARTESIAN_POINT('Ctrl Pts',(-62.4633140048678,6.86150157917666,
39.9757460620511));
#170586=CARTESIAN_POINT('Ctrl Pts',(-62.4504583709392,6.86692204703067,
39.9562444559153));
#170587=CARTESIAN_POINT('Ctrl Pts',(-62.4378472782189,6.87223940618026,
39.9371138113637));
#170588=CARTESIAN_POINT('Ctrl Pts',(-62.4251109433493,6.87558122532639,
39.9174410654381));
#170589=CARTESIAN_POINT('Ctrl Pts',(-62.4124375993841,6.87693208138258,
39.8975196504175));
#170590=CARTESIAN_POINT('Ctrl Pts',(-62.4040419533145,6.87782697616094,
39.8843224113794));
#170591=CARTESIAN_POINT('Ctrl Pts',(-62.3956740599416,6.87784715439679,
39.8710160447141));
#170592=CARTESIAN_POINT('Ctrl Pts',(-62.3873926810691,6.87697683366608,
39.8576902534424));
#170593=CARTESIAN_POINT('',(-62.0330459552232,6.83973663030303,39.2875012672119));
#170594=CARTESIAN_POINT('',(-62.3873926810691,6.87697683366608,39.8576902534424));
#170595=CARTESIAN_POINT('',(-61.110527437164,12.6642893210146,39.2875012672119));
#170596=CARTESIAN_POINT('Origin',(5.53234440788222E-15,0.,39.2875012672119));
#170597=CARTESIAN_POINT('',(-61.4590390555207,12.7383709431255,39.8576902534424));
#170598=CARTESIAN_POINT('',(-61.110527437164,12.6642893210146,39.2875012672119));
#170599=CARTESIAN_POINT('',(-61.5816197022697,13.0739701745329,40.1599502534424));
#170600=CARTESIAN_POINT('Ctrl Pts',(-61.4590390555208,12.7383709431255,
39.8576902534424));
#170601=CARTESIAN_POINT('Ctrl Pts',(-61.4710760487555,12.740929619964,39.8773836120375));
#170602=CARTESIAN_POINT('Ctrl Pts',(-61.4826680729155,12.7453875382452,
39.8969946442153));
#170603=CARTESIAN_POINT('Ctrl Pts',(-61.4936637287811,12.7516316867682,
39.9162525288271));
#170604=CARTESIAN_POINT('Ctrl Pts',(-61.5048803302354,12.7580013045755,
39.9358973794104));
#170605=CARTESIAN_POINT('Ctrl Pts',(-61.5154772731058,12.7662298081621,
39.955176219979));
#170606=CARTESIAN_POINT('Ctrl Pts',(-61.5252915748245,12.776250651289,39.9738152034302));
#170607=CARTESIAN_POINT('Ctrl Pts',(-61.5347245998185,12.7858821937447,
39.9917300792711));
#170608=CARTESIAN_POINT('Ctrl Pts',(-61.5434353195605,12.797170047018,40.0090551158196));
#170609=CARTESIAN_POINT('Ctrl Pts',(-61.5512651452214,12.8100982056074,
40.0255394551614));
#170610=CARTESIAN_POINT('Ctrl Pts',(-61.557279745591,12.8200291684151,40.0382021526201));
#170611=CARTESIAN_POINT('Ctrl Pts',(-61.562774373325,12.8309289079008,40.0503687782147));
#170612=CARTESIAN_POINT('Ctrl Pts',(-61.5676673859795,12.8428059312039,
40.0619155352442));
#170613=CARTESIAN_POINT('Ctrl Pts',(-61.5676802096931,12.8428370587639,
40.0619457972352));
#170614=CARTESIAN_POINT('Ctrl Pts',(-61.5676930289521,12.8428681938096,
40.0619760547305));
#170615=CARTESIAN_POINT('Ctrl Pts',(-61.5677058437552,12.8428993363381,
40.062006307727));
#170616=CARTESIAN_POINT('Ctrl Pts',(-61.5690798512467,12.8462384487041,
40.06525004417));
#170617=CARTESIAN_POINT('Ctrl Pts',(-61.5704011254853,12.8496624271217,
40.0684393223557));
#170618=CARTESIAN_POINT('Ctrl Pts',(-61.5716678181341,12.8531666956984,
40.0715697951759));
#170619=CARTESIAN_POINT('Ctrl Pts',(-61.5787166747147,12.8726671535572,
40.0889901646409));
#170620=CARTESIAN_POINT('Ctrl Pts',(-61.5840799821718,12.8946522063751,
40.1045963098221));
#170621=CARTESIAN_POINT('Ctrl Pts',(-61.5874651029941,12.9182844651646,
40.1176634650698));
#170622=CARTESIAN_POINT('Ctrl Pts',(-61.5889843920978,12.9288909501791,
40.1235281853046));
#170623=CARTESIAN_POINT('Ctrl Pts',(-61.5901055263649,12.9398294093986,
40.1288820140913));
#170624=CARTESIAN_POINT('Ctrl Pts',(-61.5908034580837,12.9510258874724,
40.1336621774101));
#170625=CARTESIAN_POINT('Ctrl Pts',(-61.5911067697684,12.9558917253995,
40.1357395717319));
#170626=CARTESIAN_POINT('Ctrl Pts',(-61.591330024696,12.9608061353938,40.1377083672884));
#170627=CARTESIAN_POINT('Ctrl Pts',(-61.5914710890454,12.9657629422646,
40.1395632548792));
#170628=CARTESIAN_POINT('Ctrl Pts',(-61.5919648142681,12.9831117663123,
40.146055361447));
#170629=CARTESIAN_POINT('Ctrl Pts',(-61.5914517017517,13.0009799514314,
40.151152097463));
#170630=CARTESIAN_POINT('Ctrl Pts',(-61.5898402812904,13.019102739991,40.1546258197409));
#170631=CARTESIAN_POINT('Ctrl Pts',(-61.5890345710598,13.0281641342708,
40.1563626808798));
#170632=CARTESIAN_POINT('Ctrl Pts',(-61.5879542844383,13.0372891795348,
40.1576937882008));
#170633=CARTESIAN_POINT('Ctrl Pts',(-61.5865879953991,13.0464447827194,
40.1585906813668));
#170634=CARTESIAN_POINT('Ctrl Pts',(-61.5859048508795,13.0510225843117,
40.1590391279498));
#170635=CARTESIAN_POINT('Ctrl Pts',(-61.585150205876,13.0556080254099,40.1593790209175));
#170636=CARTESIAN_POINT('Ctrl Pts',(-61.5843226328191,13.0601969695279,
40.1596068022931));
#170637=CARTESIAN_POINT('Ctrl Pts',(-61.5834950597622,13.064785913646,40.1598345836687));
#170638=CARTESIAN_POINT('Ctrl Pts',(-61.582594556983,13.0693783604296,40.1599502506865));
#170639=CARTESIAN_POINT('Ctrl Pts',(-61.5816197022697,13.0739701745329,
40.1599502534424));
#170640=CARTESIAN_POINT('',(-61.575271693745,13.1038352065732,40.1599502534424));
#170641=CARTESIAN_POINT('Origin',(1.12331902584553E-16,-3.23121069746461E-17,
40.1599502534424));
#170642=CARTESIAN_POINT('',(-61.3267881959112,13.3605623192491,39.8576902534424));
#170643=CARTESIAN_POINT('Ctrl Pts',(-61.575271693745,13.1038352065732,40.1599502534424));
#170644=CARTESIAN_POINT('Ctrl Pts',(-61.5744762229325,13.1075731191842,
40.1599502447858));
#170645=CARTESIAN_POINT('Ctrl Pts',(-61.5736362456895,13.1112908564316,
40.1598744685927));
#170646=CARTESIAN_POINT('Ctrl Pts',(-61.5727532608743,13.114986764564,40.1597246934279));
#170647=CARTESIAN_POINT('Ctrl Pts',(-61.567650697922,13.1363445541721,40.1588591777434));
#170648=CARTESIAN_POINT('Ctrl Pts',(-61.5611131206543,13.1569765024544,
40.1555254706014));
#170649=CARTESIAN_POINT('Ctrl Pts',(-61.5534303645603,13.1765564394435,
40.1500631826365));
#170650=CARTESIAN_POINT('Ctrl Pts',(-61.5503317322951,13.1844534784439,
40.1478601162469));
#170651=CARTESIAN_POINT('Ctrl Pts',(-61.5470470005027,13.1921798155763,
40.14531122283));
#170652=CARTESIAN_POINT('Ctrl Pts',(-61.5435957160156,13.1997158239902,
40.1424401896328));
#170653=CARTESIAN_POINT('Ctrl Pts',(-61.5423224015758,13.2024961535653,
40.1413809526906));
#170654=CARTESIAN_POINT('Ctrl Pts',(-61.5410263779725,13.2052504481946,
40.1402777640512));
#170655=CARTESIAN_POINT('Ctrl Pts',(-61.5397086090799,13.2079776587165,
40.1391317641987));
#170656=CARTESIAN_POINT('Ctrl Pts',(-61.5372377924062,13.213091178445,40.1369830144753));
#170657=CARTESIAN_POINT('Ctrl Pts',(-61.5346905274441,13.218109480607,40.134683756585));
#170658=CARTESIAN_POINT('Ctrl Pts',(-61.5320731679598,13.2230256493634,
40.1322415082996));
#170659=CARTESIAN_POINT('Ctrl Pts',(-61.5229124097646,13.2402322400109,
40.1236936393009));
#170660=CARTESIAN_POINT('Ctrl Pts',(-61.5128929892896,13.2561876955043,
40.113394140767));
#170661=CARTESIAN_POINT('Ctrl Pts',(-61.5022873490354,13.2705955044757,
40.101665321223));
#170662=CARTESIAN_POINT('Ctrl Pts',(-61.4969845289083,13.2777994089614,
40.095800911451));
#170663=CARTESIAN_POINT('Ctrl Pts',(-61.4915351548246,13.2846164020264,
40.0895791707949));
#170664=CARTESIAN_POINT('Ctrl Pts',(-61.4859732907798,13.291009421645,40.0830403822906));
#170665=CARTESIAN_POINT('Ctrl Pts',(-61.4831923587574,13.2942059314543,
40.0797709880385));
#170666=CARTESIAN_POINT('Ctrl Pts',(-61.4803833043594,13.2972964479274,
40.0764223317514));
#170667=CARTESIAN_POINT('Ctrl Pts',(-61.4775503861046,13.300276338427,40.0729994484778));
#170668=CARTESIAN_POINT('Ctrl Pts',(-61.4747174678497,13.3032562289267,
40.0695765652042));
#170669=CARTESIAN_POINT('Ctrl Pts',(-61.4718606611377,13.3061253662371,
40.0660793733488));
#170670=CARTESIAN_POINT('Ctrl Pts',(-61.4689842762857,13.3088793779161,
40.0625130768817));
#170671=CARTESIAN_POINT('Ctrl Pts',(-61.468959746747,13.3089028638679,40.0624826638418));
#170672=CARTESIAN_POINT('Ctrl Pts',(-61.4689352159237,13.308926341439,40.0624522459912));
#170673=CARTESIAN_POINT('Ctrl Pts',(-61.4689106838181,13.3089498106273,
40.0624218233329));
#170674=CARTESIAN_POINT('Ctrl Pts',(-61.4563817793395,13.3209358677646,
40.04688452759));
#170675=CARTESIAN_POINT('Ctrl Pts',(-61.4435806031494,13.3308520539325,
40.0302263329239));
#170676=CARTESIAN_POINT('Ctrl Pts',(-61.4306829407564,13.3387946412837,
40.0127515884746));
#170677=CARTESIAN_POINT('Ctrl Pts',(-61.4173490879857,13.347005841665,39.9946858597717));
#170678=CARTESIAN_POINT('Ctrl Pts',(-61.4039112193234,13.3531077791297,
39.9757460620491));
#170679=CARTESIAN_POINT('Ctrl Pts',(-61.3905594167273,13.3571547734346,
39.9562444559129));
#170680=CARTESIAN_POINT('Ctrl Pts',(-61.3774615935119,13.3611247853922,
39.9371138113612));
#170681=CARTESIAN_POINT('Ctrl Pts',(-61.3644457143974,13.3631169881916,
39.9174410654354));
#170682=CARTESIAN_POINT('Ctrl Pts',(-61.3517005934288,13.3631357189476,
39.8975196504146));
#170683=CARTESIAN_POINT('Ctrl Pts',(-61.3432573976115,13.3631481274168,
39.8843224113775));
#170684=CARTESIAN_POINT('Ctrl Pts',(-61.3349332352347,13.362293512079,39.8710160447132));
#170685=CARTESIAN_POINT('Ctrl Pts',(-61.3267881959112,13.3605623192491,
39.8576902534424));
#170686=CARTESIAN_POINT('',(-60.9782752797347,13.2864868029,39.2875012672119));
#170687=CARTESIAN_POINT('',(-61.3267881959112,13.3605623192491,39.8576902534424));
#170688=CARTESIAN_POINT('',(-59.4519788726606,18.9827025415101,39.2875012672119));
#170689=CARTESIAN_POINT('Origin',(5.53234440788222E-15,0.,39.2875012672119));
#170690=CARTESIAN_POINT('',(-59.790837669791,19.0928077206416,39.8576902534424));
#170691=CARTESIAN_POINT('',(-59.4519788726606,18.9827025415101,39.2875012672119));
#170692=CARTESIAN_POINT('',(-59.8776671349984,19.4393816709761,40.1599502534424));
#170693=CARTESIAN_POINT('Ctrl Pts',(-59.790837669791,19.0928077206416,39.8576902534424));
#170694=CARTESIAN_POINT('Ctrl Pts',(-59.8025412685589,19.0966105891859,
39.8773836120367));
#170695=CARTESIAN_POINT('Ctrl Pts',(-59.81360381105,19.1022557829957,39.8969946442138));
#170696=CARTESIAN_POINT('Ctrl Pts',(-59.8238865403123,19.1096150844297,
39.916252528825));
#170697=CARTESIAN_POINT('Ctrl Pts',(-59.8343758896888,19.1171222629168,
39.9358973794073));
#170698=CARTESIAN_POINT('Ctrl Pts',(-59.8440546685621,19.1264133720528,
39.9551762199751));
#170699=CARTESIAN_POINT('Ctrl Pts',(-59.8527677431762,19.1374051938284,
39.9738152034255));
#170700=CARTESIAN_POINT('Ctrl Pts',(-59.8611423227401,19.1479699932922,
39.9917300792653));
#170701=CARTESIAN_POINT('Ctrl Pts',(-59.8686254222915,19.1601065286715,
40.0090551158128));
#170702=CARTESIAN_POINT('Ctrl Pts',(-59.8750609947979,19.173782305098,40.0255394551538));
#170703=CARTESIAN_POINT('Ctrl Pts',(-59.8800045782775,19.1842875619879,
40.0382021526151));
#170704=CARTESIAN_POINT('Ctrl Pts',(-59.8843297728484,19.1957019365555,
40.0503687782124));
#170705=CARTESIAN_POINT('Ctrl Pts',(-59.8879544940743,19.2080253553783,
40.0619155352442));
#170706=CARTESIAN_POINT('Ctrl Pts',(-59.8879639938222,19.2080576528613,
40.0619457972351));
#170707=CARTESIAN_POINT('Ctrl Pts',(-59.8879734883575,19.2080899573234,
40.0619760547305));
#170708=CARTESIAN_POINT('Ctrl Pts',(-59.8879829776791,19.2081222687615,
40.0620063077269));
#170709=CARTESIAN_POINT('Ctrl Pts',(-59.8890004259295,19.2115867120122,
40.06525004417));
#170710=CARTESIAN_POINT('Ctrl Pts',(-59.8899565588874,19.2151300442836,
40.0684393223556));
#170711=CARTESIAN_POINT('Ctrl Pts',(-59.8908500166521,19.2187475215463,
40.0715697951759));
#170712=CARTESIAN_POINT('Ctrl Pts',(-59.8958219059662,19.2388779600043,
40.0889901646422));
#170713=CARTESIAN_POINT('Ctrl Pts',(-59.8988577688781,19.261303194691,40.1045963098246));
#170714=CARTESIAN_POINT('Ctrl Pts',(-59.8997541019592,19.2851598349738,
40.1176634650729));
#170715=CARTESIAN_POINT('Ctrl Pts',(-59.9001563886588,19.2958670255072,
40.1235281853065));
#170716=CARTESIAN_POINT('Ctrl Pts',(-59.9001280009022,19.3068627531428,
40.1288820140921));
#170717=CARTESIAN_POINT('Ctrl Pts',(-59.8996517586311,19.3180708494663,
40.1336621774102));
#170718=CARTESIAN_POINT('Ctrl Pts',(-59.8994447901816,19.3229417365284,
40.1357395717319));
#170719=CARTESIAN_POINT('Ctrl Pts',(-59.8991531263708,19.3278525613651,
40.1377083672884));
#170720=CARTESIAN_POINT('Ctrl Pts',(-59.89877529055,19.3327969595688,40.1395632548792));
#170721=CARTESIAN_POINT('Ctrl Pts',(-59.8974528651771,19.3501023532819,
40.146055361447));
#170722=CARTESIAN_POINT('Ctrl Pts',(-59.8950748296128,19.3678190197505,
40.151152097463));
#170723=CARTESIAN_POINT('Ctrl Pts',(-59.8915778894432,19.3856740904737,
40.1546258197409));
#170724=CARTESIAN_POINT('Ctrl Pts',(-59.8898294193584,19.3946016258353,
40.1563626808798));
#170725=CARTESIAN_POINT('Ctrl Pts',(-59.8878012237013,19.4035637624461,
40.1576937882008));
#170726=CARTESIAN_POINT('Ctrl Pts',(-59.8854853982053,19.4125263941848,
40.1585906813668));
#170727=CARTESIAN_POINT('Ctrl Pts',(-59.8843274854572,19.4170077100542,
40.1590391279498));
#170728=CARTESIAN_POINT('Ctrl Pts',(-59.8830976653666,19.4214891497437,
40.1593790209175));
#170729=CARTESIAN_POINT('Ctrl Pts',(-59.8817949505649,19.4259664502059,
40.1596068022931));
#170730=CARTESIAN_POINT('Ctrl Pts',(-59.8804922357632,19.430443750668,40.1598345836687));
#170731=CARTESIAN_POINT('Ctrl Pts',(-59.8791166246274,19.434916911376,40.1599502506865));
#170732=CARTESIAN_POINT('Ctrl Pts',(-59.8776671349984,19.4393816709761,
40.1599502534424));
#170733=CARTESIAN_POINT('',(-59.868232155624,19.4684195516701,40.1599502534424));
#170734=CARTESIAN_POINT('Origin',(1.08121605342496E-16,-4.80251501969599E-17,
40.1599502534424));
#170735=CARTESIAN_POINT('',(-59.5942745858234,19.697766688185,39.8576902534424));
#170736=CARTESIAN_POINT('Ctrl Pts',(-59.868232155624,19.4684195516701,40.1599502534424));
#170737=CARTESIAN_POINT('Ctrl Pts',(-59.8670503242228,19.4720538382631,
40.1599502447858));
#170738=CARTESIAN_POINT('Ctrl Pts',(-59.8658263391017,19.4756634078265,
40.1598744685927));
#170739=CARTESIAN_POINT('Ctrl Pts',(-59.8645618637722,19.4792467723416,
40.1597246934279));
#170740=CARTESIAN_POINT('Ctrl Pts',(-59.8572547562675,19.4999541986783,
40.1588591777434));
#170741=CARTESIAN_POINT('Ctrl Pts',(-59.8485963666845,19.5197897600828,
40.1555254706017));
#170742=CARTESIAN_POINT('Ctrl Pts',(-59.8389090368086,19.5384593694394,
40.1500631826373));
#170743=CARTESIAN_POINT('Ctrl Pts',(-59.8350019138236,19.545989252366,40.1478601162475));
#170744=CARTESIAN_POINT('Ctrl Pts',(-59.830927553988,19.5533299158496,40.1453112228304));
#170745=CARTESIAN_POINT('Ctrl Pts',(-59.8267074486192,19.5604638837582,
40.1424401896328));
#170746=CARTESIAN_POINT('Ctrl Pts',(-59.8251504859513,19.5630958847954,
40.1413809526906));
#170747=CARTESIAN_POINT('Ctrl Pts',(-59.8235736599158,19.5656996197549,
40.1402777640512));
#170748=CARTESIAN_POINT('Ctrl Pts',(-59.8219780387742,19.5682741459749,
40.1391317641987));
#170749=CARTESIAN_POINT('Ctrl Pts',(-59.8189862491337,19.5731013826373,
40.1369830144753));
#170750=CARTESIAN_POINT('Ctrl Pts',(-59.8159283829424,19.577825932323,40.134683756585));
#170751=CARTESIAN_POINT('Ctrl Pts',(-59.8128114820619,19.5824415812279,
40.1322415082996));
#170752=CARTESIAN_POINT('Ctrl Pts',(-59.8019023289802,19.5985963523949,
40.1236936393009));
#170753=CARTESIAN_POINT('Ctrl Pts',(-59.7902699966955,19.6134170876086,
40.113394140767));
#170754=CARTESIAN_POINT('Ctrl Pts',(-59.7782164291174,19.6266373778172,
40.101665321223));
#170755=CARTESIAN_POINT('Ctrl Pts',(-59.7721896453284,19.6332475229215,
40.095800911451));
#170756=CARTESIAN_POINT('Ctrl Pts',(-59.7660575536769,19.6394575570865,
40.0895791707949));
#170757=CARTESIAN_POINT('Ctrl Pts',(-59.7598579055889,19.6452341819732,
40.0830403822906));
#170758=CARTESIAN_POINT('Ctrl Pts',(-59.7567580815449,19.6481224944165,
40.0797709880385));
#170759=CARTESIAN_POINT('Ctrl Pts',(-59.7536413685032,19.6509024545775,
40.0764223317514));
#170760=CARTESIAN_POINT('Ctrl Pts',(-59.7505124858963,19.6535699003335,
40.0729994484778));
#170761=CARTESIAN_POINT('Ctrl Pts',(-59.7473836032895,19.6562373460894,
40.0695765652042));
#170762=CARTESIAN_POINT('Ctrl Pts',(-59.7442425399495,19.65879214835,40.0660793733488));
#170763=CARTESIAN_POINT('Ctrl Pts',(-59.7410940396261,19.6612304091765,
40.0625130768817));
#170764=CARTESIAN_POINT('Ctrl Pts',(-59.7410671895124,19.6612512024348,
40.0624826638418));
#170765=CARTESIAN_POINT('Ctrl Pts',(-59.741040338997,19.6612719872241,40.0624522459912));
#170766=CARTESIAN_POINT('Ctrl Pts',(-59.7410134880827,19.6612927635425,
40.0624218233329));
#170767=CARTESIAN_POINT('Ctrl Pts',(-59.7273003341234,19.6719035326708,
40.0468845275932));
#170768=CARTESIAN_POINT('Ctrl Pts',(-59.7135327604172,19.6804273096567,
40.030226332931));
#170769=CARTESIAN_POINT('Ctrl Pts',(-59.6998755263211,19.686978213853,40.0127515884857));
#170770=CARTESIAN_POINT('Ctrl Pts',(-59.6857564136365,19.6937506652793,
39.994685859787));
#170771=CARTESIAN_POINT('Ctrl Pts',(-59.6717543328814,19.6984145359315,
39.9757460620688));
#170772=CARTESIAN_POINT('Ctrl Pts',(-59.658052646764,19.7010437169722,39.9562444559372));
#170773=CARTESIAN_POINT('Ctrl Pts',(-59.6446115955477,19.7036228854571,
39.9371138113893));
#170774=CARTESIAN_POINT('Ctrl Pts',(-59.6314587768857,19.7042436449212,
39.9174410654674));
#170775=CARTESIAN_POINT('Ctrl Pts',(-59.6187815171278,19.7029300451618,
39.8975196504504));
#170776=CARTESIAN_POINT('Ctrl Pts',(-59.6103832769743,19.702059831373,39.8843224114016));
#170777=CARTESIAN_POINT('Ctrl Pts',(-59.6021940468503,19.7003397858055,
39.8710160447252));
#170778=CARTESIAN_POINT('Ctrl Pts',(-59.5942745858234,19.697766688185,39.8576902534424));
#170779=CARTESIAN_POINT('',(-59.255413859757,19.5876674457083,39.2875012672119));
#170780=CARTESIAN_POINT('',(-59.5942745858234,19.697766688185,39.8576902534424));
#170781=CARTESIAN_POINT('',(-57.1420619865019,25.093137300575,39.2875012672119));
#170782=CARTESIAN_POINT('Origin',(5.53234440788222E-15,0.,39.2875012672119));
#170783=CARTESIAN_POINT('',(-57.4675553545138,25.2380597013435,39.8576902534424));
#170784=CARTESIAN_POINT('',(-57.1420619865019,25.093137300575,39.2875012672119));
#170785=CARTESIAN_POINT('',(-57.5176823163886,25.5918112338799,40.1599502534424));
#170786=CARTESIAN_POINT('Ctrl Pts',(-57.4675553545138,25.2380597013435,
39.8576902534424));
#170787=CARTESIAN_POINT('Ctrl Pts',(-57.4787973317384,25.2430650965698,
39.8773836120369));
#170788=CARTESIAN_POINT('Ctrl Pts',(-57.4892091890305,25.2498357159837,
39.8969946442142));
#170789=CARTESIAN_POINT('Ctrl Pts',(-57.4986663319565,25.2582295402824,
39.9162525288255));
#170790=CARTESIAN_POINT('Ctrl Pts',(-57.508313505749,25.2667920292314,39.9358973794082));
#170791=CARTESIAN_POINT('Ctrl Pts',(-57.5169680778991,25.2770439485816,
39.9551762199763));
#170792=CARTESIAN_POINT('Ctrl Pts',(-57.5244844631401,25.2888863203075,
39.973815203427));
#170793=CARTESIAN_POINT('Ctrl Pts',(-57.5317088436283,25.3002686266273,
39.9917300792673));
#170794=CARTESIAN_POINT('Ctrl Pts',(-57.5378823365848,25.313120873693,40.0090551158152));
#170795=CARTESIAN_POINT('Ctrl Pts',(-57.5428531464578,25.3273944332903,
40.0255394551565));
#170796=CARTESIAN_POINT('Ctrl Pts',(-57.5466715501105,25.3383588864673,
40.0382021526169));
#170797=CARTESIAN_POINT('Ctrl Pts',(-57.54977992378,25.3501628378378,40.0503687782133));
#170798=CARTESIAN_POINT('Ctrl Pts',(-57.5520966403719,25.3627976342214,
40.0619155352442));
#170799=CARTESIAN_POINT('Ctrl Pts',(-57.5521027120729,25.3628307477695,
40.0619457972351));
#170800=CARTESIAN_POINT('Ctrl Pts',(-57.5521087778604,25.3628638677135,
40.0619760547305));
#170801=CARTESIAN_POINT('Ctrl Pts',(-57.5521148377335,25.3628969940505,
40.062006307727));
#170802=CARTESIAN_POINT('Ctrl Pts',(-57.5527645793668,25.3664488110206,
40.06525004417));
#170803=CARTESIAN_POINT('Ctrl Pts',(-57.5533450954511,25.3700726756558,
40.0684393223557));
#170804=CARTESIAN_POINT('Ctrl Pts',(-57.5538555294215,25.3737637277667,
40.0715697951759));
#170805=CARTESIAN_POINT('Ctrl Pts',(-57.5566959784093,25.3943035935289,
40.0889901646446));
#170806=CARTESIAN_POINT('Ctrl Pts',(-57.557371135226,25.4169233145218,40.1045963098288));
#170807=CARTESIAN_POINT('Ctrl Pts',(-57.5557688601525,25.4407429579562,
40.1176634650783));
#170808=CARTESIAN_POINT('Ctrl Pts',(-57.555049736911,25.4514335437868,40.1235281853097));
#170809=CARTESIAN_POINT('Ctrl Pts',(-57.5538721381535,25.4623660683441,
40.1288820140936));
#170810=CARTESIAN_POINT('Ctrl Pts',(-57.552226939703,25.473462984667,40.1336621774101));
#170811=CARTESIAN_POINT('Ctrl Pts',(-57.551511958709,25.4782855544062,40.1357395717319));
#170812=CARTESIAN_POINT('Ctrl Pts',(-57.5507085716895,25.4831389900607,
40.1377083672884));
#170813=CARTESIAN_POINT('Ctrl Pts',(-57.5498159753468,25.488016807736,40.1395632548792));
#170814=CARTESIAN_POINT('Ctrl Pts',(-57.5466918881474,25.5050891695996,
40.146055361447));
#170815=CARTESIAN_POINT('Ctrl Pts',(-57.5424749837905,25.5224602099125,
40.1511520974629));
#170816=CARTESIAN_POINT('Ctrl Pts',(-57.5371308371209,25.539851938908,40.1546258197408));
#170817=CARTESIAN_POINT('Ctrl Pts',(-57.534458763786,25.5485478034057,40.1563626808798));
#170818=CARTESIAN_POINT('Ctrl Pts',(-57.5315048804294,25.5572488403192,
40.1576937882008));
#170819=CARTESIAN_POINT('Ctrl Pts',(-57.5282648911453,25.5659203041432,
40.1585906813668));
#170820=CARTESIAN_POINT('Ctrl Pts',(-57.5266448965032,25.5702560360552,
40.1590391279498));
#170821=CARTESIAN_POINT('Ctrl Pts',(-57.5249533754917,25.5745843747451,
40.1593790209175));
#170822=CARTESIAN_POINT('Ctrl Pts',(-57.5231897917611,25.5789009773105,
40.1596068022931));
#170823=CARTESIAN_POINT('Ctrl Pts',(-57.5214262080304,25.583217579876,40.1598345836687));
#170824=CARTESIAN_POINT('Ctrl Pts',(-57.5195905600217,25.5875224456234,
40.1599502506865));
#170825=CARTESIAN_POINT('Ctrl Pts',(-57.5176823163886,25.5918112338799,
40.1599502534424));
#170826=CARTESIAN_POINT('',(-57.505263737773,25.6197038181302,40.1599502534424));
#170827=CARTESIAN_POINT('Origin',(1.02291912287982E-16,-6.32120198238069E-17,
40.1599502534424));
#170828=CARTESIAN_POINT('',(-57.2088336324697,25.8191582032625,39.8576902534424));
#170829=CARTESIAN_POINT('Ctrl Pts',(-57.505263737773,25.6197038181302,40.1599502534424));
#170830=CARTESIAN_POINT('Ctrl Pts',(-57.5037084941752,25.6231946607008,
40.1599502447858));
#170831=CARTESIAN_POINT('Ctrl Pts',(-57.5021139114131,25.6266565153807,
40.1598744685927));
#170832=CARTESIAN_POINT('Ctrl Pts',(-57.5004817994257,25.630088076187,40.1597246934279));
#170833=CARTESIAN_POINT('Ctrl Pts',(-57.4910502055662,25.6499182643595,
40.1588591777433));
#170834=CARTESIAN_POINT('Ctrl Pts',(-57.4803658667941,25.6687401163279,
40.155525470601));
#170835=CARTESIAN_POINT('Ctrl Pts',(-57.4687800995474,25.6862948499077,
40.1500631826354));
#170836=CARTESIAN_POINT('Ctrl Pts',(-57.4641072931013,25.6933750777842,
40.147860116246));
#170837=CARTESIAN_POINT('Ctrl Pts',(-57.4592879447633,25.7002496417706,
40.1453112228295));
#170838=CARTESIAN_POINT('Ctrl Pts',(-57.4543452548722,25.7069034079255,
40.1424401896328));
#170839=CARTESIAN_POINT('Ctrl Pts',(-57.452521702385,25.7093582436706,40.1413809526906));
#170840=CARTESIAN_POINT('Ctrl Pts',(-57.4506813499535,25.7117828918952,
40.1402777640512));
#170841=CARTESIAN_POINT('Ctrl Pts',(-57.4488253585221,25.7141765267653,
40.1391317641987));
#170842=CARTESIAN_POINT('Ctrl Pts',(-57.4453453745881,25.7186645921467,
40.1369830144753));
#170843=CARTESIAN_POINT('Ctrl Pts',(-57.4418104097894,25.723043626201,40.134683756585));
#170844=CARTESIAN_POINT('Ctrl Pts',(-57.4382281169311,25.727308185239,40.1322415082996));
#170845=CARTESIAN_POINT('Ctrl Pts',(-57.4256900919268,25.7422341418722,
40.1236936393009));
#170846=CARTESIAN_POINT('Ctrl Pts',(-57.4125722940991,25.7557577777296,
40.113394140767));
#170847=CARTESIAN_POINT('Ctrl Pts',(-57.399202860606,25.7676457049094,40.101665321223));
#170848=CARTESIAN_POINT('Ctrl Pts',(-57.3925181438594,25.7735896684993,
40.095800911451));
#170849=CARTESIAN_POINT('Ctrl Pts',(-57.3857705191195,25.7791247053304,
40.0895791707949));
#170850=CARTESIAN_POINT('Ctrl Pts',(-57.3790010116301,25.7842216455741,
40.0830403822906));
#170851=CARTESIAN_POINT('Ctrl Pts',(-57.3756162578855,25.786770115696,40.0797709880385));
#170852=CARTESIAN_POINT('Ctrl Pts',(-57.3722260335603,25.7892090617196,
40.0764223317514));
#170853=CARTESIAN_POINT('Ctrl Pts',(-57.368835467294,25.791534837638,40.0729994484778));
#170854=CARTESIAN_POINT('Ctrl Pts',(-57.3654449010277,25.7938606135564,
40.0695765652042));
#170855=CARTESIAN_POINT('Ctrl Pts',(-57.3620539952072,25.7960730898189,
40.0660793733488));
#170856=CARTESIAN_POINT('Ctrl Pts',(-57.3586678750408,25.7981688856971,
40.0625130768817));
#170857=CARTESIAN_POINT('Ctrl Pts',(-57.3586389985274,25.7981867584466,
40.0624826638418));
#170858=CARTESIAN_POINT('Ctrl Pts',(-57.3586101224999,25.7982046227315,
40.0624522459912));
#170859=CARTESIAN_POINT('Ctrl Pts',(-57.3585812469611,25.7982224785502,
40.0624218233329));
#170860=CARTESIAN_POINT('Ctrl Pts',(-57.3438340877015,25.807341705866,40.0468845275918));
#170861=CARTESIAN_POINT('Ctrl Pts',(-57.3292509568938,25.8143796853877,
40.0302263329279));
#170862=CARTESIAN_POINT('Ctrl Pts',(-57.3149837826051,25.819467133353,40.0127515884809));
#170863=CARTESIAN_POINT('Ctrl Pts',(-57.3002341019555,25.8247266354303,
39.9946858597802));
#170864=CARTESIAN_POINT('Ctrl Pts',(-57.2858212188304,25.8279013409269,
39.97574606206));
#170865=CARTESIAN_POINT('Ctrl Pts',(-57.2719197677283,25.8290839028441,
39.9562444559263));
#170866=CARTESIAN_POINT('Ctrl Pts',(-57.2582827514776,25.8302439699452,
39.9371138113765));
#170867=CARTESIAN_POINT('Ctrl Pts',(-57.2451370982986,25.8294864849006,
39.9174410654526));
#170868=CARTESIAN_POINT('Ctrl Pts',(-57.2326665944596,25.8268549466959,
39.8975196504337));
#170869=CARTESIAN_POINT('Ctrl Pts',(-57.2244053228583,25.8251116448919,
39.8843224113903));
#170870=CARTESIAN_POINT('Ctrl Pts',(-57.2164407479171,25.8225450142746,
39.8710160447196));
#170871=CARTESIAN_POINT('Ctrl Pts',(-57.2088336324697,25.8191582032625,
39.8576902534424));
#170872=CARTESIAN_POINT('',(-56.8833377255392,25.6742415049984,39.2875012672119));
#170873=CARTESIAN_POINT('',(-57.2088336324697,25.8191582032625,39.8576902534424));
#170874=CARTESIAN_POINT('',(-54.2060847114739,30.9286463962983,39.2875012672119));
#170875=CARTESIAN_POINT('Origin',(5.53234440788222E-15,0.,39.2875012672119));
#170876=CARTESIAN_POINT('',(-54.5146464769135,31.1067982185539,39.8576902534424));
#170877=CARTESIAN_POINT('',(-54.2060847114739,30.9286463962983,39.2875012672119));
#170878=CARTESIAN_POINT('',(-54.5275217339717,31.4638515574745,40.1599502534424));
#170879=CARTESIAN_POINT('Ctrl Pts',(-54.5146464769135,31.1067982185539,
39.8576902534424));
#170880=CARTESIAN_POINT('Ctrl Pts',(-54.5253036631391,31.1129513003049,
39.8773836120363));
#170881=CARTESIAN_POINT('Ctrl Pts',(-54.5349507607445,31.1207731649995,
39.896994644213));
#170882=CARTESIAN_POINT('Ctrl Pts',(-54.5434787028969,31.1301095476671,
39.9162525288237));
#170883=CARTESIAN_POINT('Ctrl Pts',(-54.5521780046501,31.1396335346567,
39.9358973794056));
#170884=CARTESIAN_POINT('Ctrl Pts',(-54.559713548773,31.1507339420464,39.955176219973));
#170885=CARTESIAN_POINT('Ctrl Pts',(-54.5659508935512,31.1632971162187,
39.973815203423));
#170886=CARTESIAN_POINT('Ctrl Pts',(-54.571945923139,31.175372222463,39.9917300792622));
#170887=CARTESIAN_POINT('Ctrl Pts',(-54.5767421714199,31.1887993693051,
40.0090551158092));
#170888=CARTESIAN_POINT('Ctrl Pts',(-54.5801937574264,31.2035143279653,
40.0255394551498));
#170889=CARTESIAN_POINT('Ctrl Pts',(-54.582845146024,31.2148178485882,40.0382021526126));
#170890=CARTESIAN_POINT('Ctrl Pts',(-54.5847026428005,31.2268820502029,
40.0503687782112));
#170891=CARTESIAN_POINT('Ctrl Pts',(-54.585685972327,31.2396897946774,40.0619155352442));
#170892=CARTESIAN_POINT('Ctrl Pts',(-54.5856885494583,31.2397233614916,
40.0619457972351));
#170893=CARTESIAN_POINT('Ctrl Pts',(-54.5856911200399,31.2397569340486,
40.0619760547305));
#170894=CARTESIAN_POINT('Ctrl Pts',(-54.5856936840714,31.2397905123452,
40.0620063077269));
#170895=CARTESIAN_POINT('Ctrl Pts',(-54.5859686003823,31.2433907885848,
40.06525004417));
#170896=CARTESIAN_POINT('Ctrl Pts',(-54.5861671393374,31.2470554817645,
40.0684393223557));
#170897=CARTESIAN_POINT('Ctrl Pts',(-54.5862889570921,31.2507796687843,
40.0715697951759));
#170898=CARTESIAN_POINT('Ctrl Pts',(-54.5869668451992,31.2715039227786,
40.0889901646431));
#170899=CARTESIAN_POINT('Ctrl Pts',(-54.5852738987616,31.2940703036755,
40.1045963098261));
#170900=CARTESIAN_POINT('Ctrl Pts',(-54.5811905703956,31.3175919772574,
40.1176634650748));
#170901=CARTESIAN_POINT('Ctrl Pts',(-54.5793579160779,31.328148830095,40.1235281853076));
#170902=CARTESIAN_POINT('Ctrl Pts',(-54.5770440083377,31.3388983725524,
40.1288820140926));
#170903=CARTESIAN_POINT('Ctrl Pts',(-54.5742478788457,31.349762528743,40.1336621774101));
#170904=CARTESIAN_POINT('Ctrl Pts',(-54.5730327187886,31.354483944076,40.1357395717319));
#170905=CARTESIAN_POINT('Ctrl Pts',(-54.5717264106366,31.3592268152916,
40.1377083672883));
#170906=CARTESIAN_POINT('Ctrl Pts',(-54.5703288332444,31.3639846100473,
40.1395632548791));
#170907=CARTESIAN_POINT('Ctrl Pts',(-54.5654373123716,31.3806368916922,
40.1460553614469));
#170908=CARTESIAN_POINT('Ctrl Pts',(-54.5594277405088,31.3974719850966,
40.1511520974629));
#170909=CARTESIAN_POINT('Ctrl Pts',(-54.5522949389283,31.414209824942,40.1546258197408));
#170910=CARTESIAN_POINT('Ctrl Pts',(-54.548728538138,31.4225787448647,40.1563626808798));
#170911=CARTESIAN_POINT('Ctrl Pts',(-54.5448813304462,31.4309233516996,
40.1576937882008));
#170912=CARTESIAN_POINT('Ctrl Pts',(-54.5407526753745,31.4392086412367,
40.1585906813668));
#170913=CARTESIAN_POINT('Ctrl Pts',(-54.5386883478386,31.4433512860052,
40.1590391279498));
#170914=CARTESIAN_POINT('Ctrl Pts',(-54.5365536585645,31.4474791015109,
40.1593790209175));
#170915=CARTESIAN_POINT('Ctrl Pts',(-54.5343485280974,31.4515877125786,
40.1596068022931));
#170916=CARTESIAN_POINT('Ctrl Pts',(-54.5321433976302,31.4556963236464,
40.1598345836687));
#170917=CARTESIAN_POINT('Ctrl Pts',(-54.5298678244922,31.4597857294234,
40.1599502506865));
#170918=CARTESIAN_POINT('Ctrl Pts',(-54.5275217339717,31.4638515574745,
40.1599502534424));
#170919=CARTESIAN_POINT('',(-54.5122556166608,31.4902932482912,40.1599502534424));
#170920=CARTESIAN_POINT('Origin',(9.49066947580418E-17,-7.7706325333499E-17,
40.1599502534424));
#170921=CARTESIAN_POINT('',(-54.1966007261205,31.6576696180589,39.8576902534424));
#170922=CARTESIAN_POINT('Ctrl Pts',(-54.5122556166608,31.4902932482912,
40.1599502534424));
#170923=CARTESIAN_POINT('Ctrl Pts',(-54.5103440004408,31.4936024004376,
40.1599502447858));
#170924=CARTESIAN_POINT('Ctrl Pts',(-54.5083962906202,31.4968786114297,
40.1598744685927));
#170925=CARTESIAN_POINT('Ctrl Pts',(-54.5064144237353,31.5001207716289,
40.1597246934279));
#170926=CARTESIAN_POINT('Ctrl Pts',(-54.494961678038,31.5188564579432,40.1588591777434));
#170927=CARTESIAN_POINT('Ctrl Pts',(-54.4823684499298,31.536458384324,40.1555254706011));
#170928=CARTESIAN_POINT('Ctrl Pts',(-54.4690111814043,31.5527059087901,
40.1500631826356));
#170929=CARTESIAN_POINT('Ctrl Pts',(-54.4636238877412,31.5592589091608,
40.1478601162462));
#170930=CARTESIAN_POINT('Ctrl Pts',(-54.4581123526882,31.565592054491,40.1453112228296));
#170931=CARTESIAN_POINT('Ctrl Pts',(-54.4525012314182,31.5716927188402,
40.1424401896328));
#170932=CARTESIAN_POINT('Ctrl Pts',(-54.4504310683343,31.573943493599,40.1413809526906));
#170933=CARTESIAN_POINT('Ctrl Pts',(-54.4483473527931,31.5761624901355,
40.1402777640512));
#170934=CARTESIAN_POINT('Ctrl Pts',(-54.4462513257023,31.5783490084911,
40.1391317641987));
#170935=CARTESIAN_POINT('Ctrl Pts',(-54.4423212749071,31.5824487304079,
40.1369830144753));
#170936=CARTESIAN_POINT('Ctrl Pts',(-54.4383479413152,31.5864342712174,
40.1346837565849));
#170937=CARTESIAN_POINT('Ctrl Pts',(-54.4343395048292,31.5903010169874,
40.1322415082996));
#170938=CARTESIAN_POINT('Ctrl Pts',(-54.4203099771281,31.6038346271822,
40.1236936393008));
#170939=CARTESIAN_POINT('Ctrl Pts',(-54.4058504350955,31.6159129958991,
40.113394140767));
#170940=CARTESIAN_POINT('Ctrl Pts',(-54.3913116139983,31.6263383134321,
40.101665321223));
#170941=CARTESIAN_POINT('Ctrl Pts',(-54.3840422034498,31.6315509721986,
40.095800911451));
#170942=CARTESIAN_POINT('Ctrl Pts',(-54.3767529740101,31.6363503686741,
40.0895791707949));
#170943=CARTESIAN_POINT('Ctrl Pts',(-54.36948777526,31.6407117811309,40.0830403822906));
#170944=CARTESIAN_POINT('Ctrl Pts',(-54.365855175885,31.6428924873593,40.0797709880385));
#170945=CARTESIAN_POINT('Ctrl Pts',(-54.3622285842836,31.6449636976426,
40.0764223317514));
#170946=CARTESIAN_POINT('Ctrl Pts',(-54.3586134821114,31.6469223220357,
40.0729994484778));
#170947=CARTESIAN_POINT('Ctrl Pts',(-54.3549983799392,31.6488809464288,
40.0695765652042));
#170948=CARTESIAN_POINT('Ctrl Pts',(-54.3513947831118,31.6507268563404,
40.0660793733488));
#170949=CARTESIAN_POINT('Ctrl Pts',(-54.3478081421435,31.652457225292,40.0625130768817));
#170950=CARTESIAN_POINT('Ctrl Pts',(-54.3477775556076,31.6524719817152,
40.0624826638418));
#170951=CARTESIAN_POINT('Ctrl Pts',(-54.3477469704398,31.6524867297709,
40.0624522459912));
#170952=CARTESIAN_POINT('Ctrl Pts',(-54.3477163866429,31.6525014694579,
40.0624218233329));
#170953=CARTESIAN_POINT('Ctrl Pts',(-54.3320967950451,31.6600292427984,
40.0468845275896));
#170954=CARTESIAN_POINT('Ctrl Pts',(-54.3168578829676,31.6655043152796,
40.0302263329231));
#170955=CARTESIAN_POINT('Ctrl Pts',(-54.3021370826326,31.6690725678691,
40.0127515884733));
#170956=CARTESIAN_POINT('Ctrl Pts',(-54.2869184346054,31.6727614963917,
39.9946858597701));
#170957=CARTESIAN_POINT('Ctrl Pts',(-54.2722526596735,31.6744122539946,
39.9757460620471));
#170958=CARTESIAN_POINT('Ctrl Pts',(-54.2583037507936,31.674135240392,39.9562444559105));
#170959=CARTESIAN_POINT('Ctrl Pts',(-54.2446201795125,31.6738634961709,
39.9371138113587));
#170960=CARTESIAN_POINT('Ctrl Pts',(-54.2316257183442,31.6717360657818,
39.9174410654328));
#170961=CARTESIAN_POINT('Ctrl Pts',(-54.2194985998742,31.6678154208145,
39.8975196504119));
#170962=CARTESIAN_POINT('Ctrl Pts',(-54.2114648090465,31.6652181309756,
39.8843224113757));
#170963=CARTESIAN_POINT('Ctrl Pts',(-54.203812150839,31.6618330358514,39.8710160447123));
#170964=CARTESIAN_POINT('Ctrl Pts',(-54.1966007261205,31.6576696180589,
39.8576902534424));
#170965=CARTESIAN_POINT('',(-53.8880358395968,31.4795232016794,39.2875012672119));
#170966=CARTESIAN_POINT('',(-54.1966007261205,31.6576696180589,39.8576902534424));
#170967=CARTESIAN_POINT('',(-50.6762142289945,36.4252947698683,39.2875012672119));
#170968=CARTESIAN_POINT('Origin',(5.53234440788222E-15,0.,39.2875012672119));
#170969=CARTESIAN_POINT('',(-50.964463724589,36.6347241449659,39.8576902534424));
#170970=CARTESIAN_POINT('',(-50.6762142289945,36.4252947698683,39.2875012672119));
#170971=CARTESIAN_POINT('',(-50.9399462128199,36.9911673391712,40.1599502534424));
#170972=CARTESIAN_POINT('Ctrl Pts',(-50.964463724589,36.6347241449659,39.8576902534424));
#170973=CARTESIAN_POINT('Ctrl Pts',(-50.9744193574544,36.6419574987908,
39.8773836120382));
#170974=CARTESIAN_POINT('Ctrl Pts',(-50.9831959997541,36.6507449107809,
39.8969946442167));
#170975=CARTESIAN_POINT('Ctrl Pts',(-50.9907013072149,36.6609215604566,
39.9162525288292));
#170976=CARTESIAN_POINT('Ctrl Pts',(-50.9983574255591,36.671302698694,39.9358973794129));
#170977=CARTESIAN_POINT('Ctrl Pts',(-51.0046913806569,36.6831299757391,
39.9551762199819));
#170978=CARTESIAN_POINT('Ctrl Pts',(-51.0095813473178,36.696276307595,39.9738152034334));
#170979=CARTESIAN_POINT('Ctrl Pts',(-51.0142813432067,36.7089119163756,
39.9917300792743));
#170980=CARTESIAN_POINT('Ctrl Pts',(-51.0176477981118,36.7227668523667,
40.0090551158226));
#170981=CARTESIAN_POINT('Ctrl Pts',(-51.0195423439525,36.7377619899269,
40.0255394551644));
#170982=CARTESIAN_POINT('Ctrl Pts',(-51.0209976683246,36.7492807342529,
40.0382021526219));
#170983=CARTESIAN_POINT('Ctrl Pts',(-51.0215839370835,36.761473008188,40.0503687782156));
#170984=CARTESIAN_POINT('Ctrl Pts',(-51.0212231059802,36.7743133764175,
40.0619155352442));
#170985=CARTESIAN_POINT('Ctrl Pts',(-51.0212221603062,36.7743470287327,
40.0619457972351));
#170986=CARTESIAN_POINT('Ctrl Pts',(-51.0212212075181,36.7743806860747,
40.0619760547305));
#170987=CARTESIAN_POINT('Ctrl Pts',(-51.0212202476158,36.7744143484402,
40.062006307727));
#170988=CARTESIAN_POINT('Ctrl Pts',(-51.0211173265637,36.7780236385693,
40.06525004417));
#170989=CARTESIAN_POINT('Ctrl Pts',(-51.0209317131552,36.7816890091483,
40.0684393223557));
#170990=CARTESIAN_POINT('Ctrl Pts',(-51.0206635800334,36.7854055281046,
40.0715697951759));
#170991=CARTESIAN_POINT('Ctrl Pts',(-51.0191714801765,36.8060871110647,
40.0889901646393));
#170992=CARTESIAN_POINT('Ctrl Pts',(-51.0151289787614,36.8283529098713,
40.1045963098193));
#170993=CARTESIAN_POINT('Ctrl Pts',(-51.0086093349049,36.8513189052198,
40.1176634650663));
#170994=CARTESIAN_POINT('Ctrl Pts',(-51.0056832284544,36.8616263619782,
40.1235281853025));
#170995=CARTESIAN_POINT('Ctrl Pts',(-51.0022583633875,36.8720751481021,
40.1288820140903));
#170996=CARTESIAN_POINT('Ctrl Pts',(-50.9983419378322,36.8825875141945,
40.1336621774101));
#170997=CARTESIAN_POINT('Ctrl Pts',(-50.9966399122598,36.8871560463069,
40.1357395717319));
#170998=CARTESIAN_POINT('Ctrl Pts',(-50.994844995161,36.891736389194,40.1377083672883));
#170999=CARTESIAN_POINT('Ctrl Pts',(-50.9929577488696,36.8963220336351,
40.1395632548791));
#171000=CARTESIAN_POINT('Ctrl Pts',(-50.9863523868498,36.912371789179,40.1460553614469));
#171001=CARTESIAN_POINT('Ctrl Pts',(-50.9786159896079,36.9284864868685,
40.1511520974629));
#171002=CARTESIAN_POINT('Ctrl Pts',(-50.9697726815833,36.9443870542879,
40.1546258197409));
#171003=CARTESIAN_POINT('Ctrl Pts',(-50.9653510275709,36.9523373379977,
40.1563626808798));
#171004=CARTESIAN_POINT('Ctrl Pts',(-50.9606526463563,36.9602340894953,
40.1576937882008));
#171005=CARTESIAN_POINT('Ctrl Pts',(-50.955680559906,36.9680424293794,40.1585906813668));
#171006=CARTESIAN_POINT('Ctrl Pts',(-50.9531945166809,36.9719465993214,
40.1590391279498));
#171007=CARTESIAN_POINT('Ctrl Pts',(-50.9506400472466,36.9758286664324,
40.1593790209175));
#171008=CARTESIAN_POINT('Ctrl Pts',(-50.9480175299137,36.9796842711998,
40.1596068022931));
#171009=CARTESIAN_POINT('Ctrl Pts',(-50.9453950125809,36.9835398759672,
40.1598345836687));
#171010=CARTESIAN_POINT('Ctrl Pts',(-50.9427044459691,36.9873690173883,
40.1599502506865));
#171011=CARTESIAN_POINT('Ctrl Pts',(-50.9399462128199,36.9911673391712,
40.1599502534424));
#171012=CARTESIAN_POINT('',(-50.9219998155897,37.0158684358564,40.1599502534424));
#171013=CARTESIAN_POINT('Origin',(8.60468667414046E-17,-9.13492640817437E-17,
40.1599502534424));
#171014=CARTESIAN_POINT('',(-50.5905785208481,37.1493329797265,39.8576902534424));
#171015=CARTESIAN_POINT('Ctrl Pts',(-50.9219998155897,37.0158684358564,
40.1599502534424));
#171016=CARTESIAN_POINT('Ctrl Pts',(-50.9197527708147,37.0189596418153,
40.1599502447858));
#171017=CARTESIAN_POINT('Ctrl Pts',(-50.917473273452,37.0220143142663,40.1598744685927));
#171018=CARTESIAN_POINT('Ctrl Pts',(-50.915163365418,37.0250315520728,40.1597246934279));
#171019=CARTESIAN_POINT('Ctrl Pts',(-50.9018149465622,37.0424674644279,
40.1588591777434));
#171020=CARTESIAN_POINT('Ctrl Pts',(-50.8874508031613,37.0586566148313,
40.1555254706016));
#171021=CARTESIAN_POINT('Ctrl Pts',(-50.8724683783873,37.0734189189051,
40.1500631826369));
#171022=CARTESIAN_POINT('Ctrl Pts',(-50.8664256218229,37.0793728957276,
40.1478601162472));
#171023=CARTESIAN_POINT('Ctrl Pts',(-50.8602822855854,37.0850952351368,
40.1453112228302));
#171024=CARTESIAN_POINT('Ctrl Pts',(-50.8540642095543,37.0905759575259,
40.1424401896328));
#171025=CARTESIAN_POINT('Ctrl Pts',(-50.8517701170137,37.0925980113392,
40.1413809526906));
#171026=CARTESIAN_POINT('Ctrl Pts',(-50.8494658679863,37.094587044397,40.1402777640512));
#171027=CARTESIAN_POINT('Ctrl Pts',(-50.8471527697476,37.0965424902856,
40.1391317641987));
#171028=CARTESIAN_POINT('Ctrl Pts',(-50.8428157105501,37.1002089513266,
40.1369830144753));
#171029=CARTESIAN_POINT('Ctrl Pts',(-50.8384475408392,37.1037573324721,
40.134683756585));
#171030=CARTESIAN_POINT('Ctrl Pts',(-50.8340568779945,37.1071839000981,
40.1322415082996));
#171031=CARTESIAN_POINT('Ctrl Pts',(-50.818689558038,37.1191768867893,40.1236936393009));
#171032=CARTESIAN_POINT('Ctrl Pts',(-50.8030466935688,37.1296776552303,
40.113394140767));
#171033=CARTESIAN_POINT('Ctrl Pts',(-50.787497775234,37.1385261411561,40.101665321223));
#171034=CARTESIAN_POINT('Ctrl Pts',(-50.7797233160666,37.142950384119,40.095800911451));
#171035=CARTESIAN_POINT('Ctrl Pts',(-50.7719723442504,37.1469615570466,
40.0895791707949));
#171036=CARTESIAN_POINT('Ctrl Pts',(-50.7642910532774,37.1505396571689,
40.0830403822907));
#171037=CARTESIAN_POINT('Ctrl Pts',(-50.760450407791,37.1523287072301,40.0797709880385));
#171038=CARTESIAN_POINT('Ctrl Pts',(-50.7566271826097,37.1540094891598,
40.0764223317514));
#171039=CARTESIAN_POINT('Ctrl Pts',(-50.7528271523476,37.155579502929,40.0729994484778));
#171040=CARTESIAN_POINT('Ctrl Pts',(-50.7490271220855,37.1571495166981,
40.0695765652042));
#171041=CARTESIAN_POINT('Ctrl Pts',(-50.7452503160122,37.1586086360834,
40.0660793733488));
#171042=CARTESIAN_POINT('Ctrl Pts',(-50.7415024502309,37.1599546198241,
40.0625130768817));
#171043=CARTESIAN_POINT('Ctrl Pts',(-50.7414704887851,37.1599660982465,
40.0624826638418));
#171044=CARTESIAN_POINT('Ctrl Pts',(-50.7414385295744,37.1599775684902,
40.0624522459912));
#171045=CARTESIAN_POINT('Ctrl Pts',(-50.7414065726019,37.1599890305544,
40.0624218233329));
#171046=CARTESIAN_POINT('Ctrl Pts',(-50.7250856801842,37.1658428740575,
40.0468845275916));
#171047=CARTESIAN_POINT('Ctrl Pts',(-50.7093579475509,37.1696950534571,
40.0302263329275));
#171048=CARTESIAN_POINT('Ctrl Pts',(-50.6943448053425,37.1717050161486,
40.0127515884802));
#171049=CARTESIAN_POINT('Ctrl Pts',(-50.6788239286337,37.1737829544436,
39.9946858597794));
#171050=CARTESIAN_POINT('Ctrl Pts',(-50.6640659431975,37.173891678108,39.975746062059));
#171051=CARTESIAN_POINT('Ctrl Pts',(-50.6502224037074,37.1721581240064,
39.956244455925));
#171052=CARTESIAN_POINT('Ctrl Pts',(-50.6366421974681,37.1704575457516,
39.937113811375));
#171053=CARTESIAN_POINT('Ctrl Pts',(-50.6239412983474,37.1669834785932,
39.917441065451));
#171054=CARTESIAN_POINT('Ctrl Pts',(-50.6122904324949,37.1618166822733,
39.8975196504319));
#171055=CARTESIAN_POINT('Ctrl Pts',(-50.604572142325,37.1583938608496,39.8843224113891));
#171056=CARTESIAN_POINT('Ctrl Pts',(-50.5973152449672,37.1542273890268,
39.871016044719));
#171057=CARTESIAN_POINT('Ctrl Pts',(-50.5905785208481,37.1493329797265,
39.8576902534424));
#171058=CARTESIAN_POINT('',(-50.3023253561992,36.939908654649,39.2875012672119));
#171059=CARTESIAN_POINT('',(-50.5905785208481,37.1493329797265,39.8576902534424));
#171060=CARTESIAN_POINT('',(-46.5911245387426,41.5228599914567,39.2875012672119));
#171061=CARTESIAN_POINT('Origin',(5.53234440788222E-15,0.,39.2875012672119));
#171062=CARTESIAN_POINT('',(-46.8559036426982,41.7612723673367,39.8576902534424));
#171063=CARTESIAN_POINT('',(-46.5911245387426,41.5228599914567,39.2875012672119));
#171064=CARTESIAN_POINT('',(-46.7942619810913,42.1132001506005,40.1599502534424));
#171065=CARTESIAN_POINT('Ctrl Pts',(-46.8559036426982,41.7612723673367,
39.8576902534424));
#171066=CARTESIAN_POINT('Ctrl Pts',(-46.865048646203,41.7695067430947,39.8773836120328));
#171067=CARTESIAN_POINT('Ctrl Pts',(-46.8728586744645,41.7791634256518,
39.8969946442061));
#171068=CARTESIAN_POINT('Ctrl Pts',(-46.8792591175129,41.7900688448274,
39.9162525288136));
#171069=CARTESIAN_POINT('Ctrl Pts',(-46.8857881704117,41.8011933963847,
39.9358973793919));
#171070=CARTESIAN_POINT('Ctrl Pts',(-46.8908511403464,41.8136179609569,
39.9551762199559));
#171071=CARTESIAN_POINT('Ctrl Pts',(-46.8943401533925,41.8272034165268,
39.9738152034029));
#171072=CARTESIAN_POINT('Ctrl Pts',(-46.8976936214446,41.8402610894628,
39.991730079239));
#171073=CARTESIAN_POINT('Ctrl Pts',(-46.8995933993913,41.8543920170169,
40.0090551157831));
#171074=CARTESIAN_POINT('Ctrl Pts',(-46.8999101480288,41.8695030436036,
40.0255394551213));
#171075=CARTESIAN_POINT('Ctrl Pts',(-46.9001534633409,41.8811108098749,
40.0382021525944));
#171076=CARTESIAN_POINT('Ctrl Pts',(-46.8994620808004,41.8932975750433,
40.0503687782025));
#171077=CARTESIAN_POINT('Ctrl Pts',(-46.8977610424069,41.9060298852858,
40.0619155352442));
#171078=CARTESIAN_POINT('Ctrl Pts',(-46.8977565842886,41.9060632544003,
40.0619457972351));
#171079=CARTESIAN_POINT('Ctrl Pts',(-46.8977521185698,41.9060966277703,
40.0619760547305));
#171080=CARTESIAN_POINT('Ctrl Pts',(-46.8977476452506,41.9061300053927,
40.0620063077269));
#171081=CARTESIAN_POINT('Ctrl Pts',(-46.8972680144601,41.9097087652735,
40.06525004417));
#171082=CARTESIAN_POINT('Ctrl Pts',(-46.8967002823074,41.9133346546845,
40.0684393223556));
#171083=CARTESIAN_POINT('Ctrl Pts',(-46.8960451360316,41.9170027866179,
40.0715697951759));
#171084=CARTESIAN_POINT('Ctrl Pts',(-46.8923993959675,41.9374151068061,
40.0889901646466));
#171085=CARTESIAN_POINT('Ctrl Pts',(-46.8860516300617,41.9591363747861,
40.1045963098324));
#171086=CARTESIAN_POINT('Ctrl Pts',(-46.8771671012894,41.9812950716655,
40.1176634650827));
#171087=CARTESIAN_POINT('Ctrl Pts',(-46.8731796017438,41.9912402016775,
40.1235281853125));
#171088=CARTESIAN_POINT('Ctrl Pts',(-46.8686813028933,42.0012737523661,
40.1288820140948));
#171089=CARTESIAN_POINT('Ctrl Pts',(-46.8636874904587,42.0113191526629,
40.1336621774101));
#171090=CARTESIAN_POINT('Ctrl Pts',(-46.8615172471194,42.0156847477609,
40.1357395717319));
#171091=CARTESIAN_POINT('Ctrl Pts',(-46.859253386561,42.0200523791244,40.1377083672884));
#171092=CARTESIAN_POINT('Ctrl Pts',(-46.8568971484357,42.0244156319708,
40.1395632548792));
#171093=CARTESIAN_POINT('Ctrl Pts',(-46.8486503149973,42.0396870169332,
40.146055361447));
#171094=CARTESIAN_POINT('Ctrl Pts',(-46.8392718539635,42.0549047629077,
40.1511520974629));
#171095=CARTESIAN_POINT('Ctrl Pts',(-46.8288149286281,42.0697938479571,
40.1546258197408));
#171096=CARTESIAN_POINT('Ctrl Pts',(-46.8235864659604,42.0772383904818,
40.1563626808798));
#171097=CARTESIAN_POINT('Ctrl Pts',(-46.8180883876708,42.0846007681803,
40.1576937882008));
#171098=CARTESIAN_POINT('Ctrl Pts',(-46.8123273450616,42.0918466086056,
40.1585906813668));
#171099=CARTESIAN_POINT('Ctrl Pts',(-46.809446823757,42.0954695288182,40.1590391279498));
#171100=CARTESIAN_POINT('Ctrl Pts',(-46.8065005614641,42.099063314795,40.1593790209175));
#171101=CARTESIAN_POINT('Ctrl Pts',(-46.8034893901143,42.1026236704494,
40.1596068022931));
#171102=CARTESIAN_POINT('Ctrl Pts',(-46.8004782187645,42.1061840261037,
40.1598345836687));
#171103=CARTESIAN_POINT('Ctrl Pts',(-46.7974021370897,42.1097109502942,
40.1599502506864));
#171104=CARTESIAN_POINT('Ctrl Pts',(-46.7942619810913,42.1132001506005,
40.1599502534424));
#171105=CARTESIAN_POINT('',(-46.7738319284254,42.1358900227699,40.1599502534424));
#171106=CARTESIAN_POINT('Origin',(7.58094983678529E-17,-1.03991361176645E-16,
40.1599502534424));
#171107=CARTESIAN_POINT('',(-46.4302753505421,42.2339804752705,39.8576902534424));
#171108=CARTESIAN_POINT('Ctrl Pts',(-46.7738319284254,42.1358900227699,
40.1599502534424));
#171109=CARTESIAN_POINT('Ctrl Pts',(-46.7712740741883,42.1387294146419,
40.1599502447858));
#171110=CARTESIAN_POINT('Ctrl Pts',(-46.7686877639335,42.1415290809212,
40.1598744685927));
#171111=CARTESIAN_POINT('Ctrl Pts',(-46.7660751225862,42.1442883388463,
40.1597246934279));
#171112=CARTESIAN_POINT('Ctrl Pts',(-46.7509772786444,42.1602334457359,
40.1588591777436));
#171113=CARTESIAN_POINT('Ctrl Pts',(-46.734999596514,42.1748324484411,40.1555254706029));
#171114=CARTESIAN_POINT('Ctrl Pts',(-46.7185561660749,42.1879477932289,
40.1500631826401));
#171115=CARTESIAN_POINT('Ctrl Pts',(-46.7119241523125,42.1932375134885,
40.1478601162497));
#171116=CARTESIAN_POINT('Ctrl Pts',(-46.7052163225658,42.1982863518301,
40.1453112228316));
#171117=CARTESIAN_POINT('Ctrl Pts',(-46.6984594183135,42.2030870843188,
40.1424401896328));
#171118=CARTESIAN_POINT('Ctrl Pts',(-46.6959665308742,42.2048582631419,
40.1413809526906));
#171119=CARTESIAN_POINT('Ctrl Pts',(-46.6934669941951,42.2065955404587,
40.1402777640512));
#171120=CARTESIAN_POINT('Ctrl Pts',(-46.6909621675968,42.2082984896058,
40.1391317641987));
#171121=CARTESIAN_POINT('Ctrl Pts',(-46.6862656177251,42.2114915192566,
40.1369830144753));
#171122=CARTESIAN_POINT('Ctrl Pts',(-46.6815504704768,42.2145638639317,
40.134683756585));
#171123=CARTESIAN_POINT('Ctrl Pts',(-46.6768256862943,42.2175127112219,
40.1322415082996));
#171124=CARTESIAN_POINT('Ctrl Pts',(-46.6602889416556,42.2278336767376,
40.1236936393009));
#171125=CARTESIAN_POINT('Ctrl Pts',(-46.6436341412463,42.2366417962863,
40.113394140767));
#171126=CARTESIAN_POINT('Ctrl Pts',(-46.6272454828771,42.2438165047413,
40.101665321223));
#171127=CARTESIAN_POINT('Ctrl Pts',(-46.6190511536924,42.2474038589688,
40.095800911451));
#171128=CARTESIAN_POINT('Ctrl Pts',(-46.6109233607687,42.2505828610987,
40.0895791707949));
#171129=CARTESIAN_POINT('Ctrl Pts',(-46.6029101354043,42.2533384464729,
40.0830403822906));
#171130=CARTESIAN_POINT('Ctrl Pts',(-46.598903522722,42.25471623916,40.0797709880385));
#171131=CARTESIAN_POINT('Ctrl Pts',(-46.5949255520162,42.2559881777374,
40.0764223317514));
#171132=CARTESIAN_POINT('Ctrl Pts',(-46.5909822275908,42.2571523794832,
40.0729994484778));
#171133=CARTESIAN_POINT('Ctrl Pts',(-46.5870389031655,42.258316581229,40.0695765652042));
#171134=CARTESIAN_POINT('Ctrl Pts',(-46.5831302673239,42.2593729236707,
40.0660793733488));
#171135=CARTESIAN_POINT('Ctrl Pts',(-46.5792622391316,42.2603197753211,
40.0625130768817));
#171136=CARTESIAN_POINT('Ctrl Pts',(-46.579229252952,42.2603278499826,40.0624826638418));
#171137=CARTESIAN_POINT('Ctrl Pts',(-46.5791962698503,42.260335916744,40.0624522459912));
#171138=CARTESIAN_POINT('Ctrl Pts',(-46.5791632898295,42.2603439756045,
40.0624218233329));
#171139=CARTESIAN_POINT('Ctrl Pts',(-46.5623199116986,42.2644597533378,
40.046884527588));
#171140=CARTESIAN_POINT('Ctrl Pts',(-46.5462756748339,42.2666468343728,
40.0302263329197));
#171141=CARTESIAN_POINT('Ctrl Pts',(-46.531134677875,42.2670764855937,40.012751588468));
#171142=CARTESIAN_POINT('Ctrl Pts',(-46.5154816224528,42.2675206673337,
39.9946858597626));
#171143=CARTESIAN_POINT('Ctrl Pts',(-46.5007931180847,42.2660861658582,
39.9757460620372));
#171144=CARTESIAN_POINT('Ctrl Pts',(-46.4872066206965,42.262915064436,39.9562444558982));
#171145=CARTESIAN_POINT('Ctrl Pts',(-46.4738785670777,42.2598042840354,
39.9371138113436));
#171146=CARTESIAN_POINT('Ctrl Pts',(-46.4616103837113,42.2550216427103,
39.9174410654147));
#171147=CARTESIAN_POINT('Ctrl Pts',(-46.4505634197995,42.2486653035344,
39.897519650391));
#171148=CARTESIAN_POINT('Ctrl Pts',(-46.4432451935029,42.244454451677,39.8843224113616));
#171149=CARTESIAN_POINT('Ctrl Pts',(-46.4364635650926,42.2395522518983,
39.8710160447052));
#171150=CARTESIAN_POINT('Ctrl Pts',(-46.4302753505421,42.2339804752705,
39.8576902534424));
#171151=CARTESIAN_POINT('',(-46.1654920697608,41.9955727382255,39.2875012672119));
#171152=CARTESIAN_POINT('',(-46.4302753505421,42.2339804752705,39.8576902534424));
#171153=CARTESIAN_POINT('',(-41.9955727382247,46.1654920697616,39.2875012672119));
#171154=CARTESIAN_POINT('Origin',(5.53234440788222E-15,0.,39.2875012672119));
#171155=CARTESIAN_POINT('',(-42.2339804752697,46.4302753505428,39.8576902534424));
#171156=CARTESIAN_POINT('',(-41.9955727382247,46.1654920697616,39.2875012672119));
#171157=CARTESIAN_POINT('',(-42.1358900227691,46.7738319284261,40.1599502534424));
#171158=CARTESIAN_POINT('Ctrl Pts',(-42.2339804752697,46.4302753505428,
39.8576902534424));
#171159=CARTESIAN_POINT('Ctrl Pts',(-42.2422146548469,46.4394205306943,
39.8773836120384));
#171160=CARTESIAN_POINT('Ctrl Pts',(-42.2489725007701,46.4498406831895,
39.8969946442172));
#171161=CARTESIAN_POINT('Ctrl Pts',(-42.2541979548148,46.4613553898177,
39.91625252883));
#171162=CARTESIAN_POINT('Ctrl Pts',(-42.2595284086006,46.4731014717878,
39.935897379414));
#171163=CARTESIAN_POINT('Ctrl Pts',(-42.2632649224145,46.4859871977669,
39.9551762199833));
#171164=CARTESIAN_POINT('Ctrl Pts',(-42.2653147554872,46.499862931967,39.9738152034351));
#171165=CARTESIAN_POINT('Ctrl Pts',(-42.2672849544032,46.5131996064718,
39.9917300792761));
#171166=CARTESIAN_POINT('Ctrl Pts',(-42.2676972410234,46.5274517042014,
40.0090551158245));
#171167=CARTESIAN_POINT('Ctrl Pts',(-42.2664327220877,46.5425130602579,
40.0255394551664));
#171168=CARTESIAN_POINT('Ctrl Pts',(-42.2654613625215,46.5540826713342,
40.0382021526232));
#171169=CARTESIAN_POINT('Ctrl Pts',(-42.2634999036127,46.5661304069596,
40.0503687782163));
#171170=CARTESIAN_POINT('Ctrl Pts',(-42.2604772948656,46.5786151613304,
40.0619155352442));
#171171=CARTESIAN_POINT('Ctrl Pts',(-42.2604693731471,46.5786478816451,
40.0619457972352));
#171172=CARTESIAN_POINT('Ctrl Pts',(-42.2604614434249,46.5786806053976,
40.0619760547305));
#171173=CARTESIAN_POINT('Ctrl Pts',(-42.2604535056994,46.5787133325847,
40.062006307727));
#171174=CARTESIAN_POINT('Ctrl Pts',(-42.2596024201058,46.5822223525749,
40.06525004417));
#171175=CARTESIAN_POINT('Ctrl Pts',(-42.2586587894011,46.5857690348149,
40.0684393223556));
#171176=CARTESIAN_POINT('Ctrl Pts',(-42.2576238078912,46.5893485909044,
40.0715697951759));
#171177=CARTESIAN_POINT('Ctrl Pts',(-42.2518643711132,46.609268006655,40.0889901646418));
#171178=CARTESIAN_POINT('Ctrl Pts',(-42.2432808881741,46.6302067610349,
40.1045963098239));
#171179=CARTESIAN_POINT('Ctrl Pts',(-42.2321288152516,46.651315384109,40.117663465072));
#171180=CARTESIAN_POINT('Ctrl Pts',(-42.2271236104862,46.6607892264642,
40.123528185306));
#171181=CARTESIAN_POINT('Ctrl Pts',(-42.2216011621498,46.6702976120519,
40.1288820140919));
#171182=CARTESIAN_POINT('Ctrl Pts',(-42.2155846760826,46.679765987061,40.1336621774101));
#171183=CARTESIAN_POINT('Ctrl Pts',(-42.2129699926165,46.683880814771,40.1357395717319));
#171184=CARTESIAN_POINT('Ctrl Pts',(-42.2102619919286,46.6879878819277,
40.1377083672884));
#171185=CARTESIAN_POINT('Ctrl Pts',(-42.2074625774074,46.6920809384682,
40.1395632548792));
#171186=CARTESIAN_POINT('Ctrl Pts',(-42.1976646265834,46.7064066363598,
40.146055361447));
#171187=CARTESIAN_POINT('Ctrl Pts',(-42.1867468541393,46.7205607018098,
40.151152097463));
#171188=CARTESIAN_POINT('Ctrl Pts',(-42.1747908797553,46.7342751765576,
40.1546258197409));
#171189=CARTESIAN_POINT('Ctrl Pts',(-42.1688128925634,46.7411324139316,
40.1563626808798));
#171190=CARTESIAN_POINT('Ctrl Pts',(-42.1625753552951,46.7478797540802,
40.1576937882008));
#171191=CARTESIAN_POINT('Ctrl Pts',(-42.1560884757154,46.7544837081027,
40.1585906813668));
#171192=CARTESIAN_POINT('Ctrl Pts',(-42.1528450359255,46.7577856851139,
40.1590391279498));
#171193=CARTESIAN_POINT('Ctrl Pts',(-42.1495392606402,46.7610518156853,
40.1593790209175));
#171194=CARTESIAN_POINT('Ctrl Pts',(-42.1461724262969,46.764277914225,40.1596068022931));
#171195=CARTESIAN_POINT('Ctrl Pts',(-42.1428055919536,46.7675040127647,
40.1598345836687));
#171196=CARTESIAN_POINT('Ctrl Pts',(-42.1393776974104,46.7706900780051,
40.1599502506865));
#171197=CARTESIAN_POINT('Ctrl Pts',(-42.1358900227691,46.7738319284261,
40.1599502534424));
#171198=CARTESIAN_POINT('',(-42.1132001505997,46.794261981092,40.1599502534424));
#171199=CARTESIAN_POINT('Origin',(6.43067523875891E-17,-1.15494107156905E-16,
40.1599502534424));
#171200=CARTESIAN_POINT('',(-41.7612723673359,46.8559036426989,39.8576902534424));
#171201=CARTESIAN_POINT('Ctrl Pts',(-42.1132001505997,46.794261981092,40.1599502534424));
#171202=CARTESIAN_POINT('Ctrl Pts',(-42.1103595112868,46.7968184499056,
40.1599502447859));
#171203=CARTESIAN_POINT('Ctrl Pts',(-42.1074947242963,46.7993324362836,
40.1598744685926));
#171204=CARTESIAN_POINT('Ctrl Pts',(-42.104607974281,46.80180348332,40.1597246934279));
#171205=CARTESIAN_POINT('Ctrl Pts',(-42.0879261203839,46.8160830868235,
40.1588591777433));
#171206=CARTESIAN_POINT('Ctrl Pts',(-42.0705099543453,46.8289319921076,
40.1555254706011));
#171207=CARTESIAN_POINT('Ctrl Pts',(-42.052785675898,46.8402566831519,40.1500631826359));
#171208=CARTESIAN_POINT('Ctrl Pts',(-42.0456370666755,46.8448241915603,
40.1478601162464));
#171209=CARTESIAN_POINT('Ctrl Pts',(-42.0384382358134,46.849144212699,40.1453112228297));
#171210=CARTESIAN_POINT('Ctrl Pts',(-42.0312165334047,46.8532123574523,
40.1424401896328));
#171211=CARTESIAN_POINT('Ctrl Pts',(-42.028552163663,46.8547132558793,40.1413809526906));
#171212=CARTESIAN_POINT('Ctrl Pts',(-42.0258847247792,46.8561797434812,
40.1402777640511));
#171213=CARTESIAN_POINT('Ctrl Pts',(-42.0232156132258,46.8576115380197,
40.1391317641987));
#171214=CARTESIAN_POINT('Ctrl Pts',(-42.0182110290631,46.8602961527792,
40.1369830144753));
#171215=CARTESIAN_POINT('Ctrl Pts',(-42.0132005644172,46.8628587997327,
40.1346837565849));
#171216=CARTESIAN_POINT('Ctrl Pts',(-42.0081934246212,46.8652976184991,
40.1322415082996));
#171217=CARTESIAN_POINT('Ctrl Pts',(-41.9906684353351,46.8738334841812,
40.1236936393008));
#171218=CARTESIAN_POINT('Ctrl Pts',(-41.9731841724644,46.8808524512366,
40.113394140767));
#171219=CARTESIAN_POINT('Ctrl Pts',(-41.9561353316313,46.8862747746137,
40.101665321223));
#171220=CARTESIAN_POINT('Ctrl Pts',(-41.9476109112147,46.8889859363022,
40.095800911451));
#171221=CARTESIAN_POINT('Ctrl Pts',(-41.9391953469837,46.8912979378217,
40.0895791707949));
#171222=CARTESIAN_POINT('Ctrl Pts',(-41.9309379818017,46.8932008176777,
40.0830403822906));
#171223=CARTESIAN_POINT('Ctrl Pts',(-41.9268092992106,46.8941522576057,
40.0797709880385));
#171224=CARTESIAN_POINT('Ctrl Pts',(-41.9227201664597,46.8950014172057,
40.0764223317514));
#171225=CARTESIAN_POINT('Ctrl Pts',(-41.9186767517587,46.8957470516902,
40.0729994484778));
#171226=CARTESIAN_POINT('Ctrl Pts',(-41.9146333370577,46.8964926861746,
40.0695765652042));
#171227=CARTESIAN_POINT('Ctrl Pts',(-41.9106356952802,46.897134678164,40.0660793733488));
#171228=CARTESIAN_POINT('Ctrl Pts',(-41.9066898836031,46.8976720238191,
40.0625130768817));
#171229=CARTESIAN_POINT('Ctrl Pts',(-41.9066562340933,46.8976766062522,
40.0624826638418));
#171230=CARTESIAN_POINT('Ctrl Pts',(-41.9066225884702,46.89768118115,40.0624522459912));
#171231=CARTESIAN_POINT('Ctrl Pts',(-41.9065889467371,46.8976857485123,
40.0624218233329));
#171232=CARTESIAN_POINT('Ctrl Pts',(-41.8894076224742,46.9000183671521,
40.0468845275896));
#171233=CARTESIAN_POINT('Ctrl Pts',(-41.8732226653996,46.9005163877047,
40.0302263329231));
#171234=CARTESIAN_POINT('Ctrl Pts',(-41.8581197016257,46.8993610201073,
40.0127515884734));
#171235=CARTESIAN_POINT('Ctrl Pts',(-41.8425059656456,46.898166578745,39.9946858597699));
#171236=CARTESIAN_POINT('Ctrl Pts',(-41.8280478726772,46.8952045688303,
39.9757460620467));
#171237=CARTESIAN_POINT('Ctrl Pts',(-41.8148672739026,46.8906306633413,
39.9562444559099));
#171238=CARTESIAN_POINT('Ctrl Pts',(-41.8019373978516,46.8861437631592,
39.9371138113573));
#171239=CARTESIAN_POINT('Ctrl Pts',(-41.7902363430259,46.8801049472907,
39.9174410654306));
#171240=CARTESIAN_POINT('Ctrl Pts',(-41.7799143139045,46.872628706646,39.897519650409));
#171241=CARTESIAN_POINT('Ctrl Pts',(-41.7730763314874,46.8676759593254,
39.8843224113737));
#171242=CARTESIAN_POINT('Ctrl Pts',(-41.7668442729534,46.8620917411115,
39.8710160447113));
#171243=CARTESIAN_POINT('Ctrl Pts',(-41.7612723673359,46.8559036426989,
39.8576902534424));
#171244=CARTESIAN_POINT('',(-41.5228599914559,46.5911245387433,39.2875012672119));
#171245=CARTESIAN_POINT('',(-41.7612723673359,46.8559036426989,39.8576902534424));
#171246=CARTESIAN_POINT('',(-36.9399086546482,50.3023253561999,39.2875012672119));
#171247=CARTESIAN_POINT('Origin',(5.53234440788222E-15,0.,39.2875012672119));
#171248=CARTESIAN_POINT('',(-37.1493329797256,50.5905785208487,39.8576902534424));
#171249=CARTESIAN_POINT('',(-36.9399086546482,50.3023253561999,39.2875012672119));
#171250=CARTESIAN_POINT('',(-37.0158684358555,50.9219998155903,40.1599502534424));
#171251=CARTESIAN_POINT('Ctrl Pts',(-37.1493329797256,50.5905785208487,
39.8576902534424));
#171252=CARTESIAN_POINT('Ctrl Pts',(-37.1565661199767,50.6005343088816,
39.8773836120343));
#171253=CARTESIAN_POINT('Ctrl Pts',(-37.1621977431848,50.6116037659379,
39.8969946442089));
#171254=CARTESIAN_POINT('Ctrl Pts',(-37.1661909570565,50.6236016024766,
39.9162525288178));
#171255=CARTESIAN_POINT('Ctrl Pts',(-37.1702644101608,50.6358405223205,
39.9358973793979));
#171256=CARTESIAN_POINT('Ctrl Pts',(-37.1726335298269,50.6490462309881,
39.9551762199636));
#171257=CARTESIAN_POINT('Ctrl Pts',(-37.1732217245282,50.663060218362,39.9738152034121));
#171258=CARTESIAN_POINT('Ctrl Pts',(-37.1737870683986,50.6765297750304,
39.9917300792502));
#171259=CARTESIAN_POINT('Ctrl Pts',(-37.1727073465975,50.6907468939608,
40.0090551157961));
#171260=CARTESIAN_POINT('Ctrl Pts',(-37.1698754144281,50.7055935641083,
40.0255394551359));
#171261=CARTESIAN_POINT('Ctrl Pts',(-37.1677000224047,50.7169982609304,
40.0382021526037));
#171262=CARTESIAN_POINT('Ctrl Pts',(-37.1644899772806,50.7287749695232,
40.050368778207));
#171263=CARTESIAN_POINT('Ctrl Pts',(-37.1601789145083,50.7408753824656,
40.0619155352442));
#171264=CARTESIAN_POINT('Ctrl Pts',(-37.1601676159816,50.7409070954899,
40.0619457972351));
#171265=CARTESIAN_POINT('Ctrl Pts',(-37.1601563091356,50.7409388110966,
40.0619760547305));
#171266=CARTESIAN_POINT('Ctrl Pts',(-37.1601449939713,50.7409705292825,
40.0620063077269));
#171267=CARTESIAN_POINT('Ctrl Pts',(-37.1589317782465,50.7443713638249,
40.06525004417));
#171268=CARTESIAN_POINT('Ctrl Pts',(-37.1576225876053,50.747799980701,40.0684393223557));
#171269=CARTESIAN_POINT('Ctrl Pts',(-37.1562191103351,50.7512517425809,
40.0715697951759));
#171270=CARTESIAN_POINT('Ctrl Pts',(-37.1484090784357,50.7704600126149,
40.0889901646443));
#171271=CARTESIAN_POINT('Ctrl Pts',(-37.1376839208943,50.7903868440293,
40.1045963098283));
#171272=CARTESIAN_POINT('Ctrl Pts',(-37.1243864882599,50.8102141228154,
40.1176634650776));
#171273=CARTESIAN_POINT('Ctrl Pts',(-37.1184184163487,50.8191128801057,
40.1235281853093));
#171274=CARTESIAN_POINT('Ctrl Pts',(-37.1119323236304,50.8279919247214,
40.1288820140934));
#171275=CARTESIAN_POINT('Ctrl Pts',(-37.1049590818163,50.8367795369358,
40.1336621774101));
#171276=CARTESIAN_POINT('Ctrl Pts',(-37.1019286052427,50.8405985143445,
40.1357395717319));
#171277=CARTESIAN_POINT('Ctrl Pts',(-37.0988061338475,50.8444000194071,
40.1377083672884));
#171278=CARTESIAN_POINT('Ctrl Pts',(-37.0955942139017,50.8481780352576,
40.1395632548792));
#171279=CARTESIAN_POINT('Ctrl Pts',(-37.0843524940916,50.8614010907344,
40.146055361447));
#171280=CARTESIAN_POINT('Ctrl Pts',(-37.0720150276368,50.8743364007571,
40.1511520974629));
#171281=CARTESIAN_POINT('Ctrl Pts',(-37.0586909963616,50.886726006548,40.1546258197408));
#171282=CARTESIAN_POINT('Ctrl Pts',(-37.052028980724,50.8929208094435,40.1563626808798));
#171283=CARTESIAN_POINT('Ctrl Pts',(-37.0451203242406,50.8989791867716,
40.1576937882008));
#171284=CARTESIAN_POINT('Ctrl Pts',(-37.0379786793005,50.9048689000891,
40.1585906813668));
#171285=CARTESIAN_POINT('Ctrl Pts',(-37.0344078568305,50.9078137567479,
40.1590391279498));
#171286=CARTESIAN_POINT('Ctrl Pts',(-37.0307787873186,50.9107164475037,
40.1593790209175));
#171287=CARTESIAN_POINT('Ctrl Pts',(-37.0270931777235,50.9135729431181,
40.1596068022931));
#171288=CARTESIAN_POINT('Ctrl Pts',(-37.0234075681283,50.9164294387325,
40.1598345836687));
#171289=CARTESIAN_POINT('Ctrl Pts',(-37.0196654174466,50.9192397378253,
40.1599502506865));
#171290=CARTESIAN_POINT('Ctrl Pts',(-37.0158684358555,50.9219998155903,
40.1599502534424));
#171291=CARTESIAN_POINT('',(-36.9911673391703,50.9399462128205,40.1599502534424));
#171292=CARTESIAN_POINT('Origin',(5.16646552926871E-17,-1.25731475530457E-16,
40.1599502534424));
#171293=CARTESIAN_POINT('',(-36.634724144965,50.9644637245896,39.8576902534424));
#171294=CARTESIAN_POINT('Ctrl Pts',(-36.9911673391703,50.9399462128205,
40.1599502534424));
#171295=CARTESIAN_POINT('Ctrl Pts',(-36.9880750374203,50.9421917493683,
40.1599502447858));
#171296=CARTESIAN_POINT('Ctrl Pts',(-36.9849631609,50.9443925120842,40.1598744685927));
#171297=CARTESIAN_POINT('Ctrl Pts',(-36.9818339300539,50.9465482749234,
40.1597246934279));
#171298=CARTESIAN_POINT('Ctrl Pts',(-36.9637508360915,50.9590059247098,
40.1588591777435));
#171299=CARTESIAN_POINT('Ctrl Pts',(-36.9450870013129,50.9699639572724,
40.1555254706026));
#171300=CARTESIAN_POINT('Ctrl Pts',(-36.9262760657698,50.9793739188842,
40.1500631826394));
#171301=CARTESIAN_POINT('Ctrl Pts',(-36.9186891827376,50.9831691728694,
40.1478601162492));
#171302=CARTESIAN_POINT('Ctrl Pts',(-36.9110782226493,50.9867130457549,
40.1453112228313));
#171303=CARTESIAN_POINT('Ctrl Pts',(-36.9034708445584,50.9900040313324,
40.1424401896328));
#171304=CARTESIAN_POINT('Ctrl Pts',(-36.9006641839068,50.9912182052062,
40.1413809526906));
#171305=CARTESIAN_POINT('Ctrl Pts',(-36.8978580678369,50.9923978359482,
40.1402777640512));
#171306=CARTESIAN_POINT('Ctrl Pts',(-36.895053914673,50.9935427888373,40.1391317641987));
#171307=CARTESIAN_POINT('Ctrl Pts',(-36.8897961274908,50.9956895755045,
40.1369830144753));
#171308=CARTESIAN_POINT('Ctrl Pts',(-36.8845452411465,50.9977144478402,
40.1346837565849));
#171309=CARTESIAN_POINT('Ctrl Pts',(-36.8793106050083,50.9996165178739,
40.1322415082996));
#171310=CARTESIAN_POINT('Ctrl Pts',(-36.8609893785248,51.0062737629919,
40.1236936393009));
#171311=CARTESIAN_POINT('Ctrl Pts',(-36.8428672144356,51.0114266762821,
40.113394140767));
#171312=CARTESIAN_POINT('Ctrl Pts',(-36.8253449818064,51.0150372064716,
40.101665321223));
#171313=CARTESIAN_POINT('Ctrl Pts',(-36.8165838654919,51.0168424715663,
40.095800911451));
#171314=CARTESIAN_POINT('Ctrl Pts',(-36.8079727326363,51.018262141703,40.0895791707949));
#171315=CARTESIAN_POINT('Ctrl Pts',(-36.7995616970576,51.0192914676909,
40.0830403822907));
#171316=CARTESIAN_POINT('Ctrl Pts',(-36.7953561792682,51.0198061306849,
40.0797709880385));
#171317=CARTESIAN_POINT('Ctrl Pts',(-36.7912006858663,51.0202232077372,
40.0764223317514));
#171318=CARTESIAN_POINT('Ctrl Pts',(-36.7871014813873,51.0205421056329,
40.0729994484778));
#171319=CARTESIAN_POINT('Ctrl Pts',(-36.7830022769083,51.0208610035286,
40.0695765652042));
#171320=CARTESIAN_POINT('Ctrl Pts',(-36.7789594281946,51.0210816112669,
40.0660793733488));
#171321=CARTESIAN_POINT('Ctrl Pts',(-36.7749790641711,51.0212035636554,
40.0625130768817));
#171322=CARTESIAN_POINT('Ctrl Pts',(-36.7749451200022,51.0212046036538,
40.0624826638418));
#171323=CARTESIAN_POINT('Ctrl Pts',(-36.7749111804864,51.0212056365646,
40.0624522459912));
#171324=CARTESIAN_POINT('Ctrl Pts',(-36.7748772456268,51.0212066623878,
40.0624218233329));
#171325=CARTESIAN_POINT('Ctrl Pts',(-36.7575462174132,51.0217305652765,
40.0468845275888));
#171326=CARTESIAN_POINT('Ctrl Pts',(-36.7413978659031,51.0205340689293,
40.0302263329216));
#171327=CARTESIAN_POINT('Ctrl Pts',(-36.7264984065438,51.0178063409622,
40.0127515884709));
#171328=CARTESIAN_POINT('Ctrl Pts',(-36.7110950573628,51.0149863630466,
39.9946858597669));
#171329=CARTESIAN_POINT('Ctrl Pts',(-36.6970257816846,51.0105292970922,
39.9757460620431));
#171330=CARTESIAN_POINT('Ctrl Pts',(-36.684395490921,51.0046027002009,39.9562444559056));
#171331=CARTESIAN_POINT('Ctrl Pts',(-36.6720054548649,50.9987888396535,
39.9371138113531));
#171332=CARTESIAN_POINT('Ctrl Pts',(-36.6609997277847,50.9915600117704,
39.9174410654264));
#171333=CARTESIAN_POINT('Ctrl Pts',(-36.6515157237649,50.9830457809122,
39.8975196504048));
#171334=CARTESIAN_POINT('Ctrl Pts',(-36.6452329035982,50.977405401466,39.8843224113709));
#171335=CARTESIAN_POINT('Ctrl Pts',(-36.6396186946822,50.9712003466828,
39.8710160447099));
#171336=CARTESIAN_POINT('Ctrl Pts',(-36.634724144965,50.9644637245896,39.8576902534424));
#171337=CARTESIAN_POINT('',(-36.4252947698674,50.6762142289951,39.2875012672119));
#171338=CARTESIAN_POINT('',(-36.634724144965,50.9644637245896,39.8576902534424));
#171339=CARTESIAN_POINT('',(-31.4795232016785,53.8880358395973,39.2875012672119));
#171340=CARTESIAN_POINT('Origin',(5.53234440788222E-15,0.,39.2875012672119));
#171341=CARTESIAN_POINT('',(-31.6576696180579,54.196600726121,39.8576902534424));
#171342=CARTESIAN_POINT('',(-31.4795232016785,53.8880358395973,39.2875012672119));
#171343=CARTESIAN_POINT('',(-31.4902932482903,54.5122556166614,40.1599502534424));
#171344=CARTESIAN_POINT('Ctrl Pts',(-31.6576696180579,54.196600726121,39.8576902534424));
#171345=CARTESIAN_POINT('Ctrl Pts',(-31.6638224711875,54.2072580443428,
39.8773836120385));
#171346=CARTESIAN_POINT('Ctrl Pts',(-31.6682661704396,54.2188555266773,
39.8969946442173));
#171347=CARTESIAN_POINT('Ctrl Pts',(-31.6709833936518,54.2312050423246,
39.91625252883));
#171348=CARTESIAN_POINT('Ctrl Pts',(-31.6737552164704,54.2438027078811,
39.9358973794142));
#171349=CARTESIAN_POINT('Ctrl Pts',(-31.6747309854168,54.2571837147363,
39.9551762199837));
#171350=CARTESIAN_POINT('Ctrl Pts',(-31.6738510973598,54.2711824151128,
39.9738152034356));
#171351=CARTESIAN_POINT('Ctrl Pts',(-31.6730053921561,54.2846372786697,
39.9917300792771));
#171352=CARTESIAN_POINT('Ctrl Pts',(-31.6704454915877,54.2986636530781,
40.009055115826));
#171353=CARTESIAN_POINT('Ctrl Pts',(-31.6660771734206,54.313132974099,40.0255394551682));
#171354=CARTESIAN_POINT('Ctrl Pts',(-31.6627215829905,54.3242478044044,
40.0382021526244));
#171355=CARTESIAN_POINT('Ctrl Pts',(-31.6582981215806,54.335624457862,40.0503687782168));
#171356=CARTESIAN_POINT('Ctrl Pts',(-31.6527458376963,54.3472079546997,
40.0619155352442));
#171357=CARTESIAN_POINT('Ctrl Pts',(-31.6527312861504,54.3472383129791,
40.0619457972352));
#171358=CARTESIAN_POINT('Ctrl Pts',(-31.6527167260609,54.3472686729571,
40.0619760547305));
#171359=CARTESIAN_POINT('Ctrl Pts',(-31.6527021574289,54.3472990346307,
40.0620063077269));
#171360=CARTESIAN_POINT('Ctrl Pts',(-31.6511401038183,54.3505544234703,
40.06525004417));
#171361=CARTESIAN_POINT('Ctrl Pts',(-31.6494796970072,54.3538274103386,
40.0684393223556));
#171362=CARTESIAN_POINT('Ctrl Pts',(-31.6477231007675,54.3571135597835,
40.0715697951759));
#171363=CARTESIAN_POINT('Ctrl Pts',(-31.6379480420933,54.3754002342682,
40.0889901646408));
#171364=CARTESIAN_POINT('Ctrl Pts',(-31.6251987170247,54.3940968201752,
40.104596309822));
#171365=CARTESIAN_POINT('Ctrl Pts',(-31.6099016141394,54.4124255228513,
40.1176634650697));
#171366=CARTESIAN_POINT('Ctrl Pts',(-31.6030360625235,54.4206516984363,
40.1235281853045));
#171367=CARTESIAN_POINT('Ctrl Pts',(-31.5956573884077,54.4288041214158,
40.1288820140912));
#171368=CARTESIAN_POINT('Ctrl Pts',(-31.5878037911377,54.4368146919238,
40.1336621774101));
#171369=CARTESIAN_POINT('Ctrl Pts',(-31.5843907239921,54.4402959775155,
40.1357395717319));
#171370=CARTESIAN_POINT('Ctrl Pts',(-31.5808879923396,54.4437502703991,
40.1377083672884));
#171371=CARTESIAN_POINT('Ctrl Pts',(-31.5772987574364,54.4471718528274,
40.1395632548792));
#171372=CARTESIAN_POINT('Ctrl Pts',(-31.5647364352749,54.4591473913265,
40.146055361447));
#171373=CARTESIAN_POINT('Ctrl Pts',(-31.5511144466737,54.4707222239583,
40.151152097463));
#171374=CARTESIAN_POINT('Ctrl Pts',(-31.5365683393821,54.4816512176787,
40.1546258197409));
#171375=CARTESIAN_POINT('Ctrl Pts',(-31.5292952857363,54.4871157145389,
40.1563626808798));
#171376=CARTESIAN_POINT('Ctrl Pts',(-31.521791202724,54.4924187521965,40.1576937882008));
#171377=CARTESIAN_POINT('Ctrl Pts',(-31.51407303778,54.4975296958775,40.1585906813668));
#171378=CARTESIAN_POINT('Ctrl Pts',(-31.5102139553079,54.500085167718,40.1590391279498));
#171379=CARTESIAN_POINT('Ctrl Pts',(-31.5063013524145,54.502592616171,40.1593790209175));
#171380=CARTESIAN_POINT('Ctrl Pts',(-31.5023373478775,54.5050482124963,
40.1596068022931));
#171381=CARTESIAN_POINT('Ctrl Pts',(-31.4983733433404,54.5075038088217,
40.1598345836687));
#171382=CARTESIAN_POINT('Ctrl Pts',(-31.4943579363062,54.509907551542,40.1599502506865));
#171383=CARTESIAN_POINT('Ctrl Pts',(-31.4902932482903,54.5122556166614,
40.1599502534424));
#171384=CARTESIAN_POINT('',(-31.4638515574735,54.5275217339722,40.1599502534424));
#171385=CARTESIAN_POINT('Origin',(3.80217165444466E-17,-1.34591303547096E-16,
40.1599502534424));
#171386=CARTESIAN_POINT('',(-31.106798218553,54.5146464769141,39.8576902534424));
#171387=CARTESIAN_POINT('Ctrl Pts',(-31.4638515574735,54.5275217339722,
40.1599502534424));
#171388=CARTESIAN_POINT('Ctrl Pts',(-31.4605414731915,54.529431735686,40.1599502447858));
#171389=CARTESIAN_POINT('Ctrl Pts',(-31.4572166015116,54.531295162723,40.1598744685927));
#171390=CARTESIAN_POINT('Ctrl Pts',(-31.4538791743428,54.5331120223762,
40.1597246934279));
#171391=CARTESIAN_POINT('Ctrl Pts',(-31.4345929624705,54.5436112298321,
40.1588591777434));
#171392=CARTESIAN_POINT('Ctrl Pts',(-31.4148859438247,54.5525583311786,
40.1555254706017));
#171393=CARTESIAN_POINT('Ctrl Pts',(-31.3951944477252,54.5599504658517,
40.1500631826372));
#171394=CARTESIAN_POINT('Ctrl Pts',(-31.3872524143681,54.562931883813,40.1478601162474));
#171395=CARTESIAN_POINT('Ctrl Pts',(-31.3793127123314,54.565660781029,40.1453112228303));
#171396=CARTESIAN_POINT('Ctrl Pts',(-31.3714030065914,54.568138550701,40.1424401896328));
#171397=CARTESIAN_POINT('Ctrl Pts',(-31.3684848053913,54.5690526972784,
40.1413809526905));
#171398=CARTESIAN_POINT('Ctrl Pts',(-31.3655707565302,54.5699325468792,
40.1402777640511));
#171399=CARTESIAN_POINT('Ctrl Pts',(-31.3626622846447,54.5707781137757,
40.1391317641987));
#171400=CARTESIAN_POINT('Ctrl Pts',(-31.3572088998595,54.5723635517065,
40.1369830144753));
#171401=CARTESIAN_POINT('Ctrl Pts',(-31.3517751216264,54.5738284644994,
40.1346837565849));
#171402=CARTESIAN_POINT('Ctrl Pts',(-31.3463703409151,54.5751729463231,
40.1322415082996));
#171403=CARTESIAN_POINT('Ctrl Pts',(-31.3274536084255,54.5798786327062,
40.1236936393009));
#171404=CARTESIAN_POINT('Ctrl Pts',(-31.3088920933397,54.583109035835,40.113394140767));
#171405=CARTESIAN_POINT('Ctrl Pts',(-31.291088446162,54.5848682151125,40.101665321223));
#171406=CARTESIAN_POINT('Ctrl Pts',(-31.2821866225731,54.5857478047513,
40.095800911451));
#171407=CARTESIAN_POINT('Ctrl Pts',(-31.2734742664666,54.5862595893021,
40.0895791707949));
#171408=CARTESIAN_POINT('Ctrl Pts',(-31.2650017135572,54.586404083911,40.0830403822906));
#171409=CARTESIAN_POINT('Ctrl Pts',(-31.2607654371024,54.5864763312154,
40.0797709880385));
#171410=CARTESIAN_POINT('Ctrl Pts',(-31.2565891115048,54.5864567561367,
40.0764223317514));
#171411=CARTESIAN_POINT('Ctrl Pts',(-31.2524790289898,54.5863454235315,
40.0729994484778));
#171412=CARTESIAN_POINT('Ctrl Pts',(-31.2483689464749,54.5862340909263,
40.0695765652042));
#171413=CARTESIAN_POINT('Ctrl Pts',(-31.2443251851216,54.5860308973891,
40.0660793733488));
#171414=CARTESIAN_POINT('Ctrl Pts',(-31.240353878453,54.585736120375,40.0625130768817));
#171415=CARTESIAN_POINT('Ctrl Pts',(-31.2403200115243,54.5857336065444,
40.0624826638418));
#171416=CARTESIAN_POINT('Ctrl Pts',(-31.2402861499641,54.5857310861514,
40.0624522459912));
#171417=CARTESIAN_POINT('Ctrl Pts',(-31.2402522937756,54.5857285591963,
40.0624218233329));
#171418=CARTESIAN_POINT('Ctrl Pts',(-31.2229614439845,54.5844380063441,
40.0468845275892));
#171419=CARTESIAN_POINT('Ctrl Pts',(-31.2070266227585,54.5815601021615,
40.0302263329224));
#171420=CARTESIAN_POINT('Ctrl Pts',(-31.1924939094095,54.5772898993835,
40.0127515884722));
#171421=CARTESIAN_POINT('Ctrl Pts',(-31.177469709345,54.5728752811829,39.9946858597683));
#171422=CARTESIAN_POINT('Ctrl Pts',(-31.1639433968861,54.5669719917362,
39.9757460620447));
#171423=CARTESIAN_POINT('Ctrl Pts',(-31.1520017942423,54.5597576364788,
39.9562444559074));
#171424=CARTESIAN_POINT('Ctrl Pts',(-31.1402873460085,54.5526805134389,
39.9371138113545));
#171425=CARTESIAN_POINT('Ctrl Pts',(-31.1300975277224,54.5443408740924,
39.9174410654274));
#171426=CARTESIAN_POINT('Ctrl Pts',(-31.1215554575362,54.5348819367158,
39.8975196504055));
#171427=CARTESIAN_POINT('Ctrl Pts',(-31.1158966355113,54.5286157223213,
39.8843224113713));
#171428=CARTESIAN_POINT('Ctrl Pts',(-31.11096178666,54.5218578148469,39.8710160447101));
#171429=CARTESIAN_POINT('Ctrl Pts',(-31.106798218553,54.5146464769141,39.8576902534424));
#171430=CARTESIAN_POINT('',(-30.9286463962973,54.2060847114744,39.2875012672119));
#171431=CARTESIAN_POINT('',(-31.106798218553,54.5146464769141,39.8576902534424));
#171432=CARTESIAN_POINT('',(-25.6742415049975,56.8833377255397,39.2875012672119));
#171433=CARTESIAN_POINT('Origin',(5.53234440788222E-15,0.,39.2875012672119));
#171434=CARTESIAN_POINT('',(-25.8191582032616,57.2088336324701,39.8576902534424));
#171435=CARTESIAN_POINT('',(-25.6742415049975,56.8833377255397,39.2875012672119));
#171436=CARTESIAN_POINT('',(-25.6197038181293,57.5052637377734,40.1599502534424));
#171437=CARTESIAN_POINT('Ctrl Pts',(-25.8191582032616,57.2088336324701,
39.8576902534424));
#171438=CARTESIAN_POINT('Ctrl Pts',(-25.8241633573205,57.2200757170674,
39.8773836120341));
#171439=CARTESIAN_POINT('Ctrl Pts',(-25.8273704465167,57.2320741602315,
39.8969946442087));
#171440=CARTESIAN_POINT('Ctrl Pts',(-25.8287819086036,57.2446400511037,
39.9162525288174));
#171441=CARTESIAN_POINT('Ctrl Pts',(-25.8302217324658,57.2574584397068,
39.9358973793973));
#171442=CARTESIAN_POINT('Ctrl Pts',(-25.8297934599656,57.2708681396314,
39.9551762199628));
#171443=CARTESIAN_POINT('Ctrl Pts',(-25.8274551293915,57.2846981803126,
39.9738152034111));
#171444=CARTESIAN_POINT('Ctrl Pts',(-25.8252076408405,57.2979909364506,
39.9917300792492));
#171445=CARTESIAN_POINT('Ctrl Pts',(-25.821195608316,57.3116728904364,40.0090551157951));
#171446=CARTESIAN_POINT('Ctrl Pts',(-25.8153387643658,57.3256063334144,
40.0255394551348));
#171447=CARTESIAN_POINT('Ctrl Pts',(-25.8108397400779,57.3363095208145,
40.038202152603));
#171448=CARTESIAN_POINT('Ctrl Pts',(-25.8052513267455,57.34716147416,40.0503687782067));
#171449=CARTESIAN_POINT('Ctrl Pts',(-25.7985186537236,57.3581011436976,
40.0619155352442));
#171450=CARTESIAN_POINT('Ctrl Pts',(-25.7985010085883,57.3581298146205,
40.0619457972351));
#171451=CARTESIAN_POINT('Ctrl Pts',(-25.7984833547786,57.3581584863396,
40.0619760547305));
#171452=CARTESIAN_POINT('Ctrl Pts',(-25.7984656922961,57.3581871588521,
40.0620063077269));
#171453=CARTESIAN_POINT('Ctrl Pts',(-25.7965719149858,57.3612614352675,
40.06525004417));
#171454=CARTESIAN_POINT('Ctrl Pts',(-25.7945784837693,57.3643429325989,
40.0684393223557));
#171455=CARTESIAN_POINT('Ctrl Pts',(-25.7924880141961,57.3674274658678,
40.0715697951759));
#171456=CARTESIAN_POINT('Ctrl Pts',(-25.7808550263345,57.3845921921739,
40.0889901646399));
#171457=CARTESIAN_POINT('Ctrl Pts',(-25.7662212180103,57.4018536888691,
40.1045963098205));
#171458=CARTESIAN_POINT('Ctrl Pts',(-25.7490920431318,57.4184830023364,
40.1176634650677));
#171459=CARTESIAN_POINT('Ctrl Pts',(-25.7414042322328,57.4259464685117,
40.1235281853033));
#171460=CARTESIAN_POINT('Ctrl Pts',(-25.7332138190191,57.4332829501997,
40.1288820140907));
#171461=CARTESIAN_POINT('Ctrl Pts',(-25.7245659119506,57.4404287135114,
40.1336621774101));
#171462=CARTESIAN_POINT('Ctrl Pts',(-25.7208076485109,57.4435341655925,
40.1357395717319));
#171463=CARTESIAN_POINT('Ctrl Pts',(-25.716963033262,57.4466034003414,40.1377083672884));
#171464=CARTESIAN_POINT('Ctrl Pts',(-25.7130358078099,57.4496310617744,
40.1395632548792));
#171465=CARTESIAN_POINT('Ctrl Pts',(-25.6992905187276,57.46022787679,40.146055361447));
#171466=CARTESIAN_POINT('Ctrl Pts',(-25.6845332533377,57.4703154157424,
40.1511520974629));
#171467=CARTESIAN_POINT('Ctrl Pts',(-25.6689244402251,57.4796640570499,
40.1546258197408));
#171468=CARTESIAN_POINT('Ctrl Pts',(-25.6611200336689,57.4843383777037,
40.1563626808798));
#171469=CARTESIAN_POINT('Ctrl Pts',(-25.6531027404315,57.4888279745008,
40.1576937882008));
#171470=CARTESIAN_POINT('Ctrl Pts',(-25.6448926173138,57.4931041519766,
40.1585906813668));
#171471=CARTESIAN_POINT('Ctrl Pts',(-25.6407875557549,57.4952422407145,
40.1590391279498));
#171472=CARTESIAN_POINT('Ctrl Pts',(-25.636634286776,57.4973269747347,40.1593790209175));
#171473=CARTESIAN_POINT('Ctrl Pts',(-25.6324353177602,57.4993547677438,
40.1596068022931));
#171474=CARTESIAN_POINT('Ctrl Pts',(-25.6282363487445,57.5013825607529,
40.1598345836687));
#171475=CARTESIAN_POINT('Ctrl Pts',(-25.6239916789975,57.5033534111924,
40.1599502506865));
#171476=CARTESIAN_POINT('Ctrl Pts',(-25.6197038181293,57.5052637377734,
40.1599502534424));
#171477=CARTESIAN_POINT('',(-25.5918112338789,57.5176823163891,40.1599502534424));
#171478=CARTESIAN_POINT('Origin',(2.35274110347535E-17,-1.41976521077031E-16,
40.1599502534424));
#171479=CARTESIAN_POINT('',(-25.2380597013425,57.4675553545143,39.8576902534424));
#171480=CARTESIAN_POINT('Ctrl Pts',(-25.5918112338789,57.5176823163891,
40.1599502534424));
#171481=CARTESIAN_POINT('Ctrl Pts',(-25.5883196330409,57.5192358568903,
40.1599502447858));
#171482=CARTESIAN_POINT('Ctrl Pts',(-25.5848181941914,57.5207415321517,
40.1598744685927));
#171483=CARTESIAN_POINT('Ctrl Pts',(-25.5813091362503,57.5221995827245,
40.1597246934279));
#171484=CARTESIAN_POINT('Ctrl Pts',(-25.5610311102455,57.5306253163333,
40.1588591777435));
#171485=CARTESIAN_POINT('Ctrl Pts',(-25.5404968219571,57.5374634601474,
40.1555254706023));
#171486=CARTESIAN_POINT('Ctrl Pts',(-25.5201405094577,57.5427567781065,
40.1500631826386));
#171487=CARTESIAN_POINT('Ctrl Pts',(-25.5119303403506,57.5448916950067,
40.1478601162485));
#171488=CARTESIAN_POINT('Ctrl Pts',(-25.5037488853983,57.546775718186,40.1453112228309));
#171489=CARTESIAN_POINT('Ctrl Pts',(-25.4956235123961,57.548413124991,40.1424401896328));
#171490=CARTESIAN_POINT('Ctrl Pts',(-25.4926257430706,57.5490172286908,
40.1413809526906));
#171491=CARTESIAN_POINT('Ctrl Pts',(-25.4896356883473,57.5495876573341,
40.1402777640512));
#171492=CARTESIAN_POINT('Ctrl Pts',(-25.4866547635669,57.55012457403,40.1391317641987));
#171493=CARTESIAN_POINT('Ctrl Pts',(-25.4810655296036,57.5511312928347,
40.1369830144753));
#171494=CARTESIAN_POINT('Ctrl Pts',(-25.4755083930932,57.5520201961936,
40.134683756585));
#171495=CARTESIAN_POINT('Ctrl Pts',(-25.4699926837172,57.5527923593832,
40.1322415082996));
#171496=CARTESIAN_POINT('Ctrl Pts',(-25.4506877009012,57.5554949305467,
40.1236936393009));
#171497=CARTESIAN_POINT('Ctrl Pts',(-25.4318901986623,57.5567674305413,
40.113394140767));
#171498=CARTESIAN_POINT('Ctrl Pts',(-25.4140001974202,57.5566559849707,
40.101665321223));
#171499=CARTESIAN_POINT('Ctrl Pts',(-25.4050551967992,57.5566002621853,
40.095800911451));
#171500=CARTESIAN_POINT('Ctrl Pts',(-25.3963370718384,57.5561985539315,
40.0895791707949));
#171501=CARTESIAN_POINT('Ctrl Pts',(-25.3878958286608,57.5554566340483,
40.0830403822907));
#171502=CARTESIAN_POINT('Ctrl Pts',(-25.383675207072,57.5550856741067,40.0797709880385));
#171503=CARTESIAN_POINT('Ctrl Pts',(-25.3795238059759,57.5546296613654,
40.0764223317514));
#171504=CARTESIAN_POINT('Ctrl Pts',(-25.3754478763491,57.5540893180427,
40.0729994484778));
#171505=CARTESIAN_POINT('Ctrl Pts',(-25.3713719467224,57.55354897472,40.0695765652042));
#171506=CARTESIAN_POINT('Ctrl Pts',(-25.3673715770251,57.5529242061382,
40.0660793733488));
#171507=CARTESIAN_POINT('Ctrl Pts',(-25.3634528381782,57.5522159293601,
40.0625130768817));
#171508=CARTESIAN_POINT('Ctrl Pts',(-25.363419419543,57.5522098892426,40.0624826638418));
#171509=CARTESIAN_POINT('Ctrl Pts',(-25.3633860069328,57.5522038431596,
40.0624522459912));
#171510=CARTESIAN_POINT('Ctrl Pts',(-25.3633526003507,57.5521977911121,
40.0624218233329));
#171511=CARTESIAN_POINT('Ctrl Pts',(-25.346291371152,57.5491069220866,40.0468845275908));
#171512=CARTESIAN_POINT('Ctrl Pts',(-25.3307446654471,57.5445791409896,
40.0302263329257));
#171513=CARTESIAN_POINT('Ctrl Pts',(-25.3167379215577,57.5388132486365,
40.0127515884774));
#171514=CARTESIAN_POINT('Ctrl Pts',(-25.3022574788908,57.5328523576327,
39.9946858597756));
#171515=CARTESIAN_POINT('Ctrl Pts',(-25.2894223267617,57.5255675223694,
39.9757460620541));
#171516=CARTESIAN_POINT('Ctrl Pts',(-25.2783002469356,57.5171444507329,
39.9562444559191));
#171517=CARTESIAN_POINT('Ctrl Pts',(-25.267389732471,57.5088816036429,39.9371138113683));
#171518=CARTESIAN_POINT('Ctrl Pts',(-25.2581274647609,57.4995225236683,
39.9174410654434));
#171519=CARTESIAN_POINT('Ctrl Pts',(-25.2506209171167,57.4892225138723,
39.8975196504236));
#171520=CARTESIAN_POINT('Ctrl Pts',(-25.2456480924691,57.482399118483,39.8843224113835));
#171521=CARTESIAN_POINT('Ctrl Pts',(-25.2414466709171,57.4751623993628,
39.8710160447162));
#171522=CARTESIAN_POINT('Ctrl Pts',(-25.2380597013425,57.4675553545143,
39.8576902534424));
#171523=CARTESIAN_POINT('',(-25.0931373005741,57.1420619865023,39.2875012672119));
#171524=CARTESIAN_POINT('',(-25.2380597013425,57.4675553545143,39.8576902534424));
#171525=CARTESIAN_POINT('',(-19.5876674457073,59.2554138597573,39.2875012672119));
#171526=CARTESIAN_POINT('Origin',(5.53234440788222E-15,0.,39.2875012672119));
#171527=CARTESIAN_POINT('',(-19.697766688184,59.5942745858238,39.8576902534424));
#171528=CARTESIAN_POINT('',(-19.5876674457073,59.2554138597573,39.2875012672119));
#171529=CARTESIAN_POINT('',(-19.4684195516691,59.8682321556243,40.1599502534424));
#171530=CARTESIAN_POINT('Ctrl Pts',(-19.697766688184,59.5942745858238,39.8576902534424));
#171531=CARTESIAN_POINT('Ctrl Pts',(-19.7015693056583,59.6059782661673,
39.8773836120336));
#171532=CARTESIAN_POINT('Ctrl Pts',(-19.7035046472587,59.6182462127092,
39.8969946442077));
#171533=CARTESIAN_POINT('Ctrl Pts',(-19.7035948839462,59.630890804279,39.9162525288159));
#171534=CARTESIAN_POINT('Ctrl Pts',(-19.7036869338405,59.6437894749834,
39.9358973793953));
#171535=CARTESIAN_POINT('Ctrl Pts',(-19.7018593121361,59.657080948502,39.9551762199603));
#171536=CARTESIAN_POINT('Ctrl Pts',(-19.6980881582825,59.6705908046714,
39.9738152034081));
#171537=CARTESIAN_POINT('Ctrl Pts',(-19.6944635103376,59.6835758151756,
39.9917300792457));
#171538=CARTESIAN_POINT('Ctrl Pts',(-19.6890433025229,59.696763446391,40.0090551157911));
#171539=CARTESIAN_POINT('Ctrl Pts',(-19.6817621015947,59.7100083536123,
40.0255394551304));
#171540=CARTESIAN_POINT('Ctrl Pts',(-19.6761689357012,59.7201826317381,
40.0382021526002));
#171541=CARTESIAN_POINT('Ctrl Pts',(-19.6694767982745,59.7303909886912,
40.0503687782053));
#171542=CARTESIAN_POINT('Ctrl Pts',(-19.6616375006935,59.7405669736109,
40.0619155352442));
#171543=CARTESIAN_POINT('Ctrl Pts',(-19.6616169552927,59.7405936430526,
40.0619457972351));
#171544=CARTESIAN_POINT('Ctrl Pts',(-19.6615964011817,59.7406203123794,
40.0619760547305));
#171545=CARTESIAN_POINT('Ctrl Pts',(-19.6615758383624,59.7406469815887,
40.0620063077269));
#171546=CARTESIAN_POINT('Ctrl Pts',(-19.659371085973,59.7435064631643,40.06525004417));
#171547=CARTESIAN_POINT('Ctrl Pts',(-19.6570664708007,59.7463627094292,
40.0684393223557));
#171548=CARTESIAN_POINT('Ctrl Pts',(-19.654665031516,59.7492118317301,40.0715697951759));
#171549=CARTESIAN_POINT('Ctrl Pts',(-19.6413015679145,59.7650665495268,
40.0889901646418));
#171550=CARTESIAN_POINT('Ctrl Pts',(-19.6249436073982,59.7807038364427,
40.1045963098238));
#171551=CARTESIAN_POINT('Ctrl Pts',(-19.6061700313475,59.7954515664652,
40.1176634650719));
#171552=CARTESIAN_POINT('Ctrl Pts',(-19.5977441904328,59.8020705519311,
40.1235281853059));
#171553=CARTESIAN_POINT('Ctrl Pts',(-19.588831774005,59.8085107122964,40.1288820140919));
#171554=CARTESIAN_POINT('Ctrl Pts',(-19.5794843054207,59.8147133779312,
40.1336621774101));
#171555=CARTESIAN_POINT('Ctrl Pts',(-19.5754220220075,59.817408972519,40.1357395717319));
#171556=CARTESIAN_POINT('Ctrl Pts',(-19.5712776455715,59.820059521955,40.1377083672884));
#171557=CARTESIAN_POINT('Ctrl Pts',(-19.5670554570745,59.8226600907005,
40.1395632548792));
#171558=CARTESIAN_POINT('Ctrl Pts',(-19.5522777973348,59.8317620813097,
40.146055361447));
#171559=CARTESIAN_POINT('Ctrl Pts',(-19.5365469388439,59.840251805395,40.151152097463));
#171560=CARTESIAN_POINT('Ctrl Pts',(-19.5200464333333,59.8479176686192,
40.1546258197409));
#171561=CARTESIAN_POINT('Ctrl Pts',(-19.5117961805779,59.8517506002313,
40.1563626808798));
#171562=CARTESIAN_POINT('Ctrl Pts',(-19.5033535162579,59.8553775672056,
40.1576937882008));
#171563=CARTESIAN_POINT('Ctrl Pts',(-19.4947413867934,59.8587721277811,
40.1585906813668));
#171564=CARTESIAN_POINT('Ctrl Pts',(-19.4904353220612,59.8604694080688,
40.1590391279498));
#171565=CARTESIAN_POINT('Ctrl Pts',(-19.4860868910809,59.862108586874,40.1593790209175));
#171566=CARTESIAN_POINT('Ctrl Pts',(-19.4816989623697,59.8636863596423,
40.1596068022931));
#171567=CARTESIAN_POINT('Ctrl Pts',(-19.4773110336584,59.8652641324106,
40.1598345836687));
#171568=CARTESIAN_POINT('Ctrl Pts',(-19.4728836066887,59.8667804975194,
40.1599502506865));
#171569=CARTESIAN_POINT('Ctrl Pts',(-19.4684195516691,59.8682321556243,
40.1599502534424));
#171570=CARTESIAN_POINT('',(-19.4393816709751,59.8776671349987,40.1599502534424));
#171571=CARTESIAN_POINT('Origin',(8.34054140790793E-18,-1.47806214131551E-16,
40.1599502534424));
#171572=CARTESIAN_POINT('',(-19.0928077206406,59.7908376697913,39.8576902534424));
#171573=CARTESIAN_POINT('Ctrl Pts',(-19.4393816709751,59.8776671349987,
40.1599502534424));
#171574=CARTESIAN_POINT('Ctrl Pts',(-19.4357468082906,59.8788471933726,
40.1599502447858));
#171575=CARTESIAN_POINT('Ctrl Pts',(-19.4321071647682,59.8799786203652,
40.1598744685927));
#171576=CARTESIAN_POINT('Ctrl Pts',(-19.4284649220279,59.8810618871503,
40.1597246934279));
#171577=CARTESIAN_POINT('Ctrl Pts',(-19.4074172521851,59.8873218328125,
40.1588591777435));
#171578=CARTESIAN_POINT('Ctrl Pts',(-19.3862806722119,59.8919760989602,
40.1555254706022));
#171579=CARTESIAN_POINT('Ctrl Pts',(-19.3654825713304,59.8951126055063,
40.1500631826385));
#171580=CARTESIAN_POINT('Ctrl Pts',(-19.3570942188061,59.8963776307484,
40.1478601162485));
#171581=CARTESIAN_POINT('Ctrl Pts',(-19.3487606486724,59.8973961381381,
40.1453112228309));
#171582=CARTESIAN_POINT('Ctrl Pts',(-19.3405086316967,59.8981752423038,
40.1424401896328));
#171583=CARTESIAN_POINT('Ctrl Pts',(-19.3374641384338,59.8984626844396,
40.1413809526906));
#171584=CARTESIAN_POINT('Ctrl Pts',(-19.3344308375137,59.8987174423898,
40.1402777640512));
#171585=CARTESIAN_POINT('Ctrl Pts',(-19.331410119474,59.8989398263134,40.1391317641987));
#171586=CARTESIAN_POINT('Ctrl Pts',(-19.3257462731495,59.8993567961702,
40.1369830144753));
#171587=CARTESIAN_POINT('Ctrl Pts',(-19.3201266635123,59.8996599510838,
40.134683756585));
#171588=CARTESIAN_POINT('Ctrl Pts',(-19.3145604567378,59.8998513356578,
40.1322415082996));
#171589=CARTESIAN_POINT('Ctrl Pts',(-19.295078733027,59.9005211816666,40.1236936393009));
#171590=CARTESIAN_POINT('Ctrl Pts',(-19.2762511930033,59.8998218367507,
40.113394140767));
#171591=CARTESIAN_POINT('Ctrl Pts',(-19.258470844294,59.8978409873529,40.101665321223));
#171592=CARTESIAN_POINT('Ctrl Pts',(-19.2495806699394,59.896850562654,40.095800911451));
#171593=CARTESIAN_POINT('Ctrl Pts',(-19.2409522937258,59.8955397627953,
40.0895791707949));
#171594=CARTESIAN_POINT('Ctrl Pts',(-19.2326348443069,59.8939195570494,
40.0830403822906));
#171595=CARTESIAN_POINT('Ctrl Pts',(-19.2284761195974,59.8931094541764,
40.0797709880385));
#171596=CARTESIAN_POINT('Ctrl Pts',(-19.2243951266219,59.8922219999437,
40.0764223317514));
#171597=CARTESIAN_POINT('Ctrl Pts',(-19.2203980066213,59.891258566018,40.0729994484778));
#171598=CARTESIAN_POINT('Ctrl Pts',(-19.2164008866207,59.8902951320922,
40.0695765652043));
#171599=CARTESIAN_POINT('Ctrl Pts',(-19.2124877374669,59.8892556335611,
40.0660793733488));
#171600=CARTESIAN_POINT('Ctrl Pts',(-19.2086645009646,59.8881416170477,
40.0625130768816));
#171601=CARTESIAN_POINT('Ctrl Pts',(-19.2086318967643,59.88813211682,40.0624826638418));
#171602=CARTESIAN_POINT('Ctrl Pts',(-19.2085992991797,59.8881226112893,
40.0624522459912));
#171603=CARTESIAN_POINT('Ctrl Pts',(-19.2085667082136,59.8881131004569,
40.0624218233329));
#171604=CARTESIAN_POINT('Ctrl Pts',(-19.1919220260049,59.8832557794662,
40.0468845275925));
#171605=CARTESIAN_POINT('Ctrl Pts',(-19.1769337687821,59.8771277287725,
40.0302263329295));
#171606=CARTESIAN_POINT('Ctrl Pts',(-19.1636064551696,59.8699293191679,
40.0127515884834));
#171607=CARTESIAN_POINT('Ctrl Pts',(-19.1498284206602,59.8624874641303,
39.9946858597837));
#171608=CARTESIAN_POINT('Ctrl Pts',(-19.1378250534734,59.8539008972302,
39.9757460620646));
#171609=CARTESIAN_POINT('Ctrl Pts',(-19.1276443522988,59.8443613941504,
39.956244455932));
#171610=CARTESIAN_POINT('Ctrl Pts',(-19.1176573094827,59.8350033524921,
39.9371138113831));
#171611=CARTESIAN_POINT('Ctrl Pts',(-19.1094240716913,59.8247273719282,
39.9174410654602));
#171612=CARTESIAN_POINT('Ctrl Pts',(-19.1030352898955,59.8136991387752,
39.8975196504422));
#171613=CARTESIAN_POINT('Ctrl Pts',(-19.0988029459332,59.8063933209382,
39.8843224113961));
#171614=CARTESIAN_POINT('Ctrl Pts',(-19.0953809833347,59.7987570771807,
39.8710160447225));
#171615=CARTESIAN_POINT('Ctrl Pts',(-19.0928077206406,59.7908376697913,
39.8576902534424));
#171616=CARTESIAN_POINT('',(-18.9827025415091,59.4519788726609,39.2875012672119));
#171617=CARTESIAN_POINT('',(-19.0928077206406,59.7908376697913,39.8576902534424));
#171618=CARTESIAN_POINT('',(-13.2864868028989,60.9782752797349,39.2875012672119));
#171619=CARTESIAN_POINT('Origin',(5.53234440788222E-15,0.,39.2875012672119));
#171620=CARTESIAN_POINT('',(-13.360562319248,61.3267881959114,39.8576902534424));
#171621=CARTESIAN_POINT('',(-13.2864868028989,60.9782752797349,39.2875012672119));
#171622=CARTESIAN_POINT('',(-13.1038352065721,61.5752716937453,40.1599502534424));
#171623=CARTESIAN_POINT('Ctrl Pts',(-13.360562319248,61.3267881959114,39.8576902534424));
#171624=CARTESIAN_POINT('Ctrl Pts',(-13.3631207378653,61.338825244031,39.8773836120346));
#171625=CARTESIAN_POINT('Ctrl Pts',(-13.3637631278625,61.3512282837622,
39.8969946442097));
#171626=CARTESIAN_POINT('Ctrl Pts',(-13.3625311504983,61.3638130392393,
39.9162525288189));
#171627=CARTESIAN_POINT('Ctrl Pts',(-13.3612744179065,61.3766506715107,
39.9358973793994));
#171628=CARTESIAN_POINT('Ctrl Pts',(-13.3580674708029,61.3896782944593,
39.9551762199655));
#171629=CARTESIAN_POINT('Ctrl Pts',(-13.3529048112197,61.4027199493068,
39.9738152034143));
#171630=CARTESIAN_POINT('Ctrl Pts',(-13.3479427162811,61.415254947686,39.991730079253));
#171631=CARTESIAN_POINT('Ctrl Pts',(-13.3411737181058,61.4278037696853,
40.0090551157994));
#171632=CARTESIAN_POINT('Ctrl Pts',(-13.3325479345589,61.440215027176,40.0255394551395));
#171633=CARTESIAN_POINT('Ctrl Pts',(-13.325921906957,61.4497489245037,40.038202152606));
#171634=CARTESIAN_POINT('Ctrl Pts',(-13.3181993658961,61.4592018401658,
40.0503687782081));
#171635=CARTESIAN_POINT('Ctrl Pts',(-13.3093393327438,61.468502650244,40.0619155352442));
#171636=CARTESIAN_POINT('Ctrl Pts',(-13.309316112177,61.4685270260085,40.0619457972351));
#171637=CARTESIAN_POINT('Ctrl Pts',(-13.3092928829598,61.4685514007483,
40.0619760547305));
#171638=CARTESIAN_POINT('Ctrl Pts',(-13.3092696450943,61.468575774461,40.0620063077269));
#171639=CARTESIAN_POINT('Ctrl Pts',(-13.3067780733544,61.4711891321182,
40.06525004417));
#171640=CARTESIAN_POINT('Ctrl Pts',(-13.3041875240723,61.4737888336848,
40.0684393223556));
#171641=CARTESIAN_POINT('Ctrl Pts',(-13.3015014257475,61.4763713294375,
40.0715697951759));
#171642=CARTESIAN_POINT('Ctrl Pts',(-13.2865538993096,61.4907423311184,
40.0889901646434));
#171643=CARTESIAN_POINT('Ctrl Pts',(-13.2686510078396,61.5045840828668,
40.1045963098267));
#171644=CARTESIAN_POINT('Ctrl Pts',(-13.2484387178445,61.5172886502275,
40.1176634650756));
#171645=CARTESIAN_POINT('Ctrl Pts',(-13.2393671621905,61.5229906359946,
40.1235281853082));
#171646=CARTESIAN_POINT('Ctrl Pts',(-13.2298303888482,61.5284639152932,
40.1288820140929));
#171647=CARTESIAN_POINT('Ctrl Pts',(-13.2198857715699,61.5336555255489,
40.1336621774101));
#171648=CARTESIAN_POINT('Ctrl Pts',(-13.2155639754105,61.535911729145,40.1357395717319));
#171649=CARTESIAN_POINT('Ctrl Pts',(-13.2111652444429,61.5381145532938,
40.1377083672884));
#171650=CARTESIAN_POINT('Ctrl Pts',(-13.2066943520817,61.5402595369764,
40.1395632548792));
#171651=CARTESIAN_POINT('Ctrl Pts',(-13.1910462288172,61.5477669798654,
40.146055361447));
#171652=CARTESIAN_POINT('Ctrl Pts',(-13.1745141278029,61.5545658738899,
40.1511520974629));
#171653=CARTESIAN_POINT('Ctrl Pts',(-13.1573027128854,61.5604649702291,
40.1546258197408));
#171654=CARTESIAN_POINT('Ctrl Pts',(-13.1486970054267,61.5634145183987,
40.1563626808798));
#171655=CARTESIAN_POINT('Ctrl Pts',(-13.1399214696211,61.5661391177412,
40.1576937882008));
#171656=CARTESIAN_POINT('Ctrl Pts',(-13.1310016901025,61.5686148699003,
40.1585906813668));
#171657=CARTESIAN_POINT('Ctrl Pts',(-13.1265418003432,61.5698527459798,
40.1590391279498));
#171658=CARTESIAN_POINT('Ctrl Pts',(-13.1220458496812,61.571028410384,40.1593790209175));
#171659=CARTESIAN_POINT('Ctrl Pts',(-13.1175170363398,61.5721388765029,
40.1596068022931));
#171660=CARTESIAN_POINT('Ctrl Pts',(-13.1129882229983,61.5732493426218,
40.1598345836687));
#171661=CARTESIAN_POINT('Ctrl Pts',(-13.1084265466222,61.5742946087865,
40.1599502506865));
#171662=CARTESIAN_POINT('Ctrl Pts',(-13.1038352065721,61.5752716937453,
40.1599502534424));
#171663=CARTESIAN_POINT('',(-13.0739701745318,61.5816197022699,40.1599502534424));
#171664=CARTESIAN_POINT('Origin',(-7.37250181440935E-18,-1.52016511373604E-16,
40.1599502534424));
#171665=CARTESIAN_POINT('',(-12.7383709431244,61.459039055521,39.8576902534424));
#171666=CARTESIAN_POINT('Ctrl Pts',(-13.0739701745318,61.5816197022699,
40.1599502534424));
#171667=CARTESIAN_POINT('Ctrl Pts',(-13.0702318743171,61.5824133495499,
40.1599502447858));
#171668=CARTESIAN_POINT('Ctrl Pts',(-13.0664939028179,61.5831581321229,
40.1598744685927));
#171669=CARTESIAN_POINT('Ctrl Pts',(-13.0627583804521,61.5838547466227,
40.1597246934279));
#171670=CARTESIAN_POINT('Ctrl Pts',(-13.0411716694483,61.5878803190632,
40.1588591777436));
#171671=CARTESIAN_POINT('Ctrl Pts',(-13.0196643745853,61.5902997144306,
40.1555254706027));
#171672=CARTESIAN_POINT('Ctrl Pts',(-12.9986523536687,61.5912450453417,
40.1500631826397));
#171673=CARTESIAN_POINT('Ctrl Pts',(-12.9901777222711,61.5916263190447,
40.1478601162494));
#171674=CARTESIAN_POINT('Ctrl Pts',(-12.9817833412928,61.5917681516648,
40.1453112228314));
#171675=CARTESIAN_POINT('Ctrl Pts',(-12.9734950911668,61.591680417163,40.1424401896328));
#171676=CARTESIAN_POINT('Ctrl Pts',(-12.9704372300719,61.5916480484585,
40.1413809526906));
#171677=CARTESIAN_POINT('Ctrl Pts',(-12.9673939164345,61.5915843445342,
40.1402777640511));
#171678=CARTESIAN_POINT('Ctrl Pts',(-12.9643665007545,61.5914897592007,
40.1391317641987));
#171679=CARTESIAN_POINT('Ctrl Pts',(-12.9586900963545,61.5913124117005,
40.1369830144753));
#171680=CARTESIAN_POINT('Ctrl Pts',(-12.9530695832096,61.5910264967403,
40.134683756585));
#171681=CARTESIAN_POINT('Ctrl Pts',(-12.9475138635627,61.5906350058492,
40.1322415082996));
#171682=CARTESIAN_POINT('Ctrl Pts',(-12.9280688447989,61.5892647877302,
40.1236936393009));
#171683=CARTESIAN_POINT('Ctrl Pts',(-12.9094175454587,61.5866012600731,
40.113394140767));
#171684=CARTESIAN_POINT('Ctrl Pts',(-12.8919416545036,61.5827727094486,
40.101665321223));
#171685=CARTESIAN_POINT('Ctrl Pts',(-12.8832037090261,61.5808584341363,
40.095800911451));
#171686=CARTESIAN_POINT('Ctrl Pts',(-12.8747596158551,61.5786529040703,
40.0895791707949));
#171687=CARTESIAN_POINT('Ctrl Pts',(-12.8666570879111,61.5761721637749,
40.0830403822906));
#171688=CARTESIAN_POINT('Ctrl Pts',(-12.8626058239391,61.5749317936273,
40.0797709880385));
#171689=CARTESIAN_POINT('Ctrl Pts',(-12.8586399512973,61.5736226210373,
40.0764223317514));
#171690=CARTESIAN_POINT('Ctrl Pts',(-12.854765434206,61.5722466520923,40.0729994484778));
#171691=CARTESIAN_POINT('Ctrl Pts',(-12.8508909171147,61.5708706831473,
40.0695765652042));
#171692=CARTESIAN_POINT('Ctrl Pts',(-12.8471078617854,61.5694278436303,
40.0660793733488));
#171693=CARTESIAN_POINT('Ctrl Pts',(-12.8434220158069,61.5679202927797,
40.0625130768816));
#171694=CARTESIAN_POINT('Ctrl Pts',(-12.8433905832601,61.5679074365282,
40.0624826638418));
#171695=CARTESIAN_POINT('Ctrl Pts',(-12.8433591578469,61.5678945756944,
40.0624522459912));
#171696=CARTESIAN_POINT('Ctrl Pts',(-12.8433277395702,61.5678817102797,
40.0624218233329));
#171697=CARTESIAN_POINT('Ctrl Pts',(-12.827281966969,61.561311155148,40.0468845275905));
#171698=CARTESIAN_POINT('Ctrl Pts',(-12.8130163727078,61.5536499750614,
40.0302263329252));
#171699=CARTESIAN_POINT('Ctrl Pts',(-12.8005145062063,61.5450979154851,
40.0127515884767));
#171700=CARTESIAN_POINT('Ctrl Pts',(-12.7875898348814,61.5362566309327,
39.9946858597746));
#171701=CARTESIAN_POINT('Ctrl Pts',(-12.7765497640382,61.5264624086169,
39.9757460620528));
#171702=CARTESIAN_POINT('Ctrl Pts',(-12.7674219834069,61.5159109908826,
39.9562444559174));
#171703=CARTESIAN_POINT('Ctrl Pts',(-12.75846783237,61.505560283316,39.9371138113663));
#171704=CARTESIAN_POINT('Ctrl Pts',(-12.751353829574,61.4944799879532,39.917441065441));
#171705=CARTESIAN_POINT('Ctrl Pts',(-12.7461528104583,61.4828443590704,
39.8975196504208));
#171706=CARTESIAN_POINT('Ctrl Pts',(-12.7427073176332,61.4751361628615,
39.8843224113816));
#171707=CARTESIAN_POINT('Ctrl Pts',(-12.7401023057309,61.4671840587587,
39.8710160447152));
#171708=CARTESIAN_POINT('Ctrl Pts',(-12.7383709431244,61.459039055521,39.8576902534424));
#171709=CARTESIAN_POINT('',(-12.6642893210135,61.1105274371642,39.2875012672119));
#171710=CARTESIAN_POINT('',(-12.7383709431244,61.459039055521,39.8576902534424));
#171711=CARTESIAN_POINT('',(-6.83973663030197,62.0330459552233,39.2875012672119));
#171712=CARTESIAN_POINT('Origin',(5.53234440788222E-15,0.,39.2875012672119));
#171713=CARTESIAN_POINT('',(-6.87697683366501,62.3873926810692,39.8576902534424));
#171714=CARTESIAN_POINT('',(-6.83973663030197,62.0330459552233,39.2875012672119));
#171715=CARTESIAN_POINT('',(-6.59568250079822,62.6076796697355,40.1599502534424));
#171716=CARTESIAN_POINT('Ctrl Pts',(-6.87697683366501,62.3873926810692,
39.8576902534424));
#171717=CARTESIAN_POINT('Ctrl Pts',(-6.87826302285531,62.3996312165479,
39.8773836120375));
#171718=CARTESIAN_POINT('Ctrl Pts',(-6.87760542308951,62.4120334591708,
39.8969946442153));
#171719=CARTESIAN_POINT('Ctrl Pts',(-6.87506472947472,62.4244204973417,
39.9162525288272));
#171720=CARTESIAN_POINT('Ctrl Pts',(-6.87247298342128,62.4370564393956,
39.9358973794105));
#171721=CARTESIAN_POINT('Ctrl Pts',(-6.86792184690122,62.4496774784119,
39.9551762199791));
#171722=CARTESIAN_POINT('Ctrl Pts',(-6.86142424476564,62.4621080448385,
39.9738152034302));
#171723=CARTESIAN_POINT('Ctrl Pts',(-6.85517906858276,62.4740556950282,
39.9917300792711));
#171724=CARTESIAN_POINT('Ctrl Pts',(-6.84713544260583,62.4858282202919,
40.0090551158194));
#171725=CARTESIAN_POINT('Ctrl Pts',(-6.83725958232801,62.4972698477182,
40.0255394551612));
#171726=CARTESIAN_POINT('Ctrl Pts',(-6.82967328916514,62.5060589088707,
40.0382021526199));
#171727=CARTESIAN_POINT('Ctrl Pts',(-6.82100495424893,62.5146528151171,
40.0503687782147));
#171728=CARTESIAN_POINT('Ctrl Pts',(-6.81122125790617,62.5229765487298,
40.0619155352442));
#171729=CARTESIAN_POINT('Ctrl Pts',(-6.81119561658286,62.5229983637512,
40.0619457972351));
#171730=CARTESIAN_POINT('Ctrl Pts',(-6.81116996676367,62.5230201768493,
40.0619760547305));
#171731=CARTESIAN_POINT('Ctrl Pts',(-6.81114430845093,62.5230419880218,
40.0620063077269));
#171732=CARTESIAN_POINT('Ctrl Pts',(-6.80839321554184,62.5253805892672,
40.06525004417));
#171733=CARTESIAN_POINT('Ctrl Pts',(-6.80554511475005,62.5276952632612,
40.0684393223556));
#171734=CARTESIAN_POINT('Ctrl Pts',(-6.80260378684053,62.5299828381019,
40.0715697951759));
#171735=CARTESIAN_POINT('Ctrl Pts',(-6.78623596579978,62.5427126719601,
40.0889901646384));
#171736=CARTESIAN_POINT('Ctrl Pts',(-6.76698429120954,62.5546072354075,
40.1045963098178));
#171737=CARTESIAN_POINT('Ctrl Pts',(-6.74555473735862,62.5651294462044,
40.1176634650644));
#171738=CARTESIAN_POINT('Ctrl Pts',(-6.73593685682031,62.5698519601282,
40.1235281853013));
#171739=CARTESIAN_POINT('Ctrl Pts',(-6.72588021343989,62.5742983919711,
40.1288820140898));
#171740=CARTESIAN_POINT('Ctrl Pts',(-6.71544740276709,62.5784220664834,
40.1336621774101));
#171741=CARTESIAN_POINT('Ctrl Pts',(-6.71091344436445,62.580214159649,40.1357395717319));
#171742=CARTESIAN_POINT('Ctrl Pts',(-6.70630855228228,62.5819451239083,
40.1377083672884));
#171743=CARTESIAN_POINT('Ctrl Pts',(-6.70163794008908,62.5836110216379,
40.1395632548792));
#171744=CARTESIAN_POINT('Ctrl Pts',(-6.6852907974129,62.5894416636914,40.146055361447));
#171745=CARTESIAN_POINT('Ctrl Pts',(-6.66813858303337,62.5944752375495,
40.151152097463));
#171746=CARTESIAN_POINT('Ctrl Pts',(-6.65040483057272,62.5985429352697,
40.1546258197409));
#171747=CARTESIAN_POINT('Ctrl Pts',(-6.6415379543424,62.6005767841298,40.1563626808798));
#171748=CARTESIAN_POINT('Ctrl Pts',(-6.63252569365777,62.6023691645599,
40.1576937882008));
#171749=CARTESIAN_POINT('Ctrl Pts',(-6.62339599105606,62.6038989834438,
40.1585906813668));
#171750=CARTESIAN_POINT('Ctrl Pts',(-6.6188311397552,62.6046638928858,40.1590391279498));
#171751=CARTESIAN_POINT('Ctrl Pts',(-6.61423692798793,62.6053631620638,
40.1593790209175));
#171752=CARTESIAN_POINT('Ctrl Pts',(-6.60961684864287,62.6059941550341,
40.1596068022931));
#171753=CARTESIAN_POINT('Ctrl Pts',(-6.60499676929781,62.6066251480043,
40.1598345836687));
#171754=CARTESIAN_POINT('Ctrl Pts',(-6.60035082219627,62.6071878630701,
40.1599502506865));
#171755=CARTESIAN_POINT('Ctrl Pts',(-6.59568250079822,62.6076796697355,
40.1599502534424));
#171756=CARTESIAN_POINT('',(-6.56531752495238,62.6108711573006,40.1599502534424));
#171757=CARTESIAN_POINT('Origin',(-2.34395632424767E-17,-1.54561283905549E-16,
40.1599502534424));
#171758=CARTESIAN_POINT('',(-6.24436990787996,62.4538823482276,39.8576902534424));
#171759=CARTESIAN_POINT('Ctrl Pts',(-6.56531752495238,62.6108711573006,
40.1599502534424));
#171760=CARTESIAN_POINT('Ctrl Pts',(-6.5615167448068,62.6112696981211,40.1599502447858));
#171761=CARTESIAN_POINT('Ctrl Pts',(-6.55772139932878,62.6116196762807,
40.1598744685927));
#171762=CARTESIAN_POINT('Ctrl Pts',(-6.55393352450217,62.6119220062409,
40.1597246934279));
#171763=CARTESIAN_POINT('Ctrl Pts',(-6.5320442808587,62.6136691004462,40.1588591777436));
#171764=CARTESIAN_POINT('Ctrl Pts',(-6.51040190952723,62.6138271176316,
40.1555254706026));
#171765=CARTESIAN_POINT('Ctrl Pts',(-6.48940618067211,62.6125709156645,
40.1500631826395));
#171766=CARTESIAN_POINT('Ctrl Pts',(-6.48093812023799,62.6120642605134,
40.1478601162492));
#171767=CARTESIAN_POINT('Ctrl Pts',(-6.47257489901142,62.6113278644159,
40.1453112228313));
#171768=CARTESIAN_POINT('Ctrl Pts',(-6.46434122353972,62.6103742524841,
40.1424401896328));
#171769=CARTESIAN_POINT('Ctrl Pts',(-6.4613034971788,62.6100224275775,40.1413809526906));
#171770=CARTESIAN_POINT('Ctrl Pts',(-6.45828351400525,62.6096409597322,
40.1402777640512));
#171771=CARTESIAN_POINT('Ctrl Pts',(-6.45528256968465,62.6092304414384,
40.1391317641987));
#171772=CARTESIAN_POINT('Ctrl Pts',(-6.44965579908353,62.6084607196376,
40.1369830144753));
#171773=CARTESIAN_POINT('Ctrl Pts',(-6.44409596194913,62.6075888673476,
40.134683756585));
#171774=CARTESIAN_POINT('Ctrl Pts',(-6.43861159905708,62.6066187902475,
40.1322415082996));
#171775=CARTESIAN_POINT('Ctrl Pts',(-6.41941632893489,62.6032235203971,
40.1236936393009));
#171776=CARTESIAN_POINT('Ctrl Pts',(-6.4011456178169,62.5986249921653,40.113394140767));
#171777=CARTESIAN_POINT('Ctrl Pts',(-6.38416565413432,62.5929906867159,
40.101665321223));
#171778=CARTESIAN_POINT('Ctrl Pts',(-6.37567567229303,62.5901735339912,
40.095800911451));
#171779=CARTESIAN_POINT('Ctrl Pts',(-6.36750837741642,62.5870974379669,
40.0895791707949));
#171780=CARTESIAN_POINT('Ctrl Pts',(-6.35970954393914,62.5837833426318,
40.0830403822907));
#171781=CARTESIAN_POINT('Ctrl Pts',(-6.3558101272005,62.5821262949643,40.0797709880385));
#171782=CARTESIAN_POINT('Ctrl Pts',(-6.35200282582295,62.580409747586,40.0764223317514));
#171783=CARTESIAN_POINT('Ctrl Pts',(-6.348293361661,62.5786363190253,40.0729994484778));
#171784=CARTESIAN_POINT('Ctrl Pts',(-6.34458389749904,62.5768628904647,
40.0695765652042));
#171785=CARTESIAN_POINT('Ctrl Pts',(-6.34097238394016,62.5750325180135,
40.0660793733488));
#171786=CARTESIAN_POINT('Ctrl Pts',(-6.33746431138531,62.5731479498682,
40.0625130768817));
#171787=CARTESIAN_POINT('Ctrl Pts',(-6.33743439487346,62.5731318784489,
40.0624826638418));
#171788=CARTESIAN_POINT('Ctrl Pts',(-6.33740448593519,62.5731158032179,
40.0624522459912));
#171789=CARTESIAN_POINT('Ctrl Pts',(-6.33737458457314,62.5730997241771,
40.0624218233329));
#171790=CARTESIAN_POINT('Ctrl Pts',(-6.32210352242488,62.5648879232825,
40.0468845275916));
#171791=CARTESIAN_POINT('Ctrl Pts',(-6.30871688796368,62.555777551297,40.0302263329275));
#171792=CARTESIAN_POINT('Ctrl Pts',(-6.29717744164088,62.5459655399053,
40.0127515884803));
#171793=CARTESIAN_POINT('Ctrl Pts',(-6.28524773890592,62.5358216928037,
39.9946858597795));
#171794=CARTESIAN_POINT('Ctrl Pts',(-6.27529192173375,62.5249271226238,
39.9757460620592));
#171795=CARTESIAN_POINT('Ctrl Pts',(-6.26731706752089,62.5134793937784,
39.9562444559254));
#171796=CARTESIAN_POINT('Ctrl Pts',(-6.25949391181591,62.502249424824,39.9371138113756));
#171797=CARTESIAN_POINT('Ctrl Pts',(-6.25357708651812,62.4904862126995,
39.9174410654517));
#171798=CARTESIAN_POINT('Ctrl Pts',(-6.24962081353501,62.4783706704745,
39.8975196504329));
#171799=CARTESIAN_POINT('Ctrl Pts',(-6.24699992138311,62.4703445484983,
39.8843224113898));
#171800=CARTESIAN_POINT('Ctrl Pts',(-6.24524040122936,62.4621637089605,
39.8710160447193));
#171801=CARTESIAN_POINT('Ctrl Pts',(-6.24436990787996,62.4538823482276,
39.8576902534424));
#171802=CARTESIAN_POINT('',(-6.207123496544,62.0995362748659,39.2875012672119));
#171803=CARTESIAN_POINT('',(-6.24436990787996,62.4538823482276,39.8576902534424));
#171804=CARTESIAN_POINT('',(-0.318048871876471,62.4081695979768,39.2875012672119));
#171805=CARTESIAN_POINT('Origin',(5.53234440788222E-15,0.,39.2875012672119));
#171806=CARTESIAN_POINT('',(-0.318045750792381,62.7644678366119,39.8576902534424));
#171807=CARTESIAN_POINT('',(-0.31804887187647,62.4081695979768,39.2875012672119));
#171808=CARTESIAN_POINT('Ctrl Pts',(-0.318045750792382,62.7644678366119,
39.8576902534424));
#171809=CARTESIAN_POINT('Ctrl Pts',(-0.318045618797467,62.7767737714913,
39.8773836120359));
#171810=CARTESIAN_POINT('Ctrl Pts',(-0.316095234069849,62.7890393354375,
39.8969946442122));
#171811=CARTESIAN_POINT('Ctrl Pts',(-0.312273660576672,62.8010929413171,
39.9162525288225));
#171812=CARTESIAN_POINT('Ctrl Pts',(-0.308375296775076,62.8133887511252,
39.9358973794042));
#171813=CARTESIAN_POINT('Ctrl Pts',(-0.302529834044801,62.8254649274616,
39.9551762199713));
#171814=CARTESIAN_POINT('Ctrl Pts',(-0.294768478448722,62.8371482135778,
39.9738152034211));
#171815=CARTESIAN_POINT('Ctrl Pts',(-0.287308644481687,62.8483776146195,
39.9917300792606));
#171816=CARTESIAN_POINT('Ctrl Pts',(-0.278078518356449,62.8592448608948,
40.0090551158078));
#171817=CARTESIAN_POINT('Ctrl Pts',(-0.267060783344285,62.8695915013899,
40.0255394551485));
#171818=CARTESIAN_POINT('Ctrl Pts',(-0.258597341631192,62.8775394315825,
40.0382021526118));
#171819=CARTESIAN_POINT('Ctrl Pts',(-0.249078184944433,62.8851801717861,
40.0503687782108));
#171820=CARTESIAN_POINT('Ctrl Pts',(-0.238478017627214,62.8924356323738,
40.0619155352442));
#171821=CARTESIAN_POINT('Ctrl Pts',(-0.238450236479103,62.892454647642,
40.0619457972351));
#171822=CARTESIAN_POINT('Ctrl Pts',(-0.238422447082677,62.8924736601095,
40.0619760547305));
#171823=CARTESIAN_POINT('Ctrl Pts',(-0.238394649440512,62.8924926697742,
40.0620063077269));
#171824=CARTESIAN_POINT('Ctrl Pts',(-0.235414176911847,62.8945308924032,
40.06525004417));
#171825=CARTESIAN_POINT('Ctrl Pts',(-0.232339728998654,62.8965351787718,
40.0684393223557));
#171826=CARTESIAN_POINT('Ctrl Pts',(-0.229175397308462,62.8985027695519,
40.0715697951759));
#171827=CARTESIAN_POINT('Ctrl Pts',(-0.211566610930674,62.9094519648693,
40.0889901646409));
#171828=CARTESIAN_POINT('Ctrl Pts',(-0.191177078586578,62.9192690206945,
40.1045963098222));
#171829=CARTESIAN_POINT('Ctrl Pts',(-0.168765047545422,62.9274935913879,
40.1176634650699));
#171830=CARTESIAN_POINT('Ctrl Pts',(-0.158706217642669,62.9311848926124,
40.1235281853046));
#171831=CARTESIAN_POINT('Ctrl Pts',(-0.148239886922486,62.9345557609571,
40.1288820140913));
#171832=CARTESIAN_POINT('Ctrl Pts',(-0.137433186921703,62.9375663198809,
40.1336621774101));
#171833=CARTESIAN_POINT('Ctrl Pts',(-0.132736741272955,62.9388746680683,
40.1357395717319));
#171834=CARTESIAN_POINT('Ctrl Pts',(-0.127976140237443,62.9401148076313,
40.1377083672884));
#171835=CARTESIAN_POINT('Ctrl Pts',(-0.123156980416903,62.9412833674838,
40.1395632548792));
#171836=CARTESIAN_POINT('Ctrl Pts',(-0.106289921045012,62.9453733269673,
40.146055361447));
#171837=CARTESIAN_POINT('Ctrl Pts',(-0.0887055165503932,62.9485864317703,
40.1511520974629));
#171838=CARTESIAN_POINT('Ctrl Pts',(-0.0706437212495017,62.9507781643242,
40.1546258197408));
#171839=CARTESIAN_POINT('Ctrl Pts',(-0.0616128235990559,62.9518740306011,
40.1563626808798));
#171840=CARTESIAN_POINT('Ctrl Pts',(-0.0524625782494773,62.9527145544237,
40.1576937882008));
#171841=CARTESIAN_POINT('Ctrl Pts',(-0.0432229794968555,62.9532816790167,
40.1585906813668));
#171842=CARTESIAN_POINT('Ctrl Pts',(-0.0386031801205446,62.9535652413132,
40.1590391279498));
#171843=CARTESIAN_POINT('Ctrl Pts',(-0.0339610423934489,62.9537804539255,
40.1593790209175));
#171844=CARTESIAN_POINT('Ctrl Pts',(-0.0293003156009363,62.9539250604562,
40.1596068022931));
#171845=CARTESIAN_POINT('Ctrl Pts',(-0.0246395888084235,62.9540696669868,
40.1598345836687));
#171846=CARTESIAN_POINT('Ctrl Pts',(-0.0199602729501285,62.9541436657296,
40.1599502506865));
#171847=CARTESIAN_POINT('Ctrl Pts',(-0.0152661173102018,62.9541448057648,
40.1599502534424));
#171848=CARTESIAN_POINT('',(0.318045750793707,62.7644678366119,39.8576902534424));
#171849=CARTESIAN_POINT('Ctrl Pts',(0.0152661173115319,62.9541448057648,
40.1599502534424));
#171850=CARTESIAN_POINT('Ctrl Pts',(0.0190877352453135,62.9541438736292,
40.1599502447858));
#171851=CARTESIAN_POINT('Ctrl Pts',(0.0228988721028898,62.9540952129414,
40.1598744685927));
#171852=CARTESIAN_POINT('Ctrl Pts',(0.0266975986410124,62.9539999459718,
40.1597246934279));
#171853=CARTESIAN_POINT('Ctrl Pts',(0.0486495517936765,62.953449420412,
40.1588591777434));
#171854=CARTESIAN_POINT('Ctrl Pts',(0.0701898812476337,62.9513443281453,
40.1555254706015));
#171855=CARTESIAN_POINT('Ctrl Pts',(0.0909392844453373,62.9479003565106,
40.1500631826367));
#171856=CARTESIAN_POINT('Ctrl Pts',(0.0993079960704183,62.9465113235258,
40.1478601162471));
#171857=CARTESIAN_POINT('Ctrl Pts',(0.107548428340109,62.9449047668209,
40.1453112228301));
#171858=CARTESIAN_POINT('Ctrl Pts',(0.115637319282903,62.9430957254317,
40.1424401896328));
#171859=CARTESIAN_POINT('Ctrl Pts',(0.118621628944159,62.9424282989905,
40.1413809526905));
#171860=CARTESIAN_POINT('Ctrl Pts',(0.121585194086244,62.9417332466658,
40.1402777640511));
#171861=CARTESIAN_POINT('Ctrl Pts',(0.124526788073465,62.941011293136,40.1391317641987));
#171862=CARTESIAN_POINT('Ctrl Pts',(0.130042276799505,62.9396576302675,
40.1369830144753));
#171863=CARTESIAN_POINT('Ctrl Pts',(0.135480523184277,62.938209392844,40.134683756585));
#171864=CARTESIAN_POINT('Ctrl Pts',(0.140833441494043,62.9366713579026,
40.1322415082996));
#171865=CARTESIAN_POINT('Ctrl Pts',(0.159568655578222,62.9312882356078,
40.1236936393009));
#171866=CARTESIAN_POINT('Ctrl Pts',(0.177258600739639,62.9248050892389,
40.113394140767));
#171867=CARTESIAN_POINT('Ctrl Pts',(0.193556601114317,62.9174267595942,
40.101665321223));
#171868=CARTESIAN_POINT('Ctrl Pts',(0.201705601301656,62.9137375947719,
40.095800911451));
#171869=CARTESIAN_POINT('Ctrl Pts',(0.20950661529207,62.9098246351409,40.0895791707949));
#171870=CARTESIAN_POINT('Ctrl Pts',(0.21691630865106,62.9057134946881,40.0830403822907));
#171871=CARTESIAN_POINT('Ctrl Pts',(0.220621155330555,62.9036579244618,
40.0797709880385));
#171872=CARTESIAN_POINT('Ctrl Pts',(0.224228171853212,62.9015528091475,
40.0764223317514));
#171873=CARTESIAN_POINT('Ctrl Pts',(0.227731941420199,62.8994013510256,
40.0729994484778));
#171874=CARTESIAN_POINT('Ctrl Pts',(0.231235710987187,62.8972498929038,
40.0695765652043));
#171875=CARTESIAN_POINT('Ctrl Pts',(0.234636114277394,62.8950520414621,
40.0660793733488));
#171876=CARTESIAN_POINT('Ctrl Pts',(0.237927978231581,62.8928111037451,
40.0625130768817));
#171877=CARTESIAN_POINT('Ctrl Pts',(0.237956050936881,62.8927919932396,
40.0624826638418));
#171878=CARTESIAN_POINT('Ctrl Pts',(0.237984115711677,62.8927728797351,
40.0624522459912));
#171879=CARTESIAN_POINT('Ctrl Pts',(0.238012172553515,62.8927537632335,
40.0624218233329));
#171880=CARTESIAN_POINT('Ctrl Pts',(0.252341211296938,62.8829906867849,
40.046884527592));
#171881=CARTESIAN_POINT('Ctrl Pts',(0.264702219190169,62.8725309380421,
40.0302263329284));
#171882=CARTESIAN_POINT('Ctrl Pts',(0.275152816746093,62.8615664772846,
40.0127515884816));
#171883=CARTESIAN_POINT('Ctrl Pts',(0.285956846571966,62.8502312057449,
39.9946858597813));
#171884=CARTESIAN_POINT('Ctrl Pts',(0.294719332057067,62.8383556508911,
39.9757460620614));
#171885=CARTESIAN_POINT('Ctrl Pts',(0.301453885680055,62.8261370346467,
39.956244455928));
#171886=CARTESIAN_POINT('Ctrl Pts',(0.308060333922269,62.8141508421938,
39.9371138113786));
#171887=CARTESIAN_POINT('Ctrl Pts',(0.312715155745665,62.8018335935204,
39.9174410654551));
#171888=CARTESIAN_POINT('Ctrl Pts',(0.315383336841203,62.7893708783685,
39.8975196504365));
#171889=CARTESIAN_POINT('Ctrl Pts',(0.317150913275835,62.7811147664985,
39.8843224113922));
#171890=CARTESIAN_POINT('Ctrl Pts',(0.318045664009114,62.7727948225171,
39.8710160447206));
#171891=CARTESIAN_POINT('Ctrl Pts',(0.318045750793707,62.7644678366119,
39.8576902534424));
#171892=CARTESIAN_POINT('',(0.318048871877787,62.4081695979768,39.2875012672119));
#171893=CARTESIAN_POINT('',(0.318045750793708,62.7644678366119,39.8576902534424));
#171894=CARTESIAN_POINT('',(6.20712349654526,62.0995362748658,39.2875012672119));
#171895=CARTESIAN_POINT('Origin',(5.53234440788222E-15,0.,39.2875012672119));
#171896=CARTESIAN_POINT('',(6.24436990788123,62.4538823482275,39.8576902534424));
#171897=CARTESIAN_POINT('',(6.20712349654526,62.0995362748658,39.2875012672119));
#171898=CARTESIAN_POINT('',(6.56531752495365,62.6108711573005,40.1599502534424));
#171899=CARTESIAN_POINT('Ctrl Pts',(6.24436990788122,62.4538823482275,39.8576902534424));
#171900=CARTESIAN_POINT('Ctrl Pts',(6.24565635961526,62.4661208561117,39.8773836120374));
#171901=CARTESIAN_POINT('Ctrl Pts',(6.24887816048211,62.4781153572978,39.8969946442152));
#171902=CARTESIAN_POINT('Ctrl Pts',(6.25393874389594,62.4897034690595,39.9162525288271));
#171903=CARTESIAN_POINT('Ctrl Pts',(6.2591010141573,62.5015244311583,39.9358973794102));
#171904=CARTESIAN_POINT('Ctrl Pts',(6.26617675898668,62.5129234357018,39.9551762199787));
#171905=CARTESIAN_POINT('Ctrl Pts',(6.27511683300959,62.5237314369814,39.9738152034297));
#171906=CARTESIAN_POINT('Ctrl Pts',(6.28370959326105,62.534119557209,39.9917300792702));
#171907=CARTESIAN_POINT('Ctrl Pts',(6.29402509234407,62.543962460673,40.0090551158183));
#171908=CARTESIAN_POINT('Ctrl Pts',(6.30606398948359,62.5531007542797,40.0255394551599));
#171909=CARTESIAN_POINT('Ctrl Pts',(6.31531185250446,62.5601204743206,40.038202152619));
#171910=CARTESIAN_POINT('Ctrl Pts',(6.32557753708383,62.5667243349276,40.0503687782142));
#171911=CARTESIAN_POINT('Ctrl Pts',(6.33687803771753,62.5728320301412,40.0619155352442));
#171912=CARTESIAN_POINT('Ctrl Pts',(6.33690765431437,62.5728480373211,40.0619457972351));
#171913=CARTESIAN_POINT('Ctrl Pts',(6.33693727882158,62.5728640408534,40.0619760547304));
#171914=CARTESIAN_POINT('Ctrl Pts',(6.33696691123639,62.5728800407363,40.0620063077269));
#171915=CARTESIAN_POINT('Ctrl Pts',(6.34014410870389,62.5745955535552,40.06525004417));
#171916=CARTESIAN_POINT('Ctrl Pts',(6.34341121944381,62.5762674929177,40.0684393223556));
#171917=CARTESIAN_POINT('Ctrl Pts',(6.34676388583449,62.5778935423007,40.0715697951759));
#171918=CARTESIAN_POINT('Ctrl Pts',(6.36542071199982,62.5869421374011,40.088990164642));
#171919=CARTESIAN_POINT('Ctrl Pts',(6.38672471011312,62.5945741278851,40.1045963098242));
#171920=CARTESIAN_POINT('Ctrl Pts',(6.40987366744057,62.6004109483563,40.1176634650724));
#171921=CARTESIAN_POINT('Ctrl Pts',(6.4202632400637,62.603030594214,40.1235281853061));
#171922=CARTESIAN_POINT('Ctrl Pts',(6.43102458681551,62.6052889671226,40.1288820140919));
#171923=CARTESIAN_POINT('Ctrl Pts',(6.44208677567923,62.6071534261452,40.1336621774101));
#171924=CARTESIAN_POINT('Ctrl Pts',(6.44689425333276,62.6079636948179,40.1357395717319));
#171925=CARTESIAN_POINT('Ctrl Pts',(6.45175840518046,62.6086994224562,40.1377083672883));
#171926=CARTESIAN_POINT('Ctrl Pts',(6.45667331290488,62.6093578414452,40.1395632548791));
#171927=CARTESIAN_POINT('Ctrl Pts',(6.47387548994035,62.6116623079067,40.1460553614469));
#171928=CARTESIAN_POINT('Ctrl Pts',(6.49169942613465,62.6130197402062,40.1511520974629));
#171929=CARTESIAN_POINT('Ctrl Pts',(6.5098913754668,62.6133114945131,40.1546258197408));
#171930=CARTESIAN_POINT('Ctrl Pts',(6.51898735013287,62.6134573716666,40.1563626808798));
#171931=CARTESIAN_POINT('Ctrl Pts',(6.52817532814455,62.6133368299269,40.1576937882008));
#171932=CARTESIAN_POINT('Ctrl Pts',(6.53742359207063,62.6129350466932,40.1585906813668));
#171933=CARTESIAN_POINT('Ctrl Pts',(6.54204772403368,62.6127341550763,40.1590391279498));
#171934=CARTESIAN_POINT('Ctrl Pts',(6.54668692748823,62.6124629532085,40.1593790209175));
#171935=CARTESIAN_POINT('Ctrl Pts',(6.55133723783015,62.6121195889601,40.1596068022931));
#171936=CARTESIAN_POINT('Ctrl Pts',(6.55598754817206,62.6117762247117,40.1598345836687));
#171937=CARTESIAN_POINT('Ctrl Pts',(6.56064896522335,62.6113606963859,40.1599502506865));
#171938=CARTESIAN_POINT('Ctrl Pts',(6.56531752495365,62.6108711573005,40.1599502534424));
#171939=CARTESIAN_POINT('',(6.59568250079948,62.6076796697353,40.1599502534424));
#171940=CARTESIAN_POINT('Origin',(5.63895492999586E-15,5.54032330042594E-15,
40.1599502534424));
#171941=CARTESIAN_POINT('',(6.87697683366627,62.387392681069,39.8576902534424));
#171942=CARTESIAN_POINT('Ctrl Pts',(6.59568250079949,62.6076796697354,40.1599502534424));
#171943=CARTESIAN_POINT('Ctrl Pts',(6.59948308607566,62.6072792748562,40.1599502447858));
#171944=CARTESIAN_POINT('Ctrl Pts',(6.60326825869985,62.6068325084577,40.1598744685927));
#171945=CARTESIAN_POINT('Ctrl Pts',(6.60703621730659,62.6063406883232,40.1597246934279));
#171946=CARTESIAN_POINT('Ctrl Pts',(6.62881036977204,62.6034985746713,40.1588591777434));
#171947=CARTESIAN_POINT('Ctrl Pts',(6.65001265698756,62.5991534367842,40.1555254706016));
#171948=CARTESIAN_POINT('Ctrl Pts',(6.67028839972079,62.5935594283565,40.1500631826369));
#171949=CARTESIAN_POINT('Ctrl Pts',(6.67846607318486,62.5913032360741,40.1478601162472));
#171950=CARTESIAN_POINT('Ctrl Pts',(6.68649343260107,62.588844120533,40.1453112228302));
#171951=CARTESIAN_POINT('Ctrl Pts',(6.69434891543673,62.586199469922,40.1424401896328));
#171952=CARTESIAN_POINT('Ctrl Pts',(6.69724711167717,62.5852237544098,40.1413809526905));
#171953=CARTESIAN_POINT('Ctrl Pts',(6.70012178934792,62.5842227327444,40.1402777640511));
#171954=CARTESIAN_POINT('Ctrl Pts',(6.70297180428247,62.5831972538525,40.1391317641987));
#171955=CARTESIAN_POINT('Ctrl Pts',(6.70831558228476,62.5812744809302,40.1369830144753));
#171956=CARTESIAN_POINT('Ctrl Pts',(6.71357265535449,62.5792657255653,40.1346837565849));
#171957=CARTESIAN_POINT('Ctrl Pts',(6.7187354813888,62.5771765838154,40.1322415082996));
#171958=CARTESIAN_POINT('Ctrl Pts',(6.73680537250886,62.5698645876905,40.1236936393009));
#171959=CARTESIAN_POINT('Ctrl Pts',(6.75372073697266,62.5615678538927,40.113394140767));
#171960=CARTESIAN_POINT('Ctrl Pts',(6.76915820973676,62.5525263385763,40.101665321223));
#171961=CARTESIAN_POINT('Ctrl Pts',(6.7768769461188,62.5480055809181,40.095800911451));
#171962=CARTESIAN_POINT('Ctrl Pts',(6.78422620968128,62.5432986288851,40.0895791707949));
#171963=CARTESIAN_POINT('Ctrl Pts',(6.79116558077096,62.5384354858298,40.0830403822906));
#171964=CARTESIAN_POINT('Ctrl Pts',(6.7946352663158,62.5360039143022,40.0797709880385));
#171965=CARTESIAN_POINT('Ctrl Pts',(6.79800247875573,62.5335332951357,40.0764223317514));
#171966=CARTESIAN_POINT('Ctrl Pts',(6.80126216569517,62.5310273792781,40.0729994484778));
#171967=CARTESIAN_POINT('Ctrl Pts',(6.8045218526346,62.5285214634205,40.0695765652042));
#171968=CARTESIAN_POINT('Ctrl Pts',(6.80767389012611,62.5259802131085,40.0660793733488));
#171969=CARTESIAN_POINT('Ctrl Pts',(6.81071347912929,62.5234074580024,40.0625130768817));
#171970=CARTESIAN_POINT('Ctrl Pts',(6.8107394004576,62.5233855177895,40.0624826638418));
#171971=CARTESIAN_POINT('Ctrl Pts',(6.81076531358536,62.523363575423,40.0624522459912));
#171972=CARTESIAN_POINT('Ctrl Pts',(6.81079121851035,62.5233416309051,40.0624218233329));
#171973=CARTESIAN_POINT('Ctrl Pts',(6.82402124190388,62.5121342452095,40.0468845275902));
#171974=CARTESIAN_POINT('Ctrl Pts',(6.83522119344137,62.5004397189038,40.0302263329244));
#171975=CARTESIAN_POINT('Ctrl Pts',(6.84446844329752,62.4884429377053,40.0127515884755));
#171976=CARTESIAN_POINT('Ctrl Pts',(6.85402842900344,62.4760404333329,39.9946858597728));
#171977=CARTESIAN_POINT('Ctrl Pts',(6.86150157917705,62.4633140048674,39.9757460620505));
#171978=CARTESIAN_POINT('Ctrl Pts',(6.86692204703104,62.4504583709387,39.9562444559146));
#171979=CARTESIAN_POINT('Ctrl Pts',(6.87223940618061,62.4378472782183,39.9371138113629));
#171980=CARTESIAN_POINT('Ctrl Pts',(6.87558122532671,62.4251109433487,39.9174410654371));
#171981=CARTESIAN_POINT('Ctrl Pts',(6.87693208138284,62.4124375993835,39.8975196504164));
#171982=CARTESIAN_POINT('Ctrl Pts',(6.87782697616113,62.404041953314,39.8843224113787));
#171983=CARTESIAN_POINT('Ctrl Pts',(6.87784715439695,62.3956740599414,39.8710160447138));
#171984=CARTESIAN_POINT('Ctrl Pts',(6.87697683366627,62.3873926810691,39.8576902534424));
#171985=CARTESIAN_POINT('',(6.83973663030322,62.0330459552232,39.2875012672119));
#171986=CARTESIAN_POINT('',(6.87697683366627,62.387392681069,39.8576902534424));
#171987=CARTESIAN_POINT('',(12.6642893210148,61.110527437164,39.2875012672119));
#171988=CARTESIAN_POINT('Origin',(5.53234440788222E-15,0.,39.2875012672119));
#171989=CARTESIAN_POINT('',(12.7383709431257,61.4590390555207,39.8576902534424));
#171990=CARTESIAN_POINT('',(12.6642893210148,61.110527437164,39.2875012672119));
#171991=CARTESIAN_POINT('',(13.0739701745332,61.5816197022696,40.1599502534424));
#171992=CARTESIAN_POINT('Ctrl Pts',(12.7383709431257,61.4590390555207,39.8576902534424));
#171993=CARTESIAN_POINT('Ctrl Pts',(12.7409296199642,61.4710760487551,39.8773836120368));
#171994=CARTESIAN_POINT('Ctrl Pts',(12.7453875382452,61.4826680729147,39.896994644214));
#171995=CARTESIAN_POINT('Ctrl Pts',(12.7516316867679,61.4936637287799,39.9162525288252));
#171996=CARTESIAN_POINT('Ctrl Pts',(12.7580013045749,61.5048803302339,39.9358973794079));
#171997=CARTESIAN_POINT('Ctrl Pts',(12.7662298081611,61.515477273104,39.9551762199759));
#171998=CARTESIAN_POINT('Ctrl Pts',(12.7762506512874,61.5252915748225,39.9738152034265));
#171999=CARTESIAN_POINT('Ctrl Pts',(12.7858821937424,61.5347245998162,39.9917300792667));
#172000=CARTESIAN_POINT('Ctrl Pts',(12.7971700470149,61.543435319558,40.0090551158146));
#172001=CARTESIAN_POINT('Ctrl Pts',(12.8100982056033,61.5512651452188,40.025539455156));
#172002=CARTESIAN_POINT('Ctrl Pts',(12.8200291684122,61.5572797455894,40.0382021526165));
#172003=CARTESIAN_POINT('Ctrl Pts',(12.8309289078993,61.5627743733242,40.050368778213));
#172004=CARTESIAN_POINT('Ctrl Pts',(12.8428059312041,61.5676673859794,40.0619155352442));
#172005=CARTESIAN_POINT('Ctrl Pts',(12.8428370587641,61.567680209693,40.0619457972351));
#172006=CARTESIAN_POINT('Ctrl Pts',(12.8428681938098,61.5676930289521,40.0619760547304));
#172007=CARTESIAN_POINT('Ctrl Pts',(12.8428993363383,61.5677058437551,40.0620063077269));
#172008=CARTESIAN_POINT('Ctrl Pts',(12.8462384487043,61.5690798512466,40.06525004417));
#172009=CARTESIAN_POINT('Ctrl Pts',(12.849662427122,61.5704011254853,40.0684393223556));
#172010=CARTESIAN_POINT('Ctrl Pts',(12.8531666956986,61.571667818134,40.0715697951759));
#172011=CARTESIAN_POINT('Ctrl Pts',(12.8726671535569,61.5787166747145,40.0889901646404));
#172012=CARTESIAN_POINT('Ctrl Pts',(12.8946522063743,61.5840799821715,40.1045963098214));
#172013=CARTESIAN_POINT('Ctrl Pts',(12.9182844651632,61.5874651029938,40.1176634650689));
#172014=CARTESIAN_POINT('Ctrl Pts',(12.9288909501782,61.5889843920976,40.123528185304));
#172015=CARTESIAN_POINT('Ctrl Pts',(12.9398294093983,61.5901055263648,40.128882014091));
#172016=CARTESIAN_POINT('Ctrl Pts',(12.9510258874727,61.5908034580836,40.1336621774101));
#172017=CARTESIAN_POINT('Ctrl Pts',(12.9558917253998,61.5911067697684,40.1357395717319));
#172018=CARTESIAN_POINT('Ctrl Pts',(12.9608061353941,61.591330024696,40.1377083672884));
#172019=CARTESIAN_POINT('Ctrl Pts',(12.9657629422649,61.5914710890453,40.1395632548792));
#172020=CARTESIAN_POINT('Ctrl Pts',(12.9831117663125,61.5919648142681,40.146055361447));
#172021=CARTESIAN_POINT('Ctrl Pts',(13.0009799514316,61.5914517017516,40.1511520974629));
#172022=CARTESIAN_POINT('Ctrl Pts',(13.0191027399912,61.5898402812904,40.1546258197408));
#172023=CARTESIAN_POINT('Ctrl Pts',(13.028164134271,61.5890345710598,40.1563626808798));
#172024=CARTESIAN_POINT('Ctrl Pts',(13.037289179535,61.5879542844382,40.1576937882008));
#172025=CARTESIAN_POINT('Ctrl Pts',(13.0464447827196,61.586587995399,40.1585906813668));
#172026=CARTESIAN_POINT('Ctrl Pts',(13.051022584312,61.5859048508794,40.1590391279498));
#172027=CARTESIAN_POINT('Ctrl Pts',(13.0556080254101,61.5851502058759,40.1593790209175));
#172028=CARTESIAN_POINT('Ctrl Pts',(13.0601969695282,61.5843226328191,40.1596068022931));
#172029=CARTESIAN_POINT('Ctrl Pts',(13.0647859136462,61.5834950597622,40.1598345836687));
#172030=CARTESIAN_POINT('Ctrl Pts',(13.0693783604298,61.582594556983,40.1599502506865));
#172031=CARTESIAN_POINT('Ctrl Pts',(13.0739701745332,61.5816197022696,40.1599502534424));
#172032=CARTESIAN_POINT('',(13.1038352065734,61.575271693745,40.1599502534424));
#172033=CARTESIAN_POINT('Origin',(5.62288786856779E-15,5.54286807295788E-15,
40.1599502534424));
#172034=CARTESIAN_POINT('',(13.3605623192493,61.3267881959111,39.8576902534424));
#172035=CARTESIAN_POINT('Ctrl Pts',(13.1038352065734,61.575271693745,40.1599502534424));
#172036=CARTESIAN_POINT('Ctrl Pts',(13.1075731191844,61.5744762229325,40.1599502447858));
#172037=CARTESIAN_POINT('Ctrl Pts',(13.1112908564318,61.5736362456894,40.1598744685927));
#172038=CARTESIAN_POINT('Ctrl Pts',(13.1149867645642,61.5727532608742,40.1597246934279));
#172039=CARTESIAN_POINT('Ctrl Pts',(13.1363445541734,61.5676506979217,40.1588591777433));
#172040=CARTESIAN_POINT('Ctrl Pts',(13.1569765024567,61.5611131206536,40.1555254706011));
#172041=CARTESIAN_POINT('Ctrl Pts',(13.1765564394468,61.5534303645591,40.1500631826356));
#172042=CARTESIAN_POINT('Ctrl Pts',(13.1844534784461,61.5503317322942,40.1478601162462));
#172043=CARTESIAN_POINT('Ctrl Pts',(13.1921798155775,61.5470470005022,40.1453112228296));
#172044=CARTESIAN_POINT('Ctrl Pts',(13.1997158239904,61.5435957160156,40.1424401896328));
#172045=CARTESIAN_POINT('Ctrl Pts',(13.2024961535655,61.5423224015758,40.1413809526906));
#172046=CARTESIAN_POINT('Ctrl Pts',(13.2052504481948,61.5410263779725,40.1402777640512));
#172047=CARTESIAN_POINT('Ctrl Pts',(13.2079776587167,61.5397086090799,40.1391317641987));
#172048=CARTESIAN_POINT('Ctrl Pts',(13.2130911784452,61.5372377924062,40.1369830144753));
#172049=CARTESIAN_POINT('Ctrl Pts',(13.2181094806072,61.5346905274441,40.134683756585));
#172050=CARTESIAN_POINT('Ctrl Pts',(13.2230256493636,61.5320731679598,40.1322415082996));
#172051=CARTESIAN_POINT('Ctrl Pts',(13.2402322400111,61.5229124097646,40.1236936393009));
#172052=CARTESIAN_POINT('Ctrl Pts',(13.2561876955045,61.5128929892896,40.113394140767));
#172053=CARTESIAN_POINT('Ctrl Pts',(13.2705955044759,61.5022873490354,40.101665321223));
#172054=CARTESIAN_POINT('Ctrl Pts',(13.2777994089616,61.4969845289083,40.095800911451));
#172055=CARTESIAN_POINT('Ctrl Pts',(13.2846164020267,61.4915351548246,40.0895791707949));
#172056=CARTESIAN_POINT('Ctrl Pts',(13.2910094216452,61.4859732907798,40.0830403822906));
#172057=CARTESIAN_POINT('Ctrl Pts',(13.2942059314545,61.4831923587574,40.0797709880385));
#172058=CARTESIAN_POINT('Ctrl Pts',(13.2972964479276,61.4803833043593,40.0764223317514));
#172059=CARTESIAN_POINT('Ctrl Pts',(13.3002763384272,61.4775503861045,40.0729994484778));
#172060=CARTESIAN_POINT('Ctrl Pts',(13.3032562289269,61.4747174678497,40.0695765652042));
#172061=CARTESIAN_POINT('Ctrl Pts',(13.3061253662373,61.4718606611376,40.0660793733488));
#172062=CARTESIAN_POINT('Ctrl Pts',(13.3088793779163,61.4689842762857,40.0625130768816));
#172063=CARTESIAN_POINT('Ctrl Pts',(13.3089028638681,61.468959746747,40.0624826638418));
#172064=CARTESIAN_POINT('Ctrl Pts',(13.3089263414392,61.4689352159237,40.0624522459912));
#172065=CARTESIAN_POINT('Ctrl Pts',(13.3089498106276,61.4689106838181,40.0624218233329));
#172066=CARTESIAN_POINT('Ctrl Pts',(13.320935867764,61.4563817793403,40.046884527591));
#172067=CARTESIAN_POINT('Ctrl Pts',(13.3308520539314,61.443580603151,40.0302263329261));
#172068=CARTESIAN_POINT('Ctrl Pts',(13.3387946412822,61.430682940759,40.0127515884781));
#172069=CARTESIAN_POINT('Ctrl Pts',(13.3470058416633,61.4173490879891,39.9946858597764));
#172070=CARTESIAN_POINT('Ctrl Pts',(13.3531077791279,61.4039112193276,39.9757460620551));
#172071=CARTESIAN_POINT('Ctrl Pts',(13.3571547734332,61.3905594167323,39.9562444559201));
#172072=CARTESIAN_POINT('Ctrl Pts',(13.361124785391,61.3774615935173,39.9371138113694));
#172073=CARTESIAN_POINT('Ctrl Pts',(13.3631169881909,61.3644457144034,39.9174410654445));
#172074=CARTESIAN_POINT('Ctrl Pts',(13.3631357189476,61.3517005934352,39.8975196504246));
#172075=CARTESIAN_POINT('Ctrl Pts',(13.3631481274173,61.3432573976156,39.8843224113842));
#172076=CARTESIAN_POINT('Ctrl Pts',(13.3622935120796,61.3349332352367,39.8710160447165));
#172077=CARTESIAN_POINT('Ctrl Pts',(13.3605623192493,61.3267881959111,39.8576902534424));
#172078=CARTESIAN_POINT('',(13.2864868029002,60.9782752797346,39.2875012672119));
#172079=CARTESIAN_POINT('',(13.3605623192493,61.3267881959111,39.8576902534424));
#172080=CARTESIAN_POINT('',(18.9827025415103,59.4519788726605,39.2875012672119));
#172081=CARTESIAN_POINT('Origin',(5.53234440788222E-15,0.,39.2875012672119));
#172082=CARTESIAN_POINT('',(19.0928077206418,59.7908376697909,39.8576902534424));
#172083=CARTESIAN_POINT('',(18.9827025415103,59.4519788726606,39.2875012672119));
#172084=CARTESIAN_POINT('',(19.4393816709763,59.8776671349983,40.1599502534424));
#172085=CARTESIAN_POINT('Ctrl Pts',(19.0928077206418,59.7908376697909,39.8576902534424));
#172086=CARTESIAN_POINT('Ctrl Pts',(19.0966105891856,59.8025412685583,39.8773836120355));
#172087=CARTESIAN_POINT('Ctrl Pts',(19.1022557829948,59.8136038110487,39.8969946442114));
#172088=CARTESIAN_POINT('Ctrl Pts',(19.1096150844281,59.8238865403105,39.9162525288214));
#172089=CARTESIAN_POINT('Ctrl Pts',(19.1171222629146,59.8343758896866,39.9358973794029));
#172090=CARTESIAN_POINT('Ctrl Pts',(19.1264133720499,59.8440546685596,39.9551762199699));
#172091=CARTESIAN_POINT('Ctrl Pts',(19.1374051938247,59.8527677431735,39.9738152034195));
#172092=CARTESIAN_POINT('Ctrl Pts',(19.147969993288,59.8611423227373,39.991730079259));
#172093=CARTESIAN_POINT('Ctrl Pts',(19.1601065286666,59.8686254222887,40.0090551158061));
#172094=CARTESIAN_POINT('Ctrl Pts',(19.1737823050924,59.8750609947952,40.0255394551469));
#172095=CARTESIAN_POINT('Ctrl Pts',(19.1842875619839,59.8800045782759,40.0382021526108));
#172096=CARTESIAN_POINT('Ctrl Pts',(19.1957019365535,59.8843297728477,40.0503687782103));
#172097=CARTESIAN_POINT('Ctrl Pts',(19.2080253553785,59.8879544940742,40.0619155352442));
#172098=CARTESIAN_POINT('Ctrl Pts',(19.2080576528615,59.8879639938221,40.0619457972351));
#172099=CARTESIAN_POINT('Ctrl Pts',(19.2080899573236,59.8879734883575,40.0619760547305));
#172100=CARTESIAN_POINT('Ctrl Pts',(19.2081222687617,59.8879829776791,40.0620063077269));
#172101=CARTESIAN_POINT('Ctrl Pts',(19.2115867120124,59.8890004259294,40.06525004417));
#172102=CARTESIAN_POINT('Ctrl Pts',(19.2151300442838,59.8899565588873,40.0684393223556));
#172103=CARTESIAN_POINT('Ctrl Pts',(19.2187475215465,59.890850016652,40.0715697951759));
#172104=CARTESIAN_POINT('Ctrl Pts',(19.2388779600064,59.8958219059666,40.0889901646438));
#172105=CARTESIAN_POINT('Ctrl Pts',(19.2613031946953,59.8988577688785,40.1045963098274));
#172106=CARTESIAN_POINT('Ctrl Pts',(19.2851598349806,59.8997541019594,40.1176634650765));
#172107=CARTESIAN_POINT('Ctrl Pts',(19.2958670255119,59.9001563886587,40.1235281853086));
#172108=CARTESIAN_POINT('Ctrl Pts',(19.3068627531452,59.9001280009021,40.1288820140931));
#172109=CARTESIAN_POINT('Ctrl Pts',(19.3180708494664,59.899651758631,40.1336621774101));
#172110=CARTESIAN_POINT('Ctrl Pts',(19.3229417365285,59.8994447901816,40.1357395717319));
#172111=CARTESIAN_POINT('Ctrl Pts',(19.3278525613652,59.8991531263707,40.1377083672884));
#172112=CARTESIAN_POINT('Ctrl Pts',(19.332796959569,59.8987752905499,40.1395632548792));
#172113=CARTESIAN_POINT('Ctrl Pts',(19.3501023532821,59.8974528651771,40.146055361447));
#172114=CARTESIAN_POINT('Ctrl Pts',(19.3678190197507,59.8950748296128,40.1511520974629));
#172115=CARTESIAN_POINT('Ctrl Pts',(19.3856740904739,59.8915778894432,40.1546258197408));
#172116=CARTESIAN_POINT('Ctrl Pts',(19.3946016258354,59.8898294193584,40.1563626808798));
#172117=CARTESIAN_POINT('Ctrl Pts',(19.4035637624462,59.8878012237013,40.1576937882008));
#172118=CARTESIAN_POINT('Ctrl Pts',(19.412526394185,59.8854853982052,40.1585906813668));
#172119=CARTESIAN_POINT('Ctrl Pts',(19.4170077100544,59.8843274854572,40.1590391279498));
#172120=CARTESIAN_POINT('Ctrl Pts',(19.4214891497439,59.8830976653666,40.1593790209175));
#172121=CARTESIAN_POINT('Ctrl Pts',(19.4259664502061,59.8817949505648,40.1596068022931));
#172122=CARTESIAN_POINT('Ctrl Pts',(19.4304437506682,59.8804922357631,40.1598345836687));
#172123=CARTESIAN_POINT('Ctrl Pts',(19.4349169113761,59.8791166246274,40.1599502506865));
#172124=CARTESIAN_POINT('Ctrl Pts',(19.4393816709763,59.8776671349983,40.1599502534424));
#172125=CARTESIAN_POINT('',(19.4684195516703,59.868232155624,40.1599502534424));
#172126=CARTESIAN_POINT('Origin',(5.60717482534548E-15,5.54707837019994E-15,
40.1599502534424));
#172127=CARTESIAN_POINT('',(19.6977666881852,59.5942745858234,39.8576902534424));
#172128=CARTESIAN_POINT('Ctrl Pts',(19.4684195516703,59.868232155624,40.1599502534424));
#172129=CARTESIAN_POINT('Ctrl Pts',(19.4720538382633,59.8670503242228,40.1599502447858));
#172130=CARTESIAN_POINT('Ctrl Pts',(19.4756634078267,59.8658263391016,40.1598744685927));
#172131=CARTESIAN_POINT('Ctrl Pts',(19.4792467723418,59.8645618637721,40.1597246934279));
#172132=CARTESIAN_POINT('Ctrl Pts',(19.4999541986819,59.8572547562663,40.1588591777433));
#172133=CARTESIAN_POINT('Ctrl Pts',(19.5197897600895,59.8485963666816,40.1555254706007));
#172134=CARTESIAN_POINT('Ctrl Pts',(19.5384593694488,59.8389090368037,40.1500631826346));
#172135=CARTESIAN_POINT('Ctrl Pts',(19.5459892523722,59.8350019138202,40.1478601162455));
#172136=CARTESIAN_POINT('Ctrl Pts',(19.5533299158528,59.8309275539862,40.1453112228292));
#172137=CARTESIAN_POINT('Ctrl Pts',(19.5604638837584,59.8267074486191,40.1424401896328));
#172138=CARTESIAN_POINT('Ctrl Pts',(19.5630958847956,59.8251504859512,40.1413809526905));
#172139=CARTESIAN_POINT('Ctrl Pts',(19.5656996197551,59.8235736599158,40.1402777640511));
#172140=CARTESIAN_POINT('Ctrl Pts',(19.5682741459751,59.8219780387742,40.1391317641987));
#172141=CARTESIAN_POINT('Ctrl Pts',(19.5731013826375,59.8189862491337,40.1369830144753));
#172142=CARTESIAN_POINT('Ctrl Pts',(19.5778259323232,59.8159283829423,40.1346837565849));
#172143=CARTESIAN_POINT('Ctrl Pts',(19.5824415812281,59.8128114820619,40.1322415082996));
#172144=CARTESIAN_POINT('Ctrl Pts',(19.5985963523951,59.8019023289801,40.1236936393009));
#172145=CARTESIAN_POINT('Ctrl Pts',(19.6134170876088,59.7902699966954,40.113394140767));
#172146=CARTESIAN_POINT('Ctrl Pts',(19.6266373778174,59.7782164291174,40.101665321223));
#172147=CARTESIAN_POINT('Ctrl Pts',(19.6332475229217,59.7721896453283,40.095800911451));
#172148=CARTESIAN_POINT('Ctrl Pts',(19.6394575570867,59.7660575536769,40.0895791707949));
#172149=CARTESIAN_POINT('Ctrl Pts',(19.6452341819734,59.7598579055889,40.0830403822906));
#172150=CARTESIAN_POINT('Ctrl Pts',(19.6481224944167,59.7567580815449,40.0797709880385));
#172151=CARTESIAN_POINT('Ctrl Pts',(19.6509024545777,59.7536413685031,40.0764223317514));
#172152=CARTESIAN_POINT('Ctrl Pts',(19.6535699003337,59.7505124858963,40.0729994484778));
#172153=CARTESIAN_POINT('Ctrl Pts',(19.6562373460896,59.7473836032894,40.0695765652042));
#172154=CARTESIAN_POINT('Ctrl Pts',(19.6587921483502,59.7442425399495,40.0660793733488));
#172155=CARTESIAN_POINT('Ctrl Pts',(19.6612304091767,59.7410940396261,40.0625130768816));
#172156=CARTESIAN_POINT('Ctrl Pts',(19.661251202435,59.7410671895123,40.0624826638418));
#172157=CARTESIAN_POINT('Ctrl Pts',(19.6612719872243,59.741040338997,40.0624522459912));
#172158=CARTESIAN_POINT('Ctrl Pts',(19.6612927635427,59.7410134880826,40.0624218233329));
#172159=CARTESIAN_POINT('Ctrl Pts',(19.6719035326713,59.7273003341229,40.0468845275927));
#172160=CARTESIAN_POINT('Ctrl Pts',(19.6804273096575,59.7135327604163,40.0302263329299));
#172161=CARTESIAN_POINT('Ctrl Pts',(19.6869782138539,59.6998755263197,40.0127515884841));
#172162=CARTESIAN_POINT('Ctrl Pts',(19.6937506652803,59.6857564136346,39.9946858597846));
#172163=CARTESIAN_POINT('Ctrl Pts',(19.6984145359325,59.671754332879,39.9757460620657));
#172164=CARTESIAN_POINT('Ctrl Pts',(19.7010437169729,59.6580526467613,39.9562444559333));
#172165=CARTESIAN_POINT('Ctrl Pts',(19.7036228854577,59.6446115955445,39.9371138113848));
#172166=CARTESIAN_POINT('Ctrl Pts',(19.7042436449215,59.6314587768822,39.9174410654622));
#172167=CARTESIAN_POINT('Ctrl Pts',(19.7029300451616,59.618781517124,39.8975196504446));
#172168=CARTESIAN_POINT('Ctrl Pts',(19.7020598313727,59.6103832769719,39.8843224113977));
#172169=CARTESIAN_POINT('Ctrl Pts',(19.7003397858053,59.6021940468491,39.8710160447233));
#172170=CARTESIAN_POINT('Ctrl Pts',(19.6977666881852,59.5942745858234,39.8576902534424));
#172171=CARTESIAN_POINT('',(19.5876674457085,59.2554138597569,39.2875012672119));
#172172=CARTESIAN_POINT('',(19.6977666881852,59.5942745858234,39.8576902534424));
#172173=CARTESIAN_POINT('',(25.0931373005752,57.1420619865018,39.2875012672119));
#172174=CARTESIAN_POINT('Origin',(5.53234440788222E-15,0.,39.2875012672119));
#172175=CARTESIAN_POINT('',(25.2380597013437,57.4675553545137,39.8576902534424));
#172176=CARTESIAN_POINT('',(25.0931373005752,57.1420619865019,39.2875012672119));
#172177=CARTESIAN_POINT('',(25.5918112338801,57.5176823163886,40.1599502534424));
#172178=CARTESIAN_POINT('Ctrl Pts',(25.2380597013437,57.4675553545137,39.8576902534424));
#172179=CARTESIAN_POINT('Ctrl Pts',(25.24306509657,57.4787973317381,39.8773836120366));
#172180=CARTESIAN_POINT('Ctrl Pts',(25.2498357159838,57.4892091890301,39.8969946442136));
#172181=CARTESIAN_POINT('Ctrl Pts',(25.2582295402824,57.498666331956,39.9162525288247));
#172182=CARTESIAN_POINT('Ctrl Pts',(25.2667920292312,57.5083135057483,39.9358973794071));
#172183=CARTESIAN_POINT('Ctrl Pts',(25.2770439485812,57.5169680778983,39.9551762199749));
#172184=CARTESIAN_POINT('Ctrl Pts',(25.2888863203068,57.5244844631393,39.9738152034253));
#172185=CARTESIAN_POINT('Ctrl Pts',(25.3002686266262,57.5317088436274,39.9917300792652));
#172186=CARTESIAN_POINT('Ctrl Pts',(25.3131208736915,57.5378823365839,40.0090551158128));
#172187=CARTESIAN_POINT('Ctrl Pts',(25.3273944332882,57.5428531464569,40.0255394551538));
#172188=CARTESIAN_POINT('Ctrl Pts',(25.3383588864659,57.54667155011,40.0382021526152));
#172189=CARTESIAN_POINT('Ctrl Pts',(25.3501628378371,57.5497799237798,40.0503687782124));
#172190=CARTESIAN_POINT('Ctrl Pts',(25.3627976342216,57.5520966403718,40.0619155352442));
#172191=CARTESIAN_POINT('Ctrl Pts',(25.3628307477697,57.5521027120728,40.0619457972351));
#172192=CARTESIAN_POINT('Ctrl Pts',(25.3628638677137,57.5521087778603,40.0619760547305));
#172193=CARTESIAN_POINT('Ctrl Pts',(25.3628969940507,57.5521148377334,40.0620063077269));
#172194=CARTESIAN_POINT('Ctrl Pts',(25.3664488110208,57.5527645793667,40.06525004417));
#172195=CARTESIAN_POINT('Ctrl Pts',(25.370072675656,57.553345095451,40.0684393223556));
#172196=CARTESIAN_POINT('Ctrl Pts',(25.3737637277669,57.5538555294214,40.0715697951759));
#172197=CARTESIAN_POINT('Ctrl Pts',(25.3943035935321,57.5566959784096,40.0889901646471));
#172198=CARTESIAN_POINT('Ctrl Pts',(25.4169233145287,57.5573711352261,40.1045963098334));
#172199=CARTESIAN_POINT('Ctrl Pts',(25.4407429579668,57.5557688601517,40.117663465084));
#172200=CARTESIAN_POINT('Ctrl Pts',(25.4514335437942,57.5550497369101,40.1235281853132));
#172201=CARTESIAN_POINT('Ctrl Pts',(25.462366068348,57.5538721381528,40.1288820140951));
#172202=CARTESIAN_POINT('Ctrl Pts',(25.4734629846673,57.5522269397028,40.1336621774101));
#172203=CARTESIAN_POINT('Ctrl Pts',(25.4782855544065,57.5515119587089,40.1357395717319));
#172204=CARTESIAN_POINT('Ctrl Pts',(25.483138990061,57.5507085716893,40.1377083672884));
#172205=CARTESIAN_POINT('Ctrl Pts',(25.4880168077363,57.5498159753467,40.1395632548792));
#172206=CARTESIAN_POINT('Ctrl Pts',(25.5050891695999,57.5466918881473,40.146055361447));
#172207=CARTESIAN_POINT('Ctrl Pts',(25.5224602099128,57.5424749837905,40.1511520974629));
#172208=CARTESIAN_POINT('Ctrl Pts',(25.5398519389082,57.5371308371208,40.1546258197408));
#172209=CARTESIAN_POINT('Ctrl Pts',(25.5485478034059,57.5344587637859,40.1563626808798));
#172210=CARTESIAN_POINT('Ctrl Pts',(25.5572488403194,57.5315048804294,40.1576937882008));
#172211=CARTESIAN_POINT('Ctrl Pts',(25.5659203041434,57.5282648911452,40.1585906813668));
#172212=CARTESIAN_POINT('Ctrl Pts',(25.5702560360555,57.5266448965031,40.1590391279498));
#172213=CARTESIAN_POINT('Ctrl Pts',(25.5745843747453,57.5249533754917,40.1593790209175));
#172214=CARTESIAN_POINT('Ctrl Pts',(25.5789009773107,57.523189791761,40.1596068022931));
#172215=CARTESIAN_POINT('Ctrl Pts',(25.5832175798762,57.5214262080303,40.1598345836687));
#172216=CARTESIAN_POINT('Ctrl Pts',(25.5875224456236,57.5195905600216,40.1599502506864));
#172217=CARTESIAN_POINT('Ctrl Pts',(25.5918112338801,57.5176823163886,40.1599502534424));
#172218=CARTESIAN_POINT('',(25.6197038181304,57.5052637377729,40.1599502534424));
#172219=CARTESIAN_POINT('Origin',(5.59198795571863E-15,5.55290806325446E-15,
40.1599502534424));
#172220=CARTESIAN_POINT('',(25.8191582032627,57.2088336324696,39.8576902534424));
#172221=CARTESIAN_POINT('Ctrl Pts',(25.6197038181304,57.5052637377729,40.1599502534424));
#172222=CARTESIAN_POINT('Ctrl Pts',(25.623194660701,57.5037084941751,40.1599502447858));
#172223=CARTESIAN_POINT('Ctrl Pts',(25.6266565153809,57.502113911413,40.1598744685927));
#172224=CARTESIAN_POINT('Ctrl Pts',(25.6300880761872,57.5004817994256,40.1597246934279));
#172225=CARTESIAN_POINT('Ctrl Pts',(25.6499182643587,57.4910502055666,40.1588591777434));
#172226=CARTESIAN_POINT('Ctrl Pts',(25.6687401163261,57.4803658667952,40.1555254706013));
#172227=CARTESIAN_POINT('Ctrl Pts',(25.6862948499051,57.4687800995491,40.1500631826362));
#172228=CARTESIAN_POINT('Ctrl Pts',(25.6933750777826,57.4641072931025,40.1478601162467));
#172229=CARTESIAN_POINT('Ctrl Pts',(25.7002496417699,57.4592879447638,40.1453112228299));
#172230=CARTESIAN_POINT('Ctrl Pts',(25.7069034079257,57.4543452548722,40.1424401896328));
#172231=CARTESIAN_POINT('Ctrl Pts',(25.7093582436707,57.4525217023849,40.1413809526906));
#172232=CARTESIAN_POINT('Ctrl Pts',(25.7117828918954,57.4506813499534,40.1402777640512));
#172233=CARTESIAN_POINT('Ctrl Pts',(25.7141765267655,57.448825358522,40.1391317641987));
#172234=CARTESIAN_POINT('Ctrl Pts',(25.7186645921469,57.445345374588,40.1369830144753));
#172235=CARTESIAN_POINT('Ctrl Pts',(25.7230436262012,57.4418104097894,40.1346837565849));
#172236=CARTESIAN_POINT('Ctrl Pts',(25.7273081852392,57.438228116931,40.1322415082996));
#172237=CARTESIAN_POINT('Ctrl Pts',(25.7422341418723,57.4256900919268,40.1236936393008));
#172238=CARTESIAN_POINT('Ctrl Pts',(25.7557577777298,57.412572294099,40.113394140767));
#172239=CARTESIAN_POINT('Ctrl Pts',(25.7676457049096,57.3992028606059,40.101665321223));
#172240=CARTESIAN_POINT('Ctrl Pts',(25.7735896684995,57.3925181438593,40.095800911451));
#172241=CARTESIAN_POINT('Ctrl Pts',(25.7791247053306,57.3857705191194,40.0895791707949));
#172242=CARTESIAN_POINT('Ctrl Pts',(25.7842216455743,57.3790010116301,40.0830403822906));
#172243=CARTESIAN_POINT('Ctrl Pts',(25.7867701156962,57.3756162578854,40.0797709880385));
#172244=CARTESIAN_POINT('Ctrl Pts',(25.7892090617198,57.3722260335602,40.0764223317514));
#172245=CARTESIAN_POINT('Ctrl Pts',(25.7915348376382,57.3688354672939,40.0729994484778));
#172246=CARTESIAN_POINT('Ctrl Pts',(25.7938606135566,57.3654449010277,40.0695765652042));
#172247=CARTESIAN_POINT('Ctrl Pts',(25.7960730898191,57.3620539952071,40.0660793733488));
#172248=CARTESIAN_POINT('Ctrl Pts',(25.7981688856973,57.3586678750407,40.0625130768817));
#172249=CARTESIAN_POINT('Ctrl Pts',(25.7981867584468,57.3586389985273,40.0624826638418));
#172250=CARTESIAN_POINT('Ctrl Pts',(25.7982046227317,57.3586101224998,40.0624522459912));
#172251=CARTESIAN_POINT('Ctrl Pts',(25.7982224785504,57.358581246961,40.0624218233329));
#172252=CARTESIAN_POINT('Ctrl Pts',(25.8073417058668,57.3438340877005,40.0468845275908));
#172253=CARTESIAN_POINT('Ctrl Pts',(25.8143796853889,57.3292509568918,40.0302263329258));
#172254=CARTESIAN_POINT('Ctrl Pts',(25.8194671333542,57.3149837826022,40.0127515884775));
#172255=CARTESIAN_POINT('Ctrl Pts',(25.8247266354315,57.3002341019519,39.9946858597757));
#172256=CARTESIAN_POINT('Ctrl Pts',(25.827901340928,57.285821218826,39.9757460620543));
#172257=CARTESIAN_POINT('Ctrl Pts',(25.8290839028447,57.2719197677231,39.9562444559192));
#172258=CARTESIAN_POINT('Ctrl Pts',(25.8302439699455,57.2582827514719,39.9371138113683));
#172259=CARTESIAN_POINT('Ctrl Pts',(25.8294864849003,57.2451370982925,39.9174410654434));
#172260=CARTESIAN_POINT('Ctrl Pts',(25.8268549466948,57.2326665944531,39.8975196504234));
#172261=CARTESIAN_POINT('Ctrl Pts',(25.8251116448908,57.224405322854,39.8843224113834));
#172262=CARTESIAN_POINT('Ctrl Pts',(25.8225450142739,57.216440747915,39.8710160447161));
#172263=CARTESIAN_POINT('Ctrl Pts',(25.8191582032627,57.2088336324696,39.8576902534424));
#172264=CARTESIAN_POINT('',(25.6742415049986,56.8833377255391,39.2875012672119));
#172265=CARTESIAN_POINT('',(25.8191582032627,57.2088336324696,39.8576902534424));
#172266=CARTESIAN_POINT('',(30.9286463962985,54.2060847114738,39.2875012672119));
#172267=CARTESIAN_POINT('Origin',(5.53234440788222E-15,0.,39.2875012672119));
#172268=CARTESIAN_POINT('',(31.1067982185541,54.5146464769134,39.8576902534424));
#172269=CARTESIAN_POINT('',(30.9286463962985,54.2060847114738,39.2875012672119));
#172270=CARTESIAN_POINT('',(31.4638515574747,54.5275217339716,40.1599502534424));
#172271=CARTESIAN_POINT('Ctrl Pts',(31.1067982185541,54.5146464769134,39.8576902534424));
#172272=CARTESIAN_POINT('Ctrl Pts',(31.1129513003045,54.5253036631383,39.8773836120348));
#172273=CARTESIAN_POINT('Ctrl Pts',(31.1207731649983,54.5349507607431,39.8969946442101));
#172274=CARTESIAN_POINT('Ctrl Pts',(31.130109547665,54.5434787028951,39.9162525288194));
#172275=CARTESIAN_POINT('Ctrl Pts',(31.1396335346537,54.5521780046478,39.9358973794001));
#172276=CARTESIAN_POINT('Ctrl Pts',(31.1507339420424,54.5597135487704,39.9551762199662));
#172277=CARTESIAN_POINT('Ctrl Pts',(31.1632971162134,54.5659508935486,39.9738152034151));
#172278=CARTESIAN_POINT('Ctrl Pts',(31.1753722224568,54.5719459231365,39.9917300792537));
#172279=CARTESIAN_POINT('Ctrl Pts',(31.1887993692979,54.5767421714175,40.0090551158002));
#172280=CARTESIAN_POINT('Ctrl Pts',(31.203514327957,54.5801937574243,40.0255394551403));
#172281=CARTESIAN_POINT('Ctrl Pts',(31.2148178485824,54.582845146023,40.0382021526065));
#172282=CARTESIAN_POINT('Ctrl Pts',(31.2268820502,54.5847026428002,40.0503687782083));
#172283=CARTESIAN_POINT('Ctrl Pts',(31.2396897946776,54.5856859723269,40.0619155352442));
#172284=CARTESIAN_POINT('Ctrl Pts',(31.2397233614918,54.5856885494582,40.0619457972351));
#172285=CARTESIAN_POINT('Ctrl Pts',(31.2397569340488,54.5856911200398,40.0619760547304));
#172286=CARTESIAN_POINT('Ctrl Pts',(31.2397905123454,54.5856936840712,40.0620063077269));
#172287=CARTESIAN_POINT('Ctrl Pts',(31.243390788585,54.5859686003822,40.06525004417));
#172288=CARTESIAN_POINT('Ctrl Pts',(31.2470554817647,54.5861671393373,40.0684393223556));
#172289=CARTESIAN_POINT('Ctrl Pts',(31.2507796687845,54.586288957092,40.0715697951759));
#172290=CARTESIAN_POINT('Ctrl Pts',(31.2715039227771,54.586966845199,40.0889901646416));
#172291=CARTESIAN_POINT('Ctrl Pts',(31.294070303672,54.5852738987618,40.1045963098235));
#172292=CARTESIAN_POINT('Ctrl Pts',(31.3175919772518,54.5811905703965,40.1176634650715));
#172293=CARTESIAN_POINT('Ctrl Pts',(31.3281488300912,54.5793579160787,40.1235281853056));
#172294=CARTESIAN_POINT('Ctrl Pts',(31.3388983725506,54.5770440083381,40.1288820140917));
#172295=CARTESIAN_POINT('Ctrl Pts',(31.3497625287432,54.5742478788456,40.1336621774101));
#172296=CARTESIAN_POINT('Ctrl Pts',(31.3544839440762,54.5730327187885,40.1357395717319));
#172297=CARTESIAN_POINT('Ctrl Pts',(31.3592268152918,54.5717264106366,40.1377083672883));
#172298=CARTESIAN_POINT('Ctrl Pts',(31.3639846100475,54.5703288332443,40.1395632548791));
#172299=CARTESIAN_POINT('Ctrl Pts',(31.3806368916924,54.5654373123716,40.1460553614469));
#172300=CARTESIAN_POINT('Ctrl Pts',(31.3974719850968,54.5594277405088,40.1511520974629));
#172301=CARTESIAN_POINT('Ctrl Pts',(31.4142098249422,54.5522949389282,40.1546258197409));
#172302=CARTESIAN_POINT('Ctrl Pts',(31.4225787448649,54.548728538138,40.1563626808798));
#172303=CARTESIAN_POINT('Ctrl Pts',(31.4309233516999,54.5448813304461,40.1576937882008));
#172304=CARTESIAN_POINT('Ctrl Pts',(31.4392086412369,54.5407526753744,40.1585906813668));
#172305=CARTESIAN_POINT('Ctrl Pts',(31.4433512860054,54.5386883478385,40.1590391279498));
#172306=CARTESIAN_POINT('Ctrl Pts',(31.4474791015111,54.5365536585644,40.1593790209175));
#172307=CARTESIAN_POINT('Ctrl Pts',(31.4515877125788,54.5343485280973,40.1596068022931));
#172308=CARTESIAN_POINT('Ctrl Pts',(31.4556963236466,54.5321433976301,40.1598345836687));
#172309=CARTESIAN_POINT('Ctrl Pts',(31.4597857294236,54.529867824492,40.1599502506864));
#172310=CARTESIAN_POINT('Ctrl Pts',(31.4638515574747,54.5275217339716,40.1599502534424));
#172311=CARTESIAN_POINT('',(31.4902932482914,54.5122556166607,40.1599502534424));
#172312=CARTESIAN_POINT('Origin',(5.57749365020894E-15,5.56029328078439E-15,
40.1599502534424));
#172313=CARTESIAN_POINT('',(31.6576696180591,54.1966007261204,39.8576902534424));
#172314=CARTESIAN_POINT('Ctrl Pts',(31.4902932482914,54.5122556166607,40.1599502534424));
#172315=CARTESIAN_POINT('Ctrl Pts',(31.4936024004378,54.5103440004407,40.1599502447858));
#172316=CARTESIAN_POINT('Ctrl Pts',(31.4968786114299,54.5083962906201,40.1598744685927));
#172317=CARTESIAN_POINT('Ctrl Pts',(31.5001207716291,54.5064144237352,40.1597246934279));
#172318=CARTESIAN_POINT('Ctrl Pts',(31.5188564579433,54.4949616780379,40.1588591777433));
#172319=CARTESIAN_POINT('Ctrl Pts',(31.536458384324,54.4823684499298,40.1555254706011));
#172320=CARTESIAN_POINT('Ctrl Pts',(31.5527059087901,54.4690111814044,40.1500631826357));
#172321=CARTESIAN_POINT('Ctrl Pts',(31.5592589091609,54.4636238877412,40.1478601162463));
#172322=CARTESIAN_POINT('Ctrl Pts',(31.5655920544911,54.4581123526882,40.1453112228296));
#172323=CARTESIAN_POINT('Ctrl Pts',(31.5716927188405,54.4525012314181,40.1424401896328));
#172324=CARTESIAN_POINT('Ctrl Pts',(31.5739434935993,54.4504310683342,40.1413809526905));
#172325=CARTESIAN_POINT('Ctrl Pts',(31.5761624901357,54.448347352793,40.1402777640511));
#172326=CARTESIAN_POINT('Ctrl Pts',(31.5783490084914,54.4462513257022,40.1391317641987));
#172327=CARTESIAN_POINT('Ctrl Pts',(31.5824487304082,54.442321274907,40.1369830144753));
#172328=CARTESIAN_POINT('Ctrl Pts',(31.5864342712177,54.4383479413151,40.134683756585));
#172329=CARTESIAN_POINT('Ctrl Pts',(31.5903010169876,54.4343395048291,40.1322415082996));
#172330=CARTESIAN_POINT('Ctrl Pts',(31.6038346271825,54.420309977128,40.1236936393009));
#172331=CARTESIAN_POINT('Ctrl Pts',(31.6159129958993,54.4058504350953,40.113394140767));
#172332=CARTESIAN_POINT('Ctrl Pts',(31.6263383134323,54.3913116139982,40.101665321223));
#172333=CARTESIAN_POINT('Ctrl Pts',(31.6315509721988,54.3840422034496,40.095800911451));
#172334=CARTESIAN_POINT('Ctrl Pts',(31.6363503686743,54.37675297401,40.0895791707949));
#172335=CARTESIAN_POINT('Ctrl Pts',(31.6407117811311,54.3694877752599,40.0830403822906));
#172336=CARTESIAN_POINT('Ctrl Pts',(31.6428924873595,54.3658551758849,40.0797709880385));
#172337=CARTESIAN_POINT('Ctrl Pts',(31.6449636976428,54.3622285842835,40.0764223317514));
#172338=CARTESIAN_POINT('Ctrl Pts',(31.6469223220359,54.3586134821113,40.0729994484778));
#172339=CARTESIAN_POINT('Ctrl Pts',(31.648880946429,54.3549983799391,40.0695765652042));
#172340=CARTESIAN_POINT('Ctrl Pts',(31.6507268563406,54.3513947831117,40.0660793733488));
#172341=CARTESIAN_POINT('Ctrl Pts',(31.6524572252922,54.3478081421434,40.0625130768817));
#172342=CARTESIAN_POINT('Ctrl Pts',(31.6524719817154,54.3477775556075,40.0624826638418));
#172343=CARTESIAN_POINT('Ctrl Pts',(31.6524867297711,54.3477469704397,40.0624522459912));
#172344=CARTESIAN_POINT('Ctrl Pts',(31.6525014694581,54.3477163866428,40.0624218233329));
#172345=CARTESIAN_POINT('Ctrl Pts',(31.660029242797,54.3320967950481,40.0468845275927));
#172346=CARTESIAN_POINT('Ctrl Pts',(31.6655043152774,54.3168578829737,40.0302263329298));
#172347=CARTESIAN_POINT('Ctrl Pts',(31.6690725678669,54.3021370826415,40.0127515884839));
#172348=CARTESIAN_POINT('Ctrl Pts',(31.6727614963895,54.286918434617,39.9946858597844));
#172349=CARTESIAN_POINT('Ctrl Pts',(31.6744122539932,54.2722526596876,39.9757460620654));
#172350=CARTESIAN_POINT('Ctrl Pts',(31.674135240392,54.2583037508099,39.956244455933));
#172351=CARTESIAN_POINT('Ctrl Pts',(31.6738634961724,54.2446201795303,39.9371138113845));
#172352=CARTESIAN_POINT('Ctrl Pts',(31.6717360657854,54.2316257183632,39.9174410654619));
#172353=CARTESIAN_POINT('Ctrl Pts',(31.6678154208207,54.219498599894,39.8975196504443));
#172354=CARTESIAN_POINT('Ctrl Pts',(31.665218130981,54.2114648090591,39.8843224113974));
#172355=CARTESIAN_POINT('Ctrl Pts',(31.6618330358548,54.2038121508449,39.8710160447231));
#172356=CARTESIAN_POINT('Ctrl Pts',(31.6576696180591,54.1966007261204,39.8576902534424));
#172357=CARTESIAN_POINT('',(31.4795232016796,53.8880358395967,39.2875012672119));
#172358=CARTESIAN_POINT('',(31.6576696180591,54.1966007261204,39.8576902534424));
#172359=CARTESIAN_POINT('',(36.4252947698685,50.6762142289944,39.2875012672119));
#172360=CARTESIAN_POINT('Origin',(5.53234440788222E-15,0.,39.2875012672119));
#172361=CARTESIAN_POINT('',(36.634724144966,50.9644637245889,39.8576902534424));
#172362=CARTESIAN_POINT('',(36.4252947698685,50.6762142289944,39.2875012672119));
#172363=CARTESIAN_POINT('',(36.9911673391713,50.9399462128198,40.1599502534424));
#172364=CARTESIAN_POINT('Ctrl Pts',(36.634724144966,50.9644637245889,39.8576902534424));
#172365=CARTESIAN_POINT('Ctrl Pts',(36.6419574987908,50.9744193574547,39.8773836120385));
#172366=CARTESIAN_POINT('Ctrl Pts',(36.6507449107808,50.9831959997547,39.8969946442174));
#172367=CARTESIAN_POINT('Ctrl Pts',(36.6609215604567,50.9907013072156,39.9162525288302));
#172368=CARTESIAN_POINT('Ctrl Pts',(36.6713026986945,50.9983574255601,39.9358973794146));
#172369=CARTESIAN_POINT('Ctrl Pts',(36.6831299757402,51.004691380658,39.9551762199843));
#172370=CARTESIAN_POINT('Ctrl Pts',(36.6962763075968,51.0095813473188,39.9738152034364));
#172371=CARTESIAN_POINT('Ctrl Pts',(36.7089119163785,51.0142813432078,39.9917300792784));
#172372=CARTESIAN_POINT('Ctrl Pts',(36.7227668523708,51.0176477981128,40.0090551158278));
#172373=CARTESIAN_POINT('Ctrl Pts',(36.7377619899324,51.0195423439532,40.0255394551704));
#172374=CARTESIAN_POINT('Ctrl Pts',(36.7492807342569,51.0209976683247,40.0382021526258));
#172375=CARTESIAN_POINT('Ctrl Pts',(36.7614730081902,51.0215839370833,40.0503687782175));
#172376=CARTESIAN_POINT('Ctrl Pts',(36.7743133764177,51.0212231059801,40.0619155352442));
#172377=CARTESIAN_POINT('Ctrl Pts',(36.7743470287329,51.0212221603061,40.0619457972352));
#172378=CARTESIAN_POINT('Ctrl Pts',(36.7743806860749,51.021221207518,40.0619760547305));
#172379=CARTESIAN_POINT('Ctrl Pts',(36.7744143484403,51.0212202476157,40.062006307727));
#172380=CARTESIAN_POINT('Ctrl Pts',(36.7780236385695,51.0211173265636,40.06525004417));
#172381=CARTESIAN_POINT('Ctrl Pts',(36.7816890091485,51.0209317131551,40.0684393223556));
#172382=CARTESIAN_POINT('Ctrl Pts',(36.7854055281047,51.0206635800333,40.0715697951759));
#172383=CARTESIAN_POINT('Ctrl Pts',(36.8060871110678,51.0191714801762,40.0889901646418));
#172384=CARTESIAN_POINT('Ctrl Pts',(36.8283529098778,51.0151289787602,40.1045963098238));
#172385=CARTESIAN_POINT('Ctrl Pts',(36.8513189052297,51.008609334902,40.1176634650719));
#172386=CARTESIAN_POINT('Ctrl Pts',(36.861626361985,51.0056832284521,40.1235281853059));
#172387=CARTESIAN_POINT('Ctrl Pts',(36.8720751481056,51.0022583633862,40.1288820140918));
#172388=CARTESIAN_POINT('Ctrl Pts',(36.8825875141947,50.9983419378321,40.1336621774101));
#172389=CARTESIAN_POINT('Ctrl Pts',(36.8871560463071,50.9966399122597,40.1357395717319));
#172390=CARTESIAN_POINT('Ctrl Pts',(36.8917363891942,50.9948449951609,40.1377083672884));
#172391=CARTESIAN_POINT('Ctrl Pts',(36.8963220336353,50.9929577488695,40.1395632548792));
#172392=CARTESIAN_POINT('Ctrl Pts',(36.9123717891792,50.9863523868496,40.146055361447));
#172393=CARTESIAN_POINT('Ctrl Pts',(36.9284864868686,50.9786159896077,40.1511520974629));
#172394=CARTESIAN_POINT('Ctrl Pts',(36.9443870542881,50.9697726815831,40.1546258197408));
#172395=CARTESIAN_POINT('Ctrl Pts',(36.9523373379978,50.9653510275708,40.1563626808798));
#172396=CARTESIAN_POINT('Ctrl Pts',(36.9602340894955,50.9606526463562,40.1576937882008));
#172397=CARTESIAN_POINT('Ctrl Pts',(36.9680424293795,50.9556805599059,40.1585906813668));
#172398=CARTESIAN_POINT('Ctrl Pts',(36.9719465993215,50.9531945166808,40.1590391279498));
#172399=CARTESIAN_POINT('Ctrl Pts',(36.9758286664326,50.9506400472465,40.1593790209175));
#172400=CARTESIAN_POINT('Ctrl Pts',(36.9796842712,50.9480175299136,40.1596068022931));
#172401=CARTESIAN_POINT('Ctrl Pts',(36.9835398759674,50.9453950125808,40.1598345836687));
#172402=CARTESIAN_POINT('Ctrl Pts',(36.9873690173885,50.942704445969,40.1599502506864));
#172403=CARTESIAN_POINT('Ctrl Pts',(36.9911673391713,50.9399462128198,40.1599502534424));
#172404=CARTESIAN_POINT('',(37.0158684358566,50.9219998155896,40.1599502534424));
#172405=CARTESIAN_POINT('Origin',(5.56385071146069E-15,5.56915310880103E-15,
40.1599502534424));
#172406=CARTESIAN_POINT('',(37.1493329797267,50.590578520848,39.8576902534424));
#172407=CARTESIAN_POINT('Ctrl Pts',(37.0158684358566,50.9219998155896,40.1599502534424));
#172408=CARTESIAN_POINT('Ctrl Pts',(37.0189596418154,50.9197527708146,40.1599502447858));
#172409=CARTESIAN_POINT('Ctrl Pts',(37.0220143142664,50.9174732734519,40.1598744685927));
#172410=CARTESIAN_POINT('Ctrl Pts',(37.025031552073,50.9151633654179,40.1597246934279));
#172411=CARTESIAN_POINT('Ctrl Pts',(37.0424674644282,50.901814946562,40.1588591777434));
#172412=CARTESIAN_POINT('Ctrl Pts',(37.0586566148318,50.8874508031609,40.1555254706015));
#172413=CARTESIAN_POINT('Ctrl Pts',(37.0734189189057,50.8724683783868,40.1500631826367));
#172414=CARTESIAN_POINT('Ctrl Pts',(37.079372895728,50.8664256218225,40.1478601162471));
#172415=CARTESIAN_POINT('Ctrl Pts',(37.085095235137,50.8602822855852,40.1453112228301));
#172416=CARTESIAN_POINT('Ctrl Pts',(37.090575957526,50.8540642095543,40.1424401896328));
#172417=CARTESIAN_POINT('Ctrl Pts',(37.0925980113393,50.8517701170137,40.1413809526906));
#172418=CARTESIAN_POINT('Ctrl Pts',(37.0945870443971,50.8494658679862,40.1402777640511));
#172419=CARTESIAN_POINT('Ctrl Pts',(37.0965424902857,50.8471527697475,40.1391317641987));
#172420=CARTESIAN_POINT('Ctrl Pts',(37.1002089513267,50.84281571055,40.1369830144753));
#172421=CARTESIAN_POINT('Ctrl Pts',(37.1037573324722,50.8384475408391,40.1346837565849));
#172422=CARTESIAN_POINT('Ctrl Pts',(37.1071839000983,50.8340568779944,40.1322415082996));
#172423=CARTESIAN_POINT('Ctrl Pts',(37.1191768867895,50.8186895580379,40.1236936393008));
#172424=CARTESIAN_POINT('Ctrl Pts',(37.1296776552305,50.8030466935687,40.113394140767));
#172425=CARTESIAN_POINT('Ctrl Pts',(37.1385261411562,50.7874977752339,40.101665321223));
#172426=CARTESIAN_POINT('Ctrl Pts',(37.1429503841191,50.7797233160665,40.095800911451));
#172427=CARTESIAN_POINT('Ctrl Pts',(37.1469615570468,50.7719723442503,40.0895791707949));
#172428=CARTESIAN_POINT('Ctrl Pts',(37.1505396571691,50.7642910532773,40.0830403822906));
#172429=CARTESIAN_POINT('Ctrl Pts',(37.1523287072303,50.7604504077909,40.0797709880385));
#172430=CARTESIAN_POINT('Ctrl Pts',(37.1540094891599,50.7566271826096,40.0764223317514));
#172431=CARTESIAN_POINT('Ctrl Pts',(37.1555795029291,50.7528271523475,40.0729994484778));
#172432=CARTESIAN_POINT('Ctrl Pts',(37.1571495166982,50.7490271220854,40.0695765652042));
#172433=CARTESIAN_POINT('Ctrl Pts',(37.1586086360836,50.7452503160121,40.0660793733488));
#172434=CARTESIAN_POINT('Ctrl Pts',(37.1599546198243,50.7415024502308,40.0625130768817));
#172435=CARTESIAN_POINT('Ctrl Pts',(37.1599660982467,50.741470488785,40.0624826638418));
#172436=CARTESIAN_POINT('Ctrl Pts',(37.1599775684904,50.7414385295743,40.0624522459912));
#172437=CARTESIAN_POINT('Ctrl Pts',(37.1599890305545,50.7414065726018,40.0624218233329));
#172438=CARTESIAN_POINT('Ctrl Pts',(37.1658428740582,50.7250856801826,40.0468845275902));
#172439=CARTESIAN_POINT('Ctrl Pts',(37.1696950534579,50.709357947548,40.0302263329246));
#172440=CARTESIAN_POINT('Ctrl Pts',(37.1717050161492,50.6943448053385,40.0127515884756));
#172441=CARTESIAN_POINT('Ctrl Pts',(37.1737829544441,50.6788239286284,39.9946858597729));
#172442=CARTESIAN_POINT('Ctrl Pts',(37.1738916781079,50.664065943191,39.9757460620504));
#172443=CARTESIAN_POINT('Ctrl Pts',(37.1721581240054,50.6502224036999,39.9562444559144));
#172444=CARTESIAN_POINT('Ctrl Pts',(37.1704575457498,50.6366421974596,39.9371138113623));
#172445=CARTESIAN_POINT('Ctrl Pts',(37.1669834785902,50.6239412983381,39.9174410654362));
#172446=CARTESIAN_POINT('Ctrl Pts',(37.1618166822689,50.612290432485,39.897519650415));
#172447=CARTESIAN_POINT('Ctrl Pts',(37.158393860846,50.6045721423189,39.8843224113778));
#172448=CARTESIAN_POINT('Ctrl Pts',(37.1542273890247,50.5973152449643,39.8710160447133));
#172449=CARTESIAN_POINT('Ctrl Pts',(37.1493329797266,50.590578520848,39.8576902534424));
#172450=CARTESIAN_POINT('',(36.9399086546492,50.3023253561991,39.2875012672119));
#172451=CARTESIAN_POINT('',(37.1493329797266,50.590578520848,39.8576902534424));
#172452=CARTESIAN_POINT('',(41.5228599914568,46.5911245387425,39.2875012672119));
#172453=CARTESIAN_POINT('Origin',(5.53234440788222E-15,0.,39.2875012672119));
#172454=CARTESIAN_POINT('',(41.7612723673368,46.855903642698,39.8576902534424));
#172455=CARTESIAN_POINT('',(41.5228599914568,46.5911245387425,39.2875012672119));
#172456=CARTESIAN_POINT('',(42.1132001506006,46.7942619810912,40.1599502534424));
#172457=CARTESIAN_POINT('Ctrl Pts',(41.7612723673368,46.855903642698,39.8576902534424));
#172458=CARTESIAN_POINT('Ctrl Pts',(41.7695067430961,46.8650486462045,39.8773836120362));
#172459=CARTESIAN_POINT('Ctrl Pts',(41.779163425655,46.8728586744673,39.8969946442129));
#172460=CARTESIAN_POINT('Ctrl Pts',(41.7900688448329,46.8792591175164,39.9162525288236));
#172461=CARTESIAN_POINT('Ctrl Pts',(41.8011933963927,46.885788170416,39.9358973794055));
#172462=CARTESIAN_POINT('Ctrl Pts',(41.8136179609679,46.8908511403508,39.9551762199728));
#172463=CARTESIAN_POINT('Ctrl Pts',(41.8272034165412,46.8943401533964,39.9738152034229));
#172464=CARTESIAN_POINT('Ctrl Pts',(41.8402610894808,46.897693621448,39.9917300792622));
#172465=CARTESIAN_POINT('Ctrl Pts',(41.8543920170388,46.8995933993937,40.0090551158092));
#172466=CARTESIAN_POINT('Ctrl Pts',(41.8695030436299,46.8999101480293,40.0255394551499));
#172467=CARTESIAN_POINT('Ctrl Pts',(41.8811108098934,46.9001534633397,40.0382021526126));
#172468=CARTESIAN_POINT('Ctrl Pts',(41.893297575053,46.899462080799,40.0503687782112));
#172469=CARTESIAN_POINT('Ctrl Pts',(41.906029885286,46.8977610424068,40.0619155352442));
#172470=CARTESIAN_POINT('Ctrl Pts',(41.9060632544005,46.8977565842885,40.0619457972351));
#172471=CARTESIAN_POINT('Ctrl Pts',(41.9060966277705,46.8977521185696,40.0619760547305));
#172472=CARTESIAN_POINT('Ctrl Pts',(41.9061300053929,46.8977476452504,40.0620063077269));
#172473=CARTESIAN_POINT('Ctrl Pts',(41.9097087652737,46.89726801446,40.06525004417));
#172474=CARTESIAN_POINT('Ctrl Pts',(41.9133346546847,46.8967002823072,40.0684393223556));
#172475=CARTESIAN_POINT('Ctrl Pts',(41.9170027866181,46.8960451360315,40.0715697951759));
#172476=CARTESIAN_POINT('Ctrl Pts',(41.9374151068048,46.8923993959677,40.0889901646453));
#172477=CARTESIAN_POINT('Ctrl Pts',(41.959136374783,46.8860516300625,40.10459630983));
#172478=CARTESIAN_POINT('Ctrl Pts',(41.9812950716606,46.8771671012912,40.1176634650798));
#172479=CARTESIAN_POINT('Ctrl Pts',(41.9912402016744,46.8731796017451,40.1235281853107));
#172480=CARTESIAN_POINT('Ctrl Pts',(42.0012737523646,46.8686813028939,40.128882014094));
#172481=CARTESIAN_POINT('Ctrl Pts',(42.0113191526632,46.8636874904585,40.1336621774102));
#172482=CARTESIAN_POINT('Ctrl Pts',(42.0156847477611,46.8615172471192,40.135739571732));
#172483=CARTESIAN_POINT('Ctrl Pts',(42.0200523791246,46.8592533865608,40.1377083672884));
#172484=CARTESIAN_POINT('Ctrl Pts',(42.024415631971,46.8568971484355,40.1395632548792));
#172485=CARTESIAN_POINT('Ctrl Pts',(42.0396870169335,46.8486503149971,40.146055361447));
#172486=CARTESIAN_POINT('Ctrl Pts',(42.0549047629079,46.8392718539633,40.151152097463));
#172487=CARTESIAN_POINT('Ctrl Pts',(42.0697938479573,46.8288149286279,40.1546258197409));
#172488=CARTESIAN_POINT('Ctrl Pts',(42.077238390482,46.8235864659602,40.1563626808798));
#172489=CARTESIAN_POINT('Ctrl Pts',(42.0846007681805,46.8180883876706,40.1576937882008));
#172490=CARTESIAN_POINT('Ctrl Pts',(42.0918466086057,46.8123273450614,40.1585906813668));
#172491=CARTESIAN_POINT('Ctrl Pts',(42.0954695288184,46.8094468237568,40.1590391279498));
#172492=CARTESIAN_POINT('Ctrl Pts',(42.0990633147952,46.8065005614639,40.1593790209175));
#172493=CARTESIAN_POINT('Ctrl Pts',(42.1026236704495,46.8034893901141,40.1596068022931));
#172494=CARTESIAN_POINT('Ctrl Pts',(42.1061840261039,46.8004782187644,40.1598345836687));
#172495=CARTESIAN_POINT('Ctrl Pts',(42.1097109502944,46.7974021370896,40.1599502506864));
#172496=CARTESIAN_POINT('Ctrl Pts',(42.1132001506006,46.7942619810912,40.1599502534424));
#172497=CARTESIAN_POINT('',(42.1358900227701,46.7738319284252,40.1599502534424));
#172498=CARTESIAN_POINT('Origin',(5.55120861436579E-15,5.57939047717458E-15,
40.1599502534424));
#172499=CARTESIAN_POINT('',(42.2339804752707,46.430275350542,39.8576902534424));
#172500=CARTESIAN_POINT('Ctrl Pts',(42.1358900227701,46.7738319284252,40.1599502534424));
#172501=CARTESIAN_POINT('Ctrl Pts',(42.138729414642,46.7712740741881,40.1599502447857));
#172502=CARTESIAN_POINT('Ctrl Pts',(42.1415290809214,46.7686877639334,40.1598744685927));
#172503=CARTESIAN_POINT('Ctrl Pts',(42.1442883388465,46.766075122586,40.1597246934279));
#172504=CARTESIAN_POINT('Ctrl Pts',(42.1602334457308,46.7509772786493,40.1588591777438));
#172505=CARTESIAN_POINT('Ctrl Pts',(42.1748324484317,46.7349995965244,40.1555254706051));
#172506=CARTESIAN_POINT('Ctrl Pts',(42.1879477932161,46.718556166091,40.1500631826455));
#172507=CARTESIAN_POINT('Ctrl Pts',(42.1932375134805,46.7119241523232,40.1478601162538));
#172508=CARTESIAN_POINT('Ctrl Pts',(42.1982863518264,46.705216322571,40.1453112228339));
#172509=CARTESIAN_POINT('Ctrl Pts',(42.2030870843191,46.6984594183133,40.1424401896328));
#172510=CARTESIAN_POINT('Ctrl Pts',(42.2048582631421,46.6959665308739,40.1413809526905));
#172511=CARTESIAN_POINT('Ctrl Pts',(42.2065955404589,46.6934669941948,40.1402777640511));
#172512=CARTESIAN_POINT('Ctrl Pts',(42.208298489606,46.6909621675966,40.1391317641986));
#172513=CARTESIAN_POINT('Ctrl Pts',(42.2114915192568,46.6862656177249,40.1369830144753));
#172514=CARTESIAN_POINT('Ctrl Pts',(42.214563863932,46.6815504704765,40.1346837565849));
#172515=CARTESIAN_POINT('Ctrl Pts',(42.2175127112221,46.676825686294,40.1322415082996));
#172516=CARTESIAN_POINT('Ctrl Pts',(42.2278336767378,46.6602889416554,40.1236936393008));
#172517=CARTESIAN_POINT('Ctrl Pts',(42.2366417962865,46.6436341412461,40.113394140767));
#172518=CARTESIAN_POINT('Ctrl Pts',(42.2438165047415,46.6272454828769,40.101665321223));
#172519=CARTESIAN_POINT('Ctrl Pts',(42.247403858969,46.6190511536923,40.095800911451));
#172520=CARTESIAN_POINT('Ctrl Pts',(42.2505828610989,46.6109233607685,40.0895791707949));
#172521=CARTESIAN_POINT('Ctrl Pts',(42.253338446473,46.6029101354041,40.0830403822906));
#172522=CARTESIAN_POINT('Ctrl Pts',(42.2547162391601,46.5989035227218,40.0797709880385));
#172523=CARTESIAN_POINT('Ctrl Pts',(42.2559881777376,46.594925552016,40.0764223317514));
#172524=CARTESIAN_POINT('Ctrl Pts',(42.2571523794834,46.5909822275907,40.0729994484778));
#172525=CARTESIAN_POINT('Ctrl Pts',(42.2583165812292,46.5870389031653,40.0695765652042));
#172526=CARTESIAN_POINT('Ctrl Pts',(42.2593729236709,46.5831302673238,40.0660793733488));
#172527=CARTESIAN_POINT('Ctrl Pts',(42.2603197753212,46.5792622391315,40.0625130768816));
#172528=CARTESIAN_POINT('Ctrl Pts',(42.2603278499828,46.5792292529519,40.0624826638418));
#172529=CARTESIAN_POINT('Ctrl Pts',(42.2603359167441,46.5791962698501,40.0624522459912));
#172530=CARTESIAN_POINT('Ctrl Pts',(42.2603439756046,46.5791632898293,40.0624218233329));
#172531=CARTESIAN_POINT('Ctrl Pts',(42.2644597533381,46.5623199116979,40.0468845275875));
#172532=CARTESIAN_POINT('Ctrl Pts',(42.2666468343731,46.5462756748327,40.0302263329187));
#172533=CARTESIAN_POINT('Ctrl Pts',(42.267076485594,46.5311346778733,40.0127515884664));
#172534=CARTESIAN_POINT('Ctrl Pts',(42.2675206673339,46.515481622451,39.9946858597607));
#172535=CARTESIAN_POINT('Ctrl Pts',(42.2660861658584,46.5007931180827,39.975746062035));
#172536=CARTESIAN_POINT('Ctrl Pts',(42.2629150644359,46.4872066206944,39.9562444558956));
#172537=CARTESIAN_POINT('Ctrl Pts',(42.2598042840353,46.4738785670757,39.937113811341));
#172538=CARTESIAN_POINT('Ctrl Pts',(42.25502164271,46.4616103837094,39.9174410654122));
#172539=CARTESIAN_POINT('Ctrl Pts',(42.248665303534,46.4505634197978,39.8975196503884));
#172540=CARTESIAN_POINT('Ctrl Pts',(42.2444544516767,46.4432451935018,39.8843224113599));
#172541=CARTESIAN_POINT('Ctrl Pts',(42.2395522518982,46.4364635650919,39.8710160447043));
#172542=CARTESIAN_POINT('Ctrl Pts',(42.2339804752707,46.430275350542,39.8576902534424));
#172543=CARTESIAN_POINT('',(41.9955727382256,46.1654920697607,39.2875012672119));
#172544=CARTESIAN_POINT('',(42.2339804752707,46.430275350542,39.8576902534424));
#172545=CARTESIAN_POINT('',(46.1654920697617,41.9955727382246,39.2875012672119));
#172546=CARTESIAN_POINT('Origin',(5.53234440788222E-15,0.,39.2875012672119));
#172547=CARTESIAN_POINT('',(46.430275350543,42.2339804752696,39.8576902534424));
#172548=CARTESIAN_POINT('',(46.1654920697617,41.9955727382246,39.2875012672119));
#172549=CARTESIAN_POINT('',(46.7738319284262,42.1358900227689,40.1599502534424));
#172550=CARTESIAN_POINT('Ctrl Pts',(46.430275350543,42.2339804752696,39.8576902534424));
#172551=CARTESIAN_POINT('Ctrl Pts',(46.4394205306927,42.2422146548452,39.8773836120346));
#172552=CARTESIAN_POINT('Ctrl Pts',(46.4498406831856,42.2489725007674,39.8969946442096));
#172553=CARTESIAN_POINT('Ctrl Pts',(46.4613553898112,42.2541979548116,39.9162525288188));
#172554=CARTESIAN_POINT('Ctrl Pts',(46.4731014717785,42.2595284085969,39.935897379399));
#172555=CARTESIAN_POINT('Ctrl Pts',(46.4859871977545,42.2632649224109,39.9551762199648));
#172556=CARTESIAN_POINT('Ctrl Pts',(46.4998629319511,42.2653147554846,39.9738152034134));
#172557=CARTESIAN_POINT('Ctrl Pts',(46.5131996064525,42.2672849544014,39.9917300792513));
#172558=CARTESIAN_POINT('Ctrl Pts',(46.5274517041783,42.2676972410233,40.009055115797));
#172559=CARTESIAN_POINT('Ctrl Pts',(46.5425130602309,42.2664327220898,40.0255394551366));
#172560=CARTESIAN_POINT('Ctrl Pts',(46.5540826713154,42.2654613625244,40.0382021526041));
#172561=CARTESIAN_POINT('Ctrl Pts',(46.56613040695,42.2634999036149,40.0503687782072));
#172562=CARTESIAN_POINT('Ctrl Pts',(46.5786151613306,42.2604772948654,40.0619155352442));
#172563=CARTESIAN_POINT('Ctrl Pts',(46.5786478816453,42.260469373147,40.0619457972351));
#172564=CARTESIAN_POINT('Ctrl Pts',(46.5786806053978,42.2604614434247,40.0619760547305));
#172565=CARTESIAN_POINT('Ctrl Pts',(46.5787133325848,42.2604535056992,40.0620063077269));
#172566=CARTESIAN_POINT('Ctrl Pts',(46.5822223525751,42.2596024201057,40.06525004417));
#172567=CARTESIAN_POINT('Ctrl Pts',(46.5857690348151,42.2586587894009,40.0684393223556));
#172568=CARTESIAN_POINT('Ctrl Pts',(46.5893485909045,42.257623807891,40.0715697951758));
#172569=CARTESIAN_POINT('Ctrl Pts',(46.6092680066565,42.2518643711126,40.088990164643));
#172570=CARTESIAN_POINT('Ctrl Pts',(46.630206761038,42.2432808881728,40.104596309826));
#172571=CARTESIAN_POINT('Ctrl Pts',(46.6513153841135,42.2321288152491,40.1176634650747));
#172572=CARTESIAN_POINT('Ctrl Pts',(46.6607892264673,42.2271236104843,40.1235281853076));
#172573=CARTESIAN_POINT('Ctrl Pts',(46.6702976120535,42.2216011621487,40.1288820140926));
#172574=CARTESIAN_POINT('Ctrl Pts',(46.6797659870611,42.2155846760824,40.1336621774101));
#172575=CARTESIAN_POINT('Ctrl Pts',(46.6838808147711,42.2129699926164,40.1357395717319));
#172576=CARTESIAN_POINT('Ctrl Pts',(46.6879878819278,42.2102619919285,40.1377083672883));
#172577=CARTESIAN_POINT('Ctrl Pts',(46.6920809384683,42.2074625774073,40.1395632548791));
#172578=CARTESIAN_POINT('Ctrl Pts',(46.7064066363599,42.1976646265833,40.1460553614469));
#172579=CARTESIAN_POINT('Ctrl Pts',(46.72056070181,42.1867468541392,40.1511520974629));
#172580=CARTESIAN_POINT('Ctrl Pts',(46.7342751765578,42.1747908797552,40.1546258197408));
#172581=CARTESIAN_POINT('Ctrl Pts',(46.7411324139317,42.1688128925632,40.1563626808798));
#172582=CARTESIAN_POINT('Ctrl Pts',(46.7478797540803,42.1625753552949,40.1576937882008));
#172583=CARTESIAN_POINT('Ctrl Pts',(46.7544837081028,42.1560884757152,40.1585906813668));
#172584=CARTESIAN_POINT('Ctrl Pts',(46.7577856851141,42.1528450359254,40.1590391279498));
#172585=CARTESIAN_POINT('Ctrl Pts',(46.7610518156854,42.1495392606401,40.1593790209175));
#172586=CARTESIAN_POINT('Ctrl Pts',(46.7642779142251,42.1461724262968,40.1596068022931));
#172587=CARTESIAN_POINT('Ctrl Pts',(46.7675040127649,42.1428055919535,40.1598345836686));
#172588=CARTESIAN_POINT('Ctrl Pts',(46.7706900780053,42.1393776974103,40.1599502506865));
#172589=CARTESIAN_POINT('Ctrl Pts',(46.7738319284262,42.1358900227689,40.1599502534424));
#172590=CARTESIAN_POINT('',(46.7942619810922,42.1132001505995,40.1599502534424));
#172591=CARTESIAN_POINT('Origin',(5.53970586838553E-15,5.59089322315484E-15,
40.1599502534424));
#172592=CARTESIAN_POINT('',(46.855903642699,41.7612723673357,39.8576902534424));
#172593=CARTESIAN_POINT('Ctrl Pts',(46.7942619810922,42.1132001505995,40.1599502534424));
#172594=CARTESIAN_POINT('Ctrl Pts',(46.7968184499057,42.1103595112866,40.1599502447858));
#172595=CARTESIAN_POINT('Ctrl Pts',(46.7993324362838,42.1074947242962,40.1598744685927));
#172596=CARTESIAN_POINT('Ctrl Pts',(46.8018034833201,42.1046079742808,40.1597246934279));
#172597=CARTESIAN_POINT('Ctrl Pts',(46.8160830868243,42.087926120383,40.1588591777433));
#172598=CARTESIAN_POINT('Ctrl Pts',(46.828931992109,42.0705099543436,40.1555254706008));
#172599=CARTESIAN_POINT('Ctrl Pts',(46.8402566831536,42.0527856758954,40.1500631826351));
#172600=CARTESIAN_POINT('Ctrl Pts',(46.8448241915615,42.0456370666737,40.1478601162458));
#172601=CARTESIAN_POINT('Ctrl Pts',(46.8491442126995,42.0384382358125,40.1453112228294));
#172602=CARTESIAN_POINT('Ctrl Pts',(46.8532123574524,42.0312165334046,40.1424401896328));
#172603=CARTESIAN_POINT('Ctrl Pts',(46.8547132558794,42.0285521636629,40.1413809526906));
#172604=CARTESIAN_POINT('Ctrl Pts',(46.8561797434814,42.0258847247791,40.1402777640512));
#172605=CARTESIAN_POINT('Ctrl Pts',(46.8576115380198,42.0232156132257,40.1391317641987));
#172606=CARTESIAN_POINT('Ctrl Pts',(46.8602961527793,42.018211029063,40.1369830144753));
#172607=CARTESIAN_POINT('Ctrl Pts',(46.8628587997329,42.0132005644171,40.134683756585));
#172608=CARTESIAN_POINT('Ctrl Pts',(46.8652976184992,42.0081934246211,40.1322415082996));
#172609=CARTESIAN_POINT('Ctrl Pts',(46.8738334841813,41.990668435335,40.1236936393009));
#172610=CARTESIAN_POINT('Ctrl Pts',(46.8808524512367,41.9731841724643,40.113394140767));
#172611=CARTESIAN_POINT('Ctrl Pts',(46.8862747746138,41.9561353316312,40.101665321223));
#172612=CARTESIAN_POINT('Ctrl Pts',(46.8889859363023,41.9476109112146,40.095800911451));
#172613=CARTESIAN_POINT('Ctrl Pts',(46.8912979378218,41.9391953469836,40.0895791707949));
#172614=CARTESIAN_POINT('Ctrl Pts',(46.8932008176778,41.9309379818015,40.0830403822906));
#172615=CARTESIAN_POINT('Ctrl Pts',(46.8941522576058,41.9268092992105,40.0797709880385));
#172616=CARTESIAN_POINT('Ctrl Pts',(46.8950014172059,41.9227201664596,40.0764223317514));
#172617=CARTESIAN_POINT('Ctrl Pts',(46.8957470516903,41.9186767517586,40.0729994484778));
#172618=CARTESIAN_POINT('Ctrl Pts',(46.8964926861748,41.9146333370576,40.0695765652042));
#172619=CARTESIAN_POINT('Ctrl Pts',(46.8971346781641,41.91063569528,40.0660793733488));
#172620=CARTESIAN_POINT('Ctrl Pts',(46.8976720238192,41.9066898836029,40.0625130768817));
#172621=CARTESIAN_POINT('Ctrl Pts',(46.8976766062523,41.9066562340931,40.0624826638418));
#172622=CARTESIAN_POINT('Ctrl Pts',(46.8976811811501,41.9066225884701,40.0624522459912));
#172623=CARTESIAN_POINT('Ctrl Pts',(46.8976857485125,41.906588946737,40.0624218233329));
#172624=CARTESIAN_POINT('Ctrl Pts',(46.9000183671521,41.889407622475,40.0468845275904));
#172625=CARTESIAN_POINT('Ctrl Pts',(46.9005163877048,41.8732226654012,40.030226332925));
#172626=CARTESIAN_POINT('Ctrl Pts',(46.8993610201077,41.858119701628,40.0127515884763));
#172627=CARTESIAN_POINT('Ctrl Pts',(46.8981665787457,41.8425059656487,39.994685859774));
#172628=CARTESIAN_POINT('Ctrl Pts',(46.8952045688315,41.8280478726808,39.9757460620521));
#172629=CARTESIAN_POINT('Ctrl Pts',(46.8906306633432,41.8148672739068,39.9562444559166));
#172630=CARTESIAN_POINT('Ctrl Pts',(46.8861437631619,41.8019373978563,39.9371138113654));
#172631=CARTESIAN_POINT('Ctrl Pts',(46.8801049472942,41.7902363430309,39.9174410654402));
#172632=CARTESIAN_POINT('Ctrl Pts',(46.8726287066505,41.7799143139099,39.8975196504199));
#172633=CARTESIAN_POINT('Ctrl Pts',(46.8676759593288,41.7730763314905,39.8843224113811));
#172634=CARTESIAN_POINT('Ctrl Pts',(46.8620917411135,41.7668442729547,39.871016044715));
#172635=CARTESIAN_POINT('Ctrl Pts',(46.855903642699,41.7612723673357,39.8576902534424));
#172636=CARTESIAN_POINT('',(46.5911245387435,41.5228599914557,39.2875012672119));
#172637=CARTESIAN_POINT('',(46.855903642699,41.7612723673357,39.8576902534424));
#172638=CARTESIAN_POINT('',(50.3023253562,36.939908654648,39.2875012672119));
#172639=CARTESIAN_POINT('Origin',(5.53234440788222E-15,0.,39.2875012672119));
#172640=CARTESIAN_POINT('',(50.5905785208489,37.1493329797255,39.8576902534424));
#172641=CARTESIAN_POINT('',(50.3023253562,36.939908654648,39.2875012672119));
#172642=CARTESIAN_POINT('',(50.9219998155904,37.0158684358554,40.1599502534424));
#172643=CARTESIAN_POINT('Ctrl Pts',(50.5905785208489,37.1493329797255,39.8576902534424));
#172644=CARTESIAN_POINT('Ctrl Pts',(50.6005343088819,37.1565661199767,39.8773836120345));
#172645=CARTESIAN_POINT('Ctrl Pts',(50.6116037659383,37.1621977431848,39.8969946442095));
#172646=CARTESIAN_POINT('Ctrl Pts',(50.6236016024772,37.1661909570565,39.9162525288185));
#172647=CARTESIAN_POINT('Ctrl Pts',(50.6358405223212,37.1702644101609,39.9358973793989));
#172648=CARTESIAN_POINT('Ctrl Pts',(50.6490462309891,37.1726335298269,39.9551762199648));
#172649=CARTESIAN_POINT('Ctrl Pts',(50.6630602183632,37.1732217245281,39.9738152034136));
#172650=CARTESIAN_POINT('Ctrl Pts',(50.6765297750321,37.1737870683984,39.9917300792521));
#172651=CARTESIAN_POINT('Ctrl Pts',(50.690746893963,37.1727073465971,40.0090551157985));
#172652=CARTESIAN_POINT('Ctrl Pts',(50.7055935641109,37.1698754144274,40.0255394551386));
#172653=CARTESIAN_POINT('Ctrl Pts',(50.7169982609322,37.1677000224041,40.0382021526055));
#172654=CARTESIAN_POINT('Ctrl Pts',(50.7287749695242,37.1644899772801,40.0503687782078));
#172655=CARTESIAN_POINT('Ctrl Pts',(50.7408753824657,37.1601789145081,40.0619155352442));
#172656=CARTESIAN_POINT('Ctrl Pts',(50.7409070954901,37.1601676159814,40.0619457972351));
#172657=CARTESIAN_POINT('Ctrl Pts',(50.7409388110967,37.1601563091354,40.0619760547305));
#172658=CARTESIAN_POINT('Ctrl Pts',(50.7409705292826,37.1601449939711,40.0620063077269));
#172659=CARTESIAN_POINT('Ctrl Pts',(50.744371363825,37.1589317782463,40.06525004417));
#172660=CARTESIAN_POINT('Ctrl Pts',(50.7477999807011,37.1576225876051,40.0684393223556));
#172661=CARTESIAN_POINT('Ctrl Pts',(50.751251742581,37.1562191103349,40.0715697951759));
#172662=CARTESIAN_POINT('Ctrl Pts',(50.7704600126123,37.1484090784366,40.0889901646418));
#172663=CARTESIAN_POINT('Ctrl Pts',(50.7903868440238,37.1376839208971,40.1045963098239));
#172664=CARTESIAN_POINT('Ctrl Pts',(50.8102141228071,37.1243864882653,40.117663465072));
#172665=CARTESIAN_POINT('Ctrl Pts',(50.8191128801002,37.1184184163527,40.1235281853059));
#172666=CARTESIAN_POINT('Ctrl Pts',(50.8279919247187,37.1119323236325,40.1288820140919));
#172667=CARTESIAN_POINT('Ctrl Pts',(50.8367795369359,37.1049590818162,40.1336621774101));
#172668=CARTESIAN_POINT('Ctrl Pts',(50.8405985143445,37.1019286052426,40.1357395717319));
#172669=CARTESIAN_POINT('Ctrl Pts',(50.8444000194072,37.0988061338473,40.1377083672883));
#172670=CARTESIAN_POINT('Ctrl Pts',(50.8481780352577,37.0955942139016,40.1395632548791));
#172671=CARTESIAN_POINT('Ctrl Pts',(50.8614010907345,37.0843524940915,40.1460553614469));
#172672=CARTESIAN_POINT('Ctrl Pts',(50.8743364007572,37.0720150276367,40.1511520974629));
#172673=CARTESIAN_POINT('Ctrl Pts',(50.8867260065482,37.0586909963615,40.1546258197408));
#172674=CARTESIAN_POINT('Ctrl Pts',(50.8929208094437,37.0520289807239,40.1563626808798));
#172675=CARTESIAN_POINT('Ctrl Pts',(50.8989791867717,37.0451203242405,40.1576937882008));
#172676=CARTESIAN_POINT('Ctrl Pts',(50.9048689000892,37.0379786793004,40.1585906813668));
#172677=CARTESIAN_POINT('Ctrl Pts',(50.907813756748,37.0344078568303,40.1590391279498));
#172678=CARTESIAN_POINT('Ctrl Pts',(50.9107164475038,37.0307787873185,40.1593790209175));
#172679=CARTESIAN_POINT('Ctrl Pts',(50.9135729431182,37.0270931777233,40.1596068022931));
#172680=CARTESIAN_POINT('Ctrl Pts',(50.9164294387326,37.0234075681281,40.1598345836687));
#172681=CARTESIAN_POINT('Ctrl Pts',(50.9192397378254,37.0196654174464,40.1599502506864));
#172682=CARTESIAN_POINT('Ctrl Pts',(50.9219998155904,37.0158684358554,40.1599502534424));
#172683=CARTESIAN_POINT('',(50.9399462128206,36.9911673391701,40.1599502534424));
#172684=CARTESIAN_POINT('Origin',(5.52946850001198E-15,5.60353532024975E-15,
40.1599502534424));
#172685=CARTESIAN_POINT('',(50.9644637245897,36.6347241449648,39.8576902534424));
#172686=CARTESIAN_POINT('Ctrl Pts',(50.9399462128206,36.9911673391701,40.1599502534424));
#172687=CARTESIAN_POINT('Ctrl Pts',(50.9421917493684,36.9880750374201,40.1599502447858));
#172688=CARTESIAN_POINT('Ctrl Pts',(50.9443925120844,36.9849631608998,40.1598744685927));
#172689=CARTESIAN_POINT('Ctrl Pts',(50.9465482749236,36.9818339300537,40.1597246934279));
#172690=CARTESIAN_POINT('Ctrl Pts',(50.9590059247076,36.9637508360949,40.1588591777437));
#172691=CARTESIAN_POINT('Ctrl Pts',(50.9699639572682,36.94508700132,40.1555254706039));
#172692=CARTESIAN_POINT('Ctrl Pts',(50.9793739188788,36.9262760657806,40.1500631826426));
#172693=CARTESIAN_POINT('Ctrl Pts',(50.9831691728661,36.9186891827448,40.1478601162516));
#172694=CARTESIAN_POINT('Ctrl Pts',(50.9867130457535,36.9110782226527,40.1453112228326));
#172695=CARTESIAN_POINT('Ctrl Pts',(50.9900040313326,36.9034708445582,40.1424401896328));
#172696=CARTESIAN_POINT('Ctrl Pts',(50.9912182052063,36.9006641839067,40.1413809526905));
#172697=CARTESIAN_POINT('Ctrl Pts',(50.9923978359483,36.8978580678368,40.1402777640511));
#172698=CARTESIAN_POINT('Ctrl Pts',(50.9935427888375,36.8950539146729,40.1391317641987));
#172699=CARTESIAN_POINT('Ctrl Pts',(50.9956895755046,36.8897961274906,40.1369830144753));
#172700=CARTESIAN_POINT('Ctrl Pts',(50.9977144478404,36.8845452411463,40.1346837565849));
#172701=CARTESIAN_POINT('Ctrl Pts',(50.9996165178741,36.8793106050082,40.1322415082996));
#172702=CARTESIAN_POINT('Ctrl Pts',(51.006273762992,36.8609893785247,40.1236936393009));
#172703=CARTESIAN_POINT('Ctrl Pts',(51.0114266762823,36.8428672144354,40.113394140767));
#172704=CARTESIAN_POINT('Ctrl Pts',(51.0150372064717,36.8253449818063,40.101665321223));
#172705=CARTESIAN_POINT('Ctrl Pts',(51.0168424715664,36.8165838654917,40.095800911451));
#172706=CARTESIAN_POINT('Ctrl Pts',(51.0182621417031,36.8079727326361,40.0895791707949));
#172707=CARTESIAN_POINT('Ctrl Pts',(51.019291467691,36.7995616970574,40.0830403822906));
#172708=CARTESIAN_POINT('Ctrl Pts',(51.019806130685,36.795356179268,40.0797709880385));
#172709=CARTESIAN_POINT('Ctrl Pts',(51.0202232077374,36.7912006858661,40.0764223317514));
#172710=CARTESIAN_POINT('Ctrl Pts',(51.0205421056331,36.7871014813871,40.0729994484778));
#172711=CARTESIAN_POINT('Ctrl Pts',(51.0208610035287,36.7830022769081,40.0695765652042));
#172712=CARTESIAN_POINT('Ctrl Pts',(51.0210816112671,36.7789594281944,40.0660793733488));
#172713=CARTESIAN_POINT('Ctrl Pts',(51.0212035636555,36.7749790641709,40.0625130768816));
#172714=CARTESIAN_POINT('Ctrl Pts',(51.021204603654,36.774945120002,40.0624826638418));
#172715=CARTESIAN_POINT('Ctrl Pts',(51.0212056365647,36.7749111804862,40.0624522459912));
#172716=CARTESIAN_POINT('Ctrl Pts',(51.021206662388,36.7748772456266,40.0624218233329));
#172717=CARTESIAN_POINT('Ctrl Pts',(51.0217305652767,36.7575462174121,40.0468845275879));
#172718=CARTESIAN_POINT('Ctrl Pts',(51.0205340689293,36.7413978659011,40.0302263329196));
#172719=CARTESIAN_POINT('Ctrl Pts',(51.017806340962,36.726498406541,40.0127515884679));
#172720=CARTESIAN_POINT('Ctrl Pts',(51.0149863630461,36.7110950573594,39.994685859763));
#172721=CARTESIAN_POINT('Ctrl Pts',(51.0105292970913,36.6970257816808,39.9757460620383));
#172722=CARTESIAN_POINT('Ctrl Pts',(51.0046027001994,36.6843954909168,39.9562444558998));
#172723=CARTESIAN_POINT('Ctrl Pts',(50.9987888396517,36.6720054548607,39.9371138113467));
#172724=CARTESIAN_POINT('Ctrl Pts',(50.9915600117681,36.6609997277806,39.9174410654195));
#172725=CARTESIAN_POINT('Ctrl Pts',(50.9830457809093,36.651515723761,39.8975196503974));
#172726=CARTESIAN_POINT('Ctrl Pts',(50.977405401464,36.6452329035958,39.8843224113659));
#172727=CARTESIAN_POINT('Ctrl Pts',(50.9712003466817,36.639618694681,39.8710160447074));
#172728=CARTESIAN_POINT('Ctrl Pts',(50.9644637245897,36.6347241449648,39.8576902534424));
#172729=CARTESIAN_POINT('',(50.6762142289952,36.4252947698673,39.2875012672119));
#172730=CARTESIAN_POINT('',(50.9644637245897,36.6347241449648,39.8576902534424));
#172731=CARTESIAN_POINT('',(53.8880358395974,31.4795232016783,39.2875012672119));
#172732=CARTESIAN_POINT('Origin',(5.53234440788222E-15,0.,39.2875012672119));
#172733=CARTESIAN_POINT('',(54.1966007261211,31.6576696180577,39.8576902534424));
#172734=CARTESIAN_POINT('',(53.8880358395974,31.4795232016783,39.2875012672119));
#172735=CARTESIAN_POINT('',(54.5122556166615,31.4902932482901,40.1599502534424));
#172736=CARTESIAN_POINT('Ctrl Pts',(54.1966007261211,31.6576696180577,39.8576902534424));
#172737=CARTESIAN_POINT('Ctrl Pts',(54.207258044343,31.6638224711873,39.8773836120385));
#172738=CARTESIAN_POINT('Ctrl Pts',(54.2188555266776,31.6682661704395,39.8969946442175));
#172739=CARTESIAN_POINT('Ctrl Pts',(54.231205042325,31.6709833936517,39.9162525288304));
#172740=CARTESIAN_POINT('Ctrl Pts',(54.2438027078816,31.6737552164703,39.9358973794147));
#172741=CARTESIAN_POINT('Ctrl Pts',(54.2571837147368,31.6747309854166,39.9551762199842));
#172742=CARTESIAN_POINT('Ctrl Pts',(54.2711824151134,31.6738510973596,39.9738152034363));
#172743=CARTESIAN_POINT('Ctrl Pts',(54.2846372786704,31.6730053921559,39.9917300792778));
#172744=CARTESIAN_POINT('Ctrl Pts',(54.2986636530789,31.6704454915874,40.0090551158268));
#172745=CARTESIAN_POINT('Ctrl Pts',(54.3131329740999,31.6660771734201,40.0255394551691));
#172746=CARTESIAN_POINT('Ctrl Pts',(54.324247804405,31.6627215829901,40.038202152625));
#172747=CARTESIAN_POINT('Ctrl Pts',(54.3356244578624,31.6582981215803,40.0503687782171));
#172748=CARTESIAN_POINT('Ctrl Pts',(54.3472079546998,31.6527458376961,40.0619155352442));
#172749=CARTESIAN_POINT('Ctrl Pts',(54.3472383129792,31.6527312861502,40.0619457972351));
#172750=CARTESIAN_POINT('Ctrl Pts',(54.3472686729572,31.6527167260607,40.0619760547305));
#172751=CARTESIAN_POINT('Ctrl Pts',(54.3472990346308,31.6527021574288,40.0620063077269));
#172752=CARTESIAN_POINT('Ctrl Pts',(54.3505544234704,31.6511401038181,40.06525004417));
#172753=CARTESIAN_POINT('Ctrl Pts',(54.3538274103387,31.649479697007,40.0684393223556));
#172754=CARTESIAN_POINT('Ctrl Pts',(54.3571135597836,31.6477231007673,40.0715697951759));
#172755=CARTESIAN_POINT('Ctrl Pts',(54.3754002342679,31.6379480420934,40.0889901646403));
#172756=CARTESIAN_POINT('Ctrl Pts',(54.3940968201743,31.6251987170252,40.1045963098211));
#172757=CARTESIAN_POINT('Ctrl Pts',(54.4124255228499,31.6099016141405,40.1176634650686));
#172758=CARTESIAN_POINT('Ctrl Pts',(54.4206516984354,31.6030360625242,40.1235281853038));
#172759=CARTESIAN_POINT('Ctrl Pts',(54.4288041214155,31.595657388408,40.1288820140909));
#172760=CARTESIAN_POINT('Ctrl Pts',(54.436814691924,31.5878037911375,40.1336621774101));
#172761=CARTESIAN_POINT('Ctrl Pts',(54.4402959775156,31.5843907239919,40.1357395717319));
#172762=CARTESIAN_POINT('Ctrl Pts',(54.4437502703992,31.5808879923394,40.1377083672884));
#172763=CARTESIAN_POINT('Ctrl Pts',(54.4471718528276,31.5772987574361,40.1395632548792));
#172764=CARTESIAN_POINT('Ctrl Pts',(54.4591473913267,31.5647364352747,40.146055361447));
#172765=CARTESIAN_POINT('Ctrl Pts',(54.4707222239585,31.5511144466735,40.151152097463));
#172766=CARTESIAN_POINT('Ctrl Pts',(54.4816512176788,31.5365683393819,40.1546258197409));
#172767=CARTESIAN_POINT('Ctrl Pts',(54.487115714539,31.5292952857361,40.1563626808798));
#172768=CARTESIAN_POINT('Ctrl Pts',(54.4924187521967,31.5217912027238,40.1576937882008));
#172769=CARTESIAN_POINT('Ctrl Pts',(54.4975296958776,31.5140730377798,40.1585906813668));
#172770=CARTESIAN_POINT('Ctrl Pts',(54.5000851677181,31.5102139553077,40.1590391279498));
#172771=CARTESIAN_POINT('Ctrl Pts',(54.5025926161711,31.5063013524143,40.1593790209175));
#172772=CARTESIAN_POINT('Ctrl Pts',(54.5050482124964,31.5023373478773,40.1596068022931));
#172773=CARTESIAN_POINT('Ctrl Pts',(54.5075038088218,31.4983733433402,40.1598345836687));
#172774=CARTESIAN_POINT('Ctrl Pts',(54.5099075515421,31.494357936306,40.1599502506865));
#172775=CARTESIAN_POINT('Ctrl Pts',(54.5122556166615,31.4902932482901,40.1599502534424));
#172776=CARTESIAN_POINT('',(54.5275217339723,31.4638515574734,40.1599502534424));
#172777=CARTESIAN_POINT('Origin',(5.52060867199534E-15,5.61717825899799E-15,
40.1599502534424));
#172778=CARTESIAN_POINT('',(54.5146464769142,31.1067982185528,39.8576902534424));
#172779=CARTESIAN_POINT('Ctrl Pts',(54.5275217339724,31.4638515574734,40.1599502534424));
#172780=CARTESIAN_POINT('Ctrl Pts',(54.5294317356861,31.4605414731913,40.1599502447858));
#172781=CARTESIAN_POINT('Ctrl Pts',(54.5312951627231,31.4572166015115,40.1598744685927));
#172782=CARTESIAN_POINT('Ctrl Pts',(54.5331120223763,31.4538791743426,40.1597246934279));
#172783=CARTESIAN_POINT('Ctrl Pts',(54.543611229832,31.4345929624707,40.1588591777434));
#172784=CARTESIAN_POINT('Ctrl Pts',(54.5525583311783,31.4148859438253,40.1555254706018));
#172785=CARTESIAN_POINT('Ctrl Pts',(54.5599504658514,31.3951944477263,40.1500631826375));
#172786=CARTESIAN_POINT('Ctrl Pts',(54.5629318838128,31.3872524143687,40.1478601162477));
#172787=CARTESIAN_POINT('Ctrl Pts',(54.565660781029,31.3793127123316,40.1453112228304));
#172788=CARTESIAN_POINT('Ctrl Pts',(54.5681385507011,31.3714030065912,40.1424401896328));
#172789=CARTESIAN_POINT('Ctrl Pts',(54.5690526972785,31.3684848053912,40.1413809526905));
#172790=CARTESIAN_POINT('Ctrl Pts',(54.5699325468794,31.36557075653,40.1402777640511));
#172791=CARTESIAN_POINT('Ctrl Pts',(54.5707781137758,31.3626622846446,40.1391317641987));
#172792=CARTESIAN_POINT('Ctrl Pts',(54.5723635517066,31.3572088998593,40.1369830144753));
#172793=CARTESIAN_POINT('Ctrl Pts',(54.5738284644995,31.3517751216263,40.1346837565849));
#172794=CARTESIAN_POINT('Ctrl Pts',(54.5751729463232,31.3463703409149,40.1322415082996));
#172795=CARTESIAN_POINT('Ctrl Pts',(54.5798786327064,31.3274536084253,40.1236936393008));
#172796=CARTESIAN_POINT('Ctrl Pts',(54.5831090358351,31.3088920933395,40.113394140767));
#172797=CARTESIAN_POINT('Ctrl Pts',(54.5848682151126,31.2910884461618,40.101665321223));
#172798=CARTESIAN_POINT('Ctrl Pts',(54.5857478047514,31.282186622573,40.095800911451));
#172799=CARTESIAN_POINT('Ctrl Pts',(54.5862595893022,31.2734742664665,40.0895791707949));
#172800=CARTESIAN_POINT('Ctrl Pts',(54.5864040839111,31.265001713557,40.0830403822906));
#172801=CARTESIAN_POINT('Ctrl Pts',(54.5864763312156,31.2607654371022,40.0797709880385));
#172802=CARTESIAN_POINT('Ctrl Pts',(54.5864567561368,31.2565891115046,40.0764223317514));
#172803=CARTESIAN_POINT('Ctrl Pts',(54.5863454235316,31.2524790289897,40.0729994484778));
#172804=CARTESIAN_POINT('Ctrl Pts',(54.5862340909265,31.2483689464747,40.0695765652042));
#172805=CARTESIAN_POINT('Ctrl Pts',(54.5860308973893,31.2443251851214,40.0660793733488));
#172806=CARTESIAN_POINT('Ctrl Pts',(54.5857361203751,31.2403538784528,40.0625130768817));
#172807=CARTESIAN_POINT('Ctrl Pts',(54.5857336065446,31.2403200115241,40.0624826638418));
#172808=CARTESIAN_POINT('Ctrl Pts',(54.5857310861515,31.2402861499639,40.0624522459912));
#172809=CARTESIAN_POINT('Ctrl Pts',(54.5857285591964,31.2402522937754,40.0624218233329));
#172810=CARTESIAN_POINT('Ctrl Pts',(54.5844380063443,31.2229614439847,40.0468845275895));
#172811=CARTESIAN_POINT('Ctrl Pts',(54.5815601021618,31.207026622759,40.030226332923));
#172812=CARTESIAN_POINT('Ctrl Pts',(54.5772898993838,31.1924939094102,40.0127515884733));
#172813=CARTESIAN_POINT('Ctrl Pts',(54.5728752811835,31.1774697093461,39.9946858597698));
#172814=CARTESIAN_POINT('Ctrl Pts',(54.566971991737,31.1639433968874,39.9757460620467));
#172815=CARTESIAN_POINT('Ctrl Pts',(54.5597576364798,31.1520017942437,39.9562444559099));
#172816=CARTESIAN_POINT('Ctrl Pts',(54.5526805134402,31.14028734601,39.9371138113575));
#172817=CARTESIAN_POINT('Ctrl Pts',(54.544340874094,31.130097527724,39.9174410654309));
#172818=CARTESIAN_POINT('Ctrl Pts',(54.5348819367177,31.1215554575377,39.8975196504094));
#172819=CARTESIAN_POINT('Ctrl Pts',(54.5286157223228,31.1158966355121,39.884322411374));
#172820=CARTESIAN_POINT('Ctrl Pts',(54.5218578148477,31.1109617866602,39.8710160447114));
#172821=CARTESIAN_POINT('Ctrl Pts',(54.5146464769142,31.1067982185528,39.8576902534424));
#172822=CARTESIAN_POINT('',(54.2060847114746,30.9286463962971,39.2875012672119));
#172823=CARTESIAN_POINT('',(54.5146464769142,31.1067982185528,39.8576902534424));
#172824=CARTESIAN_POINT('',(56.8833377255397,25.6742415049973,39.2875012672119));
#172825=CARTESIAN_POINT('Origin',(5.53234440788222E-15,0.,39.2875012672119));
#172826=CARTESIAN_POINT('',(57.2088336324702,25.8191582032614,39.8576902534424));
#172827=CARTESIAN_POINT('',(56.8833377255398,25.6742415049973,39.2875012672119));
#172828=CARTESIAN_POINT('',(57.5052637377735,25.6197038181291,40.1599502534424));
#172829=CARTESIAN_POINT('Ctrl Pts',(57.2088336324702,25.8191582032614,39.8576902534424));
#172830=CARTESIAN_POINT('Ctrl Pts',(57.2200757170675,25.8241633573202,39.8773836120341));
#172831=CARTESIAN_POINT('Ctrl Pts',(57.2320741602317,25.8273704465163,39.8969946442086));
#172832=CARTESIAN_POINT('Ctrl Pts',(57.2446400511038,25.8287819086031,39.9162525288172));
#172833=CARTESIAN_POINT('Ctrl Pts',(57.2574584397068,25.8302217324653,39.935897379397));
#172834=CARTESIAN_POINT('Ctrl Pts',(57.2708681396313,25.8297934599651,39.9551762199623));
#172835=CARTESIAN_POINT('Ctrl Pts',(57.2846981803123,25.8274551293912,39.9738152034104));
#172836=CARTESIAN_POINT('Ctrl Pts',(57.29799093645,25.8252076408403,39.9917300792482));
#172837=CARTESIAN_POINT('Ctrl Pts',(57.3116728904355,25.821195608316,40.0090551157937));
#172838=CARTESIAN_POINT('Ctrl Pts',(57.3256063334131,25.8153387643661,40.0255394551332));
#172839=CARTESIAN_POINT('Ctrl Pts',(57.3363095208137,25.8108397400781,40.0382021526019));
#172840=CARTESIAN_POINT('Ctrl Pts',(57.3471614741597,25.8052513267456,40.0503687782061));
#172841=CARTESIAN_POINT('Ctrl Pts',(57.3581011436977,25.7985186537234,40.0619155352442));
#172842=CARTESIAN_POINT('Ctrl Pts',(57.3581298146206,25.7985010085881,40.0619457972351));
#172843=CARTESIAN_POINT('Ctrl Pts',(57.3581584863397,25.7984833547784,40.0619760547304));
#172844=CARTESIAN_POINT('Ctrl Pts',(57.3581871588522,25.7984656922959,40.0620063077269));
#172845=CARTESIAN_POINT('Ctrl Pts',(57.3612614352676,25.7965719149857,40.06525004417));
#172846=CARTESIAN_POINT('Ctrl Pts',(57.364342932599,25.7945784837691,40.0684393223556));
#172847=CARTESIAN_POINT('Ctrl Pts',(57.3674274658679,25.7924880141959,40.0715697951759));
#172848=CARTESIAN_POINT('Ctrl Pts',(57.3845921921748,25.7808550263338,40.0889901646407));
#172849=CARTESIAN_POINT('Ctrl Pts',(57.4018536888708,25.7662212180087,40.104596309822));
#172850=CARTESIAN_POINT('Ctrl Pts',(57.4184830023389,25.7490920431292,40.1176634650696));
#172851=CARTESIAN_POINT('Ctrl Pts',(57.4259464685134,25.7414042322309,40.1235281853045));
#172852=CARTESIAN_POINT('Ctrl Pts',(57.4332829502005,25.733213819018,40.1288820140912));
#172853=CARTESIAN_POINT('Ctrl Pts',(57.4404287135114,25.7245659119504,40.1336621774101));
#172854=CARTESIAN_POINT('Ctrl Pts',(57.4435341655926,25.7208076485107,40.1357395717319));
#172855=CARTESIAN_POINT('Ctrl Pts',(57.4466034003415,25.7169630332619,40.1377083672884));
#172856=CARTESIAN_POINT('Ctrl Pts',(57.4496310617745,25.7130358078098,40.1395632548792));
#172857=CARTESIAN_POINT('Ctrl Pts',(57.4602278767901,25.6992905187274,40.146055361447));
#172858=CARTESIAN_POINT('Ctrl Pts',(57.4703154157425,25.6845332533375,40.1511520974629));
#172859=CARTESIAN_POINT('Ctrl Pts',(57.4796640570501,25.668924440225,40.1546258197408));
#172860=CARTESIAN_POINT('Ctrl Pts',(57.4843383777038,25.6611200336687,40.1563626808798));
#172861=CARTESIAN_POINT('Ctrl Pts',(57.4888279745008,25.6531027404313,40.1576937882008));
#172862=CARTESIAN_POINT('Ctrl Pts',(57.4931041519767,25.6448926173136,40.1585906813668));
#172863=CARTESIAN_POINT('Ctrl Pts',(57.4952422407146,25.6407875557547,40.1590391279498));
#172864=CARTESIAN_POINT('Ctrl Pts',(57.4973269747348,25.6366342867758,40.1593790209175));
#172865=CARTESIAN_POINT('Ctrl Pts',(57.4993547677439,25.63243531776,40.1596068022931));
#172866=CARTESIAN_POINT('Ctrl Pts',(57.501382560753,25.6282363487443,40.1598345836687));
#172867=CARTESIAN_POINT('Ctrl Pts',(57.5033534111924,25.6239916789973,40.1599502506864));
#172868=CARTESIAN_POINT('Ctrl Pts',(57.5052637377735,25.6197038181291,40.1599502534424));
#172869=CARTESIAN_POINT('',(57.5176823163891,25.5918112338787,40.1599502534424));
#172870=CARTESIAN_POINT('Origin',(5.5132234544654E-15,5.63167256450768E-15,
40.1599502534424));
#172871=CARTESIAN_POINT('',(57.4675553545144,25.2380597013423,39.8576902534424));
#172872=CARTESIAN_POINT('Ctrl Pts',(57.5176823163891,25.5918112338787,40.1599502534424));
#172873=CARTESIAN_POINT('Ctrl Pts',(57.5192358568904,25.5883196330407,40.1599502447858));
#172874=CARTESIAN_POINT('Ctrl Pts',(57.5207415321518,25.5848181941912,40.1598744685927));
#172875=CARTESIAN_POINT('Ctrl Pts',(57.5221995827245,25.5813091362501,40.1597246934279));
#172876=CARTESIAN_POINT('Ctrl Pts',(57.530625316332,25.5610311102486,40.1588591777436));
#172877=CARTESIAN_POINT('Ctrl Pts',(57.5374634601452,25.5404968219637,40.1555254706034));
#172878=CARTESIAN_POINT('Ctrl Pts',(57.5427567781039,25.5201405094677,40.1500631826413));
#172879=CARTESIAN_POINT('Ctrl Pts',(57.5448916950053,25.5119303403572,40.1478601162506));
#172880=CARTESIAN_POINT('Ctrl Pts',(57.5467757181854,25.5037488854015,40.1453112228321));
#172881=CARTESIAN_POINT('Ctrl Pts',(57.548413124991,25.4956235123959,40.1424401896328));
#172882=CARTESIAN_POINT('Ctrl Pts',(57.5490172286909,25.4926257430704,40.1413809526905));
#172883=CARTESIAN_POINT('Ctrl Pts',(57.5495876573342,25.4896356883471,40.1402777640512));
#172884=CARTESIAN_POINT('Ctrl Pts',(57.5501245740301,25.4866547635667,40.1391317641987));
#172885=CARTESIAN_POINT('Ctrl Pts',(57.5511312928348,25.4810655296034,40.1369830144753));
#172886=CARTESIAN_POINT('Ctrl Pts',(57.5520201961937,25.475508393093,40.1346837565849));
#172887=CARTESIAN_POINT('Ctrl Pts',(57.5527923593833,25.469992683717,40.1322415082996));
#172888=CARTESIAN_POINT('Ctrl Pts',(57.5554949305468,25.450687700901,40.1236936393008));
#172889=CARTESIAN_POINT('Ctrl Pts',(57.5567674305414,25.4318901986622,40.113394140767));
#172890=CARTESIAN_POINT('Ctrl Pts',(57.5566559849708,25.41400019742,40.101665321223));
#172891=CARTESIAN_POINT('Ctrl Pts',(57.5566002621854,25.405055196799,40.095800911451));
#172892=CARTESIAN_POINT('Ctrl Pts',(57.5561985539316,25.3963370718382,40.0895791707949));
#172893=CARTESIAN_POINT('Ctrl Pts',(57.5554566340484,25.3878958286606,40.0830403822906));
#172894=CARTESIAN_POINT('Ctrl Pts',(57.5550856741068,25.3836752070718,40.0797709880385));
#172895=CARTESIAN_POINT('Ctrl Pts',(57.5546296613655,25.3795238059757,40.0764223317514));
#172896=CARTESIAN_POINT('Ctrl Pts',(57.5540893180428,25.3754478763489,40.0729994484778));
#172897=CARTESIAN_POINT('Ctrl Pts',(57.5535489747201,25.3713719467222,40.0695765652042));
#172898=CARTESIAN_POINT('Ctrl Pts',(57.5529242061383,25.3673715770249,40.0660793733488));
#172899=CARTESIAN_POINT('Ctrl Pts',(57.5522159293602,25.363452838178,40.0625130768817));
#172900=CARTESIAN_POINT('Ctrl Pts',(57.5522098892427,25.3634194195428,40.0624826638418));
#172901=CARTESIAN_POINT('Ctrl Pts',(57.5522038431597,25.3633860069326,40.0624522459912));
#172902=CARTESIAN_POINT('Ctrl Pts',(57.5521977911122,25.3633526003505,40.0624218233329));
#172903=CARTESIAN_POINT('Ctrl Pts',(57.549106922086,25.3462913711479,40.0468845275872));
#172904=CARTESIAN_POINT('Ctrl Pts',(57.5445791409876,25.3307446654397,40.030226332918));
#172905=CARTESIAN_POINT('Ctrl Pts',(57.5388132486326,25.3167379215479,40.0127515884654));
#172906=CARTESIAN_POINT('Ctrl Pts',(57.5328523576269,25.3022574788784,39.994685859759));
#172907=CARTESIAN_POINT('Ctrl Pts',(57.525567522361,25.2894223267475,39.9757460620327));
#172908=CARTESIAN_POINT('Ctrl Pts',(57.5171444507216,25.2783002469205,39.9562444558927));
#172909=CARTESIAN_POINT('Ctrl Pts',(57.5088816036288,25.2673897324551,39.9371138113373));
#172910=CARTESIAN_POINT('Ctrl Pts',(57.499522523651,25.258127464745,39.9174410654078));
#172911=CARTESIAN_POINT('Ctrl Pts',(57.4892225138515,25.2506209171015,39.8975196503834));
#172912=CARTESIAN_POINT('Ctrl Pts',(57.4823991184684,25.2456480924605,39.8843224113565));
#172913=CARTESIAN_POINT('Ctrl Pts',(57.4751623993551,25.2414466709135,39.8710160447026));
#172914=CARTESIAN_POINT('Ctrl Pts',(57.4675553545144,25.2380597013423,39.8576902534424));
#172915=CARTESIAN_POINT('',(57.1420619865024,25.0931373005739,39.2875012672119));
#172916=CARTESIAN_POINT('',(57.4675553545144,25.2380597013423,39.8576902534424));
#172917=CARTESIAN_POINT('',(59.2554138597574,19.5876674457071,39.2875012672119));
#172918=CARTESIAN_POINT('Origin',(5.53234440788222E-15,0.,39.2875012672119));
#172919=CARTESIAN_POINT('',(59.5942745858238,19.6977666881838,39.8576902534424));
#172920=CARTESIAN_POINT('',(59.2554138597574,19.5876674457071,39.2875012672119));
#172921=CARTESIAN_POINT('',(59.8682321556244,19.4684195516689,40.1599502534424));
#172922=CARTESIAN_POINT('Ctrl Pts',(59.5942745858238,19.6977666881838,39.8576902534424));
#172923=CARTESIAN_POINT('Ctrl Pts',(59.6059782661682,19.7015693056585,39.877383612035));
#172924=CARTESIAN_POINT('Ctrl Pts',(59.618246212711,19.7035046472589,39.8969946442105));
#172925=CARTESIAN_POINT('Ctrl Pts',(59.6308908042817,19.7035948839462,39.91625252882));
#172926=CARTESIAN_POINT('Ctrl Pts',(59.6437894749872,19.7036869338402,39.9358973794009));
#172927=CARTESIAN_POINT('Ctrl Pts',(59.657080948507,19.7018593121352,39.9551762199673));
#172928=CARTESIAN_POINT('Ctrl Pts',(59.6705908046774,19.6980881582808,39.9738152034164));
#172929=CARTESIAN_POINT('Ctrl Pts',(59.6835758151828,19.6944635103349,39.9917300792554));
#172930=CARTESIAN_POINT('Ctrl Pts',(59.6967634463995,19.689043302519,40.009055115802));
#172931=CARTESIAN_POINT('Ctrl Pts',(59.710008353622,19.6817621015893,40.0255394551424));
#172932=CARTESIAN_POINT('Ctrl Pts',(59.7201826317446,19.6761689356968,40.0382021526078));
#172933=CARTESIAN_POINT('Ctrl Pts',(59.7303909886945,19.6694767982719,40.0503687782089));
#172934=CARTESIAN_POINT('Ctrl Pts',(59.740566973611,19.6616375006933,40.0619155352442));
#172935=CARTESIAN_POINT('Ctrl Pts',(59.7405936430527,19.6616169552925,40.0619457972351));
#172936=CARTESIAN_POINT('Ctrl Pts',(59.7406203123795,19.6615964011814,40.0619760547304));
#172937=CARTESIAN_POINT('Ctrl Pts',(59.7406469815888,19.6615758383622,40.0620063077269));
#172938=CARTESIAN_POINT('Ctrl Pts',(59.7435064631644,19.6593710859728,40.06525004417));
#172939=CARTESIAN_POINT('Ctrl Pts',(59.7463627094293,19.6570664708005,40.0684393223556));
#172940=CARTESIAN_POINT('Ctrl Pts',(59.7492118317302,19.6546650315158,40.0715697951759));
#172941=CARTESIAN_POINT('Ctrl Pts',(59.7650665495264,19.6413015679147,40.0889901646412));
#172942=CARTESIAN_POINT('Ctrl Pts',(59.7807038364419,19.6249436073989,40.1045963098228));
#172943=CARTESIAN_POINT('Ctrl Pts',(59.795451566464,19.606170031349,40.1176634650707));
#172944=CARTESIAN_POINT('Ctrl Pts',(59.8020705519303,19.5977441904338,40.1235281853051));
#172945=CARTESIAN_POINT('Ctrl Pts',(59.8085107122961,19.5888317740054,40.1288820140915));
#172946=CARTESIAN_POINT('Ctrl Pts',(59.8147133779312,19.5794843054205,40.1336621774101));
#172947=CARTESIAN_POINT('Ctrl Pts',(59.817408972519,19.5754220220073,40.1357395717319));
#172948=CARTESIAN_POINT('Ctrl Pts',(59.820059521955,19.5712776455713,40.1377083672884));
#172949=CARTESIAN_POINT('Ctrl Pts',(59.8226600907005,19.5670554570743,40.1395632548792));
#172950=CARTESIAN_POINT('Ctrl Pts',(59.8317620813098,19.5522777973346,40.146055361447));
#172951=CARTESIAN_POINT('Ctrl Pts',(59.8402518053951,19.5365469388437,40.1511520974629));
#172952=CARTESIAN_POINT('Ctrl Pts',(59.8479176686193,19.5200464333331,40.1546258197408));
#172953=CARTESIAN_POINT('Ctrl Pts',(59.8517506002314,19.5117961805777,40.1563626808798));
#172954=CARTESIAN_POINT('Ctrl Pts',(59.8553775672057,19.5033535162577,40.1576937882008));
#172955=CARTESIAN_POINT('Ctrl Pts',(59.8587721277812,19.4947413867932,40.1585906813668));
#172956=CARTESIAN_POINT('Ctrl Pts',(59.8604694080689,19.490435322061,40.1590391279498));
#172957=CARTESIAN_POINT('Ctrl Pts',(59.8621085868741,19.4860868910807,40.1593790209175));
#172958=CARTESIAN_POINT('Ctrl Pts',(59.8636863596424,19.4816989623695,40.1596068022931));
#172959=CARTESIAN_POINT('Ctrl Pts',(59.8652641324107,19.4773110336582,40.1598345836686));
#172960=CARTESIAN_POINT('Ctrl Pts',(59.8667804975195,19.4728836066885,40.1599502506864));
#172961=CARTESIAN_POINT('Ctrl Pts',(59.8682321556244,19.4684195516689,40.1599502534424));
#172962=CARTESIAN_POINT('',(59.8776671349988,19.4393816709748,40.1599502534424));
#172963=CARTESIAN_POINT('Origin',(5.50739376141089E-15,5.64685943413453E-15,
40.1599502534424));
#172964=CARTESIAN_POINT('',(59.7908376697914,19.0928077206404,39.8576902534424));
#172965=CARTESIAN_POINT('Ctrl Pts',(59.8776671349988,19.4393816709748,40.1599502534424));
#172966=CARTESIAN_POINT('Ctrl Pts',(59.8788471933727,19.4357468082904,40.1599502447858));
#172967=CARTESIAN_POINT('Ctrl Pts',(59.8799786203653,19.432107164768,40.1598744685927));
#172968=CARTESIAN_POINT('Ctrl Pts',(59.8810618871504,19.4284649220277,40.1597246934279));
#172969=CARTESIAN_POINT('Ctrl Pts',(59.8873218328124,19.4074172521853,40.1588591777435));
#172970=CARTESIAN_POINT('Ctrl Pts',(59.8919760989601,19.3862806722125,40.1555254706023));
#172971=CARTESIAN_POINT('Ctrl Pts',(59.8951126055062,19.3654825713314,40.1500631826388));
#172972=CARTESIAN_POINT('Ctrl Pts',(59.8963776307484,19.3570942188066,40.1478601162487));
#172973=CARTESIAN_POINT('Ctrl Pts',(59.8973961381381,19.3487606486725,40.1453112228309));
#172974=CARTESIAN_POINT('Ctrl Pts',(59.8981752423039,19.3405086316964,40.1424401896328));
#172975=CARTESIAN_POINT('Ctrl Pts',(59.8984626844396,19.3374641384336,40.1413809526905));
#172976=CARTESIAN_POINT('Ctrl Pts',(59.8987174423899,19.3344308375134,40.1402777640511));
#172977=CARTESIAN_POINT('Ctrl Pts',(59.8989398263135,19.3314101194737,40.1391317641986));
#172978=CARTESIAN_POINT('Ctrl Pts',(59.8993567961703,19.3257462731493,40.1369830144753));
#172979=CARTESIAN_POINT('Ctrl Pts',(59.8996599510839,19.320126663512,40.1346837565849));
#172980=CARTESIAN_POINT('Ctrl Pts',(59.8998513356578,19.3145604567375,40.1322415082996));
#172981=CARTESIAN_POINT('Ctrl Pts',(59.9005211816666,19.2950787330267,40.1236936393008));
#172982=CARTESIAN_POINT('Ctrl Pts',(59.8998218367508,19.276251193003,40.113394140767));
#172983=CARTESIAN_POINT('Ctrl Pts',(59.8978409873529,19.2584708442938,40.101665321223));
#172984=CARTESIAN_POINT('Ctrl Pts',(59.896850562654,19.2495806699392,40.095800911451));
#172985=CARTESIAN_POINT('Ctrl Pts',(59.8955397627954,19.2409522937256,40.0895791707949));
#172986=CARTESIAN_POINT('Ctrl Pts',(59.8939195570494,19.2326348443066,40.0830403822906));
#172987=CARTESIAN_POINT('Ctrl Pts',(59.8931094541765,19.2284761195972,40.0797709880385));
#172988=CARTESIAN_POINT('Ctrl Pts',(59.8922219999437,19.2243951266217,40.0764223317514));
#172989=CARTESIAN_POINT('Ctrl Pts',(59.891258566018,19.2203980066211,40.0729994484778));
#172990=CARTESIAN_POINT('Ctrl Pts',(59.8902951320923,19.2164008866205,40.0695765652042));
#172991=CARTESIAN_POINT('Ctrl Pts',(59.8892556335612,19.2124877374667,40.0660793733488));
#172992=CARTESIAN_POINT('Ctrl Pts',(59.8881416170478,19.2086645009644,40.0625130768817));
#172993=CARTESIAN_POINT('Ctrl Pts',(59.8881321168201,19.2086318967641,40.0624826638418));
#172994=CARTESIAN_POINT('Ctrl Pts',(59.8881226112894,19.2085992991795,40.0624522459912));
#172995=CARTESIAN_POINT('Ctrl Pts',(59.888113100457,19.2085667082134,40.0624218233329));
#172996=CARTESIAN_POINT('Ctrl Pts',(59.883255779466,19.1919220260038,40.0468845275916));
#172997=CARTESIAN_POINT('Ctrl Pts',(59.8771277287718,19.1769337687802,40.0302263329276));
#172998=CARTESIAN_POINT('Ctrl Pts',(59.8699293191667,19.1636064551671,40.0127515884804));
#172999=CARTESIAN_POINT('Ctrl Pts',(59.8624874641286,19.1498284206571,39.9946858597795));
#173000=CARTESIAN_POINT('Ctrl Pts',(59.8539008972278,19.1378250534699,39.9757460620591));
#173001=CARTESIAN_POINT('Ctrl Pts',(59.8443613941471,19.1276443522951,39.9562444559251));
#173002=CARTESIAN_POINT('Ctrl Pts',(59.8350033524881,19.1176573094789,39.937113811375));
#173003=CARTESIAN_POINT('Ctrl Pts',(59.8247273719232,19.1094240716875,39.9174410654508));
#173004=CARTESIAN_POINT('Ctrl Pts',(59.8136991387694,19.103035289892,39.8975196504315));
#173005=CARTESIAN_POINT('Ctrl Pts',(59.8063933209342,19.0988029459312,39.8843224113889));
#173006=CARTESIAN_POINT('Ctrl Pts',(59.7987570771787,19.0953809833338,39.8710160447189));
#173007=CARTESIAN_POINT('Ctrl Pts',(59.7908376697914,19.0928077206404,39.8576902534424));
#173008=CARTESIAN_POINT('',(59.451978872661,18.9827025415089,39.2875012672119));
#173009=CARTESIAN_POINT('',(59.7908376697914,19.0928077206404,39.8576902534424));
#173010=CARTESIAN_POINT('',(60.978275279735,13.2864868028988,39.2875012672119));
#173011=CARTESIAN_POINT('Origin',(5.53234440788222E-15,0.,39.2875012672119));
#173012=CARTESIAN_POINT('',(61.3267881959115,13.3605623192479,39.8576902534424));
#173013=CARTESIAN_POINT('',(60.978275279735,13.2864868028988,39.2875012672119));
#173014=CARTESIAN_POINT('',(61.5752716937453,13.103835206572,40.1599502534424));
#173015=CARTESIAN_POINT('Ctrl Pts',(61.3267881959115,13.3605623192479,39.8576902534424));
#173016=CARTESIAN_POINT('Ctrl Pts',(61.3388252440299,13.3631207378648,39.8773836120328));
#173017=CARTESIAN_POINT('Ctrl Pts',(61.35122828376,13.363763127862,39.896994644206));
#173018=CARTESIAN_POINT('Ctrl Pts',(61.3638130392359,13.3625311504982,39.9162525288135));
#173019=CARTESIAN_POINT('Ctrl Pts',(61.376650671506,13.3612744179069,39.9358973793921));
#173020=CARTESIAN_POINT('Ctrl Pts',(61.3896782944532,13.3580674708042,39.9551762199564));
#173021=CARTESIAN_POINT('Ctrl Pts',(61.4027199492994,13.3529048112222,39.9738152034036));
#173022=CARTESIAN_POINT('Ctrl Pts',(61.4152549476772,13.347942716285,39.9917300792404));
#173023=CARTESIAN_POINT('Ctrl Pts',(61.427803769675,13.3411737181114,40.0090551157852));
#173024=CARTESIAN_POINT('Ctrl Pts',(61.4402150271644,13.3325479345667,40.025539455124));
#173025=CARTESIAN_POINT('Ctrl Pts',(61.4497489244961,13.3259219069631,40.0382021525961));
#173026=CARTESIAN_POINT('Ctrl Pts',(61.4592018401621,13.3181993658996,40.0503687782034));
#173027=CARTESIAN_POINT('Ctrl Pts',(61.468502650244,13.3093393327436,40.0619155352442));
#173028=CARTESIAN_POINT('Ctrl Pts',(61.4685270260085,13.3093161121768,40.0619457972351));
#173029=CARTESIAN_POINT('Ctrl Pts',(61.4685514007484,13.3092928829596,40.0619760547305));
#173030=CARTESIAN_POINT('Ctrl Pts',(61.468575774461,13.3092696450942,40.0620063077269));
#173031=CARTESIAN_POINT('Ctrl Pts',(61.4711891321182,13.3067780733542,40.06525004417));
#173032=CARTESIAN_POINT('Ctrl Pts',(61.4737888336848,13.3041875240722,40.0684393223556));
#173033=CARTESIAN_POINT('Ctrl Pts',(61.4763713294376,13.3015014257474,40.0715697951759));
#173034=CARTESIAN_POINT('Ctrl Pts',(61.4907423311191,13.2865538993088,40.0889901646442));
#173035=CARTESIAN_POINT('Ctrl Pts',(61.504584082868,13.2686510078378,40.1045963098281));
#173036=CARTESIAN_POINT('Ctrl Pts',(61.5172886502292,13.2484387178417,40.1176634650774));
#173037=CARTESIAN_POINT('Ctrl Pts',(61.5229906359957,13.2393671621885,40.1235281853092));
#173038=CARTESIAN_POINT('Ctrl Pts',(61.5284639152937,13.229830388847,40.1288820140933));
#173039=CARTESIAN_POINT('Ctrl Pts',(61.5336555255489,13.2198857715698,40.1336621774101));
#173040=CARTESIAN_POINT('Ctrl Pts',(61.535911729145,13.2155639754103,40.1357395717319));
#173041=CARTESIAN_POINT('Ctrl Pts',(61.5381145532938,13.2111652444428,40.1377083672884));
#173042=CARTESIAN_POINT('Ctrl Pts',(61.5402595369764,13.2066943520815,40.1395632548792));
#173043=CARTESIAN_POINT('Ctrl Pts',(61.5477669798654,13.1910462288171,40.146055361447));
#173044=CARTESIAN_POINT('Ctrl Pts',(61.5545658738899,13.1745141278027,40.1511520974629));
#173045=CARTESIAN_POINT('Ctrl Pts',(61.5604649702291,13.1573027128853,40.1546258197408));
#173046=CARTESIAN_POINT('Ctrl Pts',(61.5634145183987,13.1486970054266,40.1563626808798));
#173047=CARTESIAN_POINT('Ctrl Pts',(61.5661391177413,13.1399214696209,40.1576937882008));
#173048=CARTESIAN_POINT('Ctrl Pts',(61.5686148699003,13.1310016901023,40.1585906813668));
#173049=CARTESIAN_POINT('Ctrl Pts',(61.5698527459799,13.126541800343,40.1590391279498));
#173050=CARTESIAN_POINT('Ctrl Pts',(61.5710284103841,13.1220458496811,40.1593790209175));
#173051=CARTESIAN_POINT('Ctrl Pts',(61.5721388765029,13.1175170363396,40.1596068022931));
#173052=CARTESIAN_POINT('Ctrl Pts',(61.5732493426218,13.1129882229981,40.1598345836687));
#173053=CARTESIAN_POINT('Ctrl Pts',(61.5742946087865,13.108426546622,40.1599502506865));
#173054=CARTESIAN_POINT('Ctrl Pts',(61.5752716937453,13.103835206572,40.1599502534424));
#173055=CARTESIAN_POINT('',(61.5816197022699,13.0739701745317,40.1599502534424));
#173056=CARTESIAN_POINT('Origin',(5.50318346416883E-15,5.66257247735684E-15,
40.1599502534424));
#173057=CARTESIAN_POINT('',(61.459039055521,12.7383709431243,39.8576902534424));
#173058=CARTESIAN_POINT('Ctrl Pts',(61.5816197022699,13.0739701745317,40.1599502534424));
#173059=CARTESIAN_POINT('Ctrl Pts',(61.58241334955,13.070231874317,40.1599502447858));
#173060=CARTESIAN_POINT('Ctrl Pts',(61.5831581321229,13.0664939028178,40.1598744685927));
#173061=CARTESIAN_POINT('Ctrl Pts',(61.5838547466227,13.0627583804519,40.1597246934279));
#173062=CARTESIAN_POINT('Ctrl Pts',(61.5878803190637,13.041171669446,40.1588591777435));
#173063=CARTESIAN_POINT('Ctrl Pts',(61.5902997144311,13.0196643745808,40.155525470602));
#173064=CARTESIAN_POINT('Ctrl Pts',(61.5912450453421,12.9986523536622,40.150063182638));
#173065=CARTESIAN_POINT('Ctrl Pts',(61.5916263190448,12.9901777222667,40.1478601162481));
#173066=CARTESIAN_POINT('Ctrl Pts',(61.5917681516648,12.9817833412905,40.1453112228306));
#173067=CARTESIAN_POINT('Ctrl Pts',(61.5916804171631,12.9734950911666,40.1424401896328));
#173068=CARTESIAN_POINT('Ctrl Pts',(61.5916480484585,12.9704372300717,40.1413809526905));
#173069=CARTESIAN_POINT('Ctrl Pts',(61.5915843445342,12.9673939164343,40.1402777640511));
#173070=CARTESIAN_POINT('Ctrl Pts',(61.5914897592008,12.9643665007543,40.1391317641987));
#173071=CARTESIAN_POINT('Ctrl Pts',(61.5913124117006,12.9586900963543,40.1369830144753));
#173072=CARTESIAN_POINT('Ctrl Pts',(61.5910264967404,12.9530695832094,40.134683756585));
#173073=CARTESIAN_POINT('Ctrl Pts',(61.5906350058492,12.9475138635626,40.1322415082996));
#173074=CARTESIAN_POINT('Ctrl Pts',(61.5892647877302,12.9280688447987,40.1236936393009));
#173075=CARTESIAN_POINT('Ctrl Pts',(61.5866012600732,12.9094175454586,40.113394140767));
#173076=CARTESIAN_POINT('Ctrl Pts',(61.5827727094486,12.8919416545035,40.101665321223));
#173077=CARTESIAN_POINT('Ctrl Pts',(61.5808584341364,12.8832037090259,40.095800911451));
#173078=CARTESIAN_POINT('Ctrl Pts',(61.5786529040704,12.8747596158549,40.0895791707949));
#173079=CARTESIAN_POINT('Ctrl Pts',(61.576172163775,12.8666570879109,40.0830403822906));
#173080=CARTESIAN_POINT('Ctrl Pts',(61.5749317936273,12.862605823939,40.0797709880385));
#173081=CARTESIAN_POINT('Ctrl Pts',(61.5736226210374,12.8586399512971,40.0764223317514));
#173082=CARTESIAN_POINT('Ctrl Pts',(61.5722466520923,12.8547654342058,40.0729994484778));
#173083=CARTESIAN_POINT('Ctrl Pts',(61.5708706831473,12.8508909171145,40.0695765652042));
#173084=CARTESIAN_POINT('Ctrl Pts',(61.5694278436303,12.8471078617853,40.0660793733488));
#173085=CARTESIAN_POINT('Ctrl Pts',(61.5679202927797,12.8434220158068,40.0625130768817));
#173086=CARTESIAN_POINT('Ctrl Pts',(61.5679074365282,12.8433905832599,40.0624826638418));
#173087=CARTESIAN_POINT('Ctrl Pts',(61.5678945756945,12.8433591578468,40.0624522459912));
#173088=CARTESIAN_POINT('Ctrl Pts',(61.5678817102797,12.8433277395701,40.0624218233329));
#173089=CARTESIAN_POINT('Ctrl Pts',(61.5613111551481,12.8272819669691,40.0468845275908));
#173090=CARTESIAN_POINT('Ctrl Pts',(61.5536499750617,12.813016372708,40.0302263329257));
#173091=CARTESIAN_POINT('Ctrl Pts',(61.5450979154855,12.8005145062067,40.0127515884775));
#173092=CARTESIAN_POINT('Ctrl Pts',(61.5362566309333,12.7875898348819,39.9946858597757));
#173093=CARTESIAN_POINT('Ctrl Pts',(61.5264624086177,12.7765497640387,39.9757460620543));
#173094=CARTESIAN_POINT('Ctrl Pts',(61.5159109908837,12.7674219834074,39.9562444559193));
#173095=CARTESIAN_POINT('Ctrl Pts',(61.5055602833174,12.7584678323706,39.9371138113686));
#173096=CARTESIAN_POINT('Ctrl Pts',(61.4944799879548,12.7513538295746,39.9174410654438));
#173097=CARTESIAN_POINT('Ctrl Pts',(61.4828443590724,12.7461528104588,39.897519650424));
#173098=CARTESIAN_POINT('Ctrl Pts',(61.4751361628629,12.7427073176333,39.8843224113838));
#173099=CARTESIAN_POINT('Ctrl Pts',(61.4671840587594,12.7401023057308,39.8710160447164));
#173100=CARTESIAN_POINT('Ctrl Pts',(61.459039055521,12.7383709431243,39.8576902534424));
#173101=CARTESIAN_POINT('',(61.1105274371643,12.6642893210133,39.2875012672119));
#173102=CARTESIAN_POINT('',(61.459039055521,12.7383709431243,39.8576902534424));
#173103=CARTESIAN_POINT('',(62.0330459552233,6.83973663030176,39.2875012672119));
#173104=CARTESIAN_POINT('Origin',(5.53234440788222E-15,0.,39.2875012672119));
#173105=CARTESIAN_POINT('',(62.3873926810692,6.8769768336648,39.8576902534424));
#173106=CARTESIAN_POINT('',(62.0330459552233,6.83973663030176,39.2875012672119));
#173107=CARTESIAN_POINT('',(62.6076796697355,6.59568250079801,40.1599502534424));
#173108=CARTESIAN_POINT('Ctrl Pts',(62.3873926810692,6.8769768336648,39.8576902534424));
#173109=CARTESIAN_POINT('Ctrl Pts',(62.3996312165469,6.87826302285496,39.8773836120357));
#173110=CARTESIAN_POINT('Ctrl Pts',(62.4120334591686,6.87760542308938,39.8969946442118));
#173111=CARTESIAN_POINT('Ctrl Pts',(62.4244204973384,6.87506472947515,39.9162525288219));
#173112=CARTESIAN_POINT('Ctrl Pts',(62.4370564393911,6.87247298342229,39.9358973794034));
#173113=CARTESIAN_POINT('Ctrl Pts',(62.4496774784062,6.86792184690318,39.9551762199703));
#173114=CARTESIAN_POINT('Ctrl Pts',(62.4621080448317,6.86142424476893,39.97381520342));
#173115=CARTESIAN_POINT('Ctrl Pts',(62.4740556950203,6.85517906858736,39.9917300792593));
#173116=CARTESIAN_POINT('Ctrl Pts',(62.4858282202829,6.8471354426121,40.0090551158062));
#173117=CARTESIAN_POINT('Ctrl Pts',(62.4972698477083,6.83725958233632,40.0255394551469));
#173118=CARTESIAN_POINT('Ctrl Pts',(62.5060589088643,6.82967328917143,40.0382021526107));
#173119=CARTESIAN_POINT('Ctrl Pts',(62.514652815114,6.82100495425239,40.0503687782103));
#173120=CARTESIAN_POINT('Ctrl Pts',(62.5229765487298,6.81122125790595,40.0619155352442));
#173121=CARTESIAN_POINT('Ctrl Pts',(62.5229983637512,6.81119561658265,40.0619457972351));
#173122=CARTESIAN_POINT('Ctrl Pts',(62.5230201768493,6.81116996676345,40.0619760547305));
#173123=CARTESIAN_POINT('Ctrl Pts',(62.5230419880218,6.81114430845071,40.0620063077269));
#173124=CARTESIAN_POINT('Ctrl Pts',(62.5253805892672,6.80839321554162,40.06525004417));
#173125=CARTESIAN_POINT('Ctrl Pts',(62.5276952632612,6.80554511474983,40.0684393223556));
#173126=CARTESIAN_POINT('Ctrl Pts',(62.5299828381019,6.80260378684031,40.0715697951759));
#173127=CARTESIAN_POINT('Ctrl Pts',(62.5427126719621,6.78623596579693,40.0889901646412));
#173128=CARTESIAN_POINT('Ctrl Pts',(62.5546072354113,6.76698429120314,40.1045963098228));
#173129=CARTESIAN_POINT('Ctrl Pts',(62.5651294462094,6.74555473734808,40.1176634650707));
#173130=CARTESIAN_POINT('Ctrl Pts',(62.5698519601314,6.7359368568129,40.1235281853051));
#173131=CARTESIAN_POINT('Ctrl Pts',(62.5742983919726,6.72588021343593,40.1288820140915));
#173132=CARTESIAN_POINT('Ctrl Pts',(62.5784220664835,6.71544740276686,40.1336621774101));
#173133=CARTESIAN_POINT('Ctrl Pts',(62.5802141596491,6.71091344436422,40.1357395717319));
#173134=CARTESIAN_POINT('Ctrl Pts',(62.5819451239083,6.70630855228205,40.1377083672884));
#173135=CARTESIAN_POINT('Ctrl Pts',(62.5836110216379,6.70163794008886,40.1395632548791));
#173136=CARTESIAN_POINT('Ctrl Pts',(62.5894416636914,6.68529079741268,40.1460553614469));
#173137=CARTESIAN_POINT('Ctrl Pts',(62.5944752375495,6.66813858303315,40.1511520974629));
#173138=CARTESIAN_POINT('Ctrl Pts',(62.5985429352697,6.6504048305725,40.1546258197408));
#173139=CARTESIAN_POINT('Ctrl Pts',(62.6005767841298,6.64153795434218,40.1563626808798));
#173140=CARTESIAN_POINT('Ctrl Pts',(62.6023691645599,6.63252569365755,40.1576937882008));
#173141=CARTESIAN_POINT('Ctrl Pts',(62.6038989834439,6.62339599105584,40.1585906813668));
#173142=CARTESIAN_POINT('Ctrl Pts',(62.6046638928858,6.61883113975498,40.1590391279498));
#173143=CARTESIAN_POINT('Ctrl Pts',(62.6053631620638,6.61423692798771,40.1593790209175));
#173144=CARTESIAN_POINT('Ctrl Pts',(62.6059941550341,6.60961684864265,40.1596068022931));
#173145=CARTESIAN_POINT('Ctrl Pts',(62.6066251480044,6.6049967692976,40.1598345836687));
#173146=CARTESIAN_POINT('Ctrl Pts',(62.6071878630701,6.60035082219605,40.1599502506865));
#173147=CARTESIAN_POINT('Ctrl Pts',(62.6076796697355,6.59568250079801,40.1599502534424));
#173148=CARTESIAN_POINT('',(62.6108711573006,6.56531752495217,40.1599502534424));
#173149=CARTESIAN_POINT('Origin',(5.50063869163689E-15,5.67863953878492E-15,
40.1599502534424));
#173150=CARTESIAN_POINT('',(62.4538823482276,6.24436990787975,39.8576902534424));
#173151=CARTESIAN_POINT('Ctrl Pts',(62.6108711573006,6.56531752495217,40.1599502534424));
#173152=CARTESIAN_POINT('Ctrl Pts',(62.6112696981211,6.56151674480659,40.1599502447858));
#173153=CARTESIAN_POINT('Ctrl Pts',(62.6116196762807,6.55772139932857,40.1598744685927));
#173154=CARTESIAN_POINT('Ctrl Pts',(62.6119220062409,6.55393352450196,40.1597246934279));
#173155=CARTESIAN_POINT('Ctrl Pts',(62.6136691004464,6.53204428085642,40.1588591777434));
#173156=CARTESIAN_POINT('Ctrl Pts',(62.6138271176316,6.51040190952294,40.155525470602));
#173157=CARTESIAN_POINT('Ctrl Pts',(62.6125709156641,6.48940618066597,40.150063182638));
#173158=CARTESIAN_POINT('Ctrl Pts',(62.6120642605131,6.48093812023388,40.147860116248));
#173159=CARTESIAN_POINT('Ctrl Pts',(62.6113278644157,6.47257489900929,40.1453112228306));
#173160=CARTESIAN_POINT('Ctrl Pts',(62.6103742524841,6.46434122353952,40.1424401896328));
#173161=CARTESIAN_POINT('Ctrl Pts',(62.6100224275775,6.46130349717859,40.1413809526906));
#173162=CARTESIAN_POINT('Ctrl Pts',(62.6096409597323,6.45828351400505,40.1402777640512));
#173163=CARTESIAN_POINT('Ctrl Pts',(62.6092304414385,6.45528256968445,40.1391317641987));
#173164=CARTESIAN_POINT('Ctrl Pts',(62.6084607196376,6.44965579908332,40.1369830144753));
#173165=CARTESIAN_POINT('Ctrl Pts',(62.6075888673476,6.44409596194893,40.134683756585));
#173166=CARTESIAN_POINT('Ctrl Pts',(62.6066187902475,6.43861159905687,40.1322415082996));
#173167=CARTESIAN_POINT('Ctrl Pts',(62.6032235203971,6.41941632893468,40.1236936393009));
#173168=CARTESIAN_POINT('Ctrl Pts',(62.5986249921653,6.40114561781669,40.113394140767));
#173169=CARTESIAN_POINT('Ctrl Pts',(62.592990686716,6.38416565413411,40.101665321223));
#173170=CARTESIAN_POINT('Ctrl Pts',(62.5901735339913,6.37567567229282,40.095800911451));
#173171=CARTESIAN_POINT('Ctrl Pts',(62.5870974379669,6.36750837741621,40.0895791707949));
#173172=CARTESIAN_POINT('Ctrl Pts',(62.5837833426318,6.35970954393893,40.0830403822906));
#173173=CARTESIAN_POINT('Ctrl Pts',(62.5821262949643,6.35581012720029,40.0797709880385));
#173174=CARTESIAN_POINT('Ctrl Pts',(62.580409747586,6.35200282582274,40.0764223317514));
#173175=CARTESIAN_POINT('Ctrl Pts',(62.5786363190254,6.34829336166079,40.0729994484778));
#173176=CARTESIAN_POINT('Ctrl Pts',(62.5768628904648,6.34458389749884,40.0695765652042));
#173177=CARTESIAN_POINT('Ctrl Pts',(62.5750325180136,6.34097238393994,40.0660793733488));
#173178=CARTESIAN_POINT('Ctrl Pts',(62.5731479498683,6.33746431138509,40.0625130768817));
#173179=CARTESIAN_POINT('Ctrl Pts',(62.5731318784489,6.33743439487324,40.0624826638418));
#173180=CARTESIAN_POINT('Ctrl Pts',(62.573115803218,6.33740448593497,40.0624522459912));
#173181=CARTESIAN_POINT('Ctrl Pts',(62.5730997241772,6.33737458457292,40.0624218233329));
#173182=CARTESIAN_POINT('Ctrl Pts',(62.5648879232826,6.32210352242476,40.0468845275917));
#173183=CARTESIAN_POINT('Ctrl Pts',(62.5557775512972,6.30871688796365,40.0302263329277));
#173184=CARTESIAN_POINT('Ctrl Pts',(62.5459655399055,6.2971774416409,40.0127515884806));
#173185=CARTESIAN_POINT('Ctrl Pts',(62.535821692804,6.28524773890599,39.99468585978));
#173186=CARTESIAN_POINT('Ctrl Pts',(62.5249271226242,6.27529192173385,39.9757460620598));
#173187=CARTESIAN_POINT('Ctrl Pts',(62.5134793937788,6.26731706752099,39.9562444559261));
#173188=CARTESIAN_POINT('Ctrl Pts',(62.5022494248245,6.25949391181599,39.9371138113764));
#173189=CARTESIAN_POINT('Ctrl Pts',(62.4904862127,6.25357708651817,39.9174410654527));
#173190=CARTESIAN_POINT('Ctrl Pts',(62.4783706704752,6.24962081353501,39.8975196504339));
#173191=CARTESIAN_POINT('Ctrl Pts',(62.4703445484988,6.24699992138299,39.8843224113905));
#173192=CARTESIAN_POINT('Ctrl Pts',(62.4621637089607,6.24524040122917,39.8710160447197));
#173193=CARTESIAN_POINT('Ctrl Pts',(62.4538823482276,6.24436990787975,39.8576902534424));
#173194=CARTESIAN_POINT('',(62.099536274866,6.20712349654379,39.2875012672119));
#173195=CARTESIAN_POINT('',(62.4538823482276,6.24436990787975,39.8576902534424));
#173196=CARTESIAN_POINT('',(62.4081695979768,0.318048871877121,39.2875012672119));
#173197=CARTESIAN_POINT('Origin',(5.53234440788222E-15,0.,39.2875012672119));
#173198=CARTESIAN_POINT('',(62.7644678366119,0.318045750793045,39.8576902534424));
#173199=CARTESIAN_POINT('',(62.4081695979768,0.318048871877129,39.2875012672119));
#173200=CARTESIAN_POINT('Ctrl Pts',(62.7644678366119,0.318045750793045,
39.8576902534424));
#173201=CARTESIAN_POINT('Ctrl Pts',(62.77677377149,0.318045618798131,39.8773836120337));
#173202=CARTESIAN_POINT('Ctrl Pts',(62.7890393354348,0.316095234070915,
39.8969946442079));
#173203=CARTESIAN_POINT('Ctrl Pts',(62.8010929413131,0.312273660578547,
39.9162525288162));
#173204=CARTESIAN_POINT('Ctrl Pts',(62.8133887511199,0.308375296777785,
39.9358973793958));
#173205=CARTESIAN_POINT('Ctrl Pts',(62.8254649274551,0.302529834048776,
39.9551762199609));
#173206=CARTESIAN_POINT('Ctrl Pts',(62.8371482135701,0.294768478454403,
39.9738152034089));
#173207=CARTESIAN_POINT('Ctrl Pts',(62.8483776146108,0.287308644488986,
39.9917300792467));
#173208=CARTESIAN_POINT('Ctrl Pts',(62.8592448608851,0.278078518365762,
40.0090551157924));
#173209=CARTESIAN_POINT('Ctrl Pts',(62.8695915013795,0.267060783356013,
40.0255394551319));
#173210=CARTESIAN_POINT('Ctrl Pts',(62.8775394315759,0.258597341640156,
40.0382021526012));
#173211=CARTESIAN_POINT('Ctrl Pts',(62.8851801717829,0.24907818494972,40.0503687782058));
#173212=CARTESIAN_POINT('Ctrl Pts',(62.8924356323738,0.238478017627863,
40.0619155352442));
#173213=CARTESIAN_POINT('Ctrl Pts',(62.892454647642,0.238450236479755,40.0619457972351));
#173214=CARTESIAN_POINT('Ctrl Pts',(62.8924736601095,0.238422447083332,
40.0619760547304));
#173215=CARTESIAN_POINT('Ctrl Pts',(62.8924926697742,0.238394649441168,
40.0620063077269));
#173216=CARTESIAN_POINT('Ctrl Pts',(62.8945308924032,0.235414176912503,
40.06525004417));
#173217=CARTESIAN_POINT('Ctrl Pts',(62.8965351787718,0.232339728999319,
40.0684393223556));
#173218=CARTESIAN_POINT('Ctrl Pts',(62.8985027695519,0.229175397309127,
40.0715697951759));
#173219=CARTESIAN_POINT('Ctrl Pts',(62.9094519648687,0.211566610932373,
40.0889901646398));
#173220=CARTESIAN_POINT('Ctrl Pts',(62.9192690206934,0.191177078589634,
40.1045963098203));
#173221=CARTESIAN_POINT('Ctrl Pts',(62.9274935913864,0.168765047550033,
40.1176634650675));
#173222=CARTESIAN_POINT('Ctrl Pts',(62.9311848926116,0.158706217646069,
40.1235281853032));
#173223=CARTESIAN_POINT('Ctrl Pts',(62.9345557609568,0.14823988692456,40.1288820140906));
#173224=CARTESIAN_POINT('Ctrl Pts',(62.9375663198809,0.137433186922361,
40.1336621774101));
#173225=CARTESIAN_POINT('Ctrl Pts',(62.9388746680683,0.132736741273613,
40.1357395717319));
#173226=CARTESIAN_POINT('Ctrl Pts',(62.9401148076313,0.127976140238101,
40.1377083672884));
#173227=CARTESIAN_POINT('Ctrl Pts',(62.9412833674838,0.123156980417561,
40.1395632548791));
#173228=CARTESIAN_POINT('Ctrl Pts',(62.9453733269673,0.106289921045671,
40.1460553614469));
#173229=CARTESIAN_POINT('Ctrl Pts',(62.9485864317704,0.0887055165510538,
40.151152097463));
#173230=CARTESIAN_POINT('Ctrl Pts',(62.9507781643242,0.0706437212501634,
40.1546258197409));
#173231=CARTESIAN_POINT('Ctrl Pts',(62.9518740306011,0.0616128235997182,
40.1563626808798));
#173232=CARTESIAN_POINT('Ctrl Pts',(62.9527145544238,0.05246257825014,40.1576937882008));
#173233=CARTESIAN_POINT('Ctrl Pts',(62.9532816790167,0.0432229794975189,
40.1585906813668));
#173234=CARTESIAN_POINT('Ctrl Pts',(62.9535652413132,0.0386031801212083,
40.1590391279498));
#173235=CARTESIAN_POINT('Ctrl Pts',(62.9537804539255,0.0339610423941129,
40.1593790209175));
#173236=CARTESIAN_POINT('Ctrl Pts',(62.9539250604562,0.0293003156016006,
40.1596068022931));
#173237=CARTESIAN_POINT('Ctrl Pts',(62.9540696669868,0.024639588809088,
40.1598345836686));
#173238=CARTESIAN_POINT('Ctrl Pts',(62.9541436657296,0.0199602729507933,
40.1599502506865));
#173239=CARTESIAN_POINT('Ctrl Pts',(62.9541448057648,0.0152661173108668,
40.1599502534424));
#173240=CARTESIAN_POINT('Origin',(5.71385722241845E-15,0.,40.5765));
#173241=CARTESIAN_POINT('',(-59.1088767419348,-0.316922544675689,39.8576902534424));
#173242=CARTESIAN_POINT('Ctrl Pts',(-58.9208513795073,-0.0152121934559198,
40.1599502534424));
#173243=CARTESIAN_POINT('Ctrl Pts',(-58.9208504012364,-0.0190220008285423,
40.1599502448875));
#173244=CARTESIAN_POINT('Ctrl Pts',(-58.9208964366351,-0.0228214099817212,
40.1598743450437));
#173245=CARTESIAN_POINT('Ctrl Pts',(-58.9209883940807,-0.0266084895330029,
40.1597243308499));
#173246=CARTESIAN_POINT('Ctrl Pts',(-58.9215313038856,-0.048967120813079,
40.1588386583938));
#173247=CARTESIAN_POINT('Ctrl Pts',(-58.9236732325286,-0.0708986527603139,
40.1553722553618));
#173248=CARTESIAN_POINT('Ctrl Pts',(-58.9271900305696,-0.0919988953507848,
40.1496902177788));
#173249=CARTESIAN_POINT('Ctrl Pts',(-58.9285037892487,-0.0998812435867534,
40.1475675976844));
#173250=CARTESIAN_POINT('Ctrl Pts',(-58.9300091878196,-0.107647933246467,
40.1451361443096));
#173251=CARTESIAN_POINT('Ctrl Pts',(-58.9316938830317,-0.115279202946911,
40.1424159447501));
#173252=CARTESIAN_POINT('Ctrl Pts',(-58.933008366749,-0.121233502390215,
40.1402935085949));
#173253=CARTESIAN_POINT('Ctrl Pts',(-58.9344322364591,-0.127104908280006,
40.1379949176048));
#173254=CARTESIAN_POINT('Ctrl Pts',(-58.9359598525093,-0.132883578273067,
40.1355293609261));
#173255=CARTESIAN_POINT('Ctrl Pts',(-58.9413065086849,-0.153108923248783,
40.1268999125509));
#173256=CARTESIAN_POINT('Ctrl Pts',(-58.9479240485795,-0.172198253417716,
40.1162251288835));
#173257=CARTESIAN_POINT('Ctrl Pts',(-58.9555707636545,-0.189729578870775,
40.1038990521418));
#173258=CARTESIAN_POINT('Ctrl Pts',(-58.959394121192,-0.198495241597304,
40.097736013771));
#173259=CARTESIAN_POINT('Ctrl Pts',(-58.9634747743348,-0.20687140316055,
40.0911601532641));
#173260=CARTESIAN_POINT('Ctrl Pts',(-58.9677825146336,-0.214805314863214,
40.084220729064));
#173261=CARTESIAN_POINT('Ctrl Pts',(-58.9720718502312,-0.222705329147628,
40.0773109533618));
#173262=CARTESIAN_POINT('Ctrl Pts',(-58.9765861722458,-0.230167055079178,
40.0700409753048));
#173263=CARTESIAN_POINT('Ctrl Pts',(-58.9812961520165,-0.237137844566648,
40.0624586415899));
#173264=CARTESIAN_POINT('Ctrl Pts',(-58.9813163616197,-0.237167754862791,
40.062426107277));
#173265=CARTESIAN_POINT('Ctrl Pts',(-58.9813365744745,-0.2371976565367,
40.0623935677889));
#173266=CARTESIAN_POINT('Ctrl Pts',(-58.9813567905789,-0.237227549587953,
40.0623610231289));
#173267=CARTESIAN_POINT('Ctrl Pts',(-58.9908903168209,-0.251324537972149,
40.0470135870235));
#173268=CARTESIAN_POINT('Ctrl Pts',(-59.0011093202327,-0.263501580512048,
40.0305755292096));
#173269=CARTESIAN_POINT('Ctrl Pts',(-59.0118294103842,-0.273820596508944,
40.0133447567344));
#173270=CARTESIAN_POINT('Ctrl Pts',(-59.0229394763222,-0.284514998003796,
39.9954871626604));
#173271=CARTESIAN_POINT('Ctrl Pts',(-59.034588573655,-0.293214009568305,
39.9767767954325));
#173272=CARTESIAN_POINT('Ctrl Pts',(-59.0465875206388,-0.299936893972227,
39.9575197577489));
#173273=CARTESIAN_POINT('Ctrl Pts',(-59.0584152157261,-0.306563827731033,
39.9385375612016));
#173274=CARTESIAN_POINT('Ctrl Pts',(-59.0705837677952,-0.311270560393244,
39.9190226977119));
#173275=CARTESIAN_POINT('Ctrl Pts',(-59.0829139906028,-0.314027284735643,
39.8992655451885));
#173276=CARTESIAN_POINT('Ctrl Pts',(-59.0915108413207,-0.315949321994157,
39.8854905069345));
#173277=CARTESIAN_POINT('Ctrl Pts',(-59.100186339707,-0.316922445687725,
39.8715976051485));
#173278=CARTESIAN_POINT('Ctrl Pts',(-59.1088767419348,-0.316922544675689,
39.8576902534424));
#173279=CARTESIAN_POINT('',(-59.4651754363832,-0.316925998273048,39.2875012672119));
#173280=CARTESIAN_POINT('',(-59.1088767419348,-0.316922544675689,39.8576902534424));
#173281=CARTESIAN_POINT('',(-59.1725467709678,-5.90061356181218,39.2875012672119));
#173282=CARTESIAN_POINT('Origin',(5.53234440788222E-15,0.,39.2875012672119));
#173283=CARTESIAN_POINT('',(-58.8181995570485,-5.86337364149541,39.8576902534424));
#173284=CARTESIAN_POINT('',(-59.1725467709678,-5.90061356181218,39.2875012672119));
#173285=CARTESIAN_POINT('',(-58.5996668978649,-6.14377718965283,40.1599502534424));
#173286=CARTESIAN_POINT('Ctrl Pts',(-58.8181995570485,-5.86337364149541,
39.8576902534424));
#173287=CARTESIAN_POINT('Ctrl Pts',(-58.8060365798455,-5.86209540502828,
39.8772619994052));
#173288=CARTESIAN_POINT('Ctrl Pts',(-58.7937272422247,-5.86273454612488,
39.8967644650367));
#173289=CARTESIAN_POINT('Ctrl Pts',(-58.7814443761802,-5.86523378400431,
39.9159282836043));
#173290=CARTESIAN_POINT('Ctrl Pts',(-58.7689396367198,-5.86777816724666,
39.9354382707185));
#173291=CARTESIAN_POINT('Ctrl Pts',(-58.7564614161384,-5.87225032431021,
39.9545987622356));
#173292=CARTESIAN_POINT('Ctrl Pts',(-58.7441787427588,-5.87864135443934,
39.9731387498235));
#173293=CARTESIAN_POINT('Ctrl Pts',(-58.7324160859241,-5.88476180492315,
39.9908938024065));
#173294=CARTESIAN_POINT('Ctrl Pts',(-58.7208319573121,-5.89264238981923,
40.0080810366197));
#173295=CARTESIAN_POINT('Ctrl Pts',(-58.709575439463,-5.90232005415971,
40.024454274256));
#173296=CARTESIAN_POINT('Ctrl Pts',(-58.7006223753283,-5.91001735013313,
40.0374770090498));
#173297=CARTESIAN_POINT('Ctrl Pts',(-58.6918764318948,-5.91885232406574,
40.0499848770044));
#173298=CARTESIAN_POINT('Ctrl Pts',(-58.6834178317481,-5.92886364759513,
40.0618424270193));
#173299=CARTESIAN_POINT('Ctrl Pts',(-58.6833947425173,-5.92889097525637,
40.0618747942791));
#173300=CARTESIAN_POINT('Ctrl Pts',(-58.683371655605,-5.92891831167191,
40.0619071564124));
#173301=CARTESIAN_POINT('Ctrl Pts',(-58.6833485710132,-5.9289456568414,
40.0619395134161));
#173302=CARTESIAN_POINT('Ctrl Pts',(-58.6787531612542,-5.9343892124318,
40.0683807661799));
#173303=CARTESIAN_POINT('Ctrl Pts',(-58.6742527563956,-5.94021607194738,
40.0746073439084));
#173304=CARTESIAN_POINT('Ctrl Pts',(-58.6698707672381,-5.94639317576837,
40.0805869293669));
#173305=CARTESIAN_POINT('Ctrl Pts',(-58.6611744062938,-5.95865206607742,
40.092453830807));
#173306=CARTESIAN_POINT('Ctrl Pts',(-58.6529445485198,-5.97229179622479,
40.1033475319609));
#173307=CARTESIAN_POINT('Ctrl Pts',(-58.6453649253901,-5.98706231729999,
40.1130129263075));
#173308=CARTESIAN_POINT('Ctrl Pts',(-58.6396802080428,-5.99814020810639,
40.1202619720674));
#173309=CARTESIAN_POINT('Ctrl Pts',(-58.6343612468744,-6.0098541687323,
40.1268200947266));
#173310=CARTESIAN_POINT('Ctrl Pts',(-58.6294855649109,-6.02209871088753,
40.1325796782703));
#173311=CARTESIAN_POINT('Ctrl Pts',(-58.6276571841746,-6.02669041419573,
40.1347395220992));
#173312=CARTESIAN_POINT('Ctrl Pts',(-58.6258911397672,-6.03135673055,40.1367870714852));
#173313=CARTESIAN_POINT('Ctrl Pts',(-58.624191520627,-6.0360920971711,40.1387166518767));
#173314=CARTESIAN_POINT('Ctrl Pts',(-58.6182428536363,-6.05266588034495,
40.1454701832469));
#173315=CARTESIAN_POINT('Ctrl Pts',(-58.6131078911177,-6.07008552874929,
40.1507785912492));
#173316=CARTESIAN_POINT('Ctrl Pts',(-58.608961992561,-6.08811254303222,
40.1543986087265));
#173317=CARTESIAN_POINT('Ctrl Pts',(-58.6068890432827,-6.09712605017368,
40.1562086174652));
#173318=CARTESIAN_POINT('Ctrl Pts',(-58.6050633610079,-6.10629139889362,
40.1575965292115));
#173319=CARTESIAN_POINT('Ctrl Pts',(-58.6035068699781,-6.11557877725374,
40.1585319382567));
#173320=CARTESIAN_POINT('Ctrl Pts',(-58.6027286244632,-6.1202224664338,
40.1589996427793));
#173321=CARTESIAN_POINT('Ctrl Pts',(-58.6020176767849,-6.12489666302693,
40.159354221642));
#173322=CARTESIAN_POINT('Ctrl Pts',(-58.6013767677628,-6.1295976405732,
40.159591874311));
#173323=CARTESIAN_POINT('Ctrl Pts',(-58.6007358587407,-6.13429861811947,
40.1598295269801));
#173324=CARTESIAN_POINT('Ctrl Pts',(-58.600164990065,-6.13902637679605,
40.1599502506896));
#173325=CARTESIAN_POINT('Ctrl Pts',(-58.5996668978649,-6.14377718965283,
40.1599502534424));
#173326=CARTESIAN_POINT('',(-58.5964866834551,-6.17403490858981,40.1599502534424));
#173327=CARTESIAN_POINT('Origin',(3.34731138317026E-16,-7.12196207432512E-18,
40.1599502534424));
#173328=CARTESIAN_POINT('',(-58.7519447039089,-6.49374646112701,39.8576902534424));
#173329=CARTESIAN_POINT('Ctrl Pts',(-58.5964866834551,-6.17403490858982,
40.1599502534424));
#173330=CARTESIAN_POINT('Ctrl Pts',(-58.5960874772333,-6.17782374318187,
40.1599502448875));
#173331=CARTESIAN_POINT('Ctrl Pts',(-58.5957361140451,-6.18160715078365,
40.1598743450437));
#173332=CARTESIAN_POINT('Ctrl Pts',(-58.5954317101325,-6.18538309648738,
40.1597243308499));
#173333=CARTESIAN_POINT('Ctrl Pts',(-58.5936345324521,-6.20767599437444,
40.1588386583938));
#173334=CARTESIAN_POINT('Ctrl Pts',(-58.5934722580544,-6.22971127560536,
40.1553722553615));
#173335=CARTESIAN_POINT('Ctrl Pts',(-58.5947642147754,-6.25106353435488,
40.149690217778));
#173336=CARTESIAN_POINT('Ctrl Pts',(-58.5952468467989,-6.25904002743736,
40.1475675976838));
#173337=CARTESIAN_POINT('Ctrl Pts',(-58.595932158504,-6.26692152735676,
40.1451361443093));
#173338=CARTESIAN_POINT('Ctrl Pts',(-58.5968099398848,-6.27468709076401,
40.1424159447501));
#173339=CARTESIAN_POINT('Ctrl Pts',(-58.5974948289521,-6.28074617289492,
40.1402935085949));
#173340=CARTESIAN_POINT('Ctrl Pts',(-58.5982971695201,-6.2867342495216,
40.1379949176048));
#173341=CARTESIAN_POINT('Ctrl Pts',(-58.5992123816356,-6.292640942714,40.1355293609261));
#173342=CARTESIAN_POINT('Ctrl Pts',(-58.6024156240399,-6.31331436888738,
40.1268999125509));
#173343=CARTESIAN_POINT('Ctrl Pts',(-58.6070015340112,-6.33299084698409,
40.1162251288835));
#173344=CARTESIAN_POINT('Ctrl Pts',(-58.6127738370723,-6.35122543337782,
40.1038990521418));
#173345=CARTESIAN_POINT('Ctrl Pts',(-58.6156599886028,-6.36034272657469,
40.097736013771));
#173346=CARTESIAN_POINT('Ctrl Pts',(-58.6188427402045,-6.36909954705062,
40.0911601532641));
#173347=CARTESIAN_POINT('Ctrl Pts',(-58.6222975626532,-6.37744027742843,
40.084220729064));
#173348=CARTESIAN_POINT('Ctrl Pts',(-58.6257376244687,-6.38574537226646,
40.0773109533619));
#173349=CARTESIAN_POINT('Ctrl Pts',(-58.6294472538099,-6.3936380972255,
40.0700409753048));
#173350=CARTESIAN_POINT('Ctrl Pts',(-58.6334027859057,-6.40106302694625,
40.0624586415899));
#173351=CARTESIAN_POINT('Ctrl Pts',(-58.6334197583214,-6.40109488586943,
40.0624261072769));
#173352=CARTESIAN_POINT('Ctrl Pts',(-58.633436734872,-6.40112673655749,
40.0623935677889));
#173353=CARTESIAN_POINT('Ctrl Pts',(-58.6334537155557,-6.4011585790098,
40.0623610231289));
#173354=CARTESIAN_POINT('Ctrl Pts',(-58.6414614796112,-6.41617486746464,
40.0470135870231));
#173355=CARTESIAN_POINT('Ctrl Pts',(-58.6503516547095,-6.42935337961447,
40.0305755292087));
#173356=CARTESIAN_POINT('Ctrl Pts',(-58.6599343882012,-6.44073642151188,
40.013344756733));
#173357=CARTESIAN_POINT('Ctrl Pts',(-58.6698657226821,-6.45253355607591,
39.9954871626584));
#173358=CARTESIAN_POINT('Ctrl Pts',(-58.6805417107304,-6.46240257578764,
39.9767767954299));
#173359=CARTESIAN_POINT('Ctrl Pts',(-58.691772193452,-6.47034286301642,
39.9575197577457));
#173360=CARTESIAN_POINT('Ctrl Pts',(-58.7028423919865,-6.47816982453019,
39.9385375611978));
#173361=CARTESIAN_POINT('Ctrl Pts',(-58.7144522959223,-6.48412273326628,
39.9190226977075));
#173362=CARTESIAN_POINT('Ctrl Pts',(-58.7264268163205,-6.48815321522591,
39.8992655451835));
#173363=CARTESIAN_POINT('Ctrl Pts',(-58.7347756649887,-6.49096333895714,
39.8854905069312));
#173364=CARTESIAN_POINT('Ctrl Pts',(-58.7433019189619,-6.49283796829136,
39.8715976051468));
#173365=CARTESIAN_POINT('Ctrl Pts',(-58.7519447039089,-6.49374646112702,
39.8576902534424));
#173366=CARTESIAN_POINT('',(-59.1062911958297,-6.53099325080016,39.2875012672119));
#173367=CARTESIAN_POINT('',(-58.7519447039089,-6.49374646112701,39.8576902534424));
#173368=CARTESIAN_POINT('',(-58.2316113004782,-12.0535047649318,39.2875012672119));
#173369=CARTESIAN_POINT('Origin',(5.53234440788222E-15,0.,39.2875012672119));
#173370=CARTESIAN_POINT('',(-57.8830978693156,-11.9794294790609,39.8576902534424));
#173371=CARTESIAN_POINT('',(-58.2316113004781,-12.0535047649318,39.2875012672119));
#173372=CARTESIAN_POINT('',(-57.6364522029208,-12.2354540642041,40.1599502534424));
#173373=CARTESIAN_POINT('Ctrl Pts',(-57.8830978693156,-11.9794294790609,
39.8576902534424));
#173374=CARTESIAN_POINT('Ctrl Pts',(-57.8711351342687,-11.9768868675911,
39.877261999404));
#173375=CARTESIAN_POINT('Ctrl Pts',(-57.8588264200515,-11.9762358312605,
39.8967644650343));
#173376=CARTESIAN_POINT('Ctrl Pts',(-57.8463495993382,-11.9774374689408,
39.9159282836008));
#173377=CARTESIAN_POINT('Ctrl Pts',(-57.8336474016795,-11.9786608125859,
39.9354382707139));
#173378=CARTESIAN_POINT('Ctrl Pts',(-57.8207700703914,-11.9818041414829,
39.95459876223));
#173379=CARTESIAN_POINT('Ctrl Pts',(-57.8078866382244,-11.9868762719064,
39.973138749817));
#173380=CARTESIAN_POINT('Ctrl Pts',(-57.7955486571718,-11.9917336614785,
39.9908938023992));
#173381=CARTESIAN_POINT('Ctrl Pts',(-57.7832042422001,-11.998360204543,
40.0080810366116));
#173382=CARTESIAN_POINT('Ctrl Pts',(-57.7709977973527,-12.006808227112,
40.0244542742473));
#173383=CARTESIAN_POINT('Ctrl Pts',(-57.7612891925185,-12.0135275064582,
40.0374770090442));
#173384=CARTESIAN_POINT('Ctrl Pts',(-57.7516676540278,-12.0213998814537,
40.0499848770018));
#173385=CARTESIAN_POINT('Ctrl Pts',(-57.7422089227118,-12.0304721974326,
40.0618424270193));
#173386=CARTESIAN_POINT('Ctrl Pts',(-57.7421831034479,-12.0304969619082,
40.0618747942791));
#173387=CARTESIAN_POINT('Ctrl Pts',(-57.7421572855746,-12.0305217353326,
40.0619071564124));
#173388=CARTESIAN_POINT('Ctrl Pts',(-57.7421314690941,-12.0305465177055,
40.0619395134162));
#173389=CARTESIAN_POINT('Ctrl Pts',(-57.7369922269699,-12.0354799018086,
40.0683807661799));
#173390=CARTESIAN_POINT('Ctrl Pts',(-57.7319074031292,-12.0408044207741,
40.0746073439084));
#173391=CARTESIAN_POINT('Ctrl Pts',(-57.726903735797,-12.0464896431813,
40.0805869293669));
#173392=CARTESIAN_POINT('Ctrl Pts',(-57.7169736114625,-12.0577723607611,
40.092453830807));
#173393=CARTESIAN_POINT('Ctrl Pts',(-57.7073630976788,-12.0704771166535,
40.1033475319609));
#173394=CARTESIAN_POINT('Ctrl Pts',(-57.698281056648,-12.0843744369109,
40.1130129263075));
#173395=CARTESIAN_POINT('Ctrl Pts',(-57.6914695258749,-12.094797427104,
40.1202619720674));
#173396=CARTESIAN_POINT('Ctrl Pts',(-57.6849552602293,-12.1058912345908,
40.1268200947266));
#173397=CARTESIAN_POINT('Ctrl Pts',(-57.6788263845868,-12.1175590523199,
40.1325796782703));
#173398=CARTESIAN_POINT('Ctrl Pts',(-57.6765280562209,-12.1219344839683,
40.1347395220992));
#173399=CARTESIAN_POINT('Ctrl Pts',(-57.674283923512,-12.1263906358454,
40.1367870714852));
#173400=CARTESIAN_POINT('Ctrl Pts',(-57.6720986344674,-12.1309224030558,
40.1387166518767));
#173401=CARTESIAN_POINT('Ctrl Pts',(-57.6644501228112,-12.1467835882923,
40.1454701832469));
#173402=CARTESIAN_POINT('Ctrl Pts',(-57.6575224410761,-12.163571060299,
40.1507785912492));
#173403=CARTESIAN_POINT('Ctrl Pts',(-57.6515149180852,-12.1810659563065,
40.1543986087265));
#173404=CARTESIAN_POINT('Ctrl Pts',(-57.6485111565898,-12.1898134043102,
40.1562086174652));
#173405=CARTESIAN_POINT('Ctrl Pts',(-57.6457374357765,-12.1987377085283,
40.1575965292115));
#173406=CARTESIAN_POINT('Ctrl Pts',(-57.6432186759796,-12.2078115120426,
40.1585319382567));
#173407=CARTESIAN_POINT('Ctrl Pts',(-57.6419592960812,-12.2123484137997,
40.1589996427793));
#173408=CARTESIAN_POINT('Ctrl Pts',(-57.6407636564618,-12.2169226903865,
40.159354221642));
#173409=CARTESIAN_POINT('Ctrl Pts',(-57.6396348724476,-12.2215309222508,
40.1595918743111));
#173410=CARTESIAN_POINT('Ctrl Pts',(-57.6385060884334,-12.226139154115,
40.1598295269801));
#173411=CARTESIAN_POINT('Ctrl Pts',(-57.637444161687,-12.2307813416095,
40.1599502506896));
#173412=CARTESIAN_POINT('Ctrl Pts',(-57.6364522029208,-12.2354540642041,
40.1599502534424));
#173413=CARTESIAN_POINT('',(-57.6301266171958,-12.2652136052657,40.1599502534424));
#173414=CARTESIAN_POINT('Origin',(3.35846787602729E-16,-1.41658944417981E-17,
40.1599502534424));
#173415=CARTESIAN_POINT('',(-57.7513140650721,-12.5994235324468,39.8576902534424));
#173416=CARTESIAN_POINT('Ctrl Pts',(-57.6301266171958,-12.2652136052657,
40.1599502534424));
#173417=CARTESIAN_POINT('Ctrl Pts',(-57.62933355681,-12.2689399558126,40.1599502448875));
#173418=CARTESIAN_POINT('Ctrl Pts',(-57.6285886446436,-12.2726659100575,
40.1598743450437));
#173419=CARTESIAN_POINT('Ctrl Pts',(-57.6278912144856,-12.2763893518624,
40.1597243308499));
#173420=CARTESIAN_POINT('Ctrl Pts',(-57.6237736395752,-12.2983722706985,
40.1588386583939));
#173421=CARTESIAN_POINT('Ctrl Pts',(-57.621308940049,-12.3202698780571,
40.1553722553623));
#173422=CARTESIAN_POINT('Ctrl Pts',(-57.6203619005013,-12.3416402131472,
40.1496902177801));
#173423=CARTESIAN_POINT('Ctrl Pts',(-57.6200081180517,-12.3496234589524,
40.1475675976854));
#173424=CARTESIAN_POINT('Ctrl Pts',(-57.6198658344726,-12.3575334177726,
40.1451361443101));
#173425=CARTESIAN_POINT('Ctrl Pts',(-57.6199270848658,-12.3653481937524,
40.1424159447501));
#173426=CARTESIAN_POINT('Ctrl Pts',(-57.6199748754952,-12.3714456739991,
40.1402935085949));
#173427=CARTESIAN_POINT('Ctrl Pts',(-57.6201468963099,-12.3774848147421,
40.1379949176048));
#173428=CARTESIAN_POINT('Ctrl Pts',(-57.6204396772352,-12.3834548161672,
40.1355293609261));
#173429=CARTESIAN_POINT('Ctrl Pts',(-57.6214644104741,-12.4043498211549,
40.1268999125509));
#173430=CARTESIAN_POINT('Ctrl Pts',(-57.6239684463328,-12.4243978675678,
40.1162251288835));
#173431=CARTESIAN_POINT('Ctrl Pts',(-57.6278030948197,-12.4431359329578,
40.1038990521418));
#173432=CARTESIAN_POINT('Ctrl Pts',(-57.6297204190631,-12.4525049656528,
40.097736013771));
#173433=CARTESIAN_POINT('Ctrl Pts',(-57.631970398231,-12.4615465034838,
40.0911601532641));
#173434=CARTESIAN_POINT('Ctrl Pts',(-57.634534451072,-12.4702026697494,
40.084220729064));
#173435=CARTESIAN_POINT('Ctrl Pts',(-57.6370875490682,-12.478821852784,
40.0773109533619));
#173436=CARTESIAN_POINT('Ctrl Pts',(-57.6399518422608,-12.4870591024242,
40.0700409753048));
#173437=CARTESIAN_POINT('Ctrl Pts',(-57.6431095890443,-12.4948568232945,
40.0624586415899));
#173438=CARTESIAN_POINT('Ctrl Pts',(-57.643123138319,-12.4948902817916,
40.062426107277));
#173439=CARTESIAN_POINT('Ctrl Pts',(-57.6431366925668,-12.4949237325311,
40.0623935677889));
#173440=CARTESIAN_POINT('Ctrl Pts',(-57.643150251786,-12.4949571755119,
40.0623610231289));
#173441=CARTESIAN_POINT('Ctrl Pts',(-57.6495445189164,-12.5107282424396,
40.0470135870218));
#173442=CARTESIAN_POINT('Ctrl Pts',(-57.6570084630829,-12.5247638376633,
40.0305755292059));
#173443=CARTESIAN_POINT('Ctrl Pts',(-57.6653488494819,-12.5370861904728,
40.0133447567286));
#173444=CARTESIAN_POINT('Ctrl Pts',(-57.6739926427273,-12.5498568062315,
39.9954871626524));
#173445=CARTESIAN_POINT('Ctrl Pts',(-57.6835785531326,-12.5607877070457,
39.9767767954222));
#173446=CARTESIAN_POINT('Ctrl Pts',(-57.693917528074,-12.569858401651,39.9575197577362));
#173447=CARTESIAN_POINT('Ctrl Pts',(-57.7041089426444,-12.5787996370916,
39.9385375611868));
#173448=CARTESIAN_POINT('Ctrl Pts',(-57.7150329979106,-12.5859335005876,
39.919022697695));
#173449=CARTESIAN_POINT('Ctrl Pts',(-57.7265206205487,-12.5911935813604,
39.8992655451695));
#173450=CARTESIAN_POINT('Ctrl Pts',(-57.7345299954327,-12.5948610032592,
39.8854905069218));
#173451=CARTESIAN_POINT('Ctrl Pts',(-57.7428135895682,-12.5976165994018,
39.8715976051421));
#173452=CARTESIAN_POINT('Ctrl Pts',(-57.7513140650721,-12.5994235324468,
39.8576902534424));
#173453=CARTESIAN_POINT('',(-58.0998260601481,-12.6735055745737,39.2875012672119));
#173454=CARTESIAN_POINT('',(-57.7513140650721,-12.5994235324468,39.8576902534424));
#173455=CARTESIAN_POINT('',(-56.6526781108324,-18.0743352474888,39.2875012672119));
#173456=CARTESIAN_POINT('Origin',(5.53234440788222E-15,0.,39.2875012672119));
#173457=CARTESIAN_POINT('',(-56.3138168485096,-17.9642361803969,39.8576902534424));
#173458=CARTESIAN_POINT('',(-56.6526781108324,-18.0743352474888,39.2875012672119));
#173459=CARTESIAN_POINT('',(-56.0417604764384,-18.1930767435946,40.1599502534424));
#173460=CARTESIAN_POINT('Ctrl Pts',(-56.3138168485096,-17.9642361803969,
39.8576902534424));
#173461=CARTESIAN_POINT('Ctrl Pts',(-56.3021854218462,-17.960457051308,
39.8772619994045));
#173462=CARTESIAN_POINT('Ctrl Pts',(-56.2900121878802,-17.9585229704407,
39.8967644650352));
#173463=CARTESIAN_POINT('Ctrl Pts',(-56.2774781111558,-17.9584138425286,
39.9159282836022));
#173464=CARTESIAN_POINT('Ctrl Pts',(-56.2647176232334,-17.9583027433679,
39.9354382707156));
#173465=CARTESIAN_POINT('Ctrl Pts',(-56.2515822679742,-17.9600828051299,
39.9545987622319));
#173466=CARTESIAN_POINT('Ctrl Pts',(-56.2382392305977,-17.9637804645263,
39.9731387498191));
#173467=CARTESIAN_POINT('Ctrl Pts',(-56.2254611028288,-17.967321574611,
39.9908938024012));
#173468=CARTESIAN_POINT('Ctrl Pts',(-56.2124916494907,-17.9726214740523,
40.0080810366136));
#173469=CARTESIAN_POINT('Ctrl Pts',(-56.1994690140086,-17.979747296548,
40.0244542742491));
#173470=CARTESIAN_POINT('Ctrl Pts',(-56.1891112379837,-17.9854149414348,
40.0374770090454));
#173471=CARTESIAN_POINT('Ctrl Pts',(-56.1787195200275,-17.9922384661035,
40.0499848770023));
#173472=CARTESIAN_POINT('Ctrl Pts',(-56.1683642893843,-18.0002723763369,
40.0618424270193));
#173473=CARTESIAN_POINT('Ctrl Pts',(-56.1683360229684,-18.0002943063021,
40.0618747942791));
#173474=CARTESIAN_POINT('Ctrl Pts',(-56.1683077570002,-18.0003162453124,
40.0619071564124));
#173475=CARTESIAN_POINT('Ctrl Pts',(-56.1682794914817,-18.0003381933678,
40.0619395134161));
#173476=CARTESIAN_POINT('Ctrl Pts',(-56.1626527236046,-18.004707354795,
40.0683807661799));
#173477=CARTESIAN_POINT('Ctrl Pts',(-56.1570391911758,-18.0094711966665,
40.0746073439084));
#173478=CARTESIAN_POINT('Ctrl Pts',(-56.1514686668952,-18.0146022491736,
40.0805869293669));
#173479=CARTESIAN_POINT('Ctrl Pts',(-56.1404135756907,-18.0247851782092,
40.092453830807));
#173480=CARTESIAN_POINT('Ctrl Pts',(-56.1295277006975,-18.0364157638825,
40.1033475319609));
#173481=CARTESIAN_POINT('Ctrl Pts',(-56.1190427465077,-18.0492876213731,
40.1130129263075));
#173482=CARTESIAN_POINT('Ctrl Pts',(-56.1111790308653,-18.0589415144911,
40.1202619720674));
#173483=CARTESIAN_POINT('Ctrl Pts',(-56.1035408324002,-18.0692936227625,
40.1268200947266));
#173484=CARTESIAN_POINT('Ctrl Pts',(-56.0962259123228,-18.0802568810128,
40.1325796782703));
#173485=CARTESIAN_POINT('Ctrl Pts',(-56.0934828172938,-18.0843681028567,
40.1347395220992));
#173486=CARTESIAN_POINT('Ctrl Pts',(-56.0907851834709,-18.0885652677241,
40.1367870714852));
#173487=CARTESIAN_POINT('Ctrl Pts',(-56.0881381670059,-18.0928437845339,
40.1387166518767));
#173488=CARTESIAN_POINT('Ctrl Pts',(-56.0788736093784,-18.1078185933684,
40.1454701832469));
#173489=CARTESIAN_POINT('Ctrl Pts',(-56.0702291095578,-18.1237899619212,
40.1507785912492));
#173490=CARTESIAN_POINT('Ctrl Pts',(-56.0624257818118,-18.1405610619115,
40.1543986087265));
#173491=CARTESIAN_POINT('Ctrl Pts',(-56.0585241179387,-18.1489466119067,
40.1562086174652));
#173492=CARTESIAN_POINT('Ctrl Pts',(-56.0548327480526,-18.1575320950784,
40.1575965292115));
#173493=CARTESIAN_POINT('Ctrl Pts',(-56.0513793155481,-18.1662929092567,
40.1585319382567));
#173494=CARTESIAN_POINT('Ctrl Pts',(-56.0496525992959,-18.1706733163458,
40.1589996427793));
#173495=CARTESIAN_POINT('Ctrl Pts',(-56.0479853674132,-18.1750975561949,
40.159354221642));
#173496=CARTESIAN_POINT('Ctrl Pts',(-56.0463810756008,-18.1795625536244,
40.159591874311));
#173497=CARTESIAN_POINT('Ctrl Pts',(-56.0447767837884,-18.1840275510539,
40.1598295269801));
#173498=CARTESIAN_POINT('Ctrl Pts',(-56.0432354336628,-18.1885333065887,
40.1599502506896));
#173499=CARTESIAN_POINT('Ctrl Pts',(-56.0417604764384,-18.1930767435946,
40.1599502534424));
#173500=CARTESIAN_POINT('',(-56.0323588238392,-18.2220120550214,40.1599502534424));
#173501=CARTESIAN_POINT('Origin',(3.37692616670652E-16,-2.10546223053625E-17,
40.1599502534424));
#173502=CARTESIAN_POINT('',(-56.1179479440989,-18.5670586829462,39.8576902534424));
#173503=CARTESIAN_POINT('Ctrl Pts',(-56.0323588238392,-18.2220120550214,
40.1599502534424));
#173504=CARTESIAN_POINT('Ctrl Pts',(-56.0311805982249,-18.2256350948466,
40.1599502448875));
#173505=CARTESIAN_POINT('Ctrl Pts',(-56.0300502984939,-18.2292627734003,
40.1598743450437));
#173506=CARTESIAN_POINT('Ctrl Pts',(-56.0289674832814,-18.2328929164988,
40.1597243308499));
#173507=CARTESIAN_POINT('Ctrl Pts',(-56.0225746241534,-18.2543250068264,
40.1588386583939));
#173508=CARTESIAN_POINT('Ctrl Pts',(-56.0178345032628,-18.2758450255457,
40.1553722553627));
#173509=CARTESIAN_POINT('Ctrl Pts',(-56.0146588434103,-18.2969992991145,
40.149690217781));
#173510=CARTESIAN_POINT('Ctrl Pts',(-56.0134725226018,-18.3049018315292,
40.1475675976861));
#173511=CARTESIAN_POINT('Ctrl Pts',(-56.0125042026269,-18.3127535860847,
40.1451361443106));
#173512=CARTESIAN_POINT('Ctrl Pts',(-56.01174825096,-18.3205319543145,40.1424159447501));
#173513=CARTESIAN_POINT('Ctrl Pts',(-56.0111584195474,-18.3266010274075,
40.1402935085949));
#173514=CARTESIAN_POINT('Ctrl Pts',(-56.0106982359127,-18.332625066177,
40.1379949176048));
#173515=CARTESIAN_POINT('Ctrl Pts',(-56.0103653778789,-18.3385929672498,
40.1355293609261));
#173516=CARTESIAN_POINT('Ctrl Pts',(-56.0092003747605,-18.3594806210046,
40.1268999125509));
#173517=CARTESIAN_POINT('Ctrl Pts',(-56.0095951017657,-18.3796805851419,
40.1162251288835));
#173518=CARTESIAN_POINT('Ctrl Pts',(-56.0114500824671,-18.3987168313627,
40.1038990521418));
#173519=CARTESIAN_POINT('Ctrl Pts',(-56.0123775728178,-18.408234954473,
40.097736013771));
#173520=CARTESIAN_POINT('Ctrl Pts',(-56.0136701283094,-18.4174621486786,
40.0911601532641));
#173521=CARTESIAN_POINT('Ctrl Pts',(-56.0153153192431,-18.4263389120628,
40.084220729064));
#173522=CARTESIAN_POINT('Ctrl Pts',(-56.016953481144,-18.4351777497211,
40.0773109533618));
#173523=CARTESIAN_POINT('Ctrl Pts',(-56.0189410563924,-18.4436692750117,
40.0700409753048));
#173524=CARTESIAN_POINT('Ctrl Pts',(-56.0212664209291,-18.4517543535697,
40.0624586415899));
#173525=CARTESIAN_POINT('Ctrl Pts',(-56.0212763986141,-18.4517890450626,
40.0624261072769));
#173526=CARTESIAN_POINT('Ctrl Pts',(-56.021286382056,-18.4518237293601,
40.0623935677888));
#173527=CARTESIAN_POINT('Ctrl Pts',(-56.021296371253,-18.4518584064611,
40.0623610231288));
#173528=CARTESIAN_POINT('Ctrl Pts',(-56.0260070845288,-18.4682114607502,
40.0470135870224));
#173529=CARTESIAN_POINT('Ctrl Pts',(-56.031963021228,-18.4829503621277,
40.0305755292074));
#173530=CARTESIAN_POINT('Ctrl Pts',(-56.0389696815142,-18.4960770195721,
40.0133447567309));
#173531=CARTESIAN_POINT('Ctrl Pts',(-56.0462312303151,-18.5096811989857,
39.9954871626557));
#173532=CARTESIAN_POINT('Ctrl Pts',(-56.0546220378354,-18.5215542196648,
39.9767767954265));
#173533=CARTESIAN_POINT('Ctrl Pts',(-56.0639562290217,-18.5316559412182,
39.9575197577416));
#173534=CARTESIAN_POINT('Ctrl Pts',(-56.0731572003559,-18.5416134885389,
39.9385375611932));
#173535=CARTESIAN_POINT('Ctrl Pts',(-56.0832757207152,-18.5498501466939,
39.9190226977025));
#173536=CARTESIAN_POINT('Ctrl Pts',(-56.094150584794,-18.5562821957351,
39.899265545178));
#173537=CARTESIAN_POINT('Ctrl Pts',(-56.1017327335105,-18.5607667347627,
39.8854905069275));
#173538=CARTESIAN_POINT('Ctrl Pts',(-56.109682911022,-18.5643731068275,
39.8715976051449));
#173539=CARTESIAN_POINT('Ctrl Pts',(-56.1179479440989,-18.5670586829462,
39.8576902534424));
#173540=CARTESIAN_POINT('',(-56.4568070719812,-18.6771643191707,39.2875012672119));
#173541=CARTESIAN_POINT('',(-56.1179479440989,-18.5670586829462,39.8576902534424));
#173542=CARTESIAN_POINT('',(-54.4530463244694,-23.8971395307765,39.2875012672119));
#173543=CARTESIAN_POINT('Origin',(5.53234440788222E-15,0.,39.2875012672119));
#173544=CARTESIAN_POINT('',(-54.1275498658875,-23.7522229508825,39.8576902534424));
#173545=CARTESIAN_POINT('',(-54.4530463244694,-23.8971395307765,39.2875012672119));
#173546=CARTESIAN_POINT('',(-53.8330634946839,-23.9513722670362,40.1599502534424));
#173547=CARTESIAN_POINT('Ctrl Pts',(-54.1275498658875,-23.7522229508825,
39.8576902534424));
#173548=CARTESIAN_POINT('Ctrl Pts',(-54.1163771839516,-23.747248709103,
39.8772619994063));
#173549=CARTESIAN_POINT('Ctrl Pts',(-54.1044728027347,-23.7440527738934,
39.8967644650387));
#173550=CARTESIAN_POINT('Ctrl Pts',(-54.0920187959658,-23.7426340760171,
39.9159282836073));
#173551=CARTESIAN_POINT('Ctrl Pts',(-54.0793398243547,-23.7411897512764,
39.9354382707224));
#173552=CARTESIAN_POINT('Ctrl Pts',(-54.0660903588241,-23.7415870431746,
39.9545987622403));
#173553=CARTESIAN_POINT('Ctrl Pts',(-54.0524339053468,-23.7438697192145,
39.9731387498289));
#173554=CARTESIAN_POINT('Ctrl Pts',(-54.0393556307021,-23.7460557526693,
39.9908938024123));
#173555=CARTESIAN_POINT('Ctrl Pts',(-54.0259032350411,-23.7499709416813,
40.0080810366259));
#173556=CARTESIAN_POINT('Ctrl Pts',(-54.0122070876424,-23.7556964921025,
40.0244542742624));
#173557=CARTESIAN_POINT('Ctrl Pts',(-54.0013136223915,-23.7602504066262,
40.0374770090539));
#173558=CARTESIAN_POINT('Ctrl Pts',(-53.9902655788097,-23.7659503210025,
40.0499848770064));
#173559=CARTESIAN_POINT('Ctrl Pts',(-53.9791273029165,-23.7728578042868,
40.0618424270193));
#173560=CARTESIAN_POINT('Ctrl Pts',(-53.9790968990413,-23.7728766594724,
40.0618747942791));
#173561=CARTESIAN_POINT('Ctrl Pts',(-53.979066494666,-23.7728955237003,
40.0619071564124));
#173562=CARTESIAN_POINT('Ctrl Pts',(-53.9790360897925,-23.7729143969707,
40.0619395134162));
#173563=CARTESIAN_POINT('Ctrl Pts',(-53.9729834442088,-23.7766714662751,
40.0683807661799));
#173564=CARTESIAN_POINT('Ctrl Pts',(-53.966902706228,-23.7808224374041,
40.0746073439084));
#173565=CARTESIAN_POINT('Ctrl Pts',(-53.9608263568287,-23.7853431031261,
40.0805869293669));
#173566=CARTESIAN_POINT('Ctrl Pts',(-53.9487674206469,-23.794314677316,
40.092453830807));
#173567=CARTESIAN_POINT('Ctrl Pts',(-53.9367254523686,-23.8047436656398,
40.1033475319609));
#173568=CARTESIAN_POINT('Ctrl Pts',(-53.924952460372,-23.8164490335994,
40.1130129263075));
#173569=CARTESIAN_POINT('Ctrl Pts',(-53.9161227163745,-23.8252280595691,
40.1202619720674));
#173570=CARTESIAN_POINT('Ctrl Pts',(-53.9074442707905,-23.8347250487605,
40.1268200947266));
#173571=CARTESIAN_POINT('Ctrl Pts',(-53.8990234500734,-23.8448636317804,
40.1325796782703));
#173572=CARTESIAN_POINT('Ctrl Pts',(-53.8958656423045,-23.8486656004128,
40.1347395220992));
#173573=CARTESIAN_POINT('Ctrl Pts',(-53.8927440632083,-23.852557793254,
40.1367870714852));
#173574=CARTESIAN_POINT('Ctrl Pts',(-53.8896643205893,-23.8565361833377,
40.1387166518767));
#173575=CARTESIAN_POINT('Ctrl Pts',(-53.8788852214227,-23.8704605486309,
40.1454701832469));
#173576=CARTESIAN_POINT('Ctrl Pts',(-53.8686186144654,-23.8854408280736,
40.1507785912492));
#173577=CARTESIAN_POINT('Ctrl Pts',(-53.8591049768559,-23.9013043843658,
40.1543986087265));
#173578=CARTESIAN_POINT('Ctrl Pts',(-53.8543481580512,-23.9092361625119,
40.1562086174652));
#173579=CARTESIAN_POINT('Ctrl Pts',(-53.8497795825132,-23.9173887602869,
40.1575965292115));
#173580=CARTESIAN_POINT('Ctrl Pts',(-53.8454293138303,-23.9257405998158,
40.1585319382567));
#173581=CARTESIAN_POINT('Ctrl Pts',(-53.8432541794888,-23.9299165195802,
40.1589996427793));
#173582=CARTESIAN_POINT('Ctrl Pts',(-53.8411336218843,-23.9341422497938,
40.159354221642));
#173583=CARTESIAN_POINT('Ctrl Pts',(-53.8390713992305,-23.9384150933425,
40.1595918743111));
#173584=CARTESIAN_POINT('Ctrl Pts',(-53.8370091765767,-23.9426879368912,
40.1598295269801));
#173585=CARTESIAN_POINT('Ctrl Pts',(-53.8350052904264,-23.9470078944656,
40.1599502506896));
#173586=CARTESIAN_POINT('Ctrl Pts',(-53.8330634946839,-23.9513722670362,
40.1599502534424));
#173587=CARTESIAN_POINT('',(-53.8206887816837,-23.9791663275011,40.1599502534424));
#173588=CARTESIAN_POINT('Origin',(3.40248402231255E-16,-2.77126713209864E-17,
40.1599502534424));
#173589=CARTESIAN_POINT('',(-53.8697418420146,-24.3312692531085,39.8576902534424));
#173590=CARTESIAN_POINT('Ctrl Pts',(-53.8206887816837,-23.9791663275011,
40.1599502534424));
#173591=CARTESIAN_POINT('Ctrl Pts',(-53.8191382997273,-23.9826463618222,
40.1599502448875));
#173592=CARTESIAN_POINT('Ctrl Pts',(-53.817634996232,-23.9861360190793,
40.1598743450437));
#173593=CARTESIAN_POINT('Ctrl Pts',(-53.816178659515,-23.9896330908639,
40.1597243308499));
#173594=CARTESIAN_POINT('Ctrl Pts',(-53.8075805576699,-24.010279538222,
40.1588386583938));
#173595=CARTESIAN_POINT('Ctrl Pts',(-53.8006169491702,-24.0311861904791,
40.1553722553612));
#173596=CARTESIAN_POINT('Ctrl Pts',(-53.7952474622065,-24.0518926318839,
40.1496902177775));
#173597=CARTESIAN_POINT('Ctrl Pts',(-53.7932416006197,-24.0596278691038,
40.1475675976834));
#173598=CARTESIAN_POINT('Ctrl Pts',(-53.7914578533664,-24.0673353939229,
40.145136144309));
#173599=CARTESIAN_POINT('Ctrl Pts',(-53.7898929820049,-24.0749921329674,
40.1424159447501));
#173600=CARTESIAN_POINT('Ctrl Pts',(-53.7886719908666,-24.0809663048718,
40.1402935085949));
#173601=CARTESIAN_POINT('Ctrl Pts',(-53.7875846446508,-24.0869092410385,
40.1379949176048));
#173602=CARTESIAN_POINT('Ctrl Pts',(-53.78662979452,-24.092809656186,40.1355293609262));
#173603=CARTESIAN_POINT('Ctrl Pts',(-53.7832878190623,-24.1134611092024,
40.1268999125509));
#173604=CARTESIAN_POINT('Ctrl Pts',(-53.7815689125023,-24.1335916760299,
40.1162251288835));
#173605=CARTESIAN_POINT('Ctrl Pts',(-53.7814239018616,-24.1527175379841,
40.1038990521418));
#173606=CARTESIAN_POINT('Ctrl Pts',(-53.7813513965412,-24.1622804689613,
40.097736013771));
#173607=CARTESIAN_POINT('Ctrl Pts',(-53.7816723668479,-24.1715922244707,
40.0911601532641));
#173608=CARTESIAN_POINT('Ctrl Pts',(-53.7823806708182,-24.1805923292964,
40.0842207290641));
#173609=CARTESIAN_POINT('Ctrl Pts',(-53.7830859485794,-24.1895539814232,
40.0773109533619));
#173610=CARTESIAN_POINT('Ctrl Pts',(-53.7841750295932,-24.1982067474361,
40.0700409753048));
#173611=CARTESIAN_POINT('Ctrl Pts',(-53.7856425347026,-24.2064906018695,
40.0624586415899));
#173612=CARTESIAN_POINT('Ctrl Pts',(-53.7856488314803,-24.2065261462708,
40.0624261072769));
#173613=CARTESIAN_POINT('Ctrl Pts',(-53.7856551347355,-24.2065616841179,
40.0623935677889));
#173614=CARTESIAN_POINT('Ctrl Pts',(-53.7856614444665,-24.2065972154095,
40.0623610231288));
#173615=CARTESIAN_POINT('Ctrl Pts',(-53.7886369923274,-24.2233530895747,
40.0470135870235));
#173616=CARTESIAN_POINT('Ctrl Pts',(-53.7930196670706,-24.2386338146178,
40.0305755292097));
#173617=CARTESIAN_POINT('Ctrl Pts',(-53.7986158348076,-24.2524209582908,
40.0133447567345));
#173618=CARTESIAN_POINT('Ctrl Pts',(-53.8044155801157,-24.2667096511226,
39.9954871626604));
#173619=CARTESIAN_POINT('Ctrl Pts',(-53.8115193533079,-24.2793947083673,
39.9767767954325));
#173620=CARTESIAN_POINT('Ctrl Pts',(-53.8197464933872,-24.2904167802934,
39.9575197577489));
#173621=CARTESIAN_POINT('Ctrl Pts',(-53.8278562137176,-24.3012815425221,
39.9385375612015));
#173622=CARTESIAN_POINT('Ctrl Pts',(-53.8370583385436,-24.3105307527857,
39.9190226977117));
#173623=CARTESIAN_POINT('Ctrl Pts',(-53.8472012967764,-24.3180642992198,
39.8992655451882));
#173624=CARTESIAN_POINT('Ctrl Pts',(-53.8542731477173,-24.3233168218288,
39.8854905069344));
#173625=CARTESIAN_POINT('Ctrl Pts',(-53.8618028047964,-24.3277344576494,
39.8715976051484));
#173626=CARTESIAN_POINT('Ctrl Pts',(-53.8697418420146,-24.3312692531085,
39.8576902534424));
#173627=CARTESIAN_POINT('',(-54.1952354911873,-24.4761921430389,39.2875012672119));
#173628=CARTESIAN_POINT('',(-53.8697418420146,-24.3312692531085,39.8576902534424));
#173629=CARTESIAN_POINT('',(-51.6568155675429,-29.4581217525671,39.2875012672119));
#173630=CARTESIAN_POINT('Origin',(5.53234440788222E-15,0.,39.2875012672119));
#173631=CARTESIAN_POINT('',(-51.3482501200167,-29.279975396246,39.8576902534424));
#173632=CARTESIAN_POINT('',(-51.6568155675429,-29.4581217525671,39.2875012672119));
#173633=CARTESIAN_POINT('',(-51.0345602039888,-29.4472515437732,40.1599502534424));
#173634=CARTESIAN_POINT('Ctrl Pts',(-51.3482501200167,-29.2799753962459,
39.8576902534424));
#173635=CARTESIAN_POINT('Ctrl Pts',(-51.3376585930521,-29.2738605406108,
39.8772619994035));
#173636=CARTESIAN_POINT('Ctrl Pts',(-51.326153491479,-29.2694377663943,
39.8967644650332));
#173637=CARTESIAN_POINT('Ctrl Pts',(-51.3139160033731,-29.2667250421043,
39.9159282835992));
#173638=CARTESIAN_POINT('Ctrl Pts',(-51.3014574615426,-29.2639633161072,
39.9354382707117));
#173639=CARTESIAN_POINT('Ctrl Pts',(-51.288239049661,-29.2629734853272,
39.9545987622272));
#173640=CARTESIAN_POINT('Ctrl Pts',(-51.2744188030484,-29.2638161685322,
39.9731387498136));
#173641=CARTESIAN_POINT('Ctrl Pts',(-51.2611836698449,-29.2646231747151,
39.9908938023951));
#173642=CARTESIAN_POINT('Ctrl Pts',(-51.2473957191261,-29.2671107576648,
40.0080810366069));
#173643=CARTESIAN_POINT('Ctrl Pts',(-51.2331761176712,-29.2713733056795,
40.024454274242));
#173644=CARTESIAN_POINT('Ctrl Pts',(-51.2218663142702,-29.2747635962011,
40.0374770090408));
#173645=CARTESIAN_POINT('Ctrl Pts',(-51.2102829897306,-29.2792774508342,
40.0499848770002));
#173646=CARTESIAN_POINT('Ctrl Pts',(-51.1984837018592,-29.2849828273427,
40.0618424270193));
#173647=CARTESIAN_POINT('Ctrl Pts',(-51.1984514936361,-29.2849984011672,
40.0618747942791));
#173648=CARTESIAN_POINT('Ctrl Pts',(-51.1984192839704,-29.2850139839323,
40.0619071564124));
#173649=CARTESIAN_POINT('Ctrl Pts',(-51.198387072864,-29.2850295756383,
40.0619395134161));
#173650=CARTESIAN_POINT('Ctrl Pts',(-51.1919748636254,-29.2881333895824,
40.0683807661799));
#173651=CARTESIAN_POINT('Ctrl Pts',(-51.1854935419303,-29.2916260110605,
40.0746073439084));
#173652=CARTESIAN_POINT('Ctrl Pts',(-51.1789779411679,-29.2954867606376,
40.0805869293669));
#173653=CARTESIAN_POINT('Ctrl Pts',(-51.1660472802371,-29.3031486855377,
40.092453830807));
#173654=CARTESIAN_POINT('Ctrl Pts',(-51.152981152998,-29.3122618143334,
40.1033475319609));
#173655=CARTESIAN_POINT('Ctrl Pts',(-51.1400491105586,-29.3226724463011,
40.1130129263075));
#173656=CARTESIAN_POINT('Ctrl Pts',(-51.1303500787291,-29.3304804202768,
40.1202619720674));
#173657=CARTESIAN_POINT('Ctrl Pts',(-51.1207264688922,-29.3390182393874,
40.1268200947266));
#173658=CARTESIAN_POINT('Ctrl Pts',(-51.1112920078093,-29.3482210667396,
40.1325796782703));
#173659=CARTESIAN_POINT('Ctrl Pts',(-51.1077540849032,-29.3516721269967,
40.1347395220992));
#173660=CARTESIAN_POINT('Ctrl Pts',(-51.1042427612074,-29.3552167041323,
40.1367870714852));
#173661=CARTESIAN_POINT('Ctrl Pts',(-51.100764034739,-29.3588513794157,
40.1387166518767));
#173662=CARTESIAN_POINT('Ctrl Pts',(-51.0885884920994,-29.3715727429076,
40.1454701832469));
#173663=CARTESIAN_POINT('Ctrl Pts',(-51.0768122610998,-29.3853978061639,
40.1507785912492));
#173664=CARTESIAN_POINT('Ctrl Pts',(-51.0656925470314,-29.4001800143155,
40.1543986087265));
#173665=CARTESIAN_POINT('Ctrl Pts',(-51.0601326899972,-29.4075711183913,
40.1562086174652));
#173666=CARTESIAN_POINT('Ctrl Pts',(-51.0547369630769,-29.4152015092023,
40.1575965292115));
#173667=CARTESIAN_POINT('Ctrl Pts',(-51.0495375206696,-29.4230528695802,
40.1585319382567));
#173668=CARTESIAN_POINT('Ctrl Pts',(-51.046937799466,-29.4269785497691,
40.1589996427793));
#173669=CARTESIAN_POINT('Ctrl Pts',(-51.0443871494124,-29.4309594723628,
40.159354221642));
#173670=CARTESIAN_POINT('Ctrl Pts',(-51.0418895900602,-29.4349933478625,
40.159591874311));
#173671=CARTESIAN_POINT('Ctrl Pts',(-51.039392030708,-29.4390272233622,
40.1598295269801));
#173672=CARTESIAN_POINT('Ctrl Pts',(-51.0369475635291,-29.4431140526173,
40.1599502506895));
#173673=CARTESIAN_POINT('Ctrl Pts',(-51.0345602039888,-29.4472515437732,
40.1599502534424));
#173674=CARTESIAN_POINT('',(-51.0193480105329,-29.4735998357335,40.1599502534424));
#173675=CARTESIAN_POINT('Origin',(3.434861425631E-16,-3.40670945103686E-17,
40.1599502534424));
#173676=CARTESIAN_POINT('',(-51.031327575341,-29.8289013456883,39.8576902534424));
#173677=CARTESIAN_POINT('Ctrl Pts',(-51.0193480105329,-29.4735998357335,
40.1599502534424));
#173678=CARTESIAN_POINT('Ctrl Pts',(-51.0174422596392,-29.4768987365662,
40.1599502448875));
#173679=CARTESIAN_POINT('Ctrl Pts',(-51.0155824228873,-29.4802121391116,
40.1598743450437));
#173680=CARTESIAN_POINT('Ctrl Pts',(-51.0137685205956,-29.483537824932,
40.1597243308499));
#173681=CARTESIAN_POINT('Ctrl Pts',(-51.0030593786376,-29.5031724225186,
40.1588386583938));
#173682=CARTESIAN_POINT('Ctrl Pts',(-50.9939485772813,-29.5232366506522,
40.1553722553611));
#173683=CARTESIAN_POINT('Ctrl Pts',(-50.9864440924291,-29.5432683957839,
40.1496902177772));
#173684=CARTESIAN_POINT('Ctrl Pts',(-50.9836406667025,-29.5507515889354,
40.1475675976832));
#173685=CARTESIAN_POINT('Ctrl Pts',(-50.9810610352785,-29.5582304387676,
40.1451361443089));
#173686=CARTESIAN_POINT('Ctrl Pts',(-50.9787043892801,-29.5656816597956,
40.1424159447501));
#173687=CARTESIAN_POINT('Ctrl Pts',(-50.9768656158505,-29.5714954762339,
40.1402935085949));
#173688=CARTESIAN_POINT('Ctrl Pts',(-50.9751630202463,-29.5772921977454,
40.1379949176048));
#173689=CARTESIAN_POINT('Ctrl Pts',(-50.9735966395564,-29.5830604807846,
40.1355293609261));
#173690=CARTESIAN_POINT('Ctrl Pts',(-50.9681143071419,-29.6032494714217,
40.1268999125509));
#173691=CARTESIAN_POINT('Ctrl Pts',(-50.9643005997168,-29.6230900862365,
40.1162251288835));
#173692=CARTESIAN_POINT('Ctrl Pts',(-50.9621571865007,-29.6420960169784,
40.1038990521418));
#173693=CARTESIAN_POINT('Ctrl Pts',(-50.9610854798927,-29.6515989823493,
40.0977360137709));
#173694=CARTESIAN_POINT('Ctrl Pts',(-50.9604313483968,-29.6608932776207,
40.0911601532641));
#173695=CARTESIAN_POINT('Ctrl Pts',(-50.9601950050771,-29.669918116856,
40.084220729064));
#173696=CARTESIAN_POINT('Ctrl Pts',(-50.9599596715278,-29.6789043977153,
40.0773109533619));
#173697=CARTESIAN_POINT('Ctrl Pts',(-50.9601383261075,-29.6876236029354,
40.0700409753048));
#173698=CARTESIAN_POINT('Ctrl Pts',(-50.9607318934965,-29.6960154736014,
40.0624586415899));
#173699=CARTESIAN_POINT('Ctrl Pts',(-50.9607344403782,-29.6960514814793,
40.0624261072769));
#173700=CARTESIAN_POINT('Ctrl Pts',(-50.960736994387,-29.6960874835159,
40.0623935677889));
#173701=CARTESIAN_POINT('Ctrl Pts',(-50.9607395555213,-29.6961234797099,
40.0623610231289));
#173702=CARTESIAN_POINT('Ctrl Pts',(-50.9619473372424,-29.7130985928884,
40.0470135870235));
#173703=CARTESIAN_POINT('Ctrl Pts',(-50.9647087325285,-29.7287537227769,
40.0305755292096));
#173704=CARTESIAN_POINT('Ctrl Pts',(-50.9688330949321,-29.743050297848,
40.0133447567344));
#173705=CARTESIAN_POINT('Ctrl Pts',(-50.9731074935248,-29.7578669541898,
39.9954871626603));
#173706=CARTESIAN_POINT('Ctrl Pts',(-50.9788464019639,-29.7712250678589,
39.9767767954323));
#173707=CARTESIAN_POINT('Ctrl Pts',(-50.9858763526686,-29.7830467300313,
39.9575197577486));
#173708=CARTESIAN_POINT('Ctrl Pts',(-50.992805970203,-29.7946996705593,
39.9385375612012));
#173709=CARTESIAN_POINT('Ctrl Pts',(-51.0009908790911,-29.8048600966482,
39.9190226977114));
#173710=CARTESIAN_POINT('Ctrl Pts',(-51.0102908031057,-29.8134126013638,
39.8992655451879));
#173711=CARTESIAN_POINT('Ctrl Pts',(-51.0167748755906,-29.8193755598155,
39.8854905069341));
#173712=CARTESIAN_POINT('Ctrl Pts',(-51.0238015157368,-29.8245560588483,
39.8715976051482));
#173713=CARTESIAN_POINT('Ctrl Pts',(-51.0313275753411,-29.8289013456882,
39.8576902534424));
#173714=CARTESIAN_POINT('',(-51.3398895692699,-30.0070536838155,39.2875012672119));
#173715=CARTESIAN_POINT('',(-51.031327575341,-29.8289013456883,39.8576902534424));
#173716=CARTESIAN_POINT('',(-48.2946219293748,-34.6963546279283,39.2875012672119));
#173717=CARTESIAN_POINT('Origin',(5.53234440788222E-15,0.,39.2875012672119));
#173718=CARTESIAN_POINT('',(-48.0063682005189,-34.4869303039394,39.8576902534424));
#173719=CARTESIAN_POINT('',(-48.2946219293748,-34.6963546279283,39.2875012672119));
#173720=CARTESIAN_POINT('',(-47.6769115920306,-34.6205005703632,40.1599502534424));
#173721=CARTESIAN_POINT('Ctrl Pts',(-48.0063682005189,-34.4869303039394,
39.8576902534424));
#173722=CARTESIAN_POINT('Ctrl Pts',(-47.9964738715087,-34.4797418300851,
39.8772619994058));
#173723=CARTESIAN_POINT('Ctrl Pts',(-47.9854941018767,-34.4741406737008,
39.8967644650379));
#173724=CARTESIAN_POINT('Ctrl Pts',(-47.9736072089107,-34.4701636441721,
39.9159282836061));
#173725=CARTESIAN_POINT('Ctrl Pts',(-47.9615055952487,-34.4661147749668,
39.9354382707209));
#173726=CARTESIAN_POINT('Ctrl Pts',(-47.9484630606988,-34.4637486663029,
39.9545987622386));
#173727=CARTESIAN_POINT('Ctrl Pts',(-47.9346304384606,-34.4631421240615,
39.9731387498271));
#173728=CARTESIAN_POINT('Ctrl Pts',(-47.9213834535833,-34.462561261246,
39.9908938024107));
#173729=CARTESIAN_POINT('Ctrl Pts',(-47.9074110114758,-34.463593983657,
40.0080810366245));
#173730=CARTESIAN_POINT('Ctrl Pts',(-47.8928237488894,-34.4663468279011,
40.0244542742612));
#173731=CARTESIAN_POINT('Ctrl Pts',(-47.8812215199217,-34.4685363496872,
40.0374770090531));
#173732=CARTESIAN_POINT('Ctrl Pts',(-47.8692298237635,-34.4718146898375,
40.049984877006));
#173733=CARTESIAN_POINT('Ctrl Pts',(-47.8568987993929,-34.4762554502655,
40.0618424270192));
#173734=CARTESIAN_POINT('Ctrl Pts',(-47.8568651397019,-34.476267572099,
40.0618747942791));
#173735=CARTESIAN_POINT('Ctrl Pts',(-47.8568314776416,-34.4762797026732,
40.0619071564124));
#173736=CARTESIAN_POINT('Ctrl Pts',(-47.8567978132139,-34.4762918419887,
40.0619395134162));
#173737=CARTESIAN_POINT('Ctrl Pts',(-47.8500962938266,-34.4787083945374,
40.0683807661799));
#173738=CARTESIAN_POINT('Ctrl Pts',(-47.843285399134,-34.4815044004729,
40.0746073439084));
#173739=CARTESIAN_POINT('Ctrl Pts',(-47.836401933294,-34.4846629347249,
40.0805869293669));
#173740=CARTESIAN_POINT('Ctrl Pts',(-47.8227412186412,-34.4909312646827,
40.092453830807));
#173741=CARTESIAN_POINT('Ctrl Pts',(-47.8087940876657,-34.4986286886041,
40.1033475319609));
#173742=CARTESIAN_POINT('Ctrl Pts',(-47.7948446809467,-34.5076305235174,
40.1130129263075));
#173743=CARTESIAN_POINT('Ctrl Pts',(-47.7843826259074,-34.5143818997025,
40.1202619720674));
#173744=CARTESIAN_POINT('Ctrl Pts',(-47.7739192901009,-34.5218670065993,
40.1268200947266));
#173745=CARTESIAN_POINT('Ctrl Pts',(-47.763574554582,-34.5300332501816,
40.1325796782703));
#173746=CARTESIAN_POINT('Ctrl Pts',(-47.7596952787625,-34.533095591525,
40.1347395220992));
#173747=CARTESIAN_POINT('Ctrl Pts',(-47.7558326812644,-34.5362537178262,
40.1367870714852));
#173748=CARTESIAN_POINT('Ctrl Pts',(-47.7519930846017,-34.5395048560462,
40.1387166518767));
#173749=CARTESIAN_POINT('Ctrl Pts',(-47.7385544962822,-34.5508838398163,
40.1454701832469));
#173750=CARTESIAN_POINT('Ctrl Pts',(-47.7253976640914,-34.5634022166001,
40.1507785912492));
#173751=CARTESIAN_POINT('Ctrl Pts',(-47.7127937034783,-34.5769411196452,
40.1543986087265));
#173752=CARTESIAN_POINT('Ctrl Pts',(-47.7064917231718,-34.5837105711677,
40.1562086174652));
#173753=CARTESIAN_POINT('Ctrl Pts',(-47.7003279615826,-34.5907351548563,
40.1575965292115));
#173754=CARTESIAN_POINT('Ctrl Pts',(-47.69433631163,-34.5980000149358,40.1585319382567));
#173755=CARTESIAN_POINT('Ctrl Pts',(-47.6913404866536,-34.6016324449756,
40.1589996427793));
#173756=CARTESIAN_POINT('Ctrl Pts',(-47.6883876896069,-34.6053249441283,
40.159354221642));
#173757=CARTESIAN_POINT('Ctrl Pts',(-47.6854821573391,-34.609075655595,
40.159591874311));
#173758=CARTESIAN_POINT('Ctrl Pts',(-47.6825766250713,-34.6128263670616,
40.1598295269801));
#173759=CARTESIAN_POINT('Ctrl Pts',(-47.6797183589577,-34.6166352918407,
40.1599502506896));
#173760=CARTESIAN_POINT('Ctrl Pts',(-47.6769115920305,-34.6205005703632,
40.1599502534424));
#173761=CARTESIAN_POINT('',(-47.6590285860937,-34.6451144164183,40.1599502534424));
#173762=CARTESIAN_POINT('Origin',(3.4737036430558E-16,-4.00482714832972E-17,
40.1599502534424));
#173763=CARTESIAN_POINT('',(-47.6338034047601,-34.9997217530258,39.8576902534424));
#173764=CARTESIAN_POINT('Ctrl Pts',(-47.6590285860937,-34.6451144164183,
40.1599502534424));
#173765=CARTESIAN_POINT('Ctrl Pts',(-47.6567884460683,-34.6481960403149,
40.1599502448875));
#173766=CARTESIAN_POINT('Ctrl Pts',(-47.6545924528205,-34.6512968858168,
40.1598743450437));
#173767=CARTESIAN_POINT('Ctrl Pts',(-47.6524408584472,-34.6544147487632,
40.1597243308499));
#173768=CARTESIAN_POINT('Ctrl Pts',(-47.6397380079794,-34.6728223758142,
40.1588386583939));
#173769=CARTESIAN_POINT('Ctrl Pts',(-47.6285798336148,-34.6918243519377,
40.1553722553626));
#173770=CARTESIAN_POINT('Ctrl Pts',(-47.619022571582,-34.7109619288003,
40.1496902177808));
#173771=CARTESIAN_POINT('Ctrl Pts',(-47.6154522966321,-34.7181110904577,
40.1475675976859));
#173772=CARTESIAN_POINT('Ctrl Pts',(-47.6121050440169,-34.7252793254635,
40.1451361443104));
#173773=CARTESIAN_POINT('Ctrl Pts',(-47.6089824432867,-34.7324433913424,
40.1424159447501));
#173774=CARTESIAN_POINT('Ctrl Pts',(-47.6065460335523,-34.738033154925,
40.1402935085949));
#173775=CARTESIAN_POINT('Ctrl Pts',(-47.6042468425534,-34.7436201516875,
40.1379949176048));
#173776=CARTESIAN_POINT('Ctrl Pts',(-47.602086092899,-34.7491931041022,
40.1355293609261));
#173777=CARTESIAN_POINT('Ctrl Pts',(-47.5945234691089,-34.7686984375538,
40.1268999125509));
#173778=CARTESIAN_POINT('Ctrl Pts',(-47.5886567445952,-34.7880317224282,
40.1162251288835));
#173779=CARTESIAN_POINT('Ctrl Pts',(-47.5845384124876,-34.8067094890032,
40.1038990521418));
#173780=CARTESIAN_POINT('Ctrl Pts',(-47.5824792464338,-34.8160483722907,
40.097736013771));
#173781=CARTESIAN_POINT('Ctrl Pts',(-47.5808571799368,-34.8252233770801,
40.0911601532641));
#173782=CARTESIAN_POINT('Ctrl Pts',(-47.5796787787541,-34.8341740726978,
40.0842207290641));
#173783=CARTESIAN_POINT('Ctrl Pts',(-47.5785054122578,-34.8430865267161,
40.0773109533619));
#173784=CARTESIAN_POINT('Ctrl Pts',(-47.5777716830264,-34.8517766417063,
40.0700409753048));
#173785=CARTESIAN_POINT('Ctrl Pts',(-47.5774848094465,-34.8601845855137,
40.0624586415899));
#173786=CARTESIAN_POINT('Ctrl Pts',(-47.577483578528,-34.8602206623583,
40.0624261072769));
#173787=CARTESIAN_POINT('Ctrl Pts',(-47.5774823553081,-34.8602567341386,
40.0623935677888));
#173788=CARTESIAN_POINT('Ctrl Pts',(-47.5774811397854,-34.8602928008531,
40.0623610231288));
#173789=CARTESIAN_POINT('Ctrl Pts',(-47.5769079226575,-34.8773011701534,
40.047013587023));
#173790=CARTESIAN_POINT('Ctrl Pts',(-47.5780177840619,-34.8931591840084,
40.0305755292085));
#173791=CARTESIAN_POINT('Ctrl Pts',(-47.5806251537548,-34.9078085542098,
40.0133447567327));
#173792=CARTESIAN_POINT('Ctrl Pts',(-47.5833273744267,-34.9229908396747,
39.9954871626579));
#173793=CARTESIAN_POINT('Ctrl Pts',(-47.5876385414313,-34.9368756554797,
39.9767767954292));
#173794=CARTESIAN_POINT('Ctrl Pts',(-47.5933942811507,-34.949367387294,
39.9575197577448));
#173795=CARTESIAN_POINT('Ctrl Pts',(-47.5990678735498,-34.9616808340667,
39.9385375611966));
#173796=CARTESIAN_POINT('Ctrl Pts',(-47.6061458909259,-34.9726411562266,
39.9190226977059));
#173797=CARTESIAN_POINT('Ctrl Pts',(-47.6145008888092,-34.9821189161924,
39.8992655451816));
#173798=CARTESIAN_POINT('Ctrl Pts',(-47.6203261419824,-34.9887269790652,
39.8854905069299));
#173799=CARTESIAN_POINT('Ctrl Pts',(-47.6267727798548,-34.9946135826776,
39.8715976051461));
#173800=CARTESIAN_POINT('Ctrl Pts',(-47.6338034047601,-34.9997217530258,
39.8576902534424));
#173801=CARTESIAN_POINT('',(-47.9220530736689,-35.2091516650525,39.2875012672119));
#173802=CARTESIAN_POINT('',(-47.6338034047601,-34.9997217530258,39.8576902534424));
#173803=CARTESIAN_POINT('',(-44.4033023070491,-39.5544469813068,39.2875012672119));
#173804=CARTESIAN_POINT('Origin',(5.53234440788222E-15,0.,39.2875012672119));
#173805=CARTESIAN_POINT('',(-44.1385184650378,-39.3160391863688,39.8576902534424));
#173806=CARTESIAN_POINT('',(-44.4033023070491,-39.5544469813068,39.2875012672119));
#173807=CARTESIAN_POINT('',(-43.7969047596348,-39.4144401478987,40.1599502534424));
#173808=CARTESIAN_POINT('Ctrl Pts',(-44.1385184650378,-39.3160391863687,
39.8576902534424));
#173809=CARTESIAN_POINT('Ctrl Pts',(-44.1294297383233,-39.3078558527208,
39.8772619994037));
#173810=CARTESIAN_POINT('Ctrl Pts',(-44.1190955972887,-39.3011376816112,
39.8967644650337));
#173811=CARTESIAN_POINT('Ctrl Pts',(-44.1076895347526,-39.2959399200119,
39.9159282835999));
#173812=CARTESIAN_POINT('Ctrl Pts',(-44.096077437074,-39.2906482678568,
39.9354382707126));
#173813=CARTESIAN_POINT('Ctrl Pts',(-44.0833536765974,-39.2869318048901,
39.9545987622283));
#173814=CARTESIAN_POINT('Ctrl Pts',(-44.0696602318415,-39.2848826826045,
39.9731387498149));
#173815=CARTESIAN_POINT('Ctrl Pts',(-44.0565465320329,-39.2829203148436,
39.9908938023966));
#173816=CARTESIAN_POINT('Ctrl Pts',(-44.042542683541,-39.2824868619907,
40.0080810366086));
#173817=CARTESIAN_POINT('Ctrl Pts',(-44.0277475809293,-39.2836998417232,
40.0244542742438));
#173818=CARTESIAN_POINT('Ctrl Pts',(-44.0159800428336,-39.2846646059149,
40.037477009042));
#173819=CARTESIAN_POINT('Ctrl Pts',(-44.0037113585784,-39.2866715134039,
40.0499848770007));
#173820=CARTESIAN_POINT('Ctrl Pts',(-43.9909836989806,-39.289799003855,
40.0618424270193));
#173821=CARTESIAN_POINT('Ctrl Pts',(-43.9909489566042,-39.289807540888,
40.0618747942791));
#173822=CARTESIAN_POINT('Ctrl Pts',(-43.990914210958,-39.2898160863662,
40.0619071564124));
#173823=CARTESIAN_POINT('Ctrl Pts',(-43.9908794620435,-39.2898246402904,
40.0619395134161));
#173824=CARTESIAN_POINT('Ctrl Pts',(-43.9839620557563,-39.2915274551883,
40.0683807661799));
#173825=CARTESIAN_POINT('Ctrl Pts',(-43.9768962096537,-39.293596211955,
40.0746073439084));
#173826=CARTESIAN_POINT('Ctrl Pts',(-43.9697202954283,-39.2960179253197,
40.0805869293669));
#173827=CARTESIAN_POINT('Ctrl Pts',(-43.955479196702,-39.3008239832003,
40.092453830807));
#173828=CARTESIAN_POINT('Ctrl Pts',(-43.9408038696757,-39.3070213676602,
40.1033475319609));
#173829=CARTESIAN_POINT('Ctrl Pts',(-43.9259899312961,-39.3145157795322,
40.1130129263075));
#173830=CARTESIAN_POINT('Ctrl Pts',(-43.9148794775114,-39.3201365884362,
40.1202619720674));
#173831=CARTESIAN_POINT('Ctrl Pts',(-43.9036910542319,-39.3264869747217,
40.1268200947266));
#173832=CARTESIAN_POINT('Ctrl Pts',(-43.8925493833643,-39.3335271634606,
40.1325796782703));
#173833=CARTESIAN_POINT('Ctrl Pts',(-43.888371256789,-39.3361672342377,
40.1347395220992));
#173834=CARTESIAN_POINT('Ctrl Pts',(-43.8841997049151,-39.3389043086119,
40.1367870714852));
#173835=CARTESIAN_POINT('Ctrl Pts',(-43.8800413054826,-39.3417362896178,
40.1387166518767));
#173836=CARTESIAN_POINT('Ctrl Pts',(-43.865486907469,-39.3516482231386,
40.1454701832469));
#173837=CARTESIAN_POINT('Ctrl Pts',(-43.8510936230937,-39.3627227594942,
40.1507785912492));
#173838=CARTESIAN_POINT('Ctrl Pts',(-43.8371435075661,-39.3748700223779,
40.1543986087265));
#173839=CARTESIAN_POINT('Ctrl Pts',(-43.8301684498022,-39.3809436538197,
40.1562086174652));
#173840=CARTESIAN_POINT('Ctrl Pts',(-43.8233041850059,-39.387285467577,
40.1575965292115));
#173841=CARTESIAN_POINT('Ctrl Pts',(-43.8165859732786,-39.3938842320308,
40.1585319382567));
#173842=CARTESIAN_POINT('Ctrl Pts',(-43.813226867415,-39.3971836142578,
40.1589996427793));
#173843=CARTESIAN_POINT('Ctrl Pts',(-43.8099042748374,-39.4005472341762,
40.159354221642));
#173844=CARTESIAN_POINT('Ctrl Pts',(-43.8066226032736,-39.4039736880301,
40.159591874311));
#173845=CARTESIAN_POINT('Ctrl Pts',(-43.8033409317098,-39.4074001418839,
40.1598295269801));
#173846=CARTESIAN_POINT('Ctrl Pts',(-43.8001001824232,-39.4108894308101,
40.1599502506895));
#173847=CARTESIAN_POINT('Ctrl Pts',(-43.7969047596348,-39.4144401478987,
40.1599502534424));
#173848=CARTESIAN_POINT('',(-43.7765468711724,-39.4370498736006,40.1599502534424));
#173849=CARTESIAN_POINT('Origin',(3.51858511112454E-16,-4.55906712132145E-17,
40.1599502534424));
#173850=CARTESIAN_POINT('',(-43.7143933160625,-39.7870778846745,39.8576902534424));
#173851=CARTESIAN_POINT('Ctrl Pts',(-43.7765468711724,-39.4370498736006,
40.1599502534424));
#173852=CARTESIAN_POINT('Ctrl Pts',(-43.7739968854581,-39.4398804576446,
40.1599502448875));
#173853=CARTESIAN_POINT('Ctrl Pts',(-43.771488795476,-39.4427347725909,
40.1598743450437));
#173854=CARTESIAN_POINT('Ctrl Pts',(-43.7690230823394,-39.4456106527045,
40.1597243308499));
#173855=CARTESIAN_POINT('Ctrl Pts',(-43.7544656984485,-39.4625896314089,
40.158838658394));
#173856=CARTESIAN_POINT('Ctrl Pts',(-43.7413824023679,-39.4803211658986,
40.155372255363));
#173857=CARTESIAN_POINT('Ctrl Pts',(-43.7298770745169,-39.4983548991982,
40.1496902177819));
#173858=CARTESIAN_POINT('Ctrl Pts',(-43.7255790670243,-39.5050917016472,
40.1475675976867));
#173859=CARTESIAN_POINT('Ctrl Pts',(-43.721500866419,-39.5118707851407,
40.1451361443109));
#173860=CARTESIAN_POINT('Ctrl Pts',(-43.7176465228246,-39.5186692048625,
40.1424159447501));
#173861=CARTESIAN_POINT('Ctrl Pts',(-43.7146391706004,-39.5239736729699,
40.1402935085949));
#173862=CARTESIAN_POINT('Ctrl Pts',(-43.7117685746243,-39.5292897326777,
40.1379949176048));
#173863=CARTESIAN_POINT('Ctrl Pts',(-43.7090371296309,-39.5346062960351,
40.1355293609261));
#173864=CARTESIAN_POINT('Ctrl Pts',(-43.699477072154,-39.5532142677861,
40.1268999125509));
#173865=CARTESIAN_POINT('Ctrl Pts',(-43.6916216076132,-39.5718284032053,
40.1162251288835));
#173866=CARTESIAN_POINT('Ctrl Pts',(-43.6855734779224,-39.5899733680943,
40.1038990521418));
#173867=CARTESIAN_POINT('Ctrl Pts',(-43.682549413077,-39.5990458505388,
40.097736013771));
#173868=CARTESIAN_POINT('Ctrl Pts',(-43.6799771832789,-39.6080010415737,
40.0911601532641));
#173869=CARTESIAN_POINT('Ctrl Pts',(-43.677869635043,-39.6167795278795,
40.084220729064));
#173870=CARTESIAN_POINT('Ctrl Pts',(-43.6757710912487,-39.6255205083455,
40.0773109533619));
#173871=CARTESIAN_POINT('Ctrl Pts',(-43.6741330170974,-39.6340863223875,
40.0700409753048));
#173872=CARTESIAN_POINT('Ctrl Pts',(-43.6729688455955,-39.6424182201445,
40.0624586415899));
#173873=CARTESIAN_POINT('Ctrl Pts',(-43.672963850363,-39.6424539706904,
40.0624261072769));
#173874=CARTESIAN_POINT('Ctrl Pts',(-43.6729588633162,-39.6424897170044,
40.0623935677889));
#173875=CARTESIAN_POINT('Ctrl Pts',(-43.6729538844541,-39.6425254590849,
40.0623610231289));
#173876=CARTESIAN_POINT('Ctrl Pts',(-43.6706059487639,-39.6593807372529,
40.0470135870232));
#173877=CARTESIAN_POINT('Ctrl Pts',(-43.6700521164126,-39.6752678913557,
40.0305755292089));
#173878=CARTESIAN_POINT('Ctrl Pts',(-43.6711139265064,-39.6901095551213,
40.0133447567333));
#173879=CARTESIAN_POINT('Ctrl Pts',(-43.6722143631621,-39.7054911294118,
39.995487162659));
#173880=CARTESIAN_POINT('Ctrl Pts',(-43.6750505546837,-39.7197505224047,
39.9767767954308));
#173881=CARTESIAN_POINT('Ctrl Pts',(-43.6794690223284,-39.7327754618328,
39.9575197577469));
#173882=CARTESIAN_POINT('Ctrl Pts',(-43.6838244285256,-39.74561450615,39.9385375611994));
#173883=CARTESIAN_POINT('Ctrl Pts',(-43.6897180061492,-39.7572546407973,
39.9190226977096));
#173884=CARTESIAN_POINT('Ctrl Pts',(-43.6970365387951,-39.7675538156914,
39.899265545186));
#173885=CARTESIAN_POINT('Ctrl Pts',(-43.7021391499651,-39.7747345836676,
39.8854905069329));
#173886=CARTESIAN_POINT('Ctrl Pts',(-43.7079351548518,-39.7812627970003,
39.8715976051476));
#173887=CARTESIAN_POINT('Ctrl Pts',(-43.7143933160625,-39.7870778846745,
39.8576902534424));
#173888=CARTESIAN_POINT('',(-43.9791725362585,-40.0254908126586,39.2875012672119));
#173889=CARTESIAN_POINT('',(-43.7143933160625,-39.7870778846745,39.8576902534424));
#173890=CARTESIAN_POINT('',(-40.025490812659,-43.9791725362581,39.2875012672119));
#173891=CARTESIAN_POINT('Origin',(5.53234440788222E-15,0.,39.2875012672119));
#173892=CARTESIAN_POINT('',(-39.7870778846749,-43.7143933160621,39.8576902534424));
#173893=CARTESIAN_POINT('',(-40.025490812659,-43.9791725362581,39.2875012672119));
#173894=CARTESIAN_POINT('',(-39.437049873601,-43.776546871172,40.1599502534424));
#173895=CARTESIAN_POINT('Ctrl Pts',(-39.7870778846749,-43.7143933160621,
39.8576902534424));
#173896=CARTESIAN_POINT('Ctrl Pts',(-39.778894338246,-43.7053047809342,
39.8772619994065));
#173897=CARTESIAN_POINT('Ctrl Pts',(-39.7693190488178,-43.6975432007863,
39.8967644650393));
#173898=CARTESIAN_POINT('Ctrl Pts',(-39.7585187839162,-43.6911816548796,
39.9159282836082));
#173899=CARTESIAN_POINT('Ctrl Pts',(-39.7475234267896,-43.6847051962224,
39.9354382707237));
#173900=CARTESIAN_POINT('Ctrl Pts',(-39.7352578445645,-43.6796790972989,
39.9545987622422));
#173901=CARTESIAN_POINT('Ctrl Pts',(-39.7218536055326,-43.6762098455828,
39.9731387498312));
#173902=CARTESIAN_POINT('Ctrl Pts',(-39.7090168672273,-43.6728874729895,
39.9908938024155));
#173903=CARTESIAN_POINT('Ctrl Pts',(-39.69513504144,-43.6709925938748,40.0080810366299));
#173904=CARTESIAN_POINT('Ctrl Pts',(-39.6802941970377,-43.670652419439,
40.0244542742671));
#173905=CARTESIAN_POINT('Ctrl Pts',(-39.6684902774348,-43.6703818558793,
40.0374770090569));
#173906=CARTESIAN_POINT('Ctrl Pts',(-39.6560790233668,-43.6710953426078,
40.0499848770078));
#173907=CARTESIAN_POINT('Ctrl Pts',(-39.643094175457,-43.6728752976392,
40.0618424270193));
#173908=CARTESIAN_POINT('Ctrl Pts',(-39.6430587310401,-43.6728801563383,
40.0618747942791));
#173909=CARTESIAN_POINT('Ctrl Pts',(-39.6430232824884,-43.6728850230944,
40.0619071564124));
#173910=CARTESIAN_POINT('Ctrl Pts',(-39.6429878298037,-43.6728898979087,
40.0619395134161));
#173911=CARTESIAN_POINT('Ctrl Pts',(-39.6359303251673,-43.6738603187594,
40.0683807661799));
#173912=CARTESIAN_POINT('Ctrl Pts',(-39.6286869425433,-43.6751791606253,
40.0746073439084));
#173913=CARTESIAN_POINT('Ctrl Pts',(-39.6212972007503,-43.6768375203043,
40.0805869293669));
#173914=CARTESIAN_POINT('Ctrl Pts',(-39.6066317464083,-43.6801286499318,
40.092453830807));
#173915=CARTESIAN_POINT('Ctrl Pts',(-39.5913890092851,-43.6847580950892,
40.1033475319609));
#173916=CARTESIAN_POINT('Ctrl Pts',(-39.5758728438539,-43.6906629735751,
40.1130129263075));
#173917=CARTESIAN_POINT('Ctrl Pts',(-39.5642357197805,-43.6950916324395,
40.1202619720674));
#173918=CARTESIAN_POINT('Ctrl Pts',(-39.5524447917348,-43.7002377219526,
40.1268200947266));
#173919=CARTESIAN_POINT('Ctrl Pts',(-39.540628255996,-43.706074722067,40.1325796782703));
#173920=CARTESIAN_POINT('Ctrl Pts',(-39.5361970550939,-43.7082635971098,
40.1347395220992));
#173921=CARTESIAN_POINT('Ctrl Pts',(-39.5317622532395,-43.7105496315974,
40.1367870714852));
#173922=CARTESIAN_POINT('Ctrl Pts',(-39.5273306113316,-43.7129314276128,
40.1387166518767));
#173923=CARTESIAN_POINT('Ctrl Pts',(-39.5118198646542,-43.7212677136665,
40.1454701832469));
#173924=CARTESIAN_POINT('Ctrl Pts',(-39.4963478239301,-43.7307770746561,
40.1507785912492));
#173925=CARTESIAN_POINT('Ctrl Pts',(-39.4812043938728,-43.7413996094241,
40.1543986087265));
#173926=CARTESIAN_POINT('Ctrl Pts',(-39.4736326788442,-43.7467108768082,
40.1562086174652));
#173927=CARTESIAN_POINT('Ctrl Pts',(-39.4661431171622,-43.7523004383955,
40.1575965292115));
#173928=CARTESIAN_POINT('Ctrl Pts',(-39.4587719497939,-43.7581608097795,
40.1585319382567));
#173929=CARTESIAN_POINT('Ctrl Pts',(-39.4550863661098,-43.7610909954715,
40.1589996427793));
#173930=CARTESIAN_POINT('Ctrl Pts',(-39.4514303810208,-43.7640888836318,
40.159354221642));
#173931=CARTESIAN_POINT('Ctrl Pts',(-39.4478085248414,-43.7671535389275,
40.159591874311));
#173932=CARTESIAN_POINT('Ctrl Pts',(-39.4441866686621,-43.7702181942231,
40.1598295269801));
#173933=CARTESIAN_POINT('Ctrl Pts',(-39.4405989425298,-43.7733496179167,
40.1599502506895));
#173934=CARTESIAN_POINT('Ctrl Pts',(-39.437049873601,-43.776546871172,40.1599502534424));
#173935=CARTESIAN_POINT('',(-39.4144401478992,-43.7969047596345,40.1599502534424));
#173936=CARTESIAN_POINT('Origin',(3.56901409908097E-16,-5.06335700088594E-17,
40.1599502534424));
#173937=CARTESIAN_POINT('',(-39.3160391863692,-44.1385184650374,39.8576902534424));
#173938=CARTESIAN_POINT('Ctrl Pts',(-39.4144401478992,-43.7969047596345,
40.1599502534424));
#173939=CARTESIAN_POINT('Ctrl Pts',(-39.4116082546731,-43.7994532913549,
40.1599502448875));
#173940=CARTESIAN_POINT('Ctrl Pts',(-39.4088155471153,-43.8020298032736,
40.1598743450437));
#173941=CARTESIAN_POINT('Ctrl Pts',(-39.4060627300845,-43.80463219181,40.1597243308499));
#173942=CARTESIAN_POINT('Ctrl Pts',(-39.3898103065094,-43.8199964969294,
40.1588386583938));
#173943=CARTESIAN_POINT('Ctrl Pts',(-39.3749452320384,-43.8362633193889,
40.1553722553611));
#173944=CARTESIAN_POINT('Ctrl Pts',(-39.3616178931456,-43.8529956277758,
40.1496902177772));
#173945=CARTESIAN_POINT('Ctrl Pts',(-39.3566392429844,-43.8592462611932,
40.1475675976832));
#173946=CARTESIAN_POINT('Ctrl Pts',(-39.3518747760124,-43.8655619201113,
40.1451361443089));
#173947=CARTESIAN_POINT('Ctrl Pts',(-39.3473309185527,-43.871920208761,
40.1424159447501));
#173948=CARTESIAN_POINT('Ctrl Pts',(-39.3437855730188,-43.8768812645307,
40.1402935085949));
#173949=CARTESIAN_POINT('Ctrl Pts',(-39.3403750229161,-43.8818681433211,
40.1379949176048));
#173950=CARTESIAN_POINT('Ctrl Pts',(-39.3371028088665,-43.8868700682405,
40.1355293609261));
#173951=CARTESIAN_POINT('Ctrl Pts',(-39.3256500596931,-43.9043768054584,
40.1268999125509));
#173952=CARTESIAN_POINT('Ctrl Pts',(-39.3158919212385,-43.9220678510595,
40.1162251288835));
#173953=CARTESIAN_POINT('Ctrl Pts',(-39.3079802585391,-43.93948121423,40.1038990521418));
#173954=CARTESIAN_POINT('Ctrl Pts',(-39.3040244271894,-43.9481878958153,
40.097736013771));
#173955=CARTESIAN_POINT('Ctrl Pts',(-39.3005302159781,-43.9568251581487,
40.0911601532641));
#173956=CARTESIAN_POINT('Ctrl Pts',(-39.2975166114287,-43.9653352562097,
40.084220729064));
#173957=CARTESIAN_POINT('Ctrl Pts',(-39.2945158824213,-43.9738089951121,
40.0773109533619));
#173958=CARTESIAN_POINT('Ctrl Pts',(-39.2919914104331,-43.9821566593549,
40.0700409753048));
#173959=CARTESIAN_POINT('Ctrl Pts',(-39.2899626959158,-43.9903212250461,
40.0624586415899));
#173960=CARTESIAN_POINT('Ctrl Pts',(-39.2899539910981,-43.9903562576028,
40.0624261072769));
#173961=CARTESIAN_POINT('Ctrl Pts',(-39.2899452948636,-43.9903912868064,
40.0623935677888));
#173962=CARTESIAN_POINT('Ctrl Pts',(-39.2899366072115,-43.9904263126553,
40.0623610231288));
#173963=CARTESIAN_POINT('Ctrl Pts',(-39.2858396774348,-44.0069438297326,
40.0470135870265));
#173964=CARTESIAN_POINT('Ctrl Pts',(-39.2836282192311,-44.022686061095,
40.0305755292161));
#173965=CARTESIAN_POINT('Ctrl Pts',(-39.2831328363118,-44.0375574100482,
40.0133447567446));
#173966=CARTESIAN_POINT('Ctrl Pts',(-39.2826194323365,-44.052969749415,
39.9954871626743));
#173967=CARTESIAN_POINT('Ctrl Pts',(-39.2839495744662,-44.0674474907,39.9767767954504));
#173968=CARTESIAN_POINT('Ctrl Pts',(-39.2869823603782,-44.0808629337781,
39.9575197577708));
#173969=CARTESIAN_POINT('Ctrl Pts',(-39.2899718616304,-44.0940869083826,
39.9385375612269));
#173970=CARTESIAN_POINT('Ctrl Pts',(-39.2946164282299,-44.1062793237656,
39.9190226977407));
#173971=CARTESIAN_POINT('Ctrl Pts',(-39.3008183122606,-44.1172870736725,
39.8992655452207));
#173972=CARTESIAN_POINT('Ctrl Pts',(-39.3051423761534,-44.124961872762,
39.8854905069562));
#173973=CARTESIAN_POINT('Ctrl Pts',(-39.310224245815,-44.1320601713495,
39.8715976051593));
#173974=CARTESIAN_POINT('Ctrl Pts',(-39.3160391863692,-44.1385184650374,
39.8576902534424));
#173975=CARTESIAN_POINT('',(-39.5544469813073,-44.4033023070487,39.2875012672119));
#173976=CARTESIAN_POINT('',(-39.3160391863692,-44.1385184650374,39.8576902534424));
#173977=CARTESIAN_POINT('',(-35.209151665053,-47.9220530736685,39.2875012672119));
#173978=CARTESIAN_POINT('Origin',(5.53234440788222E-15,0.,39.2875012672119));
#173979=CARTESIAN_POINT('',(-34.9997217530263,-47.6338034047598,39.8576902534424));
#173980=CARTESIAN_POINT('',(-35.209151665053,-47.9220530736685,39.2875012672119));
#173981=CARTESIAN_POINT('',(-34.6451144164188,-47.6590285860934,40.1599502534424));
#173982=CARTESIAN_POINT('Ctrl Pts',(-34.9997217530263,-47.6338034047598,
39.8576902534424));
#173983=CARTESIAN_POINT('Ctrl Pts',(-34.9925330475314,-47.6239092440462,
39.8772619994059));
#173984=CARTESIAN_POINT('Ctrl Pts',(-34.9838215185863,-47.6151892923575,
39.8967644650381));
#173985=CARTESIAN_POINT('Ctrl Pts',(-34.9737453812839,-47.6077336605719,
39.9159282836064));
#173986=CARTESIAN_POINT('Ctrl Pts',(-34.9634872321454,-47.6001433528495,
39.9354382707214));
#173987=CARTESIAN_POINT('Ctrl Pts',(-34.9518142124603,-47.5938626849608,
39.9545987622393));
#173988=CARTESIAN_POINT('Ctrl Pts',(-34.9388460388034,-47.5890113136614,
39.9731387498278));
#173989=CARTESIAN_POINT('Ctrl Pts',(-34.9264269039957,-47.5843653368443,
39.9908938024117));
#173990=CARTESIAN_POINT('Ctrl Pts',(-34.9128191931051,-47.5810297921587,
40.0080810366257));
#173991=CARTESIAN_POINT('Ctrl Pts',(-34.8980952063128,-47.5791401905748,
40.0244542742626));
#173992=CARTESIAN_POINT('Ctrl Pts',(-34.8863842314085,-47.5776372636136,
40.037477009054));
#173993=CARTESIAN_POINT('Ctrl Pts',(-34.8739663878163,-47.577049512472,
40.0499848770064));
#173994=CARTESIAN_POINT('Ctrl Pts',(-34.8608666162964,-47.5774624305258,
40.0618424270193));
#173995=CARTESIAN_POINT('Ctrl Pts',(-34.8608308581753,-47.5774635576579,
40.0618747942791));
#173996=CARTESIAN_POINT('Ctrl Pts',(-34.8607950951,-47.5774646923709,40.0619071564124));
#173997=CARTESIAN_POINT('Ctrl Pts',(-34.8607593270719,-47.5774658346658,
40.0619395134162));
#173998=CARTESIAN_POINT('Ctrl Pts',(-34.8536390475841,-47.5776932293353,
40.0683807661799));
#173999=CARTESIAN_POINT('Ctrl Pts',(-34.8462974884545,-47.578247706793,
40.0746073439084));
#174000=CARTESIAN_POINT('Ctrl Pts',(-34.8387748826515,-47.5791245434505,
40.0805869293669));
#174001=CARTESIAN_POINT('Ctrl Pts',(-34.8238457504804,-47.5808646865201,
40.092453830807));
#174002=CARTESIAN_POINT('Ctrl Pts',(-34.808202605878,-47.583875471205,40.1033475319609));
#174003=CARTESIAN_POINT('Ctrl Pts',(-34.7921542117506,-47.5881261212204,
40.1130129263075));
#174004=CARTESIAN_POINT('Ctrl Pts',(-34.780117916155,-47.5913141087319,
40.1202619720674));
#174005=CARTESIAN_POINT('Ctrl Pts',(-34.7678536672182,-47.5951995198392,
40.1268200947267));
#174006=CARTESIAN_POINT('Ctrl Pts',(-34.7554917310465,-47.5997693799342,
40.1325796782703));
#174007=CARTESIAN_POINT('Ctrl Pts',(-34.7508560049821,-47.6014830774699,
40.1347395220992));
#174008=CARTESIAN_POINT('Ctrl Pts',(-34.7462065417643,-47.6032930257986,
40.1367870714852));
#174009=CARTESIAN_POINT('Ctrl Pts',(-34.7415502113773,-47.6051985413678,
40.1387166518767));
#174010=CARTESIAN_POINT('Ctrl Pts',(-34.7252530550225,-47.6118678458599,
40.1454701832469));
#174011=CARTESIAN_POINT('Ctrl Pts',(-34.7088717728655,-47.6197078449345,
40.1507785912492));
#174012=CARTESIAN_POINT('Ctrl Pts',(-34.6927009428672,-47.6286892688732,
40.1543986087265));
#174013=CARTESIAN_POINT('Ctrl Pts',(-34.684615527868,-47.6331799808425,
40.1562086174652));
#174014=CARTESIAN_POINT('Ctrl Pts',(-34.6765827265055,-47.6379560498535,
40.1575965292115));
#174015=CARTESIAN_POINT('Ctrl Pts',(-34.6686393635484,-47.6430138207123,
40.1585319382567));
#174016=CARTESIAN_POINT('Ctrl Pts',(-34.6646676820698,-47.6455427061418,
40.1589996427793));
#174017=CARTESIAN_POINT('Ctrl Pts',(-34.6607183602073,-47.6481420170541,
40.159354221642));
#174018=CARTESIAN_POINT('Ctrl Pts',(-34.6567960012265,-47.6508112967867,
40.1595918743111));
#174019=CARTESIAN_POINT('Ctrl Pts',(-34.6528736422457,-47.6534805765194,
40.1598295269801));
#174020=CARTESIAN_POINT('Ctrl Pts',(-34.6489782471461,-47.656219826447,
40.1599502506896));
#174021=CARTESIAN_POINT('Ctrl Pts',(-34.6451144164188,-47.6590285860934,
40.1599502534424));
#174022=CARTESIAN_POINT('',(-34.6205005703637,-47.6769115920302,40.1599502534424));
#174023=CARTESIAN_POINT('Origin',(3.62443809638014E-16,-5.51217168157313E-17,
40.1599502534424));
#174024=CARTESIAN_POINT('',(-34.4869303039399,-48.0063682005185,39.8576902534424));
#174025=CARTESIAN_POINT('Ctrl Pts',(-34.6205005703637,-47.6769115920302,
40.1599502534424));
#174026=CARTESIAN_POINT('Ctrl Pts',(-34.6174177964407,-47.6791501491801,
40.1599502448875));
#174027=CARTESIAN_POINT('Ctrl Pts',(-34.6143710687956,-47.6814206292677,
40.1598743450437));
#174028=CARTESIAN_POINT('Ctrl Pts',(-34.61136130831,-47.6837210139134,40.1597243308499));
#174029=CARTESIAN_POINT('Ctrl Pts',(-34.5935919100082,-47.6973023109013,
40.1588386583937));
#174030=CARTESIAN_POINT('Ctrl Pts',(-34.5771079220164,-47.7119261986147,
40.155372255361));
#174031=CARTESIAN_POINT('Ctrl Pts',(-34.5621045891978,-47.7271737594119,
40.1496902177769));
#174032=CARTESIAN_POINT('Ctrl Pts',(-34.5564998434977,-47.7328697405547,
40.147567597683));
#174033=CARTESIAN_POINT('Ctrl Pts',(-34.5511013106533,-47.7386527792213,
40.1451361443088));
#174034=CARTESIAN_POINT('Ctrl Pts',(-34.5459177227788,-47.7445012740628,
40.1424159447501));
#174035=CARTESIAN_POINT('Ctrl Pts',(-34.5418732274829,-47.7490645631294,
40.1402935085949));
#174036=CARTESIAN_POINT('Ctrl Pts',(-34.537960089954,-47.7536676237149,
40.1379949176048));
#174037=CARTESIAN_POINT('Ctrl Pts',(-34.5341829579102,-47.7583001080602,
40.1355293609261));
#174038=CARTESIAN_POINT('Ctrl Pts',(-34.5209629957568,-47.7745138032686,
40.1268999125509));
#174039=CARTESIAN_POINT('Ctrl Pts',(-34.5094090955954,-47.7910879322537,
40.1162251288835));
#174040=CARTESIAN_POINT('Ctrl Pts',(-34.4997205817196,-47.807578909255,
40.1038990521418));
#174041=CARTESIAN_POINT('Ctrl Pts',(-34.4948763247817,-47.8158243977557,
40.097736013771));
#174042=CARTESIAN_POINT('Ctrl Pts',(-34.4904984154664,-47.824049099734,
40.0911601532641));
#174043=CARTESIAN_POINT('Ctrl Pts',(-34.4866117722854,-47.832197571135,
40.084220729064));
#174044=CARTESIAN_POINT('Ctrl Pts',(-34.4827417346799,-47.8403112284173,
40.0773109533619));
#174045=CARTESIAN_POINT('Ctrl Pts',(-34.4793585234982,-47.8483492841043,
40.0700409753048));
#174046=CARTESIAN_POINT('Ctrl Pts',(-34.4764874929864,-47.8562570650396,
40.0624586415899));
#174047=CARTESIAN_POINT('Ctrl Pts',(-34.4764751739553,-47.856290995783,
40.062426107277));
#174048=CARTESIAN_POINT('Ctrl Pts',(-34.4764628638109,-47.856324924089,
40.0623935677889));
#174049=CARTESIAN_POINT('Ctrl Pts',(-34.4764505625524,-47.8563588499556,
40.0623610231289));
#174050=CARTESIAN_POINT('Ctrl Pts',(-34.4706495255073,-47.872357636576,
40.0470135870232));
#174051=CARTESIAN_POINT('Ctrl Pts',(-34.4668046706499,-47.8877824700235,
40.030575529209));
#174052=CARTESIAN_POINT('Ctrl Pts',(-34.4647575222376,-47.9025205705587,
40.0133447567334));
#174053=CARTESIAN_POINT('Ctrl Pts',(-34.462635902594,-47.9177948141924,
39.9954871626587));
#174054=CARTESIAN_POINT('Ctrl Pts',(-34.462445422019,-47.9323322826113,
39.9767767954302));
#174055=CARTESIAN_POINT('Ctrl Pts',(-34.4640592983654,-47.9459912469416,
39.9575197577459));
#174056=CARTESIAN_POINT('Ctrl Pts',(-34.4656501410751,-47.9594552672033,
39.9385375611976));
#174057=CARTESIAN_POINT('Ctrl Pts',(-34.4689948098118,-47.9720663806699,
39.919022697707));
#174058=CARTESIAN_POINT('Ctrl Pts',(-34.4740120960943,-47.9836621023791,
39.8992655451827));
#174059=CARTESIAN_POINT('Ctrl Pts',(-34.4775102373562,-47.9917468458617,
39.8854905069307));
#174060=CARTESIAN_POINT('Ctrl Pts',(-34.4818222937577,-47.9993374592455,
39.8715976051465));
#174061=CARTESIAN_POINT('Ctrl Pts',(-34.4869303039399,-48.0063682005185,
39.8576902534424));
#174062=CARTESIAN_POINT('',(-34.6963546279287,-48.2946219293745,39.2875012672119));
#174063=CARTESIAN_POINT('',(-34.4869303039399,-48.0063682005185,39.8576902534424));
#174064=CARTESIAN_POINT('',(-30.007053683816,-51.3398895692696,39.2875012672119));
#174065=CARTESIAN_POINT('Origin',(5.53234440788222E-15,0.,39.2875012672119));
#174066=CARTESIAN_POINT('',(-29.8289013456888,-51.0313275753407,39.8576902534424));
#174067=CARTESIAN_POINT('',(-30.007053683816,-51.3398895692696,39.2875012672119));
#174068=CARTESIAN_POINT('',(-29.473599835734,-51.0193480105326,40.1599502534424));
#174069=CARTESIAN_POINT('Ctrl Pts',(-29.8289013456888,-51.0313275753407,
39.8576902534424));
#174070=CARTESIAN_POINT('Ctrl Pts',(-29.822786242089,-51.0207361915361,
39.877261999407));
#174071=CARTESIAN_POINT('Ctrl Pts',(-29.8150339189602,-51.0111534059212,
39.8967644650402));
#174072=CARTESIAN_POINT('Ctrl Pts',(-29.8057923055248,-51.0026853737185,
39.9159282836095));
#174073=CARTESIAN_POINT('Ctrl Pts',(-29.7963837548019,-50.9940643779303,
39.9354382707254));
#174074=CARTESIAN_POINT('Ctrl Pts',(-29.7854311897019,-50.9865979533879,
39.9545987622442));
#174075=CARTESIAN_POINT('Ctrl Pts',(-29.7730411634431,-50.9804176151442,
39.9731387498335));
#174076=CARTESIAN_POINT('Ctrl Pts',(-29.7611756987718,-50.9744989363977,
39.9908938024178));
#174077=CARTESIAN_POINT('Ctrl Pts',(-29.7479911917047,-50.969759271067,
40.0080810366322));
#174078=CARTESIAN_POINT('Ctrl Pts',(-29.7335453816016,-50.966340945206,
40.0244542742694));
#174079=CARTESIAN_POINT('Ctrl Pts',(-29.7220556592906,-50.9636221212266,
40.0374770090583));
#174080=CARTESIAN_POINT('Ctrl Pts',(-29.7097672786705,-50.9617395717399,
40.0499848770085));
#174081=CARTESIAN_POINT('Ctrl Pts',(-29.6966961073823,-50.9607809287994,
40.0618424270193));
#174082=CARTESIAN_POINT('Ctrl Pts',(-29.6966604273306,-50.9607783120156,
40.0618747942791));
#174083=CARTESIAN_POINT('Ctrl Pts',(-29.6966247415593,-50.9607757022531,
40.0619071564124));
#174084=CARTESIAN_POINT('Ctrl Pts',(-29.6965890500698,-50.9607730995134,
40.0619395134161));
#174085=CARTESIAN_POINT('Ctrl Pts',(-29.6894840070028,-50.9602549766183,
40.0683807661799));
#174086=CARTESIAN_POINT('Ctrl Pts',(-29.6821247070256,-50.9600390146966,
40.0746073439084));
#174087=CARTESIAN_POINT('Ctrl Pts',(-29.6745516564559,-50.9601247215269,
40.0805869293669));
#174088=CARTESIAN_POINT('Ctrl Pts',(-29.6595224131521,-50.9602948126669,
40.092453830807));
#174089=CARTESIAN_POINT('Ctrl Pts',(-29.6436502506361,-50.9616539500923,
40.1033475319609));
#174090=CARTESIAN_POINT('Ctrl Pts',(-29.6272454573769,-50.9642038006261,
40.1130129263075));
#174091=CARTESIAN_POINT('Ctrl Pts',(-29.6149418624325,-50.9661161885264,
40.1202619720674));
#174092=CARTESIAN_POINT('Ctrl Pts',(-29.6023386622824,-50.9686983518506,
40.1268200947266));
#174093=CARTESIAN_POINT('Ctrl Pts',(-29.5895667656375,-50.9719510035828,
40.1325796782703));
#174094=CARTESIAN_POINT('Ctrl Pts',(-29.5847773043956,-50.9731707479824,
40.1347395220992));
#174095=CARTESIAN_POINT('Ctrl Pts',(-29.5799641203064,-50.9744847799796,
40.1367870714852));
#174096=CARTESIAN_POINT('Ctrl Pts',(-29.5751341171702,-50.9758931378753,
40.1387166518767));
#174097=CARTESIAN_POINT('Ctrl Pts',(-29.5582291061935,-50.9808223905103,
40.1454701832469));
#174098=CARTESIAN_POINT('Ctrl Pts',(-29.5411180593589,-50.9869071309994,
40.1507785912492));
#174099=CARTESIAN_POINT('Ctrl Pts',(-29.524097000417,-50.9941490417485,
40.1543986087265));
#174100=CARTESIAN_POINT('Ctrl Pts',(-29.5155864709461,-50.997769997123,
40.1562086174652));
#174101=CARTESIAN_POINT('Ctrl Pts',(-29.5070984389558,-51.0016802459461,
40.1575965292115));
#174102=CARTESIAN_POINT('Ctrl Pts',(-29.4986699095566,-51.0058800022839,
40.1585319382567));
#174103=CARTESIAN_POINT('Ctrl Pts',(-29.494455644857,-51.0079798804528,
40.1589996427793));
#174104=CARTESIAN_POINT('Ctrl Pts',(-29.4902562558177,-51.0101521355227,
40.159354221642));
#174105=CARTESIAN_POINT('Ctrl Pts',(-29.4860763682213,-51.012396794505,
40.1595918743111));
#174106=CARTESIAN_POINT('Ctrl Pts',(-29.481896480625,-51.0146414534874,
40.1598295269801));
#174107=CARTESIAN_POINT('Ctrl Pts',(-29.4777360953218,-51.0169585178537,
40.1599502506895));
#174108=CARTESIAN_POINT('Ctrl Pts',(-29.473599835734,-51.0193480105326,
40.1599502534424));
#174109=CARTESIAN_POINT('',(-29.4472515437738,-51.0345602039885,40.1599502534424));
#174110=CARTESIAN_POINT('Origin',(3.68424986610942E-16,-5.90059385582098E-17,
40.1599502534424));
#174111=CARTESIAN_POINT('',(-29.2799753962465,-51.3482501200164,39.8576902534424));
#174112=CARTESIAN_POINT('Ctrl Pts',(-29.4472515437738,-51.0345602039885,
40.1599502534424));
#174113=CARTESIAN_POINT('Ctrl Pts',(-29.4439516646701,-51.0364642604674,
40.1599502448875));
#174114=CARTESIAN_POINT('Ctrl Pts',(-29.4406842975234,-51.0384038328687,
40.1598743450437));
#174115=CARTESIAN_POINT('Ctrl Pts',(-29.4374505691487,-51.0403770101283,
40.1597243308499));
#174116=CARTESIAN_POINT('Ctrl Pts',(-29.4183588813689,-51.0520264994513,
40.1588386583938));
#174117=CARTESIAN_POINT('Ctrl Pts',(-29.4004365818804,-51.0648472300426,
40.1553722553618));
#174118=CARTESIAN_POINT('Ctrl Pts',(-29.3839216347917,-51.0784429877812,
40.149690217779));
#174119=CARTESIAN_POINT('Ctrl Pts',(-29.3777522003172,-51.0835219102899,
40.1475675976845));
#174120=CARTESIAN_POINT('Ctrl Pts',(-29.3717787490539,-51.088708968525,
40.1451361443097));
#174121=CARTESIAN_POINT('Ctrl Pts',(-29.3660122232361,-51.0939835922267,
40.1424159447501));
#174122=CARTESIAN_POINT('Ctrl Pts',(-29.3615128905151,-51.0980991182404,
40.1402935085949));
#174123=CARTESIAN_POINT('Ctrl Pts',(-29.3571400387136,-51.102267928526,
40.1379949176048));
#174124=CARTESIAN_POINT('Ctrl Pts',(-29.3528993717246,-51.1064802178292,
40.1355293609261));
#174125=CARTESIAN_POINT('Ctrl Pts',(-29.3380570372632,-51.1212232303904,
40.1268999125509));
#174126=CARTESIAN_POINT('Ctrl Pts',(-29.3248339623429,-51.1364988531342,
40.1162251288835));
#174127=CARTESIAN_POINT('Ctrl Pts',(-29.3134747466761,-51.1518867653712,
40.1038990521418));
#174128=CARTESIAN_POINT('Ctrl Pts',(-29.3077951388427,-51.1595807214897,
40.097736013771));
#174129=CARTESIAN_POINT('Ctrl Pts',(-29.3025814967141,-51.167302751557,
40.0911601532641));
#174130=CARTESIAN_POINT('Ctrl Pts',(-29.2978643977776,-51.17500031994,40.084220729064));
#174131=CARTESIAN_POINT('Ctrl Pts',(-29.2931674525158,-51.1826650006751,
40.0773109533619));
#174132=CARTESIAN_POINT('Ctrl Pts',(-29.2889625693103,-51.1903053811864,
40.0700409753048));
#174133=CARTESIAN_POINT('Ctrl Pts',(-29.2852806784151,-51.1978697380628,
40.0624586415899));
#174134=CARTESIAN_POINT('Ctrl Pts',(-29.2852648801404,-51.1979021952407,
40.0624261072769));
#174135=CARTESIAN_POINT('Ctrl Pts',(-29.2852490909586,-51.1979346509234,
40.0623935677888));
#174136=CARTESIAN_POINT('Ctrl Pts',(-29.285233310869,-51.197967105109,40.0623610231288));
#174137=CARTESIAN_POINT('Ctrl Pts',(-29.2777917239326,-51.2132718752139,
40.0470135870239));
#174138=CARTESIAN_POINT('Ctrl Pts',(-29.2723555974561,-51.2282103130394,
40.0305755292105));
#174139=CARTESIAN_POINT('Ctrl Pts',(-29.2687791125364,-51.2426536914396,
40.0133447567357));
#174140=CARTESIAN_POINT('Ctrl Pts',(-29.2650725221326,-51.2576224915267,
39.9954871626622));
#174141=CARTESIAN_POINT('Ctrl Pts',(-29.2633635057962,-51.27206041153,39.976776795435));
#174142=CARTESIAN_POINT('Ctrl Pts',(-29.2635407906074,-51.2858132466382,
39.957519757752));
#174143=CARTESIAN_POINT('Ctrl Pts',(-29.2637155451665,-51.2993697979311,
39.9385375612053));
#174144=CARTESIAN_POINT('Ctrl Pts',(-29.2657236711464,-51.312261439481,
39.9190226977163));
#174145=CARTESIAN_POINT('Ctrl Pts',(-29.2695013892381,-51.3243180878377,
39.8992655451936));
#174146=CARTESIAN_POINT('Ctrl Pts',(-29.2721352815043,-51.3327241975823,
39.885490506938));
#174147=CARTESIAN_POINT('Ctrl Pts',(-29.2756302808581,-51.3407239614232,
39.8715976051502));
#174148=CARTESIAN_POINT('Ctrl Pts',(-29.2799753962465,-51.3482501200164,
39.8576902534424));
#174149=CARTESIAN_POINT('',(-29.4581217525676,-51.6568155675426,39.2875012672119));
#174150=CARTESIAN_POINT('',(-29.2799753962465,-51.3482501200164,39.8576902534424));
#174151=CARTESIAN_POINT('',(-24.4761921430394,-54.1952354911871,39.2875012672119));
#174152=CARTESIAN_POINT('Origin',(5.53234440788222E-15,0.,39.2875012672119));
#174153=CARTESIAN_POINT('',(-24.331269253109,-53.8697418420144,39.8576902534424));
#174154=CARTESIAN_POINT('',(-24.4761921430394,-54.1952354911871,39.2875012672119));
#174155=CARTESIAN_POINT('',(-23.9791663275016,-53.8206887816835,40.1599502534424));
#174156=CARTESIAN_POINT('Ctrl Pts',(-24.331269253109,-53.8697418420144,
39.8576902534424));
#174157=CARTESIAN_POINT('Ctrl Pts',(-24.3262947497604,-53.858569276538,
39.877261999404));
#174158=CARTESIAN_POINT('Ctrl Pts',(-24.3195865685243,-53.8482286480035,
39.8967644650344));
#174159=CARTESIAN_POINT('Ctrl Pts',(-24.311280732009,-53.8388409929178,
39.9159282836009));
#174160=CARTESIAN_POINT('Ctrl Pts',(-24.3028248617547,-53.8292837624991,
39.935438270714));
#174161=CARTESIAN_POINT('Ctrl Pts',(-24.2927127498381,-53.8207133850136,
39.95459876223));
#174162=CARTESIAN_POINT('Ctrl Pts',(-24.2810366187012,-53.8132717929053,
39.973138749817));
#174163=CARTESIAN_POINT('Ctrl Pts',(-24.2698548246833,-53.8061452585126,
39.990893802399));
#174164=CARTESIAN_POINT('Ctrl Pts',(-24.2572379736618,-53.8000534013019,
40.0080810366113));
#174165=CARTESIAN_POINT('Ctrl Pts',(-24.2432286115706,-53.7951438030566,
40.0244542742468));
#174166=CARTESIAN_POINT('Ctrl Pts',(-24.2320860256476,-53.7912388700597,
40.0374770090439));
#174167=CARTESIAN_POINT('Ctrl Pts',(-24.2200617420608,-53.7880821478315,
40.0499848770016));
#174168=CARTESIAN_POINT('Ctrl Pts',(-24.2071623814825,-53.7857624469882,
40.0618424270193));
#174169=CARTESIAN_POINT('Ctrl Pts',(-24.2071271704182,-53.7857561149584,
40.0618747942791));
#174170=CARTESIAN_POINT('Ctrl Pts',(-24.2070919529318,-53.7857497893136,
40.0619071564124));
#174171=CARTESIAN_POINT('Ctrl Pts',(-24.2070567290244,-53.7857434700554,
40.0619395134162));
#174172=CARTESIAN_POINT('Ctrl Pts',(-24.2000447667167,-53.7844855062585,
40.0683807661799));
#174173=CARTESIAN_POINT('Ctrl Pts',(-24.1927483559227,-53.7835014710815,
40.0746073439084));
#174174=CARTESIAN_POINT('Ctrl Pts',(-24.1852078325131,-53.7827951090624,
40.0805869293669));
#174175=CARTESIAN_POINT('Ctrl Pts',(-24.1702431416111,-53.7813932847187,
40.092453830807));
#174176=CARTESIAN_POINT('Ctrl Pts',(-24.1543158599158,-53.7810858838906,
40.1033475319609));
#174177=CARTESIAN_POINT('Ctrl Pts',(-24.1377344018726,-53.7819069982468,
40.1130129263075));
#174178=CARTESIAN_POINT('Ctrl Pts',(-24.1252983083403,-53.7825228340139,
40.1202619720675));
#174179=CARTESIAN_POINT('Ctrl Pts',(-24.1124942402751,-53.7837734588333,
40.1268200947266));
#174180=CARTESIAN_POINT('Ctrl Pts',(-24.0994523147292,-53.7856732654697,
40.1325796782703));
#174181=CARTESIAN_POINT('Ctrl Pts',(-24.0945615926495,-53.7863856929583,
40.1347395220992));
#174182=CARTESIAN_POINT('Ctrl Pts',(-24.089637421941,-53.7871894118145,
40.1367870714852));
#174183=CARTESIAN_POINT('Ctrl Pts',(-24.0846866645808,-53.7880851817729,
40.1387166518767));
#174184=CARTESIAN_POINT('Ctrl Pts',(-24.06735901382,-53.7912203766272,40.1454701832469));
#174185=CARTESIAN_POINT('Ctrl Pts',(-24.0497056745176,-53.7954831928408,
40.1507785912492));
#174186=CARTESIAN_POINT('Ctrl Pts',(-24.0320208729158,-53.8009062465107,
40.1543986087265));
#174187=CARTESIAN_POINT('Ctrl Pts',(-24.023178472115,-53.8036177733456,
40.1562086174652));
#174188=CARTESIAN_POINT('Ctrl Pts',(-24.0143282061515,-53.8066193604763,
40.1575965292115));
#174189=CARTESIAN_POINT('Ctrl Pts',(-24.0055068550422,-53.8099150888838,
40.1585319382567));
#174190=CARTESIAN_POINT('Ctrl Pts',(-24.0010961794876,-53.8115629530876,
40.1589996427793));
#174191=CARTESIAN_POINT('Ctrl Pts',(-23.9966927326565,-53.8132843526339,
40.159354221642));
#174192=CARTESIAN_POINT('Ctrl Pts',(-23.9923011121677,-53.8150797979124,
40.159591874311));
#174193=CARTESIAN_POINT('Ctrl Pts',(-23.987909491679,-53.8168752431909,
40.1598295269801));
#174194=CARTESIAN_POINT('Ctrl Pts',(-23.9835296982243,-53.8187447357539,
40.1599502506895));
#174195=CARTESIAN_POINT('Ctrl Pts',(-23.9791663275016,-53.8206887816835,
40.1599502534424));
#174196=CARTESIAN_POINT('',(-23.9513722670367,-53.8330634946837,40.1599502534424));
#174197=CARTESIAN_POINT('Origin',(3.74779409800327E-16,-6.22436788900567E-17,
40.1599502534424));
#174198=CARTESIAN_POINT('',(-23.752222950883,-54.1275498658872,39.8576902534424));
#174199=CARTESIAN_POINT('Ctrl Pts',(-23.9513722670367,-53.8330634946837,
40.1599502534424));
#174200=CARTESIAN_POINT('Ctrl Pts',(-23.9478914369183,-53.8346121892502,
40.1599502448875));
#174201=CARTESIAN_POINT('Ctrl Pts',(-23.9444392282283,-53.8361996036042,
40.1598743450437));
#174202=CARTESIAN_POINT('Ctrl Pts',(-23.9410169613692,-53.8378239549347,
40.1597243308499));
#174203=CARTESIAN_POINT('Ctrl Pts',(-23.920812156637,-53.8474140023509,
40.1588386583939));
#174204=CARTESIAN_POINT('Ctrl Pts',(-23.9016479061145,-53.8582911092143,
40.1553722553622));
#174205=CARTESIAN_POINT('Ctrl Pts',(-23.8838022859714,-53.8700861059286,
40.1496902177798));
#174206=CARTESIAN_POINT('Ctrl Pts',(-23.8771357563386,-53.874492324064,
40.1475675976852));
#174207=CARTESIAN_POINT('Ctrl Pts',(-23.8706528330392,-53.8790265713711,
40.1451361443101));
#174208=CARTESIAN_POINT('Ctrl Pts',(-23.8643665485424,-53.8836695340508,
40.1424159447502));
#174209=CARTESIAN_POINT('Ctrl Pts',(-23.8594616740271,-53.8872922064473,
40.1402935085949));
#174210=CARTESIAN_POINT('Ctrl Pts',(-23.8546770178326,-53.890981092075,
40.1379949176048));
#174211=CARTESIAN_POINT('Ctrl Pts',(-23.8500192775334,-53.8947270356131,
40.1355293609261));
#174212=CARTESIAN_POINT('Ctrl Pts',(-23.8337171864861,-53.9078378379964,
40.1268999125509));
#174213=CARTESIAN_POINT('Ctrl Pts',(-23.818969811583,-53.9216475915793,
40.1162251288835));
#174214=CARTESIAN_POINT('Ctrl Pts',(-23.806064348069,-53.9357638458655,
40.1038990521418));
#174215=CARTESIAN_POINT('Ctrl Pts',(-23.7996116163121,-53.9428219730085,
40.097736013771));
#174216=CARTESIAN_POINT('Ctrl Pts',(-23.7936193631243,-53.9499567269874,
40.0911601532641));
#174217=CARTESIAN_POINT('Ctrl Pts',(-23.7881234899554,-53.9571190561825,
40.084220729064));
#174218=CARTESIAN_POINT('Ctrl Pts',(-23.7826510977526,-53.9642507845243,
40.0773109533619));
#174219=CARTESIAN_POINT('Ctrl Pts',(-23.7776706121036,-53.971409780252,
40.0700409753048));
#174220=CARTESIAN_POINT('Ctrl Pts',(-23.773218200392,-53.9785478363928,
40.0624586415899));
#174221=CARTESIAN_POINT('Ctrl Pts',(-23.773199095963,-53.9785784643975,
40.0624261072769));
#174222=CARTESIAN_POINT('Ctrl Pts',(-23.7731800007333,-53.9786090918657,
40.0623935677888));
#174223=CARTESIAN_POINT('Ctrl Pts',(-23.7731609147026,-53.9786397187953,
40.0623610231288));
#174224=CARTESIAN_POINT('Ctrl Pts',(-23.7641603094579,-53.9930827901221,
40.0470135870232));
#174225=CARTESIAN_POINT('Ctrl Pts',(-23.7571924707012,-54.0073711636762,
40.030575529209));
#174226=CARTESIAN_POINT('Ctrl Pts',(-23.7521258339916,-54.0213615752664,
40.0133447567334));
#174227=CARTESIAN_POINT('Ctrl Pts',(-23.7468748830077,-54.0358609305021,
39.9954871626591));
#174228=CARTESIAN_POINT('Ctrl Pts',(-23.743666055251,-54.0500411172181,
39.976776795431));
#174229=CARTESIAN_POINT('Ctrl Pts',(-23.7424048061582,-54.0637371441659,
39.9575197577471));
#174230=CARTESIAN_POINT('Ctrl Pts',(-23.74116155792,-54.0772376980782,39.9385375611998));
#174231=CARTESIAN_POINT('Ctrl Pts',(-23.7418111396959,-54.0902686241898,
39.9190226977101));
#174232=CARTESIAN_POINT('Ctrl Pts',(-23.7443079001282,-54.1026541040323,
39.8992655451867));
#174233=CARTESIAN_POINT('Ctrl Pts',(-23.7460486859234,-54.1112894809377,
39.8854905069334));
#174234=CARTESIAN_POINT('Ctrl Pts',(-23.748688336284,-54.1196107481453,
39.8715976051479));
#174235=CARTESIAN_POINT('Ctrl Pts',(-23.7522229508831,-54.1275498658872,
39.8576902534424));
#174236=CARTESIAN_POINT('',(-23.8971395307771,-54.4530463244691,39.2875012672119));
#174237=CARTESIAN_POINT('',(-23.752222950883,-54.1275498658872,39.8576902534424));
#174238=CARTESIAN_POINT('',(-18.6771643191712,-56.456807071981,39.2875012672119));
#174239=CARTESIAN_POINT('Origin',(5.53234440788222E-15,0.,39.2875012672119));
#174240=CARTESIAN_POINT('',(-18.5670586829468,-56.1179479440987,39.8576902534424));
#174241=CARTESIAN_POINT('',(-18.6771643191712,-56.456807071981,39.2875012672119));
#174242=CARTESIAN_POINT('',(-18.2220120550219,-56.032358823839,40.1599502534424));
#174243=CARTESIAN_POINT('Ctrl Pts',(-18.5670586829468,-56.1179479440987,
39.8576902534424));
#174244=CARTESIAN_POINT('Ctrl Pts',(-18.5632792815475,-56.1063166059131,
39.8772619994065));
#174245=CARTESIAN_POINT('Ctrl Pts',(-18.557688738439,-56.0953314285464,
39.8967644650392));
#174246=CARTESIAN_POINT('Ctrl Pts',(-18.5504096793237,-56.0851270036894,
39.915928283608));
#174247=CARTESIAN_POINT('Ctrl Pts',(-18.5429991338188,-56.0747382496545,
39.9354382707233));
#174248=CARTESIAN_POINT('Ctrl Pts',(-18.5338382654958,-56.0651578180738,
39.9545987622416));
#174249=CARTESIAN_POINT('Ctrl Pts',(-18.5230039556122,-56.0565365037404,
39.9731387498305));
#174250=CARTESIAN_POINT('Ctrl Pts',(-18.5126283423185,-56.048280193503,
39.9908938024142));
#174251=CARTESIAN_POINT('Ctrl Pts',(-18.5007173801975,-56.0409028880747,
40.0080810366281));
#174252=CARTESIAN_POINT('Ctrl Pts',(-18.4872979556147,-56.0345558080315,
40.0244542742649));
#174253=CARTESIAN_POINT('Ctrl Pts',(-18.4766245865927,-56.0295075492857,
40.0374770090555));
#174254=CARTESIAN_POINT('Ctrl Pts',(-18.464996140618,-56.0251112400294,
40.0499848770071));
#174255=CARTESIAN_POINT('Ctrl Pts',(-18.4524099188568,-56.0214558964133,
40.0618424270193));
#174256=CARTESIAN_POINT('Ctrl Pts',(-18.4523755625598,-56.0214459185126,
40.0618747942791));
#174257=CARTESIAN_POINT('Ctrl Pts',(-18.4523411992083,-56.0214359462906,
40.0619071564124));
#174258=CARTESIAN_POINT('Ctrl Pts',(-18.4523068288036,-56.0214259797491,
40.0619395134162));
#174259=CARTESIAN_POINT('Ctrl Pts',(-18.4454647717816,-56.0194419575649,
40.0683807661799));
#174260=CARTESIAN_POINT('Ctrl Pts',(-18.4383111911741,-56.0177006304279,
40.0746073439084));
#174261=CARTESIAN_POINT('Ctrl Pts',(-18.4308858104772,-56.0162099386097,
40.0805869293669));
#174262=CARTESIAN_POINT('Ctrl Pts',(-18.4161496282621,-56.0132515574632,
40.092453830807));
#174263=CARTESIAN_POINT('Ctrl Pts',(-18.4003417300186,-56.0112809863293,
40.1033475319609));
#174264=CARTESIAN_POINT('Ctrl Pts',(-18.3837652771157,-56.0103643682071,
40.1130129263075));
#174265=CARTESIAN_POINT('Ctrl Pts',(-18.3713329374386,-56.0096769046155,
40.1202619720674));
#174266=CARTESIAN_POINT('Ctrl Pts',(-18.3584682855075,-56.0095822888228,
40.1268200947266));
#174267=CARTESIAN_POINT('Ctrl Pts',(-18.3452992211262,-56.0101084356843,
40.1325796782703));
#174268=CARTESIAN_POINT('Ctrl Pts',(-18.3403608219831,-56.0103057407574,
40.1347395220992));
#174269=CARTESIAN_POINT('Ctrl Pts',(-18.3353796149,-56.0105903407606,40.1367870714852));
#174270=CARTESIAN_POINT('Ctrl Pts',(-18.3303623448495,-56.0109637085385,
40.1387166518767));
#174271=CARTESIAN_POINT('Ctrl Pts',(-18.3128018996725,-56.0122704957613,
40.1454701832469));
#174272=CARTESIAN_POINT('Ctrl Pts',(-18.2947996815818,-56.0146646833928,
40.1507785912492));
#174273=CARTESIAN_POINT('Ctrl Pts',(-18.2766448957073,-56.0182094638726,
40.1543986087265));
#174274=CARTESIAN_POINT('Ctrl Pts',(-18.2675675027701,-56.0199818541126,
40.1562086174652));
#174275=CARTESIAN_POINT('Ctrl Pts',(-18.2584519681994,-56.0220418935342,
40.1575965292115));
#174276=CARTESIAN_POINT('Ctrl Pts',(-18.2493344439487,-56.0243974853213,
40.1585319382567));
#174277=CARTESIAN_POINT('Ctrl Pts',(-18.2447756818233,-56.0255752812148,
40.1589996427793));
#174278=CARTESIAN_POINT('Ctrl Pts',(-18.2402164222855,-56.026826965224,
40.159354221642));
#174279=CARTESIAN_POINT('Ctrl Pts',(-18.2356611844174,-56.0281535255244,
40.159591874311));
#174280=CARTESIAN_POINT('Ctrl Pts',(-18.2311059465494,-56.0294800858249,
40.1598295269801));
#174281=CARTESIAN_POINT('Ctrl Pts',(-18.2265547308768,-56.0308815240328,
40.1599502506895));
#174282=CARTESIAN_POINT('Ctrl Pts',(-18.2220120550219,-56.032358823839,
40.1599502534424));
#174283=CARTESIAN_POINT('',(-18.1930767435952,-56.0417604764382,40.1599502534424));
#174284=CARTESIAN_POINT('Origin',(3.81437458815951E-16,-6.47994644506575E-17,
40.1599502534424));
#174285=CARTESIAN_POINT('',(-17.9642361803975,-56.3138168485094,39.8576902534424));
#174286=CARTESIAN_POINT('Ctrl Pts',(-18.1930767435952,-56.0417604764382,
40.1599502534424));
#174287=CARTESIAN_POINT('Ctrl Pts',(-18.1894530991653,-56.0429368412708,
40.1599502448875));
#174288=CARTESIAN_POINT('Ctrl Pts',(-18.1858538720526,-56.0441547055336,
40.1598743450437));
#174289=CARTESIAN_POINT('Ctrl Pts',(-18.1822805617811,-56.0454124342019,
40.1597243308499));
#174290=CARTESIAN_POINT('Ctrl Pts',(-18.1611840081625,-56.0528379691462,
40.1588386583938));
#174291=CARTESIAN_POINT('Ctrl Pts',(-18.1409877741429,-56.0616522804241,
40.1553722553617));
#174292=CARTESIAN_POINT('Ctrl Pts',(-18.122007001292,-56.0715172876635,
40.1496902177785));
#174293=CARTESIAN_POINT('Ctrl Pts',(-18.1149164163972,-56.0752025259765,
40.1475675976842));
#174294=CARTESIAN_POINT('Ctrl Pts',(-18.1079950493283,-56.0790342841916,
40.1451361443095));
#174295=CARTESIAN_POINT('Ctrl Pts',(-18.1012578800032,-56.082994716577,
40.1424159447502));
#174296=CARTESIAN_POINT('Ctrl Pts',(-18.0960012025252,-56.0860848445995,
40.1402935085949));
#174297=CARTESIAN_POINT('Ctrl Pts',(-18.0908571636321,-56.0892533893665,
40.1379949176048));
#174298=CARTESIAN_POINT('Ctrl Pts',(-18.0858333812,-56.0924919457981,40.1355293609261));
#174299=CARTESIAN_POINT('Ctrl Pts',(-18.0682501426879,-56.1038268933089,
40.1268999125509));
#174300=CARTESIAN_POINT('Ctrl Pts',(-18.0521400431274,-56.116019475181,
40.1162251288835));
#174301=CARTESIAN_POINT('Ctrl Pts',(-18.0378297267253,-56.1287094108802,
40.1038990521418));
#174302=CARTESIAN_POINT('Ctrl Pts',(-18.0306745685242,-56.1350543787299,
40.097736013771));
#174303=CARTESIAN_POINT('Ctrl Pts',(-18.0239693566573,-56.1415236867628,
40.0911601532641));
#174304=CARTESIAN_POINT('Ctrl Pts',(-18.0177549231924,-56.1480723047925,
40.0842207290641));
#174305=CARTESIAN_POINT('Ctrl Pts',(-18.0115670407226,-56.1545929440328,
40.0773109533619));
#174306=CARTESIAN_POINT('Ctrl Pts',(-18.0058655198732,-56.1611921195216,
40.0700409753048));
#174307=CARTESIAN_POINT('Ctrl Pts',(-18.0006913688997,-56.16782566889,40.0624586415899));
#174308=CARTESIAN_POINT('Ctrl Pts',(-18.0006691676285,-56.1678541321547,
40.0624261072769));
#174309=CARTESIAN_POINT('Ctrl Pts',(-18.0006469755623,-56.1678825958473,
40.0623935677888));
#174310=CARTESIAN_POINT('Ctrl Pts',(-18.000624792701,-56.167911059966,40.0623610231288));
#174311=CARTESIAN_POINT('Ctrl Pts',(-17.9901637816642,-56.1813341912006,
40.047013587025));
#174312=CARTESIAN_POINT('Ctrl Pts',(-17.9817405717279,-56.1948159540701,
40.0305755292129));
#174313=CARTESIAN_POINT('Ctrl Pts',(-17.9752392943607,-56.2082001169709,
40.0133447567395));
#174314=CARTESIAN_POINT('Ctrl Pts',(-17.9685015133149,-56.222071169383,
39.9954871626674));
#174315=CARTESIAN_POINT('Ctrl Pts',(-17.963828030726,-56.2358382617167,
39.9767767954415));
#174316=CARTESIAN_POINT('Ctrl Pts',(-17.9611420662374,-56.2493274239651,
39.9575197577599));
#174317=CARTESIAN_POINT('Ctrl Pts',(-17.9584944364888,-56.2626240656018,
39.9385375612143));
#174318=CARTESIAN_POINT('Ctrl Pts',(-17.9577783571054,-56.2756515067207,
39.9190226977264));
#174319=CARTESIAN_POINT('Ctrl Pts',(-17.9589668048467,-56.2882301201392,
39.8992655452047));
#174320=CARTESIAN_POINT('Ctrl Pts',(-17.959795411757,-56.2970001532144,
39.8854905069454));
#174321=CARTESIAN_POINT('Ctrl Pts',(-17.9615507925633,-56.3055517542492,
39.8715976051539));
#174322=CARTESIAN_POINT('Ctrl Pts',(-17.9642361803975,-56.3138168485094,
39.8576902534424));
#174323=CARTESIAN_POINT('',(-18.0743352474894,-56.6526781108323,39.2875012672119));
#174324=CARTESIAN_POINT('',(-17.9642361803975,-56.3138168485094,39.8576902534424));
#174325=CARTESIAN_POINT('',(-12.6735055745743,-58.0998260601479,39.2875012672119));
#174326=CARTESIAN_POINT('Origin',(5.53234440788222E-15,0.,39.2875012672119));
#174327=CARTESIAN_POINT('',(-12.5994235324474,-57.751314065072,39.8576902534424));
#174328=CARTESIAN_POINT('',(-12.6735055745743,-58.0998260601479,39.2875012672119));
#174329=CARTESIAN_POINT('',(-12.2652136052663,-57.6301266171957,40.1599502534424));
#174330=CARTESIAN_POINT('Ctrl Pts',(-12.5994235324474,-57.751314065072,
39.8576902534424));
#174331=CARTESIAN_POINT('Ctrl Pts',(-12.5968806409107,-57.7393513895537,
39.8772619994062));
#174332=CARTESIAN_POINT('Ctrl Pts',(-12.5924689870913,-57.7278420192582,
39.8967644650387));
#174333=CARTESIAN_POINT('Ctrl Pts',(-12.5862964562724,-57.716932626445,
39.9159282836073));
#174334=CARTESIAN_POINT('Ctrl Pts',(-12.5800124270059,-57.7058261701582,
39.9354382707225));
#174335=CARTESIAN_POINT('Ctrl Pts',(-12.5719031706688,-57.6953406496962,
39.9545987622405));
#174336=CARTESIAN_POINT('Ctrl Pts',(-12.5620293850071,-57.6856340700621,
39.9731387498292));
#174337=CARTESIAN_POINT('Ctrl Pts',(-12.5525736298301,-57.676338441843,
39.990893802413));
#174338=CARTESIAN_POINT('Ctrl Pts',(-12.5414990556053,-57.6677565154992,
40.0080810366269));
#174339=CARTESIAN_POINT('Ctrl Pts',(-12.5288165945578,-57.660041493595,
40.0244542742637));
#174340=CARTESIAN_POINT('Ctrl Pts',(-12.5187293820967,-57.6539052188769,
40.0374770090547));
#174341=CARTESIAN_POINT('Ctrl Pts',(-12.507624177416,-57.6483174894745,
40.0499848770067));
#174342=CARTESIAN_POINT('Ctrl Pts',(-12.495488991745,-57.643366551794,40.0618424270193));
#174343=CARTESIAN_POINT('Ctrl Pts',(-12.49545586663,-57.6433530373423,40.0618747942791));
#174344=CARTESIAN_POINT('Ctrl Pts',(-12.4954227339057,-57.643339527801,
40.0619071564124));
#174345=CARTESIAN_POINT('Ctrl Pts',(-12.4953895935729,-57.6433260231716,
40.0619395134161));
#174346=CARTESIAN_POINT('Ctrl Pts',(-12.4887924048451,-57.6406376799625,
40.0683807661799));
#174347=CARTESIAN_POINT('Ctrl Pts',(-12.4818600305505,-57.6381581392099,
40.0746073439084));
#174348=CARTESIAN_POINT('Ctrl Pts',(-12.4746311465908,-57.635899449924,
40.0805869293669));
#174349=CARTESIAN_POINT('Ctrl Pts',(-12.4602849257588,-57.6314169246176,
40.092453830807));
#174350=CARTESIAN_POINT('Ctrl Pts',(-12.4447696056082,-57.6278047731677,
40.1033475319609));
#174351=CARTESIAN_POINT('Ctrl Pts',(-12.4283797729326,-57.6251604652271,
40.1130129263075));
#174352=CARTESIAN_POINT('Ctrl Pts',(-12.4160873984258,-57.6231772342717,
40.1202619720674));
#174353=CARTESIAN_POINT('Ctrl Pts',(-12.4033031104474,-57.6217384144974,
40.1268200947266));
#174354=CARTESIAN_POINT('Ctrl Pts',(-12.3901511902558,-57.6208851370089,
40.1325796782703));
#174355=CARTESIAN_POINT('Ctrl Pts',(-12.3852192201839,-57.6205651579507,
40.1347395220992));
#174356=CARTESIAN_POINT('Ctrl Pts',(-12.3802355518734,-57.6203275209637,
40.1367870714852));
#174357=CARTESIAN_POINT('Ctrl Pts',(-12.3752067393931,-57.6201743958657,
40.1387166518767));
#174358=CARTESIAN_POINT('Ctrl Pts',(-12.3576058957119,-57.6196384580227,
40.1454701832469));
#174359=CARTESIAN_POINT('Ctrl Pts',(-12.3394520349016,-57.6201377858514,
40.1507785912492));
#174360=CARTESIAN_POINT('Ctrl Pts',(-12.3210261723876,-57.6217654557844,
40.1543986087265));
#174361=CARTESIAN_POINT('Ctrl Pts',(-12.3118132411305,-57.622579290751,
40.1562086174652));
#174362=CARTESIAN_POINT('Ctrl Pts',(-12.302532309657,-57.6236752122406,
40.1575965292115));
#174363=CARTESIAN_POINT('Ctrl Pts',(-12.2932185057685,-57.6250648590507,
40.1585319382567));
#174364=CARTESIAN_POINT('Ctrl Pts',(-12.2885616038243,-57.6257596824557,
40.1589996427793));
#174365=CARTESIAN_POINT('Ctrl Pts',(-12.2838964837812,-57.6265279372158,
40.159354221642));
#174366=CARTESIAN_POINT('Ctrl Pts',(-12.2792275366732,-57.6273710784659,
40.159591874311));
#174367=CARTESIAN_POINT('Ctrl Pts',(-12.2745585895652,-57.6282142197161,
40.1598295269801));
#174368=CARTESIAN_POINT('Ctrl Pts',(-12.2698858157461,-57.6291322491186,
40.1599502506895));
#174369=CARTESIAN_POINT('Ctrl Pts',(-12.2652136052663,-57.6301266171957,
40.1599502534424));
#174370=CARTESIAN_POINT('',(-12.2354540642047,-57.6364522029206,40.1599502534424));
#174371=CARTESIAN_POINT('Origin',(3.88326186679512E-16,-6.6645293518578E-17,
40.1599502534424));
#174372=CARTESIAN_POINT('',(-11.9794294790614,-57.8830978693155,39.8576902534424));
#174373=CARTESIAN_POINT('Ctrl Pts',(-12.2354540642047,-57.6364522029206,
40.1599502534424));
#174374=CARTESIAN_POINT('Ctrl Pts',(-12.2317273068699,-57.6372433495199,
40.1599502448875));
#174375=CARTESIAN_POINT('Ctrl Pts',(-12.2280204952201,-57.6380783205158,
40.1598743450437));
#174376=CARTESIAN_POINT('Ctrl Pts',(-12.2243352914712,-57.6389556465833,
40.1597243308499));
#174377=CARTESIAN_POINT('Ctrl Pts',(-12.2025781272236,-57.6441353133404,
40.1588386583938));
#174378=CARTESIAN_POINT('Ctrl Pts',(-12.181571183874,-57.6507902575932,
40.1553722553615));
#174379=CARTESIAN_POINT('Ctrl Pts',(-12.1616632156355,-57.6586171922733,
40.1496902177781));
#174380=CARTESIAN_POINT('Ctrl Pts',(-12.1542262614095,-57.6615410745223,
40.1475675976839));
#174381=CARTESIAN_POINT('Ctrl Pts',(-12.1469422825162,-57.6646283621014,
40.1451361443093));
#174382=CARTESIAN_POINT('Ctrl Pts',(-12.139828042199,-57.6678628728673,
40.1424159447501));
#174383=CARTESIAN_POINT('Ctrl Pts',(-12.1342771550167,-57.6703866004265,
40.1402935085949));
#174384=CARTESIAN_POINT('Ctrl Pts',(-12.1288300925916,-57.6730000890932,
40.1379949176048));
#174385=CARTESIAN_POINT('Ctrl Pts',(-12.1234953096383,-57.6756957761164,
40.1355293609261));
#174386=CARTESIAN_POINT('Ctrl Pts',(-12.104823569302,-57.6851306806978,
40.1268999125509));
#174387=CARTESIAN_POINT('Ctrl Pts',(-12.0875272507062,-57.6955725063805,
40.1162251288835));
#174388=CARTESIAN_POINT('Ctrl Pts',(-12.071968868237,-57.7066970899019,
40.1038990521418));
#174389=CARTESIAN_POINT('Ctrl Pts',(-12.0641896770024,-57.7122593816626,
40.097736013771));
#174390=CARTESIAN_POINT('Ctrl Pts',(-12.0568449701605,-57.7179923646568,
40.0911601532641));
#174391=CARTESIAN_POINT('Ctrl Pts',(-12.0499800630333,-57.7238555234916,
40.084220729064));
#174392=CARTESIAN_POINT('Ctrl Pts',(-12.0431444860318,-57.7296936321424,
40.0773109533618));
#174393=CARTESIAN_POINT('Ctrl Pts',(-12.0367843970375,-57.7356606854448,
40.0700409753047));
#174394=CARTESIAN_POINT('Ctrl Pts',(-12.0309451958829,-57.7417170494856,
40.0624586415899));
#174395=CARTESIAN_POINT('Ctrl Pts',(-12.0309201410113,-57.7417430361608,
40.0624261072769));
#174396=CARTESIAN_POINT('Ctrl Pts',(-12.0308950952495,-57.7417690242238,
40.0623935677888));
#174397=CARTESIAN_POINT('Ctrl Pts',(-12.0308700585976,-57.7417950136726,
40.0623610231288));
#174398=CARTESIAN_POINT('Ctrl Pts',(-12.0190632547924,-57.7540511381832,
40.0470135870234));
#174399=CARTESIAN_POINT('Ctrl Pts',(-12.0092769601257,-57.7665785813561,
40.0305755292095));
#174400=CARTESIAN_POINT('Ctrl Pts',(-12.0014122714555,-57.7792098558809,
40.0133447567342));
#174401=CARTESIAN_POINT('Ctrl Pts',(-11.9932614808863,-57.7923006313193,
39.9954871626601));
#174402=CARTESIAN_POINT('Ctrl Pts',(-11.9871745471187,-57.805503794129,
39.9767767954322));
#174403=CARTESIAN_POINT('Ctrl Pts',(-11.9830932952244,-57.8186383015961,
39.9575197577485));
#174404=CARTESIAN_POINT('Ctrl Pts',(-11.9790702919521,-57.8315853501706,
39.9385375612013));
#174405=CARTESIAN_POINT('Ctrl Pts',(-11.9769963969268,-57.8444665749274,
39.9190226977116));
#174406=CARTESIAN_POINT('Ctrl Pts',(-11.9768635110975,-57.8571005080023,
39.8992655451883));
#174407=CARTESIAN_POINT('Ctrl Pts',(-11.9767708607331,-57.8659091109221,
39.8854905069344));
#174408=CARTESIAN_POINT('Ctrl Pts',(-11.9776227396652,-57.8745973526463,
39.8715976051484));
#174409=CARTESIAN_POINT('Ctrl Pts',(-11.9794294790615,-57.8830978693155,
39.8576902534424));
#174410=CARTESIAN_POINT('',(-12.0535047649324,-58.2316113004781,39.2875012672119));
#174411=CARTESIAN_POINT('',(-11.9794294790614,-57.8830978693155,39.8576902534424));
#174412=CARTESIAN_POINT('',(-6.53099325080075,-59.1062911958296,39.2875012672119));
#174413=CARTESIAN_POINT('Origin',(5.53234440788222E-15,0.,39.2875012672119));
#174414=CARTESIAN_POINT('',(-6.4937464611276,-58.7519447039088,39.8576902534424));
#174415=CARTESIAN_POINT('',(-6.53099325080075,-59.1062911958296,39.2875012672119));
#174416=CARTESIAN_POINT('',(-6.1740349085904,-58.5964866834551,40.1599502534424));
#174417=CARTESIAN_POINT('Ctrl Pts',(-6.4937464611276,-58.7519447039088,
39.8576902534424));
#174418=CARTESIAN_POINT('Ctrl Pts',(-6.49246793990533,-58.739781756634,
39.8772619994064));
#174419=CARTESIAN_POINT('Ctrl Pts',(-6.48928351037725,-58.7278742924789,
39.8967644650391));
#174420=CARTESIAN_POINT('Ctrl Pts',(-6.48428513539387,-58.7163794572999,
39.915928283608));
#174421=CARTESIAN_POINT('Ctrl Pts',(-6.47919647150502,-58.7046769834202,
39.9354382707233));
#174422=CARTESIAN_POINT('Ctrl Pts',(-6.47222767386294,-58.6934012556331,
39.9545987622416));
#174423=CARTESIAN_POINT('Ctrl Pts',(-6.46342259168479,-58.682715758016,
39.9731387498305));
#174424=CARTESIAN_POINT('Ctrl Pts',(-6.45499029385669,-58.6724826566631,
39.9908938024145));
#174425=CARTESIAN_POINT('Ctrl Pts',(-6.44487344288068,-58.6627901347846,
40.0080810366285));
#174426=CARTESIAN_POINT('Ctrl Pts',(-6.43306689706524,-58.6537916984138,
40.0244542742654));
#174427=CARTESIAN_POINT('Ctrl Pts',(-6.42367635877621,-58.6466346380338,
40.0374770090558));
#174428=CARTESIAN_POINT('Ctrl Pts',(-6.41321606633668,-58.6399167088185,
40.0499848770073));
#174429=CARTESIAN_POINT('Ctrl Pts',(-6.40166487239057,-58.6337244205833,
40.0618424270192));
#174430=CARTESIAN_POINT('Ctrl Pts',(-6.40163334138329,-58.6337075176478,
40.0618747942791));
#174431=CARTESIAN_POINT('Ctrl Pts',(-6.40160180229505,-58.6336906188004,
40.0619071564124));
#174432=CARTESIAN_POINT('Ctrl Pts',(-6.40157025512661,-58.6336737240427,
40.0619395134161));
#174433=CARTESIAN_POINT('Ctrl Pts',(-6.3952902148734,-58.6303105138594,
40.0683807661799));
#174434=CARTESIAN_POINT('Ctrl Pts',(-6.38865499943491,-58.6271199258587,
40.0746073439084));
#174435=CARTESIAN_POINT('Ctrl Pts',(-6.38170181337804,-58.6241179857776,
40.0805869293668));
#174436=CARTESIAN_POINT('Ctrl Pts',(-6.36790273412669,-58.6181604277965,
40.092453830807));
#174437=CARTESIAN_POINT('Ctrl Pts',(-6.35284998116341,-58.6129462715178,
40.1033475319609));
#174438=CARTESIAN_POINT('Ctrl Pts',(-6.33682633915145,-58.60860324535,40.1130129263075));
#174439=CARTESIAN_POINT('Ctrl Pts',(-6.32480860764249,-58.6053459757241,
40.1202619720674));
#174440=CARTESIAN_POINT('Ctrl Pts',(-6.31224475095125,-58.6025787159788,
40.1268200947266));
#174441=CARTESIAN_POINT('Ctrl Pts',(-6.2992540701391,-58.600355362827,40.1325796782703));
#174442=CARTESIAN_POINT('Ctrl Pts',(-6.29438256483455,-58.5995216053951,
40.1347395220992));
#174443=CARTESIAN_POINT('Ctrl Pts',(-6.28945103740957,-58.5987643350184,
40.1367870714852));
#174444=CARTESIAN_POINT('Ctrl Pts',(-6.28446577922136,-58.598086394715,
40.1387166518767));
#174445=CARTESIAN_POINT('Ctrl Pts',(-6.26701737556263,-58.5957136036534,
40.1454701832469));
#174446=CARTESIAN_POINT('Ctrl Pts',(-6.24891076953076,-58.5943126009392,
40.1507785912492));
#174447=CARTESIAN_POINT('Ctrl Pts',(-6.23041570798265,-58.5940053272331,
40.1543986087265));
#174448=CARTESIAN_POINT('Ctrl Pts',(-6.2211681772086,-58.59385169038,40.1562086174652));
#174449=CARTESIAN_POINT('Ctrl Pts',(-6.21182353265963,-58.5939714867925,
40.1575965292115));
#174450=CARTESIAN_POINT('Ctrl Pts',(-6.20241549311782,-58.5943799633642,
40.1585319382567));
#174451=CARTESIAN_POINT('Ctrl Pts',(-6.19771147334692,-58.5945842016501,
40.1589996427793));
#174452=CARTESIAN_POINT('Ctrl Pts',(-6.19299160483011,-58.5948606100012,
40.159354221642));
#174453=CARTESIAN_POINT('Ctrl Pts',(-6.18826010244368,-58.5952110945691,
40.159591874311));
#174454=CARTESIAN_POINT('Ctrl Pts',(-6.18352860005725,-58.595561579137,
40.1598295269801));
#174455=CARTESIAN_POINT('Ctrl Pts',(-6.17878546397932,-58.5959861416118,
40.1599502506895));
#174456=CARTESIAN_POINT('Ctrl Pts',(-6.1740349085904,-58.5964866834551,
40.1599502534424));
#174457=CARTESIAN_POINT('',(-6.14377718965342,-58.5996668978648,40.1599502534424));
#174458=CARTESIAN_POINT('Origin',(3.95370119046986E-16,-6.77609428042844E-17,
40.1599502534424));
#174459=CARTESIAN_POINT('',(-5.86337364149601,-58.8181995570485,39.8576902534424));
#174460=CARTESIAN_POINT('Ctrl Pts',(-6.14377718965342,-58.5996668978648,
40.1599502534424));
#174461=CARTESIAN_POINT('Ctrl Pts',(-6.13998815054705,-58.600064158263,
40.1599502448875));
#174462=CARTESIAN_POINT('Ctrl Pts',(-6.13621436696423,-58.6005070878751,
40.1598743450437));
#174463=CARTESIAN_POINT('Ctrl Pts',(-6.13245764560146,-58.6009943991739,
40.1597243308499));
#174464=CARTESIAN_POINT('Ctrl Pts',(-6.11027824676966,-58.6038714482307,
40.1588386583938));
#174465=CARTESIAN_POINT('Ctrl Pts',(-6.08869075055779,-58.6082941124963,
40.1553722553615));
#174466=CARTESIAN_POINT('Ctrl Pts',(-6.06807370279808,-58.6139972210825,
40.1496902177781));
#174467=CARTESIAN_POINT('Ctrl Pts',(-6.06037186006718,-58.616127712602,
40.1475675976838));
#174468=CARTESIAN_POINT('Ctrl Pts',(-6.05280507414612,-58.6184367045765,
40.1451361443093));
#174469=CARTESIAN_POINT('Ctrl Pts',(-6.04539170794196,-58.6209098557463,
40.1424159447501));
#174470=CARTESIAN_POINT('Ctrl Pts',(-6.03960742773698,-58.6228395323549,
40.1402935085949));
#174471=CARTESIAN_POINT('Ctrl Pts',(-6.03391702093568,-58.6248693309927,
40.1379949176048));
#174472=CARTESIAN_POINT('Ctrl Pts',(-6.02832968645966,-58.6269926140964,
40.1355293609261));
#174473=CARTESIAN_POINT('Ctrl Pts',(-6.00877401579359,-58.6344241049594,
40.1268999125508));
#174474=CARTESIAN_POINT('Ctrl Pts',(-5.99048098024847,-58.6430007716254,
40.1162251288835));
#174475=CARTESIAN_POINT('Ctrl Pts',(-5.97384499260642,-58.6524381197038,
40.1038990521418));
#174476=CARTESIAN_POINT('Ctrl Pts',(-5.96552699878539,-58.657156793743,
40.0977360137709));
#174477=CARTESIAN_POINT('Ctrl Pts',(-5.95762326711375,-58.6620906399372,
40.0911601532641));
#174478=CARTESIAN_POINT('Ctrl Pts',(-5.95018309968312,-58.667204101582,
40.084220729064));
#174479=CARTESIAN_POINT('Ctrl Pts',(-5.942774720162,-58.6722957161033,40.0773109533618));
#174480=CARTESIAN_POINT('Ctrl Pts',(-5.93582574548873,-58.6775652709344,
40.0700409753047));
#174481=CARTESIAN_POINT('Ctrl Pts',(-5.92938546966289,-58.682978094856,
40.0624586415899));
#174482=CARTESIAN_POINT('Ctrl Pts',(-5.92935783569725,-58.6830013202262,
40.0624261072769));
#174483=CARTESIAN_POINT('Ctrl Pts',(-5.92933021064649,-58.6830245479289,
40.0623935677888));
#174484=CARTESIAN_POINT('Ctrl Pts',(-5.92930259451082,-58.6830477779621,
40.0623610231288));
#174485=CARTESIAN_POINT('Ctrl Pts',(-5.91627935575207,-58.6940026150819,
40.047013587024));
#174486=CARTESIAN_POINT('Ctrl Pts',(-5.90523719704842,-58.7054384852672,
40.0305755292109));
#174487=CARTESIAN_POINT('Ctrl Pts',(-5.89609526425068,-58.7171784805273,
40.0133447567363));
#174488=CARTESIAN_POINT('Ctrl Pts',(-5.88662076592572,-58.729345553715,
39.995487162663));
#174489=CARTESIAN_POINT('Ctrl Pts',(-5.87918707069946,-58.741840130384,
39.976776795436));
#174490=CARTESIAN_POINT('Ctrl Pts',(-5.87375524644868,-58.7544760786557,
39.9575197577532));
#174491=CARTESIAN_POINT('Ctrl Pts',(-5.86840094651777,-58.7669316835932,
39.9385375612066));
#174492=CARTESIAN_POINT('Ctrl Pts',(-5.86499195787729,-58.7795255625926,
39.9190226977177));
#174493=CARTESIAN_POINT('Ctrl Pts',(-5.86353919440072,-58.7920763953083,
39.8992655451951));
#174494=CARTESIAN_POINT('Ctrl Pts',(-5.86252630185744,-58.8008270591809,
39.885490506939));
#174495=CARTESIAN_POINT('Ctrl Pts',(-5.86246534555152,-58.8095567514049,
39.8715976051507));
#174496=CARTESIAN_POINT('Ctrl Pts',(-5.86337364149604,-58.8181995570485,
39.8576902534424));
#174497=CARTESIAN_POINT('',(-5.90061356181277,-59.1725467709677,39.2875012672119));
#174498=CARTESIAN_POINT('',(-5.863373641496,-58.8181995570485,39.8576902534424));
#174499=CARTESIAN_POINT('',(-0.316925998273249,-59.4651754363832,39.2875012672119));
#174500=CARTESIAN_POINT('Origin',(5.53234440788222E-15,0.,39.2875012672119));
#174501=CARTESIAN_POINT('',(-0.316922544675889,-59.1088767419348,39.8576902534424));
#174502=CARTESIAN_POINT('',(-0.316925998273249,-59.4651754363832,39.2875012672119));
#174503=CARTESIAN_POINT('',(-0.0152121934561199,-58.9208513795073,40.1599502534424));
#174504=CARTESIAN_POINT('Ctrl Pts',(-0.316922544675889,-59.1088767419348,
39.8576902534424));
#174505=CARTESIAN_POINT('Ctrl Pts',(-0.316922401514067,-59.0966467826991,
39.8772619994066));
#174506=CARTESIAN_POINT('Ctrl Pts',(-0.31500008555365,-59.0844716853535,
39.8967644650393));
#174507=CARTESIAN_POINT('Ctrl Pts',(-0.311230629648154,-59.0725173476285,
39.9159282836083));
#174508=CARTESIAN_POINT('Ctrl Pts',(-0.307393083603557,-59.0603470709087,
39.9354382707237));
#174509=CARTESIAN_POINT('Ctrl Pts',(-0.30164109626188,-59.0484046750299,
39.954598762242));
#174510=CARTESIAN_POINT('Ctrl Pts',(-0.294001187890306,-59.0368573319776,
39.973138749831));
#174511=CARTESIAN_POINT('Ctrl Pts',(-0.286684733430826,-59.0257988734909,
39.990893802415));
#174512=CARTESIAN_POINT('Ctrl Pts',(-0.2776364480401,-59.0151019493757,
40.0080810366291));
#174513=CARTESIAN_POINT('Ctrl Pts',(-0.266835172443557,-59.0049186872903,
40.024454274266));
#174514=CARTESIAN_POINT('Ctrl Pts',(-0.258244193028963,-58.9968192554994,
40.0374770090562));
#174515=CARTESIAN_POINT('Ctrl Pts',(-0.248543417983242,-58.9890447295094,
40.0499848770074));
#174516=CARTESIAN_POINT('Ctrl Pts',(-0.237702773059699,-58.981678934725,
40.0618424270193));
#174517=CARTESIAN_POINT('Ctrl Pts',(-0.23767318162044,-58.9816588284979,
40.0618747942791));
#174518=CARTESIAN_POINT('Ctrl Pts',(-0.23764358171718,-58.9816387254916,
40.0619071564124));
#174519=CARTESIAN_POINT('Ctrl Pts',(-0.237613973350494,-58.9816186257082,
40.0619395134161));
#174520=CARTESIAN_POINT('Ctrl Pts',(-0.231719887006989,-58.9776173965852,
40.0683807661799));
#174521=CARTESIAN_POINT('Ctrl Pts',(-0.225454527233562,-58.9737507180862,
40.0746073439084));
#174522=CARTESIAN_POINT('Ctrl Pts',(-0.218853219640932,-58.9700384170936,
40.0805869293669));
#174523=CARTESIAN_POINT('Ctrl Pts',(-0.205752467570129,-58.9626710986899,
40.092453830807));
#174524=CARTESIAN_POINT('Ctrl Pts',(-0.191327202905632,-58.9559120649696,
40.1033475319609));
#174525=CARTESIAN_POINT('Ctrl Pts',(-0.17584530993245,-58.9499179036781,
40.1130129263075));
#174526=CARTESIAN_POINT('Ctrl Pts',(-0.164233890202564,-58.9454222827095,
40.1202619720674));
#174527=CARTESIAN_POINT('Ctrl Pts',(-0.152028117041501,-58.9413569016699,
40.1268200947266));
#174528=CARTESIAN_POINT('Ctrl Pts',(-0.139341004226341,-58.9377878323772,
40.1325796782703));
#174529=CARTESIAN_POINT('Ctrl Pts',(-0.134583336920656,-58.9364494313924,
40.1347395220992));
#174530=CARTESIAN_POINT('Ctrl Pts',(-0.129757981227665,-58.9351808244388,
40.1367870714852));
#174531=CARTESIAN_POINT('Ctrl Pts',(-0.124870896863519,-58.933985496586,
40.1387166518767));
#174532=CARTESIAN_POINT('Ctrl Pts',(-0.10776610158901,-58.9298018491012,
40.1454701832469));
#174533=CARTESIAN_POINT('Ctrl Pts',(-0.089905130100263,-58.9265158655229,
40.1507785912492));
#174534=CARTESIAN_POINT('Ctrl Pts',(-0.0715435052827867,-58.9242770147326,
40.1543986087265));
#174535=CARTESIAN_POINT('Ctrl Pts',(-0.0623626928740485,-58.9231575893375,
40.1562086174652));
#174536=CARTESIAN_POINT('Ctrl Pts',(-0.0530567171307724,-58.9222999481582,
40.1575965292115));
#174537=CARTESIAN_POINT('Ctrl Pts',(-0.0436575183856271,-58.9217227791368,
40.1585319382567));
#174538=CARTESIAN_POINT('Ctrl Pts',(-0.0389579190130544,-58.9214341946262,
40.1589996427793));
#174539=CARTESIAN_POINT('Ctrl Pts',(-0.0342350138896586,-58.9212157281805,
40.159354221642));
#174540=CARTESIAN_POINT('Ctrl Pts',(-0.0294927955550829,-58.9210697160839,
40.159591874311));
#174541=CARTESIAN_POINT('Ctrl Pts',(-0.0247505772205073,-58.9209237039872,
40.1598295269801));
#174542=CARTESIAN_POINT('Ctrl Pts',(-0.0199890456752399,-58.9208501479391,
40.1599502506895));
#174543=CARTESIAN_POINT('Ctrl Pts',(-0.0152121934561203,-58.9208513795073,
40.1599502534424));
#174544=CARTESIAN_POINT('',(0.0152121934557198,-58.9208513795073,40.1599502534424));
#174545=CARTESIAN_POINT('Origin',(4.02492081121313E-16,-6.81341890207372E-17,
40.1599502534424));
#174546=CARTESIAN_POINT('',(0.316922544675488,-59.1088767419348,39.8576902534424));
#174547=CARTESIAN_POINT('Ctrl Pts',(0.0152121934557198,-58.9208513795073,
40.1599502534424));
#174548=CARTESIAN_POINT('Ctrl Pts',(0.0190220008283426,-58.9208504012364,
40.1599502448875));
#174549=CARTESIAN_POINT('Ctrl Pts',(0.0228214099815219,-58.9208964366351,
40.1598743450437));
#174550=CARTESIAN_POINT('Ctrl Pts',(0.0266084895328039,-58.9209883940807,
40.1597243308499));
#174551=CARTESIAN_POINT('Ctrl Pts',(0.0489671208138393,-58.9215313038857,
40.1588386583938));
#174552=CARTESIAN_POINT('Ctrl Pts',(0.0708986527619951,-58.9236732325288,
40.1553722553614));
#174553=CARTESIAN_POINT('Ctrl Pts',(0.0919988953533014,-58.9271900305701,
40.149690217778));
#174554=CARTESIAN_POINT('Ctrl Pts',(0.0998812435883289,-58.9285037892491,
40.1475675976838));
#174555=CARTESIAN_POINT('Ctrl Pts',(0.107647933247126,-58.9300091878198,
40.1451361443093));
#174556=CARTESIAN_POINT('Ctrl Pts',(0.115279202946685,-58.9316938830317,
40.1424159447501));
#174557=CARTESIAN_POINT('Ctrl Pts',(0.12123350238999,-58.933008366749,40.1402935085949));
#174558=CARTESIAN_POINT('Ctrl Pts',(0.127104908279783,-58.9344322364591,
40.1379949176048));
#174559=CARTESIAN_POINT('Ctrl Pts',(0.132883578272846,-58.9359598525093,
40.1355293609261));
#174560=CARTESIAN_POINT('Ctrl Pts',(0.153108923248566,-58.9413065086849,
40.1268999125509));
#174561=CARTESIAN_POINT('Ctrl Pts',(0.172198253417505,-58.9479240485795,
40.1162251288835));
#174562=CARTESIAN_POINT('Ctrl Pts',(0.189729578870567,-58.9555707636545,
40.1038990521418));
#174563=CARTESIAN_POINT('Ctrl Pts',(0.198495241597098,-58.959394121192,
40.097736013771));
#174564=CARTESIAN_POINT('Ctrl Pts',(0.206871403160346,-58.9634747743348,
40.0911601532641));
#174565=CARTESIAN_POINT('Ctrl Pts',(0.214805314863011,-58.9677825146336,
40.0842207290641));
#174566=CARTESIAN_POINT('Ctrl Pts',(0.222705329147431,-58.9720718502312,
40.0773109533619));
#174567=CARTESIAN_POINT('Ctrl Pts',(0.230167055078978,-58.9765861722458,
40.0700409753048));
#174568=CARTESIAN_POINT('Ctrl Pts',(0.237137844566452,-58.9812961520165,
40.0624586415899));
#174569=CARTESIAN_POINT('Ctrl Pts',(0.237167754862592,-58.9813163616197,
40.0624261072769));
#174570=CARTESIAN_POINT('Ctrl Pts',(0.237197656536499,-58.9813365744745,
40.0623935677888));
#174571=CARTESIAN_POINT('Ctrl Pts',(0.237227549587748,-58.9813567905789,
40.0623610231288));
#174572=CARTESIAN_POINT('Ctrl Pts',(0.251324537972111,-58.990890316821,
40.0470135870233));
#174573=CARTESIAN_POINT('Ctrl Pts',(0.263501580512134,-59.0011093202329,
40.0305755292092));
#174574=CARTESIAN_POINT('Ctrl Pts',(0.273820596509111,-59.0118294103846,
40.0133447567338));
#174575=CARTESIAN_POINT('Ctrl Pts',(0.284514998004039,-59.0229394763227,
39.9954871626595));
#174576=CARTESIAN_POINT('Ctrl Pts',(0.29321400956858,-59.0345885736557,
39.9767767954314));
#174577=CARTESIAN_POINT('Ctrl Pts',(0.299936893972488,-59.0465875206396,
39.9575197577476));
#174578=CARTESIAN_POINT('Ctrl Pts',(0.306563827731274,-59.058415215727,
39.9385375612));
#174579=CARTESIAN_POINT('Ctrl Pts',(0.311270560393424,-59.0705837677963,
39.9190226977101));
#174580=CARTESIAN_POINT('Ctrl Pts',(0.314027284735721,-59.082913990604,
39.8992655451865));
#174581=CARTESIAN_POINT('Ctrl Pts',(0.315949321994053,-59.0915108413215,
39.8854905069332));
#174582=CARTESIAN_POINT('Ctrl Pts',(0.316922445687527,-59.1001863397074,
39.8715976051478));
#174583=CARTESIAN_POINT('Ctrl Pts',(0.316922544675488,-59.1088767419348,
39.8576902534424));
#174584=CARTESIAN_POINT('',(0.316925998272844,-59.4651754363832,39.2875012672119));
#174585=CARTESIAN_POINT('',(0.316922544675488,-59.1088767419348,39.8576902534424));
#174586=CARTESIAN_POINT('',(5.90061356181238,-59.1725467709678,39.2875012672119));
#174587=CARTESIAN_POINT('Origin',(5.53234440788222E-15,0.,39.2875012672119));
#174588=CARTESIAN_POINT('',(5.86337364149561,-58.8181995570485,39.8576902534424));
#174589=CARTESIAN_POINT('',(5.90061356181238,-59.1725467709677,39.2875012672119));
#174590=CARTESIAN_POINT('',(6.14377718965303,-58.5996668978649,40.1599502534424));
#174591=CARTESIAN_POINT('Ctrl Pts',(5.86337364149561,-58.8181995570485,
39.8576902534424));
#174592=CARTESIAN_POINT('Ctrl Pts',(5.86209540502861,-58.8060365798462,
39.8772619994041));
#174593=CARTESIAN_POINT('Ctrl Pts',(5.8627345461251,-58.7937272422261,39.8967644650344));
#174594=CARTESIAN_POINT('Ctrl Pts',(5.86523378400419,-58.7814443761823,
39.915928283601));
#174595=CARTESIAN_POINT('Ctrl Pts',(5.86777816724618,-58.7689396367226,
39.935438270714));
#174596=CARTESIAN_POINT('Ctrl Pts',(5.87225032430913,-58.756461416142,39.9545987622301));
#174597=CARTESIAN_POINT('Ctrl Pts',(5.8786413544374,-58.7441787427631,39.973138749817));
#174598=CARTESIAN_POINT('Ctrl Pts',(5.88476180492035,-58.7324160859292,
39.9908938023989));
#174599=CARTESIAN_POINT('Ctrl Pts',(5.8926423898153,-58.7208319573178,40.0080810366112));
#174600=CARTESIAN_POINT('Ctrl Pts',(5.90232005415442,-58.7095754394694,
40.0244542742466));
#174601=CARTESIAN_POINT('Ctrl Pts',(5.91001735012912,-58.7006223753325,
40.0374770090438));
#174602=CARTESIAN_POINT('Ctrl Pts',(5.91885232406354,-58.6918764318968,
40.0499848770016));
#174603=CARTESIAN_POINT('Ctrl Pts',(5.92886364759533,-58.683417831748,40.0618424270192));
#174604=CARTESIAN_POINT('Ctrl Pts',(5.92889097525656,-58.6833947425173,
40.0618747942791));
#174605=CARTESIAN_POINT('Ctrl Pts',(5.92891831167211,-58.683371655605,40.0619071564124));
#174606=CARTESIAN_POINT('Ctrl Pts',(5.92894565684159,-58.6833485710132,
40.0619395134162));
#174607=CARTESIAN_POINT('Ctrl Pts',(5.93438921243199,-58.6787531612542,
40.0683807661799));
#174608=CARTESIAN_POINT('Ctrl Pts',(5.94021607194758,-58.6742527563956,
40.0746073439084));
#174609=CARTESIAN_POINT('Ctrl Pts',(5.94639317576857,-58.6698707672381,
40.0805869293669));
#174610=CARTESIAN_POINT('Ctrl Pts',(5.95865206607762,-58.6611744062938,
40.092453830807));
#174611=CARTESIAN_POINT('Ctrl Pts',(5.97229179622499,-58.6529445485198,
40.1033475319609));
#174612=CARTESIAN_POINT('Ctrl Pts',(5.98706231730019,-58.6453649253901,
40.1130129263075));
#174613=CARTESIAN_POINT('Ctrl Pts',(5.99814020810659,-58.6396802080428,
40.1202619720674));
#174614=CARTESIAN_POINT('Ctrl Pts',(6.0098541687325,-58.6343612468744,40.1268200947266));
#174615=CARTESIAN_POINT('Ctrl Pts',(6.02209871088773,-58.6294855649109,
40.1325796782703));
#174616=CARTESIAN_POINT('Ctrl Pts',(6.02669041419593,-58.6276571841746,
40.1347395220992));
#174617=CARTESIAN_POINT('Ctrl Pts',(6.0313567305502,-58.6258911397672,40.1367870714852));
#174618=CARTESIAN_POINT('Ctrl Pts',(6.0360920971713,-58.624191520627,40.1387166518767));
#174619=CARTESIAN_POINT('Ctrl Pts',(6.05266588034515,-58.6182428536363,
40.1454701832469));
#174620=CARTESIAN_POINT('Ctrl Pts',(6.07008552874949,-58.6131078911177,
40.1507785912492));
#174621=CARTESIAN_POINT('Ctrl Pts',(6.08811254303242,-58.608961992561,40.1543986087265));
#174622=CARTESIAN_POINT('Ctrl Pts',(6.09712605017388,-58.6068890432827,
40.1562086174652));
#174623=CARTESIAN_POINT('Ctrl Pts',(6.10629139889382,-58.6050633610079,
40.1575965292115));
#174624=CARTESIAN_POINT('Ctrl Pts',(6.11557877725394,-58.6035068699781,
40.1585319382567));
#174625=CARTESIAN_POINT('Ctrl Pts',(6.120222466434,-58.6027286244632,40.1589996427793));
#174626=CARTESIAN_POINT('Ctrl Pts',(6.12489666302713,-58.6020176767849,
40.159354221642));
#174627=CARTESIAN_POINT('Ctrl Pts',(6.1295976405734,-58.6013767677628,40.159591874311));
#174628=CARTESIAN_POINT('Ctrl Pts',(6.13429861811967,-58.6007358587407,
40.1598295269801));
#174629=CARTESIAN_POINT('Ctrl Pts',(6.13902637679625,-58.6001649900651,
40.1599502506895));
#174630=CARTESIAN_POINT('Ctrl Pts',(6.14377718965303,-58.5996668978649,
40.1599502534424));
#174631=CARTESIAN_POINT('',(6.17403490859001,-58.5964866834551,40.1599502534424));
#174632=CARTESIAN_POINT('Origin',(5.66232193761676E-15,5.18494695161684E-15,
40.1599502534424));
#174633=CARTESIAN_POINT('',(6.4937464611272,-58.7519447039089,39.8576902534424));
#174634=CARTESIAN_POINT('Ctrl Pts',(6.17403490859001,-58.5964866834551,
40.1599502534424));
#174635=CARTESIAN_POINT('Ctrl Pts',(6.17782374318207,-58.5960874772333,
40.1599502448875));
#174636=CARTESIAN_POINT('Ctrl Pts',(6.18160715078385,-58.5957361140451,
40.1598743450437));
#174637=CARTESIAN_POINT('Ctrl Pts',(6.18538309648758,-58.5954317101325,
40.1597243308499));
#174638=CARTESIAN_POINT('Ctrl Pts',(6.20767599437374,-58.5936345324522,
40.1588386583938));
#174639=CARTESIAN_POINT('Ctrl Pts',(6.22971127560378,-58.5934722580544,
40.1553722553617));
#174640=CARTESIAN_POINT('Ctrl Pts',(6.25106353435248,-58.5947642147752,
40.1496902177787));
#174641=CARTESIAN_POINT('Ctrl Pts',(6.25904002743583,-58.5952468467988,
40.1475675976843));
#174642=CARTESIAN_POINT('Ctrl Pts',(6.26692152735609,-58.5959321585039,
40.1451361443095));
#174643=CARTESIAN_POINT('Ctrl Pts',(6.27468709076417,-58.5968099398848,
40.1424159447501));
#174644=CARTESIAN_POINT('Ctrl Pts',(6.28074617289508,-58.5974948289521,
40.1402935085949));
#174645=CARTESIAN_POINT('Ctrl Pts',(6.28673424952176,-58.5982971695201,
40.1379949176048));
#174646=CARTESIAN_POINT('Ctrl Pts',(6.29264094271416,-58.5992123816356,
40.1355293609261));
#174647=CARTESIAN_POINT('Ctrl Pts',(6.31331436888755,-58.6024156240399,
40.1268999125509));
#174648=CARTESIAN_POINT('Ctrl Pts',(6.33299084698427,-58.6070015340112,
40.1162251288835));
#174649=CARTESIAN_POINT('Ctrl Pts',(6.35122543337801,-58.6127738370723,
40.1038990521418));
#174650=CARTESIAN_POINT('Ctrl Pts',(6.36034272657487,-58.6156599886028,
40.097736013771));
#174651=CARTESIAN_POINT('Ctrl Pts',(6.36909954705081,-58.6188427402045,
40.0911601532641));
#174652=CARTESIAN_POINT('Ctrl Pts',(6.37744027742862,-58.6222975626532,
40.084220729064));
#174653=CARTESIAN_POINT('Ctrl Pts',(6.38574537226665,-58.6257376244687,
40.0773109533618));
#174654=CARTESIAN_POINT('Ctrl Pts',(6.39363809722571,-58.6294472538099,
40.0700409753047));
#174655=CARTESIAN_POINT('Ctrl Pts',(6.40106302694645,-58.6334027859057,
40.0624586415899));
#174656=CARTESIAN_POINT('Ctrl Pts',(6.40109488586963,-58.6334197583214,
40.0624261072769));
#174657=CARTESIAN_POINT('Ctrl Pts',(6.40112673655769,-58.633436734872,40.0623935677888));
#174658=CARTESIAN_POINT('Ctrl Pts',(6.40115857901001,-58.6334537155557,
40.0623610231288));
#174659=CARTESIAN_POINT('Ctrl Pts',(6.41617486746476,-58.6414614796111,
40.0470135870231));
#174660=CARTESIAN_POINT('Ctrl Pts',(6.42935337961453,-58.6503516547094,
40.0305755292089));
#174661=CARTESIAN_POINT('Ctrl Pts',(6.4407364215119,-58.659934388201,40.0133447567333));
#174662=CARTESIAN_POINT('Ctrl Pts',(6.45253355607587,-58.6698657226818,
39.9954871626588));
#174663=CARTESIAN_POINT('Ctrl Pts',(6.46240257578758,-58.68054171073,39.9767767954305));
#174664=CARTESIAN_POINT('Ctrl Pts',(6.47034286301635,-58.6917721934516,
39.9575197577464));
#174665=CARTESIAN_POINT('Ctrl Pts',(6.47816982453009,-58.7028423919859,
39.9385375611987));
#174666=CARTESIAN_POINT('Ctrl Pts',(6.48412273326619,-58.7144522959216,
39.9190226977086));
#174667=CARTESIAN_POINT('Ctrl Pts',(6.48815321522585,-58.7264268163197,
39.8992655451849));
#174668=CARTESIAN_POINT('Ctrl Pts',(6.49096333895723,-58.7347756649882,
39.8854905069321));
#174669=CARTESIAN_POINT('Ctrl Pts',(6.49283796829152,-58.7433019189616,
39.8715976051472));
#174670=CARTESIAN_POINT('Ctrl Pts',(6.49374646112718,-58.7519447039089,
39.8576902534424));
#174671=CARTESIAN_POINT('',(6.53099325080036,-59.1062911958297,39.2875012672119));
#174672=CARTESIAN_POINT('',(6.49374646112721,-58.7519447039089,39.8576902534424));
#174673=CARTESIAN_POINT('',(12.053504764932,-58.2316113004781,39.2875012672119));
#174674=CARTESIAN_POINT('Origin',(5.53234440788222E-15,0.,39.2875012672119));
#174675=CARTESIAN_POINT('',(11.9794294790611,-57.8830978693156,39.8576902534424));
#174676=CARTESIAN_POINT('',(12.053504764932,-58.2316113004781,39.2875012672119));
#174677=CARTESIAN_POINT('',(12.2354540642043,-57.6364522029207,40.1599502534424));
#174678=CARTESIAN_POINT('Ctrl Pts',(11.9794294790611,-57.8830978693156,
39.8576902534424));
#174679=CARTESIAN_POINT('Ctrl Pts',(11.9768868675911,-57.8711351342675,
39.877261999406));
#174680=CARTESIAN_POINT('Ctrl Pts',(11.9762358312606,-57.858826420049,39.8967644650382));
#174681=CARTESIAN_POINT('Ctrl Pts',(11.9774374689414,-57.8463495993344,
39.9159282836066));
#174682=CARTESIAN_POINT('Ctrl Pts',(11.978660812587,-57.8336474016744,39.9354382707216));
#174683=CARTESIAN_POINT('Ctrl Pts',(11.9818041414849,-57.820770070385,39.9545987622394));
#174684=CARTESIAN_POINT('Ctrl Pts',(11.9868762719096,-57.8078866382167,
39.973138749828));
#174685=CARTESIAN_POINT('Ctrl Pts',(11.9917336614829,-57.7955486571629,
39.9908938024116));
#174686=CARTESIAN_POINT('Ctrl Pts',(11.9983602045489,-57.7832042421901,
40.0080810366254));
#174687=CARTESIAN_POINT('Ctrl Pts',(12.0068082271198,-57.7709977973416,
40.0244542742621));
#174688=CARTESIAN_POINT('Ctrl Pts',(12.0135275064643,-57.7612891925112,
40.0374770090537));
#174689=CARTESIAN_POINT('Ctrl Pts',(12.0213998814573,-57.7516676540242,
40.0499848770063));
#174690=CARTESIAN_POINT('Ctrl Pts',(12.0304721974328,-57.7422089227118,
40.0618424270193));
#174691=CARTESIAN_POINT('Ctrl Pts',(12.0304969619084,-57.7421831034478,
40.0618747942791));
#174692=CARTESIAN_POINT('Ctrl Pts',(12.0305217353328,-57.7421572855745,
40.0619071564124));
#174693=CARTESIAN_POINT('Ctrl Pts',(12.0305465177056,-57.742131469094,40.0619395134162));
#174694=CARTESIAN_POINT('Ctrl Pts',(12.0354799018087,-57.7369922269699,
40.0683807661799));
#174695=CARTESIAN_POINT('Ctrl Pts',(12.0408044207743,-57.7319074031292,
40.0746073439084));
#174696=CARTESIAN_POINT('Ctrl Pts',(12.0464896431815,-57.7269037357969,
40.0805869293669));
#174697=CARTESIAN_POINT('Ctrl Pts',(12.0577723607613,-57.7169736114624,
40.092453830807));
#174698=CARTESIAN_POINT('Ctrl Pts',(12.0704771166537,-57.7073630976788,
40.1033475319609));
#174699=CARTESIAN_POINT('Ctrl Pts',(12.0843744369111,-57.698281056648,40.1130129263075));
#174700=CARTESIAN_POINT('Ctrl Pts',(12.0947974271042,-57.6914695258749,
40.1202619720674));
#174701=CARTESIAN_POINT('Ctrl Pts',(12.105891234591,-57.6849552602293,40.1268200947266));
#174702=CARTESIAN_POINT('Ctrl Pts',(12.1175590523201,-57.6788263845868,
40.1325796782703));
#174703=CARTESIAN_POINT('Ctrl Pts',(12.1219344839685,-57.6765280562208,
40.1347395220992));
#174704=CARTESIAN_POINT('Ctrl Pts',(12.1263906358456,-57.6742839235119,
40.1367870714852));
#174705=CARTESIAN_POINT('Ctrl Pts',(12.130922403056,-57.6720986344673,40.1387166518767));
#174706=CARTESIAN_POINT('Ctrl Pts',(12.1467835882925,-57.6644501228111,
40.1454701832469));
#174707=CARTESIAN_POINT('Ctrl Pts',(12.1635710602992,-57.657522441076,40.1507785912492));
#174708=CARTESIAN_POINT('Ctrl Pts',(12.1810659563067,-57.6515149180852,
40.1543986087265));
#174709=CARTESIAN_POINT('Ctrl Pts',(12.1898134043104,-57.6485111565898,
40.1562086174652));
#174710=CARTESIAN_POINT('Ctrl Pts',(12.1987377085285,-57.6457374357764,
40.1575965292115));
#174711=CARTESIAN_POINT('Ctrl Pts',(12.2078115120428,-57.6432186759796,
40.1585319382567));
#174712=CARTESIAN_POINT('Ctrl Pts',(12.2123484137999,-57.6419592960811,
40.1589996427793));
#174713=CARTESIAN_POINT('Ctrl Pts',(12.2169226903867,-57.6407636564617,
40.159354221642));
#174714=CARTESIAN_POINT('Ctrl Pts',(12.221530922251,-57.6396348724475,40.159591874311));
#174715=CARTESIAN_POINT('Ctrl Pts',(12.2261391541152,-57.6385060884334,
40.1598295269801));
#174716=CARTESIAN_POINT('Ctrl Pts',(12.2307813416097,-57.6374441616869,
40.1599502506895));
#174717=CARTESIAN_POINT('Ctrl Pts',(12.2354540642043,-57.6364522029207,
40.1599502534424));
#174718=CARTESIAN_POINT('',(12.2652136052659,-57.6301266171958,40.1599502534424));
#174719=CARTESIAN_POINT('Origin',(5.66936586998423E-15,5.18606260090255E-15,
40.1599502534424));
#174720=CARTESIAN_POINT('',(12.599423532447,-57.751314065072,39.8576902534424));
#174721=CARTESIAN_POINT('Ctrl Pts',(12.2652136052659,-57.6301266171958,
40.1599502534424));
#174722=CARTESIAN_POINT('Ctrl Pts',(12.2689399558127,-57.6293335568099,
40.1599502448875));
#174723=CARTESIAN_POINT('Ctrl Pts',(12.2726659100577,-57.6285886446436,
40.1598743450437));
#174724=CARTESIAN_POINT('Ctrl Pts',(12.2763893518626,-57.6278912144856,
40.1597243308499));
#174725=CARTESIAN_POINT('Ctrl Pts',(12.2983722707009,-57.6237736395748,
40.1588386583938));
#174726=CARTESIAN_POINT('Ctrl Pts',(12.3202698780618,-57.6213089400485,
40.1553722553616));
#174727=CARTESIAN_POINT('Ctrl Pts',(12.341640213154,-57.6203619005009,40.1496902177784));
#174728=CARTESIAN_POINT('Ctrl Pts',(12.349623458957,-57.6200081180515,40.1475675976841));
#174729=CARTESIAN_POINT('Ctrl Pts',(12.357533417775,-57.6198658344726,40.1451361443094));
#174730=CARTESIAN_POINT('Ctrl Pts',(12.3653481937526,-57.6199270848658,
40.1424159447501));
#174731=CARTESIAN_POINT('Ctrl Pts',(12.3714456739993,-57.6199748754952,
40.1402935085949));
#174732=CARTESIAN_POINT('Ctrl Pts',(12.3774848147423,-57.6201468963098,
40.1379949176048));
#174733=CARTESIAN_POINT('Ctrl Pts',(12.3834548161673,-57.6204396772352,
40.1355293609261));
#174734=CARTESIAN_POINT('Ctrl Pts',(12.404349821155,-57.621464410474,40.1268999125509));
#174735=CARTESIAN_POINT('Ctrl Pts',(12.4243978675679,-57.6239684463327,
40.1162251288835));
#174736=CARTESIAN_POINT('Ctrl Pts',(12.443135932958,-57.6278030948196,40.1038990521418));
#174737=CARTESIAN_POINT('Ctrl Pts',(12.452504965653,-57.6297204190631,40.097736013771));
#174738=CARTESIAN_POINT('Ctrl Pts',(12.461546503484,-57.631970398231,40.0911601532641));
#174739=CARTESIAN_POINT('Ctrl Pts',(12.4702026697495,-57.6345344510719,
40.084220729064));
#174740=CARTESIAN_POINT('Ctrl Pts',(12.4788218527842,-57.6370875490681,
40.0773109533619));
#174741=CARTESIAN_POINT('Ctrl Pts',(12.4870591024244,-57.6399518422607,
40.0700409753048));
#174742=CARTESIAN_POINT('Ctrl Pts',(12.4948568232946,-57.6431095890442,
40.0624586415899));
#174743=CARTESIAN_POINT('Ctrl Pts',(12.4948902817918,-57.6431231383189,
40.0624261072769));
#174744=CARTESIAN_POINT('Ctrl Pts',(12.4949237325312,-57.6431366925668,
40.0623935677889));
#174745=CARTESIAN_POINT('Ctrl Pts',(12.494957175512,-57.6431502517859,40.0623610231289));
#174746=CARTESIAN_POINT('Ctrl Pts',(12.5107282424386,-57.6495445189159,
40.0470135870229));
#174747=CARTESIAN_POINT('Ctrl Pts',(12.5247638376614,-57.6570084630818,
40.0305755292084));
#174748=CARTESIAN_POINT('Ctrl Pts',(12.5370861904701,-57.66534884948,40.0133447567324));
#174749=CARTESIAN_POINT('Ctrl Pts',(12.5498568062282,-57.6739926427246,
39.9954871626576));
#174750=CARTESIAN_POINT('Ctrl Pts',(12.560787707042,-57.683578553129,39.976776795429));
#174751=CARTESIAN_POINT('Ctrl Pts',(12.5698584016472,-57.6939175280694,
39.9575197577446));
#174752=CARTESIAN_POINT('Ctrl Pts',(12.5787996370877,-57.7041089426389,
39.9385375611966));
#174753=CARTESIAN_POINT('Ctrl Pts',(12.5859335005839,-57.7150329979042,
39.9190226977063));
#174754=CARTESIAN_POINT('Ctrl Pts',(12.5911935813571,-57.7265206205413,
39.8992655451822));
#174755=CARTESIAN_POINT('Ctrl Pts',(12.5948610032577,-57.7345299954275,
39.8854905069303));
#174756=CARTESIAN_POINT('Ctrl Pts',(12.5976165994014,-57.7428135895655,
39.8715976051464));
#174757=CARTESIAN_POINT('Ctrl Pts',(12.599423532447,-57.751314065072,39.8576902534424));
#174758=CARTESIAN_POINT('',(12.6735055745739,-58.099826060148,39.2875012672119));
#174759=CARTESIAN_POINT('',(12.599423532447,-57.751314065072,39.8576902534424));
#174760=CARTESIAN_POINT('',(18.074335247489,-56.6526781108324,39.2875012672119));
#174761=CARTESIAN_POINT('Origin',(5.53234440788222E-15,0.,39.2875012672119));
#174762=CARTESIAN_POINT('',(17.9642361803971,-56.3138168485095,39.8576902534424));
#174763=CARTESIAN_POINT('',(18.074335247489,-56.6526781108324,39.2875012672119));
#174764=CARTESIAN_POINT('',(18.1930767435948,-56.0417604764384,40.1599502534424));
#174765=CARTESIAN_POINT('Ctrl Pts',(17.9642361803971,-56.3138168485095,
39.8576902534424));
#174766=CARTESIAN_POINT('Ctrl Pts',(17.9604570513081,-56.3021854218454,
39.8772619994058));
#174767=CARTESIAN_POINT('Ctrl Pts',(17.9585229704408,-56.2900121878784,
39.8967644650379));
#174768=CARTESIAN_POINT('Ctrl Pts',(17.958413842529,-56.2774781111531,39.9159282836061));
#174769=CARTESIAN_POINT('Ctrl Pts',(17.9583027433685,-56.2647176232298,
39.9354382707207));
#174770=CARTESIAN_POINT('Ctrl Pts',(17.960082805131,-56.2515822679697,39.9545987622382));
#174771=CARTESIAN_POINT('Ctrl Pts',(17.9637804645281,-56.2382392305924,
39.9731387498264));
#174772=CARTESIAN_POINT('Ctrl Pts',(17.9673215746134,-56.2254611028227,
39.9908938024093));
#174773=CARTESIAN_POINT('Ctrl Pts',(17.9726214740556,-56.2124916494839,
40.0080810366224));
#174774=CARTESIAN_POINT('Ctrl Pts',(17.9797472965523,-56.1994690140011,
40.0244542742585));
#174775=CARTESIAN_POINT('Ctrl Pts',(17.9854149414383,-56.1891112379787,
40.0374770090514));
#174776=CARTESIAN_POINT('Ctrl Pts',(17.9922384661056,-56.178719520025,40.0499848770052));
#174777=CARTESIAN_POINT('Ctrl Pts',(18.0002723763371,-56.1683642893843,
40.0618424270193));
#174778=CARTESIAN_POINT('Ctrl Pts',(18.0002943063023,-56.1683360229683,
40.0618747942791));
#174779=CARTESIAN_POINT('Ctrl Pts',(18.0003162453126,-56.1683077570001,
40.0619071564124));
#174780=CARTESIAN_POINT('Ctrl Pts',(18.000338193368,-56.1682794914816,40.0619395134161));
#174781=CARTESIAN_POINT('Ctrl Pts',(18.0047073547952,-56.1626527236046,
40.0683807661799));
#174782=CARTESIAN_POINT('Ctrl Pts',(18.0094711966667,-56.1570391911758,
40.0746073439084));
#174783=CARTESIAN_POINT('Ctrl Pts',(18.0146022491738,-56.1514686668951,
40.0805869293669));
#174784=CARTESIAN_POINT('Ctrl Pts',(18.0247851782094,-56.1404135756907,
40.092453830807));
#174785=CARTESIAN_POINT('Ctrl Pts',(18.0364157638827,-56.1295277006974,
40.1033475319609));
#174786=CARTESIAN_POINT('Ctrl Pts',(18.0492876213734,-56.1190427465076,
40.1130129263075));
#174787=CARTESIAN_POINT('Ctrl Pts',(18.0589415144913,-56.1111790308653,
40.1202619720674));
#174788=CARTESIAN_POINT('Ctrl Pts',(18.0692936227627,-56.1035408324001,
40.1268200947266));
#174789=CARTESIAN_POINT('Ctrl Pts',(18.080256881013,-56.0962259123227,40.1325796782703));
#174790=CARTESIAN_POINT('Ctrl Pts',(18.0843681028569,-56.0934828172937,
40.1347395220992));
#174791=CARTESIAN_POINT('Ctrl Pts',(18.0885652677243,-56.0907851834708,
40.1367870714852));
#174792=CARTESIAN_POINT('Ctrl Pts',(18.0928437845341,-56.0881381670059,
40.1387166518767));
#174793=CARTESIAN_POINT('Ctrl Pts',(18.1078185933686,-56.0788736093784,
40.1454701832469));
#174794=CARTESIAN_POINT('Ctrl Pts',(18.1237899619214,-56.0702291095577,
40.1507785912492));
#174795=CARTESIAN_POINT('Ctrl Pts',(18.1405610619117,-56.0624257818117,
40.1543986087265));
#174796=CARTESIAN_POINT('Ctrl Pts',(18.1489466119069,-56.0585241179387,
40.1562086174652));
#174797=CARTESIAN_POINT('Ctrl Pts',(18.1575320950786,-56.0548327480525,
40.1575965292115));
#174798=CARTESIAN_POINT('Ctrl Pts',(18.1662929092569,-56.0513793155481,
40.1585319382567));
#174799=CARTESIAN_POINT('Ctrl Pts',(18.170673316346,-56.0496525992958,40.1589996427793));
#174800=CARTESIAN_POINT('Ctrl Pts',(18.1750975561951,-56.0479853674131,
40.159354221642));
#174801=CARTESIAN_POINT('Ctrl Pts',(18.1795625536246,-56.0463810756007,
40.1595918743111));
#174802=CARTESIAN_POINT('Ctrl Pts',(18.1840275510542,-56.0447767837883,
40.1598295269801));
#174803=CARTESIAN_POINT('Ctrl Pts',(18.1885333065889,-56.0432354336628,
40.1599502506895));
#174804=CARTESIAN_POINT('Ctrl Pts',(18.1930767435948,-56.0417604764383,
40.1599502534424));
#174805=CARTESIAN_POINT('',(18.2220120550216,-56.0323588238392,40.1599502534424));
#174806=CARTESIAN_POINT('Origin',(5.6762545978478E-15,5.18790842997046E-15,
40.1599502534424));
#174807=CARTESIAN_POINT('',(18.5670586829464,-56.1179479440989,39.8576902534424));
#174808=CARTESIAN_POINT('Ctrl Pts',(18.2220120550216,-56.0323588238392,
40.1599502534424));
#174809=CARTESIAN_POINT('Ctrl Pts',(18.2256350948468,-56.0311805982248,
40.1599502448875));
#174810=CARTESIAN_POINT('Ctrl Pts',(18.2292627734005,-56.0300502984938,
40.1598743450437));
#174811=CARTESIAN_POINT('Ctrl Pts',(18.232892916499,-56.0289674832813,40.1597243308499));
#174812=CARTESIAN_POINT('Ctrl Pts',(18.2543250068277,-56.022574624153,40.1588386583939));
#174813=CARTESIAN_POINT('Ctrl Pts',(18.2758450255481,-56.0178345032623,
40.1553722553623));
#174814=CARTESIAN_POINT('Ctrl Pts',(18.296999299118,-56.0146588434098,40.1496902177801));
#174815=CARTESIAN_POINT('Ctrl Pts',(18.3049018315316,-56.0134725226015,
40.1475675976854));
#174816=CARTESIAN_POINT('Ctrl Pts',(18.3127535860859,-56.0125042026268,
40.1451361443102));
#174817=CARTESIAN_POINT('Ctrl Pts',(18.3205319543147,-56.01174825096,40.1424159447501));
#174818=CARTESIAN_POINT('Ctrl Pts',(18.3266010274077,-56.0111584195473,
40.1402935085949));
#174819=CARTESIAN_POINT('Ctrl Pts',(18.3326250661772,-56.0106982359126,
40.1379949176048));
#174820=CARTESIAN_POINT('Ctrl Pts',(18.33859296725,-56.0103653778788,40.1355293609261));
#174821=CARTESIAN_POINT('Ctrl Pts',(18.3594806210048,-56.0092003747604,
40.1268999125509));
#174822=CARTESIAN_POINT('Ctrl Pts',(18.3796805851421,-56.0095951017656,
40.1162251288835));
#174823=CARTESIAN_POINT('Ctrl Pts',(18.3987168313629,-56.011450082467,40.1038990521418));
#174824=CARTESIAN_POINT('Ctrl Pts',(18.4082349544732,-56.0123775728178,
40.097736013771));
#174825=CARTESIAN_POINT('Ctrl Pts',(18.4174621486788,-56.0136701283093,
40.0911601532641));
#174826=CARTESIAN_POINT('Ctrl Pts',(18.426338912063,-56.015315319243,40.0842207290641));
#174827=CARTESIAN_POINT('Ctrl Pts',(18.4351777497213,-56.016953481144,40.0773109533619));
#174828=CARTESIAN_POINT('Ctrl Pts',(18.4436692750118,-56.0189410563924,
40.0700409753047));
#174829=CARTESIAN_POINT('Ctrl Pts',(18.4517543535699,-56.0212664209291,
40.0624586415899));
#174830=CARTESIAN_POINT('Ctrl Pts',(18.4517890450628,-56.0212763986141,
40.0624261072769));
#174831=CARTESIAN_POINT('Ctrl Pts',(18.4518237293603,-56.021286382056,40.0623935677888));
#174832=CARTESIAN_POINT('Ctrl Pts',(18.4518584064613,-56.0212963712529,
40.0623610231288));
#174833=CARTESIAN_POINT('Ctrl Pts',(18.4682114607472,-56.0260070845278,
40.0470135870254));
#174834=CARTESIAN_POINT('Ctrl Pts',(18.4829503621221,-56.0319630212257,
40.0305755292138));
#174835=CARTESIAN_POINT('Ctrl Pts',(18.4960770195644,-56.0389696815101,
40.013344756741));
#174836=CARTESIAN_POINT('Ctrl Pts',(18.5096811989761,-56.0462312303092,
39.9954871626695));
#174837=CARTESIAN_POINT('Ctrl Pts',(18.5215542196539,-56.0546220378273,
39.9767767954443));
#174838=CARTESIAN_POINT('Ctrl Pts',(18.5316559412067,-56.0639562290112,
39.9575197577634));
#174839=CARTESIAN_POINT('Ctrl Pts',(18.5416134885271,-56.0731572003431,
39.9385375612185));
#174840=CARTESIAN_POINT('Ctrl Pts',(18.5498501466824,-56.0832757207001,
39.9190226977313));
#174841=CARTESIAN_POINT('Ctrl Pts',(18.5562821957245,-56.0941505847762,
39.8992655452103));
#174842=CARTESIAN_POINT('Ctrl Pts',(18.5607667347571,-56.101732733498,39.8854905069492));
#174843=CARTESIAN_POINT('Ctrl Pts',(18.5643731068255,-56.1096829110155,
39.8715976051558));
#174844=CARTESIAN_POINT('Ctrl Pts',(18.5670586829464,-56.1179479440989,
39.8576902534424));
#174845=CARTESIAN_POINT('',(18.6771643191709,-56.4568070719812,39.2875012672119));
#174846=CARTESIAN_POINT('',(18.5670586829464,-56.1179479440989,39.8576902534424));
#174847=CARTESIAN_POINT('',(23.8971395307767,-54.4530463244693,39.2875012672119));
#174848=CARTESIAN_POINT('Origin',(5.53234440788222E-15,0.,39.2875012672119));
#174849=CARTESIAN_POINT('',(23.7522229508827,-54.1275498658874,39.8576902534424));
#174850=CARTESIAN_POINT('',(23.8971395307767,-54.4530463244693,39.2875012672119));
#174851=CARTESIAN_POINT('',(23.9513722670364,-53.8330634946838,40.1599502534424));
#174852=CARTESIAN_POINT('Ctrl Pts',(23.7522229508827,-54.1275498658874,
39.8576902534424));
#174853=CARTESIAN_POINT('Ctrl Pts',(23.7472487091037,-54.116377183953,39.8772619994037));
#174854=CARTESIAN_POINT('Ctrl Pts',(23.7440527738942,-54.1044728027377,
39.8967644650337));
#174855=CARTESIAN_POINT('Ctrl Pts',(23.7426340760177,-54.0920187959705,
39.9159282836));
#174856=CARTESIAN_POINT('Ctrl Pts',(23.7411897512766,-54.0793398243611,
39.9354382707127));
#174857=CARTESIAN_POINT('Ctrl Pts',(23.7415870431742,-54.0660903588324,
39.9545987622285));
#174858=CARTESIAN_POINT('Ctrl Pts',(23.7438697192129,-54.0524339053569,
39.9731387498152));
#174859=CARTESIAN_POINT('Ctrl Pts',(23.7460557526666,-54.0393556307138,
39.990893802397));
#174860=CARTESIAN_POINT('Ctrl Pts',(23.7499709416771,-54.0259032350543,
40.0080810366091));
#174861=CARTESIAN_POINT('Ctrl Pts',(23.7556964920965,-54.0122070876573,
40.0244542742445));
#174862=CARTESIAN_POINT('Ctrl Pts',(23.7602504066211,-54.0013136224016,
40.0374770090424));
#174863=CARTESIAN_POINT('Ctrl Pts',(23.7659503209996,-53.9902655788147,
40.0499848770009));
#174864=CARTESIAN_POINT('Ctrl Pts',(23.772857804287,-53.9791273029164,40.0618424270192));
#174865=CARTESIAN_POINT('Ctrl Pts',(23.7728766594726,-53.9790968990413,
40.0618747942791));
#174866=CARTESIAN_POINT('Ctrl Pts',(23.7728955237005,-53.9790664946659,
40.0619071564124));
#174867=CARTESIAN_POINT('Ctrl Pts',(23.772914396971,-53.9790360897924,40.0619395134161));
#174868=CARTESIAN_POINT('Ctrl Pts',(23.7766714662754,-53.9729834442088,
40.0683807661799));
#174869=CARTESIAN_POINT('Ctrl Pts',(23.7808224374043,-53.9669027062279,
40.0746073439084));
#174870=CARTESIAN_POINT('Ctrl Pts',(23.7853431031263,-53.9608263568286,
40.0805869293668));
#174871=CARTESIAN_POINT('Ctrl Pts',(23.7943146773162,-53.9487674206468,
40.092453830807));
#174872=CARTESIAN_POINT('Ctrl Pts',(23.8047436656399,-53.9367254523685,
40.1033475319609));
#174873=CARTESIAN_POINT('Ctrl Pts',(23.8164490335995,-53.9249524603719,
40.1130129263075));
#174874=CARTESIAN_POINT('Ctrl Pts',(23.8252280595692,-53.9161227163744,
40.1202619720674));
#174875=CARTESIAN_POINT('Ctrl Pts',(23.8347250487607,-53.9074442707905,
40.1268200947266));
#174876=CARTESIAN_POINT('Ctrl Pts',(23.8448636317806,-53.8990234500734,
40.1325796782703));
#174877=CARTESIAN_POINT('Ctrl Pts',(23.848665600413,-53.8958656423044,40.1347395220992));
#174878=CARTESIAN_POINT('Ctrl Pts',(23.8525577932542,-53.8927440632082,
40.1367870714852));
#174879=CARTESIAN_POINT('Ctrl Pts',(23.8565361833379,-53.8896643205892,
40.1387166518767));
#174880=CARTESIAN_POINT('Ctrl Pts',(23.8704605486311,-53.8788852214226,
40.1454701832469));
#174881=CARTESIAN_POINT('Ctrl Pts',(23.8854408280738,-53.8686186144653,
40.1507785912492));
#174882=CARTESIAN_POINT('Ctrl Pts',(23.901304384366,-53.8591049768559,40.1543986087265));
#174883=CARTESIAN_POINT('Ctrl Pts',(23.9092361625121,-53.8543481580511,
40.1562086174652));
#174884=CARTESIAN_POINT('Ctrl Pts',(23.9173887602871,-53.8497795825131,
40.1575965292115));
#174885=CARTESIAN_POINT('Ctrl Pts',(23.9257405998159,-53.8454293138302,
40.1585319382567));
#174886=CARTESIAN_POINT('Ctrl Pts',(23.9299165195804,-53.8432541794887,
40.1589996427793));
#174887=CARTESIAN_POINT('Ctrl Pts',(23.934142249794,-53.8411336218842,40.159354221642));
#174888=CARTESIAN_POINT('Ctrl Pts',(23.9384150933427,-53.8390713992304,
40.159591874311));
#174889=CARTESIAN_POINT('Ctrl Pts',(23.9426879368913,-53.8370091765766,
40.1598295269801));
#174890=CARTESIAN_POINT('Ctrl Pts',(23.9470078944659,-53.8350052904264,
40.1599502506895));
#174891=CARTESIAN_POINT('Ctrl Pts',(23.9513722670364,-53.8330634946838,
40.1599502534424));
#174892=CARTESIAN_POINT('',(23.9791663275012,-53.8206887816837,40.1599502534424));
#174893=CARTESIAN_POINT('Origin',(5.68291264686342E-15,5.19046421553107E-15,
40.1599502534424));
#174894=CARTESIAN_POINT('',(24.3312692531087,-53.8697418420146,39.8576902534424));
#174895=CARTESIAN_POINT('Ctrl Pts',(23.9791663275012,-53.8206887816837,
40.1599502534424));
#174896=CARTESIAN_POINT('Ctrl Pts',(23.9826463618224,-53.8191382997272,
40.1599502448875));
#174897=CARTESIAN_POINT('Ctrl Pts',(23.9861360190795,-53.8176349962319,
40.1598743450437));
#174898=CARTESIAN_POINT('Ctrl Pts',(23.9896330908641,-53.8161786595149,
40.1597243308499));
#174899=CARTESIAN_POINT('Ctrl Pts',(24.0102795382215,-53.8075805576701,
40.1588386583938));
#174900=CARTESIAN_POINT('Ctrl Pts',(24.0311861904778,-53.8006169491706,
40.1553722553615));
#174901=CARTESIAN_POINT('Ctrl Pts',(24.0518926318819,-53.795247462207,40.1496902177781));
#174902=CARTESIAN_POINT('Ctrl Pts',(24.0596278691025,-53.7932416006199,
40.1475675976838));
#174903=CARTESIAN_POINT('Ctrl Pts',(24.0673353939224,-53.7914578533665,
40.1451361443093));
#174904=CARTESIAN_POINT('Ctrl Pts',(24.0749921329677,-53.7898929820048,
40.1424159447501));
#174905=CARTESIAN_POINT('Ctrl Pts',(24.0809663048721,-53.7886719908665,
40.1402935085949));
#174906=CARTESIAN_POINT('Ctrl Pts',(24.0869092410388,-53.7875846446507,
40.1379949176048));
#174907=CARTESIAN_POINT('Ctrl Pts',(24.0928096561863,-53.7866297945199,
40.1355293609261));
#174908=CARTESIAN_POINT('Ctrl Pts',(24.1134611092026,-53.7832878190622,
40.1268999125509));
#174909=CARTESIAN_POINT('Ctrl Pts',(24.1335916760301,-53.7815689125023,
40.1162251288835));
#174910=CARTESIAN_POINT('Ctrl Pts',(24.1527175379843,-53.7814239018615,
40.1038990521418));
#174911=CARTESIAN_POINT('Ctrl Pts',(24.1622804689615,-53.7813513965411,
40.0977360137709));
#174912=CARTESIAN_POINT('Ctrl Pts',(24.1715922244709,-53.7816723668478,
40.0911601532641));
#174913=CARTESIAN_POINT('Ctrl Pts',(24.1805923292966,-53.7823806708181,
40.084220729064));
#174914=CARTESIAN_POINT('Ctrl Pts',(24.1895539814234,-53.7830859485793,
40.0773109533618));
#174915=CARTESIAN_POINT('Ctrl Pts',(24.1982067474363,-53.7841750295931,
40.0700409753047));
#174916=CARTESIAN_POINT('Ctrl Pts',(24.2064906018697,-53.7856425347025,
40.0624586415899));
#174917=CARTESIAN_POINT('Ctrl Pts',(24.206526146271,-53.7856488314803,40.0624261072769));
#174918=CARTESIAN_POINT('Ctrl Pts',(24.2065616841181,-53.7856551347355,
40.0623935677888));
#174919=CARTESIAN_POINT('Ctrl Pts',(24.2065972154097,-53.7856614444665,
40.0623610231288));
#174920=CARTESIAN_POINT('Ctrl Pts',(24.2233530895738,-53.7886369923271,
40.0470135870244));
#174921=CARTESIAN_POINT('Ctrl Pts',(24.2386338146162,-53.79301966707,40.0305755292117));
#174922=CARTESIAN_POINT('Ctrl Pts',(24.2524209582886,-53.7986158348064,
40.0133447567377));
#174923=CARTESIAN_POINT('Ctrl Pts',(24.2667096511195,-53.8044155801139,
39.9954871626651));
#174924=CARTESIAN_POINT('Ctrl Pts',(24.2793947083637,-53.8115193533052,
39.9767767954389));
#174925=CARTESIAN_POINT('Ctrl Pts',(24.2904167802894,-53.8197464933835,
39.9575197577569));
#174926=CARTESIAN_POINT('Ctrl Pts',(24.3012815425175,-53.8278562137128,
39.9385375612115));
#174927=CARTESIAN_POINT('Ctrl Pts',(24.3105307527809,-53.8370583385375,
39.9190226977238));
#174928=CARTESIAN_POINT('Ctrl Pts',(24.318064299215,-53.8472012967688,39.8992655452024));
#174929=CARTESIAN_POINT('Ctrl Pts',(24.3233168218262,-53.8542731477119,
39.8854905069439));
#174930=CARTESIAN_POINT('Ctrl Pts',(24.3277344576485,-53.8618028047936,
39.8715976051531));
#174931=CARTESIAN_POINT('Ctrl Pts',(24.3312692531087,-53.8697418420146,
39.8576902534424));
#174932=CARTESIAN_POINT('',(24.4761921430391,-54.1952354911873,39.2875012672119));
#174933=CARTESIAN_POINT('',(24.3312692531087,-53.8697418420146,39.8576902534424));
#174934=CARTESIAN_POINT('',(29.4581217525673,-51.6568155675428,39.2875012672119));
#174935=CARTESIAN_POINT('Origin',(5.53234440788222E-15,0.,39.2875012672119));
#174936=CARTESIAN_POINT('',(29.2799753962461,-51.3482501200166,39.8576902534424));
#174937=CARTESIAN_POINT('',(29.4581217525673,-51.6568155675428,39.2875012672119));
#174938=CARTESIAN_POINT('',(29.4472515437734,-51.0345602039887,40.1599502534424));
#174939=CARTESIAN_POINT('Ctrl Pts',(29.2799753962461,-51.3482501200166,
39.8576902534424));
#174940=CARTESIAN_POINT('Ctrl Pts',(29.273860540611,-51.337658593052,39.8772619994036));
#174941=CARTESIAN_POINT('Ctrl Pts',(29.2694377663945,-51.3261534914788,
39.8967644650335));
#174942=CARTESIAN_POINT('Ctrl Pts',(29.2667250421045,-51.3139160033728,
39.9159282835996));
#174943=CARTESIAN_POINT('Ctrl Pts',(29.2639633161073,-51.3014574615422,
39.9354382707121));
#174944=CARTESIAN_POINT('Ctrl Pts',(29.2629734853274,-51.2882390496606,
39.9545987622277));
#174945=CARTESIAN_POINT('Ctrl Pts',(29.2638161685324,-51.2744188030479,
39.9731387498142));
#174946=CARTESIAN_POINT('Ctrl Pts',(29.2646231747154,-51.2611836698443,
39.9908938023957));
#174947=CARTESIAN_POINT('Ctrl Pts',(29.2671107576651,-51.2473957191255,
40.0080810366075));
#174948=CARTESIAN_POINT('Ctrl Pts',(29.2713733056799,-51.2331761176706,
40.0244542742427));
#174949=CARTESIAN_POINT('Ctrl Pts',(29.2747635962015,-51.2218663142697,
40.0374770090412));
#174950=CARTESIAN_POINT('Ctrl Pts',(29.2792774508344,-51.2102829897303,
40.0499848770004));
#174951=CARTESIAN_POINT('Ctrl Pts',(29.2849828273429,-51.1984837018591,
40.0618424270193));
#174952=CARTESIAN_POINT('Ctrl Pts',(29.2849984011674,-51.1984514936361,
40.0618747942791));
#174953=CARTESIAN_POINT('Ctrl Pts',(29.2850139839325,-51.1984192839703,
40.0619071564124));
#174954=CARTESIAN_POINT('Ctrl Pts',(29.2850295756385,-51.1983870728639,
40.0619395134161));
#174955=CARTESIAN_POINT('Ctrl Pts',(29.2881333895826,-51.1919748636253,
40.0683807661799));
#174956=CARTESIAN_POINT('Ctrl Pts',(29.2916260110607,-51.1854935419302,
40.0746073439084));
#174957=CARTESIAN_POINT('Ctrl Pts',(29.2954867606378,-51.1789779411678,
40.0805869293669));
#174958=CARTESIAN_POINT('Ctrl Pts',(29.3031486855379,-51.166047280237,40.092453830807));
#174959=CARTESIAN_POINT('Ctrl Pts',(29.3122618143336,-51.1529811529979,
40.1033475319609));
#174960=CARTESIAN_POINT('Ctrl Pts',(29.3226724463013,-51.1400491105585,
40.1130129263075));
#174961=CARTESIAN_POINT('Ctrl Pts',(29.330480420277,-51.130350078729,40.1202619720674));
#174962=CARTESIAN_POINT('Ctrl Pts',(29.3390182393876,-51.1207264688921,
40.1268200947266));
#174963=CARTESIAN_POINT('Ctrl Pts',(29.3482210667398,-51.1112920078092,
40.1325796782703));
#174964=CARTESIAN_POINT('Ctrl Pts',(29.3516721269969,-51.1077540849031,
40.1347395220992));
#174965=CARTESIAN_POINT('Ctrl Pts',(29.3552167041325,-51.1042427612073,
40.1367870714852));
#174966=CARTESIAN_POINT('Ctrl Pts',(29.3588513794159,-51.1007640347389,
40.1387166518767));
#174967=CARTESIAN_POINT('Ctrl Pts',(29.3715727429078,-51.0885884920993,
40.1454701832469));
#174968=CARTESIAN_POINT('Ctrl Pts',(29.3853978061641,-51.0768122610997,
40.1507785912492));
#174969=CARTESIAN_POINT('Ctrl Pts',(29.4001800143157,-51.0656925470313,
40.1543986087265));
#174970=CARTESIAN_POINT('Ctrl Pts',(29.4075711183915,-51.0601326899971,
40.1562086174652));
#174971=CARTESIAN_POINT('Ctrl Pts',(29.4152015092025,-51.0547369630768,
40.1575965292115));
#174972=CARTESIAN_POINT('Ctrl Pts',(29.4230528695803,-51.0495375206695,
40.1585319382567));
#174973=CARTESIAN_POINT('Ctrl Pts',(29.4269785497693,-51.0469377994658,
40.1589996427793));
#174974=CARTESIAN_POINT('Ctrl Pts',(29.430959472363,-51.0443871494123,40.159354221642));
#174975=CARTESIAN_POINT('Ctrl Pts',(29.4349933478627,-51.0418895900601,
40.159591874311));
#174976=CARTESIAN_POINT('Ctrl Pts',(29.4390272233624,-51.0393920307079,
40.1598295269801));
#174977=CARTESIAN_POINT('Ctrl Pts',(29.4431140526175,-51.036947563529,40.1599502506895));
#174978=CARTESIAN_POINT('Ctrl Pts',(29.4472515437734,-51.0345602039887,
40.1599502534424));
#174979=CARTESIAN_POINT('',(29.4735998357337,-51.0193480105328,40.1599502534424));
#174980=CARTESIAN_POINT('Origin',(5.68926707005281E-15,5.19370195586291E-15,
40.1599502534424));
#174981=CARTESIAN_POINT('',(29.8289013456884,-51.0313275753409,39.8576902534424));
#174982=CARTESIAN_POINT('Ctrl Pts',(29.4735998357337,-51.0193480105328,
40.1599502534424));
#174983=CARTESIAN_POINT('Ctrl Pts',(29.4768987365664,-51.0174422596391,
40.1599502448875));
#174984=CARTESIAN_POINT('Ctrl Pts',(29.4802121391118,-51.0155824228872,
40.1598743450437));
#174985=CARTESIAN_POINT('Ctrl Pts',(29.4835378249322,-51.0137685205955,
40.1597243308499));
#174986=CARTESIAN_POINT('Ctrl Pts',(29.5031724225184,-51.0030593786378,
40.1588386583938));
#174987=CARTESIAN_POINT('Ctrl Pts',(29.5232366506516,-50.9939485772816,
40.1553722553613));
#174988=CARTESIAN_POINT('Ctrl Pts',(29.5432683957828,-50.9864440924295,
40.1496902177776));
#174989=CARTESIAN_POINT('Ctrl Pts',(29.5507515889348,-50.9836406667027,
40.1475675976835));
#174990=CARTESIAN_POINT('Ctrl Pts',(29.5582304387674,-50.9810610352785,
40.1451361443091));
#174991=CARTESIAN_POINT('Ctrl Pts',(29.5656816597957,-50.9787043892801,
40.1424159447501));
#174992=CARTESIAN_POINT('Ctrl Pts',(29.571495476234,-50.9768656158505,40.1402935085949));
#174993=CARTESIAN_POINT('Ctrl Pts',(29.5772921977456,-50.9751630202462,
40.1379949176048));
#174994=CARTESIAN_POINT('Ctrl Pts',(29.5830604807847,-50.9735966395564,
40.1355293609261));
#174995=CARTESIAN_POINT('Ctrl Pts',(29.6032494714218,-50.9681143071419,
40.1268999125509));
#174996=CARTESIAN_POINT('Ctrl Pts',(29.6230900862367,-50.9643005997167,
40.1162251288835));
#174997=CARTESIAN_POINT('Ctrl Pts',(29.6420960169785,-50.9621571865006,
40.1038990521418));
#174998=CARTESIAN_POINT('Ctrl Pts',(29.6515989823495,-50.9610854798926,
40.097736013771));
#174999=CARTESIAN_POINT('Ctrl Pts',(29.6608932776208,-50.9604313483967,
40.0911601532641));
#175000=CARTESIAN_POINT('Ctrl Pts',(29.6699181168562,-50.960195005077,40.084220729064));
#175001=CARTESIAN_POINT('Ctrl Pts',(29.6789043977155,-50.9599596715277,
40.0773109533618));
#175002=CARTESIAN_POINT('Ctrl Pts',(29.6876236029356,-50.9601383261074,
40.0700409753048));
#175003=CARTESIAN_POINT('Ctrl Pts',(29.6960154736015,-50.9607318934964,
40.0624586415899));
#175004=CARTESIAN_POINT('Ctrl Pts',(29.6960514814794,-50.9607344403781,
40.0624261072769));
#175005=CARTESIAN_POINT('Ctrl Pts',(29.6960874835161,-50.9607369943869,
40.0623935677888));
#175006=CARTESIAN_POINT('Ctrl Pts',(29.69612347971,-50.9607395555212,40.0623610231288));
#175007=CARTESIAN_POINT('Ctrl Pts',(29.7130985928867,-50.9619473372422,
40.0470135870252));
#175008=CARTESIAN_POINT('Ctrl Pts',(29.7287537227735,-50.9647087325278,
40.0305755292133));
#175009=CARTESIAN_POINT('Ctrl Pts',(29.7430502978434,-50.9688330949306,
40.0133447567401));
#175010=CARTESIAN_POINT('Ctrl Pts',(29.7578669541839,-50.9731074935224,
39.9954871626683));
#175011=CARTESIAN_POINT('Ctrl Pts',(29.7712250678519,-50.9788464019604,
39.9767767954429));
#175012=CARTESIAN_POINT('Ctrl Pts',(29.7830467300236,-50.9858763526636,
39.9575197577617));
#175013=CARTESIAN_POINT('Ctrl Pts',(29.794699670551,-50.9928059701967,39.9385375612167));
#175014=CARTESIAN_POINT('Ctrl Pts',(29.8048600966396,-51.0009908790831,
39.9190226977294));
#175015=CARTESIAN_POINT('Ctrl Pts',(29.8134126013553,-51.0102908030958,
39.8992655452084));
#175016=CARTESIAN_POINT('Ctrl Pts',(29.8193755598108,-51.0167748755835,
39.8854905069479));
#175017=CARTESIAN_POINT('Ctrl Pts',(29.8245560588464,-51.0238015157329,
39.8715976051552));
#175018=CARTESIAN_POINT('Ctrl Pts',(29.8289013456884,-51.0313275753409,
39.8576902534424));
#175019=CARTESIAN_POINT('',(30.0070536838157,-51.3398895692698,39.2875012672119));
#175020=CARTESIAN_POINT('',(29.8289013456884,-51.0313275753409,39.8576902534424));
#175021=CARTESIAN_POINT('',(34.6963546279284,-48.2946219293747,39.2875012672119));
#175022=CARTESIAN_POINT('Origin',(5.53234440788222E-15,0.,39.2875012672119));
#175023=CARTESIAN_POINT('',(34.4869303039396,-48.0063682005188,39.8576902534424));
#175024=CARTESIAN_POINT('',(34.6963546279284,-48.2946219293747,39.2875012672119));
#175025=CARTESIAN_POINT('',(34.6205005703634,-47.6769115920305,40.1599502534424));
#175026=CARTESIAN_POINT('Ctrl Pts',(34.4869303039396,-48.0063682005188,
39.8576902534424));
#175027=CARTESIAN_POINT('Ctrl Pts',(34.4797418300849,-47.9964738715081,
39.8772619994068));
#175028=CARTESIAN_POINT('Ctrl Pts',(34.4741406737004,-47.9854941018754,
39.8967644650398));
#175029=CARTESIAN_POINT('Ctrl Pts',(34.4701636441718,-47.9736072089088,
39.9159282836089));
#175030=CARTESIAN_POINT('Ctrl Pts',(34.4661147749664,-47.9615055952461,
39.9354382707247));
#175031=CARTESIAN_POINT('Ctrl Pts',(34.4637486663026,-47.9484630606955,
39.9545987622433));
#175032=CARTESIAN_POINT('Ctrl Pts',(34.4631421240615,-47.9346304384564,
39.9731387498325));
#175033=CARTESIAN_POINT('Ctrl Pts',(34.4625612612463,-47.9213834535785,
39.9908938024167));
#175034=CARTESIAN_POINT('Ctrl Pts',(34.4635939836577,-47.9074110114703,
40.0080810366309));
#175035=CARTESIAN_POINT('Ctrl Pts',(34.4663468279024,-47.8928237488832,
40.024454274268));
#175036=CARTESIAN_POINT('Ctrl Pts',(34.4685363496885,-47.8812215199175,
40.0374770090575));
#175037=CARTESIAN_POINT('Ctrl Pts',(34.4718146898385,-47.8692298237612,
40.0499848770081));
#175038=CARTESIAN_POINT('Ctrl Pts',(34.4762554502657,-47.8568987993928,
40.0618424270193));
#175039=CARTESIAN_POINT('Ctrl Pts',(34.4762675720991,-47.8568651397018,
40.0618747942791));
#175040=CARTESIAN_POINT('Ctrl Pts',(34.4762797026733,-47.8568314776415,
40.0619071564124));
#175041=CARTESIAN_POINT('Ctrl Pts',(34.4762918419889,-47.8567978132139,
40.0619395134161));
#175042=CARTESIAN_POINT('Ctrl Pts',(34.4787083945375,-47.8500962938265,
40.0683807661799));
#175043=CARTESIAN_POINT('Ctrl Pts',(34.4815044004731,-47.8432853991339,
40.0746073439084));
#175044=CARTESIAN_POINT('Ctrl Pts',(34.4846629347251,-47.8364019332939,
40.0805869293669));
#175045=CARTESIAN_POINT('Ctrl Pts',(34.4909312646828,-47.8227412186411,
40.092453830807));
#175046=CARTESIAN_POINT('Ctrl Pts',(34.4986286886042,-47.8087940876656,
40.1033475319609));
#175047=CARTESIAN_POINT('Ctrl Pts',(34.5076305235176,-47.7948446809466,
40.1130129263075));
#175048=CARTESIAN_POINT('Ctrl Pts',(34.5143818997026,-47.7843826259073,
40.1202619720674));
#175049=CARTESIAN_POINT('Ctrl Pts',(34.5218670065994,-47.7739192901008,
40.1268200947266));
#175050=CARTESIAN_POINT('Ctrl Pts',(34.5300332501818,-47.763574554582,40.1325796782703));
#175051=CARTESIAN_POINT('Ctrl Pts',(34.5330955915252,-47.7596952787624,
40.1347395220992));
#175052=CARTESIAN_POINT('Ctrl Pts',(34.5362537178264,-47.7558326812643,
40.1367870714852));
#175053=CARTESIAN_POINT('Ctrl Pts',(34.5395048560464,-47.7519930846016,
40.1387166518767));
#175054=CARTESIAN_POINT('Ctrl Pts',(34.5508838398164,-47.7385544962821,
40.1454701832469));
#175055=CARTESIAN_POINT('Ctrl Pts',(34.5634022166003,-47.7253976640913,
40.1507785912492));
#175056=CARTESIAN_POINT('Ctrl Pts',(34.5769411196453,-47.7127937034783,
40.1543986087265));
#175057=CARTESIAN_POINT('Ctrl Pts',(34.5837105711679,-47.7064917231718,
40.1562086174652));
#175058=CARTESIAN_POINT('Ctrl Pts',(34.5907351548565,-47.7003279615825,
40.1575965292115));
#175059=CARTESIAN_POINT('Ctrl Pts',(34.598000014936,-47.6943363116299,40.1585319382567));
#175060=CARTESIAN_POINT('Ctrl Pts',(34.6016324449757,-47.6913404866536,
40.1589996427793));
#175061=CARTESIAN_POINT('Ctrl Pts',(34.6053249441285,-47.6883876896068,
40.159354221642));
#175062=CARTESIAN_POINT('Ctrl Pts',(34.6090756555951,-47.685482157339,40.159591874311));
#175063=CARTESIAN_POINT('Ctrl Pts',(34.6128263670618,-47.6825766250712,
40.1598295269801));
#175064=CARTESIAN_POINT('Ctrl Pts',(34.6166352918409,-47.6797183589577,
40.1599502506895));
#175065=CARTESIAN_POINT('Ctrl Pts',(34.6205005703634,-47.6769115920305,
40.1599502534424));
#175066=CARTESIAN_POINT('',(34.6451144164185,-47.6590285860936,40.1599502534424));
#175067=CARTESIAN_POINT('Origin',(5.69524824702573E-15,5.19758617760539E-15,
40.1599502534424));
#175068=CARTESIAN_POINT('',(34.9997217530259,-47.63380340476,39.8576902534424));
#175069=CARTESIAN_POINT('Ctrl Pts',(34.6451144164185,-47.6590285860936,
40.1599502534424));
#175070=CARTESIAN_POINT('Ctrl Pts',(34.648196040315,-47.6567884460682,40.1599502448875));
#175071=CARTESIAN_POINT('Ctrl Pts',(34.651296885817,-47.6545924528204,40.1598743450437));
#175072=CARTESIAN_POINT('Ctrl Pts',(34.6544147487634,-47.6524408584472,
40.1597243308499));
#175073=CARTESIAN_POINT('Ctrl Pts',(34.6728223758152,-47.6397380079788,
40.1588386583939));
#175074=CARTESIAN_POINT('Ctrl Pts',(34.6918243519396,-47.6285798336136,
40.1553722553623));
#175075=CARTESIAN_POINT('Ctrl Pts',(34.7109619288031,-47.6190225715805,
40.14969021778));
#175076=CARTESIAN_POINT('Ctrl Pts',(34.7181110904596,-47.6154522966311,
40.1475675976853));
#175077=CARTESIAN_POINT('Ctrl Pts',(34.7252793254645,-47.6121050440165,
40.1451361443101));
#175078=CARTESIAN_POINT('Ctrl Pts',(34.7324433913425,-47.6089824432866,
40.1424159447501));
#175079=CARTESIAN_POINT('Ctrl Pts',(34.7380331549251,-47.6065460335523,
40.1402935085949));
#175080=CARTESIAN_POINT('Ctrl Pts',(34.7436201516876,-47.6042468425533,
40.1379949176048));
#175081=CARTESIAN_POINT('Ctrl Pts',(34.7491931041024,-47.6020860928989,
40.1355293609261));
#175082=CARTESIAN_POINT('Ctrl Pts',(34.7686984375539,-47.5945234691088,
40.1268999125509));
#175083=CARTESIAN_POINT('Ctrl Pts',(34.7880317224283,-47.5886567445951,
40.1162251288835));
#175084=CARTESIAN_POINT('Ctrl Pts',(34.8067094890034,-47.5845384124875,
40.1038990521418));
#175085=CARTESIAN_POINT('Ctrl Pts',(34.8160483722909,-47.5824792464336,
40.097736013771));
#175086=CARTESIAN_POINT('Ctrl Pts',(34.8252233770802,-47.5808571799366,
40.0911601532641));
#175087=CARTESIAN_POINT('Ctrl Pts',(34.8341740726979,-47.5796787787539,
40.084220729064));
#175088=CARTESIAN_POINT('Ctrl Pts',(34.8430865267162,-47.5785054122577,
40.0773109533618));
#175089=CARTESIAN_POINT('Ctrl Pts',(34.8517766417065,-47.5777716830263,
40.0700409753048));
#175090=CARTESIAN_POINT('Ctrl Pts',(34.8601845855138,-47.5774848094464,
40.0624586415899));
#175091=CARTESIAN_POINT('Ctrl Pts',(34.8602206623585,-47.5774835785279,
40.0624261072769));
#175092=CARTESIAN_POINT('Ctrl Pts',(34.8602567341388,-47.577482355308,40.0623935677889));
#175093=CARTESIAN_POINT('Ctrl Pts',(34.8602928008533,-47.5774811397853,
40.0623610231288));
#175094=CARTESIAN_POINT('Ctrl Pts',(34.8773011701546,-47.5769079226574,
40.047013587022));
#175095=CARTESIAN_POINT('Ctrl Pts',(34.8931591840106,-47.5780177840619,
40.0305755292066));
#175096=CARTESIAN_POINT('Ctrl Pts',(34.9078085542128,-47.580625153755,40.0133447567296));
#175097=CARTESIAN_POINT('Ctrl Pts',(34.9229908396783,-47.5833273744273,
39.9954871626538));
#175098=CARTESIAN_POINT('Ctrl Pts',(34.9368756554839,-47.5876385414323,
39.976776795424));
#175099=CARTESIAN_POINT('Ctrl Pts',(34.9493673872986,-47.5933942811523,
39.9575197577385));
#175100=CARTESIAN_POINT('Ctrl Pts',(34.9616808340714,-47.5990678735518,
39.9385375611895));
#175101=CARTESIAN_POINT('Ctrl Pts',(34.9726411562313,-47.6061458909284,
39.9190226976982));
#175102=CARTESIAN_POINT('Ctrl Pts',(34.9821189161968,-47.6145008888124,
39.8992655451732));
#175103=CARTESIAN_POINT('Ctrl Pts',(34.9887269790679,-47.6203261419847,
39.8854905069243));
#175104=CARTESIAN_POINT('Ctrl Pts',(34.9946135826789,-47.626772779856,39.8715976051433));
#175105=CARTESIAN_POINT('Ctrl Pts',(34.9997217530259,-47.6338034047601,
39.8576902534424));
#175106=CARTESIAN_POINT('',(35.2091516650527,-47.9220530736688,39.2875012672119));
#175107=CARTESIAN_POINT('',(34.9997217530259,-47.63380340476,39.8576902534424));
#175108=CARTESIAN_POINT('',(39.554446981307,-44.403302307049,39.2875012672119));
#175109=CARTESIAN_POINT('Origin',(5.53234440788222E-15,0.,39.2875012672119));
#175110=CARTESIAN_POINT('',(39.3160391863689,-44.1385184650376,39.8576902534424));
#175111=CARTESIAN_POINT('',(39.554446981307,-44.403302307049,39.2875012672119));
#175112=CARTESIAN_POINT('',(39.4144401478989,-43.7969047596347,40.1599502534424));
#175113=CARTESIAN_POINT('Ctrl Pts',(39.3160391863689,-44.1385184650377,
39.8576902534424));
#175114=CARTESIAN_POINT('Ctrl Pts',(39.3078558527209,-44.1294297383233,
39.8772619994037));
#175115=CARTESIAN_POINT('Ctrl Pts',(39.3011376816113,-44.1190955972887,
39.8967644650336));
#175116=CARTESIAN_POINT('Ctrl Pts',(39.2959399200121,-44.1076895347526,
39.9159282835998));
#175117=CARTESIAN_POINT('Ctrl Pts',(39.2906482678569,-44.0960774370739,
39.9354382707125));
#175118=CARTESIAN_POINT('Ctrl Pts',(39.2869318048902,-44.0833536765974,
39.9545987622282));
#175119=CARTESIAN_POINT('Ctrl Pts',(39.2848826826046,-44.0696602318415,
39.9731387498148));
#175120=CARTESIAN_POINT('Ctrl Pts',(39.2829203148437,-44.0565465320328,
39.9908938023966));
#175121=CARTESIAN_POINT('Ctrl Pts',(39.2824868619908,-44.0425426835408,
40.0080810366086));
#175122=CARTESIAN_POINT('Ctrl Pts',(39.2836998417234,-44.0277475809291,
40.0244542742439));
#175123=CARTESIAN_POINT('Ctrl Pts',(39.284664605915,-44.0159800428334,40.037477009042));
#175124=CARTESIAN_POINT('Ctrl Pts',(39.286671513404,-44.0037113585782,40.0499848770007));
#175125=CARTESIAN_POINT('Ctrl Pts',(39.2897990038552,-43.9909836989804,
40.0618424270192));
#175126=CARTESIAN_POINT('Ctrl Pts',(39.2898075408882,-43.9909489566041,
40.0618747942791));
#175127=CARTESIAN_POINT('Ctrl Pts',(39.2898160863664,-43.9909142109578,
40.0619071564124));
#175128=CARTESIAN_POINT('Ctrl Pts',(39.2898246402906,-43.9908794620434,
40.0619395134161));
#175129=CARTESIAN_POINT('Ctrl Pts',(39.2915274551884,-43.9839620557562,
40.0683807661799));
#175130=CARTESIAN_POINT('Ctrl Pts',(39.2935962119552,-43.9768962096536,
40.0746073439084));
#175131=CARTESIAN_POINT('Ctrl Pts',(39.2960179253199,-43.9697202954281,
40.0805869293669));
#175132=CARTESIAN_POINT('Ctrl Pts',(39.3008239832004,-43.9554791967018,
40.092453830807));
#175133=CARTESIAN_POINT('Ctrl Pts',(39.3070213676603,-43.9408038696755,
40.1033475319609));
#175134=CARTESIAN_POINT('Ctrl Pts',(39.3145157795323,-43.925989931296,40.1130129263075));
#175135=CARTESIAN_POINT('Ctrl Pts',(39.3201365884364,-43.9148794775113,
40.1202619720674));
#175136=CARTESIAN_POINT('Ctrl Pts',(39.3264869747219,-43.9036910542318,
40.1268200947266));
#175137=CARTESIAN_POINT('Ctrl Pts',(39.3335271634607,-43.8925493833642,
40.1325796782703));
#175138=CARTESIAN_POINT('Ctrl Pts',(39.3361672342378,-43.8883712567889,
40.1347395220992));
#175139=CARTESIAN_POINT('Ctrl Pts',(39.338904308612,-43.8841997049149,40.1367870714852));
#175140=CARTESIAN_POINT('Ctrl Pts',(39.341736289618,-43.8800413054825,40.1387166518767));
#175141=CARTESIAN_POINT('Ctrl Pts',(39.3516482231388,-43.8654869074688,
40.1454701832469));
#175142=CARTESIAN_POINT('Ctrl Pts',(39.3627227594944,-43.8510936230936,
40.1507785912492));
#175143=CARTESIAN_POINT('Ctrl Pts',(39.374870022378,-43.8371435075659,40.1543986087265));
#175144=CARTESIAN_POINT('Ctrl Pts',(39.3809436538198,-43.8301684498021,
40.1562086174652));
#175145=CARTESIAN_POINT('Ctrl Pts',(39.3872854675771,-43.8233041850057,
40.1575965292115));
#175146=CARTESIAN_POINT('Ctrl Pts',(39.393884232031,-43.8165859732785,40.1585319382567));
#175147=CARTESIAN_POINT('Ctrl Pts',(39.3971836142579,-43.8132268674149,
40.1589996427793));
#175148=CARTESIAN_POINT('Ctrl Pts',(39.4005472341764,-43.8099042748372,
40.159354221642));
#175149=CARTESIAN_POINT('Ctrl Pts',(39.4039736880302,-43.8066226032735,
40.1595918743111));
#175150=CARTESIAN_POINT('Ctrl Pts',(39.4074001418841,-43.8033409317097,
40.1598295269801));
#175151=CARTESIAN_POINT('Ctrl Pts',(39.4108894308102,-43.8001001824231,
40.1599502506895));
#175152=CARTESIAN_POINT('Ctrl Pts',(39.4144401478989,-43.7969047596347,
40.1599502534424));
#175153=CARTESIAN_POINT('',(39.4370498736007,-43.7765468711723,40.1599502534424));
#175154=CARTESIAN_POINT('Origin',(5.70079064675565E-15,5.20207432441226E-15,
40.1599502534424));
#175155=CARTESIAN_POINT('',(39.7870778846746,-43.7143933160624,39.8576902534424));
#175156=CARTESIAN_POINT('Ctrl Pts',(39.4370498736007,-43.7765468711723,
40.1599502534424));
#175157=CARTESIAN_POINT('Ctrl Pts',(39.4398804576448,-43.773996885458,40.1599502448875));
#175158=CARTESIAN_POINT('Ctrl Pts',(39.4427347725911,-43.7714887954758,
40.1598743450437));
#175159=CARTESIAN_POINT('Ctrl Pts',(39.4456106527046,-43.7690230823392,
40.1597243308499));
#175160=CARTESIAN_POINT('Ctrl Pts',(39.4625896314128,-43.7544656984451,
40.1588386583938));
#175161=CARTESIAN_POINT('Ctrl Pts',(39.4803211659066,-43.741382402362,40.1553722553615));
#175162=CARTESIAN_POINT('Ctrl Pts',(39.4983548992104,-43.7298770745092,
40.1496902177781));
#175163=CARTESIAN_POINT('Ctrl Pts',(39.5050917016554,-43.7255790670193,
40.1475675976838));
#175164=CARTESIAN_POINT('Ctrl Pts',(39.5118707851449,-43.7215008664166,
40.1451361443093));
#175165=CARTESIAN_POINT('Ctrl Pts',(39.5186692048627,-43.7176465228244,
40.1424159447501));
#175166=CARTESIAN_POINT('Ctrl Pts',(39.5239736729701,-43.7146391706002,
40.1402935085949));
#175167=CARTESIAN_POINT('Ctrl Pts',(39.5292897326779,-43.7117685746242,
40.1379949176048));
#175168=CARTESIAN_POINT('Ctrl Pts',(39.5346062960353,-43.7090371296308,
40.1355293609261));
#175169=CARTESIAN_POINT('Ctrl Pts',(39.5532142677863,-43.6994770721539,
40.1268999125508));
#175170=CARTESIAN_POINT('Ctrl Pts',(39.5718284032055,-43.691621607613,40.1162251288835));
#175171=CARTESIAN_POINT('Ctrl Pts',(39.5899733680945,-43.6855734779223,
40.1038990521418));
#175172=CARTESIAN_POINT('Ctrl Pts',(39.599045850539,-43.6825494130769,40.0977360137709));
#175173=CARTESIAN_POINT('Ctrl Pts',(39.6080010415738,-43.6799771832788,
40.0911601532641));
#175174=CARTESIAN_POINT('Ctrl Pts',(39.6167795278797,-43.6778696350429,
40.084220729064));
#175175=CARTESIAN_POINT('Ctrl Pts',(39.6255205083456,-43.6757710912486,
40.0773109533618));
#175176=CARTESIAN_POINT('Ctrl Pts',(39.6340863223877,-43.6741330170972,
40.0700409753048));
#175177=CARTESIAN_POINT('Ctrl Pts',(39.6424182201447,-43.6729688455953,
40.0624586415899));
#175178=CARTESIAN_POINT('Ctrl Pts',(39.6424539706906,-43.6729638503628,
40.0624261072769));
#175179=CARTESIAN_POINT('Ctrl Pts',(39.6424897170046,-43.6729588633161,
40.0623935677889));
#175180=CARTESIAN_POINT('Ctrl Pts',(39.6425254590851,-43.6729538844539,
40.0623610231289));
#175181=CARTESIAN_POINT('Ctrl Pts',(39.6593807372547,-43.6706059487636,
40.0470135870217));
#175182=CARTESIAN_POINT('Ctrl Pts',(39.6752678913589,-43.6700521164124,
40.0305755292057));
#175183=CARTESIAN_POINT('Ctrl Pts',(39.6901095551258,-43.6711139265066,
40.0133447567283));
#175184=CARTESIAN_POINT('Ctrl Pts',(39.7054911294178,-43.6722143631629,
39.9954871626517));
#175185=CARTESIAN_POINT('Ctrl Pts',(39.7197505224119,-43.6750505546854,
39.9767767954212));
#175186=CARTESIAN_POINT('Ctrl Pts',(39.7327754618409,-43.6794690223312,
39.9575197577348));
#175187=CARTESIAN_POINT('Ctrl Pts',(39.7456145061592,-43.6838244285297,
39.9385375611848));
#175188=CARTESIAN_POINT('Ctrl Pts',(39.7572546408072,-43.6897180061549,
39.9190226976923));
#175189=CARTESIAN_POINT('Ctrl Pts',(39.7675538157017,-43.6970365388026,
39.8992655451661));
#175190=CARTESIAN_POINT('Ctrl Pts',(39.7747345836738,-43.7021391499707,
39.8854905069195));
#175191=CARTESIAN_POINT('Ctrl Pts',(39.7812627970031,-43.707935154855,39.8715976051409));
#175192=CARTESIAN_POINT('Ctrl Pts',(39.7870778846746,-43.7143933160624,
39.8576902534424));
#175193=CARTESIAN_POINT('',(40.0254908126588,-43.9791725362583,39.2875012672119));
#175194=CARTESIAN_POINT('',(39.7870778846746,-43.7143933160624,39.8576902534424));
#175195=CARTESIAN_POINT('',(43.9791725362582,-40.0254908126589,39.2875012672119));
#175196=CARTESIAN_POINT('Origin',(5.53234440788222E-15,0.,39.2875012672119));
#175197=CARTESIAN_POINT('',(43.7143933160623,-39.7870778846748,39.8576902534424));
#175198=CARTESIAN_POINT('',(43.9791725362582,-40.0254908126589,39.2875012672119));
#175199=CARTESIAN_POINT('',(43.7765468711722,-39.4370498736009,40.1599502534424));
#175200=CARTESIAN_POINT('Ctrl Pts',(43.7143933160623,-39.7870778846748,
39.8576902534424));
#175201=CARTESIAN_POINT('Ctrl Pts',(43.7053047809348,-39.7788943382461,
39.8772619994057));
#175202=CARTESIAN_POINT('Ctrl Pts',(43.6975432007873,-39.7693190488183,
39.8967644650376));
#175203=CARTESIAN_POINT('Ctrl Pts',(43.6911816548807,-39.7585187839172,
39.9159282836057));
#175204=CARTESIAN_POINT('Ctrl Pts',(43.6847051962237,-39.7475234267912,
39.9354382707203));
#175205=CARTESIAN_POINT('Ctrl Pts',(43.6796790973003,-39.735257844567,39.9545987622378));
#175206=CARTESIAN_POINT('Ctrl Pts',(43.6762098455841,-39.7218536055359,
39.9731387498261));
#175207=CARTESIAN_POINT('Ctrl Pts',(43.6728874729907,-39.7090168672317,
39.9908938024093));
#175208=CARTESIAN_POINT('Ctrl Pts',(43.6709925938757,-39.6951350414458,
40.0080810366227));
#175209=CARTESIAN_POINT('Ctrl Pts',(43.6706524194394,-39.6802941970447,
40.024454274259));
#175210=CARTESIAN_POINT('Ctrl Pts',(43.6703818558792,-39.6684902774397,
40.0374770090517));
#175211=CARTESIAN_POINT('Ctrl Pts',(43.6710953426076,-39.6560790233694,
40.0499848770053));
#175212=CARTESIAN_POINT('Ctrl Pts',(43.6728752976393,-39.6430941754569,
40.0618424270193));
#175213=CARTESIAN_POINT('Ctrl Pts',(43.6728801563384,-39.64305873104,40.0618747942791));
#175214=CARTESIAN_POINT('Ctrl Pts',(43.6728850230945,-39.6430232824883,
40.0619071564124));
#175215=CARTESIAN_POINT('Ctrl Pts',(43.6728898979088,-39.6429878298035,
40.0619395134161));
#175216=CARTESIAN_POINT('Ctrl Pts',(43.6738603187595,-39.6359303251672,
40.0683807661799));
#175217=CARTESIAN_POINT('Ctrl Pts',(43.6751791606254,-39.6286869425432,
40.0746073439084));
#175218=CARTESIAN_POINT('Ctrl Pts',(43.6768375203044,-39.6212972007502,
40.0805869293669));
#175219=CARTESIAN_POINT('Ctrl Pts',(43.6801286499319,-39.6066317464081,
40.092453830807));
#175220=CARTESIAN_POINT('Ctrl Pts',(43.6847580950893,-39.5913890092849,
40.1033475319609));
#175221=CARTESIAN_POINT('Ctrl Pts',(43.6906629735752,-39.5758728438537,
40.1130129263075));
#175222=CARTESIAN_POINT('Ctrl Pts',(43.6950916324396,-39.5642357197803,
40.1202619720674));
#175223=CARTESIAN_POINT('Ctrl Pts',(43.7002377219528,-39.5524447917346,
40.1268200947266));
#175224=CARTESIAN_POINT('Ctrl Pts',(43.7060747220671,-39.5406282559958,
40.1325796782703));
#175225=CARTESIAN_POINT('Ctrl Pts',(43.70826359711,-39.5361970550938,40.1347395220992));
#175226=CARTESIAN_POINT('Ctrl Pts',(43.7105496315975,-39.5317622532393,
40.1367870714852));
#175227=CARTESIAN_POINT('Ctrl Pts',(43.7129314276129,-39.5273306113315,
40.1387166518767));
#175228=CARTESIAN_POINT('Ctrl Pts',(43.7212677136666,-39.5118198646541,
40.1454701832469));
#175229=CARTESIAN_POINT('Ctrl Pts',(43.7307770746562,-39.49634782393,40.1507785912491));
#175230=CARTESIAN_POINT('Ctrl Pts',(43.7413996094243,-39.4812043938727,
40.1543986087265));
#175231=CARTESIAN_POINT('Ctrl Pts',(43.7467108768083,-39.473632678844,40.1562086174652));
#175232=CARTESIAN_POINT('Ctrl Pts',(43.7523004383956,-39.4661431171621,
40.1575965292115));
#175233=CARTESIAN_POINT('Ctrl Pts',(43.7581608097796,-39.4587719497938,
40.1585319382567));
#175234=CARTESIAN_POINT('Ctrl Pts',(43.7610909954716,-39.4550863661096,
40.1589996427793));
#175235=CARTESIAN_POINT('Ctrl Pts',(43.764088883632,-39.4514303810207,40.159354221642));
#175236=CARTESIAN_POINT('Ctrl Pts',(43.7671535389276,-39.4478085248413,
40.159591874311));
#175237=CARTESIAN_POINT('Ctrl Pts',(43.7702181942232,-39.4441866686619,
40.1598295269801));
#175238=CARTESIAN_POINT('Ctrl Pts',(43.7733496179168,-39.4405989425296,
40.1599502506895));
#175239=CARTESIAN_POINT('Ctrl Pts',(43.7765468711722,-39.4370498736009,
40.1599502534424));
#175240=CARTESIAN_POINT('',(43.7969047596346,-39.414440147899,40.1599502534424));
#175241=CARTESIAN_POINT('Origin',(5.7058335455513E-15,5.20711722320791E-15,
40.1599502534424));
#175242=CARTESIAN_POINT('',(44.1385184650375,-39.3160391863691,39.8576902534424));
#175243=CARTESIAN_POINT('Ctrl Pts',(43.7969047596346,-39.414440147899,40.1599502534424));
#175244=CARTESIAN_POINT('Ctrl Pts',(43.799453291355,-39.411608254673,40.1599502448875));
#175245=CARTESIAN_POINT('Ctrl Pts',(43.8020298032738,-39.4088155471152,
40.1598743450437));
#175246=CARTESIAN_POINT('Ctrl Pts',(43.8046321918101,-39.4060627300843,
40.1597243308499));
#175247=CARTESIAN_POINT('Ctrl Pts',(43.8199964969274,-39.3898103065115,
40.1588386583939));
#175248=CARTESIAN_POINT('Ctrl Pts',(43.8362633193845,-39.3749452320424,
40.1553722553621));
#175249=CARTESIAN_POINT('Ctrl Pts',(43.8529956277689,-39.3616178931511,
40.1496902177795));
#175250=CARTESIAN_POINT('Ctrl Pts',(43.8592462611886,-39.3566392429878,
40.147567597685));
#175251=CARTESIAN_POINT('Ctrl Pts',(43.865561920109,-39.351874776014,40.1451361443099));
#175252=CARTESIAN_POINT('Ctrl Pts',(43.8719202087611,-39.3473309185525,
40.1424159447501));
#175253=CARTESIAN_POINT('Ctrl Pts',(43.8768812645308,-39.3437855730187,
40.1402935085949));
#175254=CARTESIAN_POINT('Ctrl Pts',(43.8818681433212,-39.3403750229159,
40.1379949176048));
#175255=CARTESIAN_POINT('Ctrl Pts',(43.8868700682406,-39.3371028088664,
40.1355293609261));
#175256=CARTESIAN_POINT('Ctrl Pts',(43.9043768054585,-39.325650059693,40.1268999125508));
#175257=CARTESIAN_POINT('Ctrl Pts',(43.9220678510596,-39.3158919212384,
40.1162251288835));
#175258=CARTESIAN_POINT('Ctrl Pts',(43.9394812142301,-39.307980258539,40.1038990521418));
#175259=CARTESIAN_POINT('Ctrl Pts',(43.9481878958154,-39.3040244271893,
40.0977360137709));
#175260=CARTESIAN_POINT('Ctrl Pts',(43.9568251581488,-39.300530215978,40.0911601532641));
#175261=CARTESIAN_POINT('Ctrl Pts',(43.9653352562098,-39.2975166114285,
40.084220729064));
#175262=CARTESIAN_POINT('Ctrl Pts',(43.9738089951123,-39.2945158824212,
40.0773109533618));
#175263=CARTESIAN_POINT('Ctrl Pts',(43.982156659355,-39.2919914104329,40.0700409753048));
#175264=CARTESIAN_POINT('Ctrl Pts',(43.9903212250463,-39.2899626959157,
40.0624586415899));
#175265=CARTESIAN_POINT('Ctrl Pts',(43.9903562576029,-39.2899539910979,
40.0624261072769));
#175266=CARTESIAN_POINT('Ctrl Pts',(43.9903912868066,-39.2899452948635,
40.0623935677889));
#175267=CARTESIAN_POINT('Ctrl Pts',(43.9904263126554,-39.2899366072113,
40.0623610231288));
#175268=CARTESIAN_POINT('Ctrl Pts',(44.006943829738,-39.2858396774333,40.0470135870217));
#175269=CARTESIAN_POINT('Ctrl Pts',(44.0226860611052,-39.2836282192294,
40.0305755292057));
#175270=CARTESIAN_POINT('Ctrl Pts',(44.0375574100625,-39.283132836311,40.0133447567283));
#175271=CARTESIAN_POINT('Ctrl Pts',(44.0529697494336,-39.2826194323366,
39.995487162652));
#175272=CARTESIAN_POINT('Ctrl Pts',(44.0674474907222,-39.2839495744683,
39.9767767954217));
#175273=CARTESIAN_POINT('Ctrl Pts',(44.080862933803,-39.2869823603832,39.9575197577357));
#175274=CARTESIAN_POINT('Ctrl Pts',(44.0940869084097,-39.2899718616383,
39.9385375611862));
#175275=CARTESIAN_POINT('Ctrl Pts',(44.1062793237942,-39.2946164282413,
39.9190226976944));
#175276=CARTESIAN_POINT('Ctrl Pts',(44.1172870737017,-39.3008183122765,
39.8992655451689));
#175277=CARTESIAN_POINT('Ctrl Pts',(44.1249618727802,-39.3051423761658,
39.8854905069213));
#175278=CARTESIAN_POINT('Ctrl Pts',(44.1320601713578,-39.310224245822,39.8715976051418));
#175279=CARTESIAN_POINT('Ctrl Pts',(44.1385184650375,-39.3160391863691,
39.8576902534424));
#175280=CARTESIAN_POINT('',(44.4033023070489,-39.5544469813072,39.2875012672119));
#175281=CARTESIAN_POINT('',(44.1385184650375,-39.3160391863691,39.8576902534424));
#175282=CARTESIAN_POINT('',(47.9220530736687,-35.2091516650529,39.2875012672119));
#175283=CARTESIAN_POINT('Origin',(5.53234440788222E-15,0.,39.2875012672119));
#175284=CARTESIAN_POINT('',(47.6338034047599,-34.9997217530261,39.8576902534424));
#175285=CARTESIAN_POINT('',(47.9220530736687,-35.2091516650529,39.2875012672119));
#175286=CARTESIAN_POINT('',(47.6590285860935,-34.6451144164186,40.1599502534424));
#175287=CARTESIAN_POINT('Ctrl Pts',(47.6338034047599,-34.9997217530261,
39.8576902534424));
#175288=CARTESIAN_POINT('Ctrl Pts',(47.6239092440476,-34.9925330475317,
39.8772619994039));
#175289=CARTESIAN_POINT('Ctrl Pts',(47.6151892923597,-34.9838215185875,
39.8967644650341));
#175290=CARTESIAN_POINT('Ctrl Pts',(47.6077336605747,-34.9737453812864,
39.9159282836005));
#175291=CARTESIAN_POINT('Ctrl Pts',(47.600143352853,-34.9634872321492,39.9354382707132));
#175292=CARTESIAN_POINT('Ctrl Pts',(47.5938626849646,-34.951814212466,39.954598762229));
#175293=CARTESIAN_POINT('Ctrl Pts',(47.589011313665,-34.9388460388113,39.9731387498156));
#175294=CARTESIAN_POINT('Ctrl Pts',(47.584365336848,-34.9264269040061,39.990893802397));
#175295=CARTESIAN_POINT('Ctrl Pts',(47.581029792162,-34.9128191931185,40.0080810366088));
#175296=CARTESIAN_POINT('Ctrl Pts',(47.5791401905773,-34.8980952063294,
40.0244542742438));
#175297=CARTESIAN_POINT('Ctrl Pts',(47.5776372636143,-34.8863842314202,
40.037477009042));
#175298=CARTESIAN_POINT('Ctrl Pts',(47.5770495124719,-34.8739663878225,
40.0499848770007));
#175299=CARTESIAN_POINT('Ctrl Pts',(47.5774624305259,-34.8608666162962,
40.0618424270193));
#175300=CARTESIAN_POINT('Ctrl Pts',(47.5774635576581,-34.8608308581752,
40.0618747942791));
#175301=CARTESIAN_POINT('Ctrl Pts',(47.577464692371,-34.8607950950998,40.0619071564124));
#175302=CARTESIAN_POINT('Ctrl Pts',(47.5774658346659,-34.8607593270717,
40.0619395134161));
#175303=CARTESIAN_POINT('Ctrl Pts',(47.5776932293355,-34.853639047584,40.0683807661799));
#175304=CARTESIAN_POINT('Ctrl Pts',(47.5782477067931,-34.8462974884544,
40.0746073439084));
#175305=CARTESIAN_POINT('Ctrl Pts',(47.5791245434507,-34.8387748826513,
40.0805869293668));
#175306=CARTESIAN_POINT('Ctrl Pts',(47.5808646865202,-34.8238457504803,
40.092453830807));
#175307=CARTESIAN_POINT('Ctrl Pts',(47.5838754712052,-34.8082026058778,
40.1033475319609));
#175308=CARTESIAN_POINT('Ctrl Pts',(47.5881261212205,-34.7921542117504,
40.1130129263075));
#175309=CARTESIAN_POINT('Ctrl Pts',(47.591314108732,-34.7801179161549,40.1202619720674));
#175310=CARTESIAN_POINT('Ctrl Pts',(47.5951995198393,-34.7678536672181,
40.1268200947266));
#175311=CARTESIAN_POINT('Ctrl Pts',(47.5997693799344,-34.7554917310464,
40.1325796782703));
#175312=CARTESIAN_POINT('Ctrl Pts',(47.60148307747,-34.750856004982,40.1347395220992));
#175313=CARTESIAN_POINT('Ctrl Pts',(47.6032930257987,-34.7462065417642,
40.1367870714852));
#175314=CARTESIAN_POINT('Ctrl Pts',(47.6051985413679,-34.7415502113771,
40.1387166518767));
#175315=CARTESIAN_POINT('Ctrl Pts',(47.6118678458601,-34.7252530550223,
40.1454701832469));
#175316=CARTESIAN_POINT('Ctrl Pts',(47.6197078449347,-34.7088717728653,
40.1507785912492));
#175317=CARTESIAN_POINT('Ctrl Pts',(47.6286892688733,-34.692700942867,40.1543986087265));
#175318=CARTESIAN_POINT('Ctrl Pts',(47.6331799808426,-34.6846155278679,
40.1562086174652));
#175319=CARTESIAN_POINT('Ctrl Pts',(47.6379560498536,-34.6765827265054,
40.1575965292115));
#175320=CARTESIAN_POINT('Ctrl Pts',(47.6430138207125,-34.6686393635482,
40.1585319382567));
#175321=CARTESIAN_POINT('Ctrl Pts',(47.6455427061419,-34.6646676820696,
40.1589996427793));
#175322=CARTESIAN_POINT('Ctrl Pts',(47.6481420170542,-34.6607183602071,
40.159354221642));
#175323=CARTESIAN_POINT('Ctrl Pts',(47.6508112967868,-34.6567960012263,
40.159591874311));
#175324=CARTESIAN_POINT('Ctrl Pts',(47.6534805765195,-34.6528736422456,
40.1598295269801));
#175325=CARTESIAN_POINT('Ctrl Pts',(47.6562198264472,-34.6489782471459,
40.1599502506895));
#175326=CARTESIAN_POINT('Ctrl Pts',(47.6590285860935,-34.6451144164186,
40.1599502534424));
#175327=CARTESIAN_POINT('',(47.6769115920304,-34.6205005703635,40.1599502534424));
#175328=CARTESIAN_POINT('Origin',(5.71032169235817E-15,5.21265962293783E-15,
40.1599502534424));
#175329=CARTESIAN_POINT('',(48.0063682005187,-34.4869303039397,39.8576902534424));
#175330=CARTESIAN_POINT('Ctrl Pts',(47.6769115920304,-34.6205005703635,
40.1599502534424));
#175331=CARTESIAN_POINT('Ctrl Pts',(47.6791501491803,-34.6174177964406,
40.1599502448875));
#175332=CARTESIAN_POINT('Ctrl Pts',(47.6814206292678,-34.6143710687955,
40.1598743450437));
#175333=CARTESIAN_POINT('Ctrl Pts',(47.6837210139136,-34.6113613083098,
40.1597243308499));
#175334=CARTESIAN_POINT('Ctrl Pts',(47.6973023109009,-34.5935919100088,
40.1588386583938));
#175335=CARTESIAN_POINT('Ctrl Pts',(47.7119261986137,-34.5771079220176,
40.1553722553613));
#175336=CARTESIAN_POINT('Ctrl Pts',(47.7271737594101,-34.5621045891995,
40.1496902177776));
#175337=CARTESIAN_POINT('Ctrl Pts',(47.7328697405536,-34.5564998434987,
40.1475675976835));
#175338=CARTESIAN_POINT('Ctrl Pts',(47.7386527792208,-34.5511013106537,
40.1451361443091));
#175339=CARTESIAN_POINT('Ctrl Pts',(47.7445012740629,-34.5459177227786,
40.1424159447501));
#175340=CARTESIAN_POINT('Ctrl Pts',(47.7490645631296,-34.5418732274828,
40.1402935085949));
#175341=CARTESIAN_POINT('Ctrl Pts',(47.7536676237151,-34.5379600899538,
40.1379949176048));
#175342=CARTESIAN_POINT('Ctrl Pts',(47.7583001080603,-34.53418295791,40.1355293609261));
#175343=CARTESIAN_POINT('Ctrl Pts',(47.7745138032687,-34.5209629957567,
40.1268999125509));
#175344=CARTESIAN_POINT('Ctrl Pts',(47.7910879322539,-34.5094090955953,
40.1162251288835));
#175345=CARTESIAN_POINT('Ctrl Pts',(47.8075789092552,-34.4997205817194,
40.1038990521418));
#175346=CARTESIAN_POINT('Ctrl Pts',(47.8158243977558,-34.4948763247815,
40.0977360137709));
#175347=CARTESIAN_POINT('Ctrl Pts',(47.8240490997342,-34.4904984154663,
40.0911601532641));
#175348=CARTESIAN_POINT('Ctrl Pts',(47.8321975711351,-34.4866117722853,
40.084220729064));
#175349=CARTESIAN_POINT('Ctrl Pts',(47.8403112284174,-34.4827417346798,
40.0773109533618));
#175350=CARTESIAN_POINT('Ctrl Pts',(47.8483492841045,-34.479358523498,40.0700409753047));
#175351=CARTESIAN_POINT('Ctrl Pts',(47.8562570650397,-34.4764874929863,
40.0624586415899));
#175352=CARTESIAN_POINT('Ctrl Pts',(47.8562909957831,-34.4764751739551,
40.0624261072769));
#175353=CARTESIAN_POINT('Ctrl Pts',(47.8563249240891,-34.4764628638107,
40.0623935677888));
#175354=CARTESIAN_POINT('Ctrl Pts',(47.8563588499558,-34.4764505625523,
40.0623610231288));
#175355=CARTESIAN_POINT('Ctrl Pts',(47.8723576365755,-34.4706495255074,
40.0470135870237));
#175356=CARTESIAN_POINT('Ctrl Pts',(47.8877824700225,-34.4668046706501,
40.0305755292102));
#175357=CARTESIAN_POINT('Ctrl Pts',(47.9025205705571,-34.4647575222378,
40.0133447567353));
#175358=CARTESIAN_POINT('Ctrl Pts',(47.9177948141903,-34.4626359025942,
39.9954871626613));
#175359=CARTESIAN_POINT('Ctrl Pts',(47.9323322826087,-34.462445422019,39.9767767954335));
#175360=CARTESIAN_POINT('Ctrl Pts',(47.9459912469386,-34.464059298365,39.95751975775));
#175361=CARTESIAN_POINT('Ctrl Pts',(47.9594552672001,-34.4656501410745,
39.9385375612023));
#175362=CARTESIAN_POINT('Ctrl Pts',(47.9720663806666,-34.4689948098108,
39.9190226977123));
#175363=CARTESIAN_POINT('Ctrl Pts',(47.9836621023758,-34.4740120960928,
39.8992655451885));
#175364=CARTESIAN_POINT('Ctrl Pts',(47.9917468458596,-34.4775102373549,
39.8854905069345));
#175365=CARTESIAN_POINT('Ctrl Pts',(47.9993374592446,-34.4818222937569,
39.8715976051484));
#175366=CARTESIAN_POINT('Ctrl Pts',(48.0063682005187,-34.4869303039397,
39.8576902534424));
#175367=CARTESIAN_POINT('',(48.2946219293746,-34.6963546279286,39.2875012672119));
#175368=CARTESIAN_POINT('',(48.0063682005187,-34.4869303039397,39.8576902534424));
#175369=CARTESIAN_POINT('',(51.3398895692697,-30.0070536838158,39.2875012672119));
#175370=CARTESIAN_POINT('Origin',(5.53234440788222E-15,0.,39.2875012672119));
#175371=CARTESIAN_POINT('',(51.0313275753408,-29.8289013456886,39.8576902534424));
#175372=CARTESIAN_POINT('',(51.3398895692697,-30.0070536838158,39.2875012672119));
#175373=CARTESIAN_POINT('',(51.0193480105327,-29.4735998357338,40.1599502534424));
#175374=CARTESIAN_POINT('Ctrl Pts',(51.0313275753408,-29.8289013456886,
39.8576902534424));
#175375=CARTESIAN_POINT('Ctrl Pts',(51.0207361915351,-29.8227862420882,
39.8772619994089));
#175376=CARTESIAN_POINT('Ctrl Pts',(51.0111534059195,-29.8150339189585,
39.8967644650441));
#175377=CARTESIAN_POINT('Ctrl Pts',(51.0026853737161,-29.8057923055218,
39.9159282836152));
#175378=CARTESIAN_POINT('Ctrl Pts',(50.9940643779273,-29.7963837547977,
39.935438270733));
#175379=CARTESIAN_POINT('Ctrl Pts',(50.9865979533845,-29.7854311896963,
39.9545987622535));
#175380=CARTESIAN_POINT('Ctrl Pts',(50.9804176151407,-29.7730411634356,
39.9731387498444));
#175381=CARTESIAN_POINT('Ctrl Pts',(50.9744989363941,-29.7611756987626,
39.9908938024301));
#175382=CARTESIAN_POINT('Ctrl Pts',(50.9697592710636,-29.7479911916937,
40.0080810366458));
#175383=CARTESIAN_POINT('Ctrl Pts',(50.9663409452031,-29.7335453815885,
40.024454274284));
#175384=CARTESIAN_POINT('Ctrl Pts',(50.9636221212252,-29.7220556592812,
40.0374770090677));
#175385=CARTESIAN_POINT('Ctrl Pts',(50.9617395717397,-29.7097672786655,
40.0499848770129));
#175386=CARTESIAN_POINT('Ctrl Pts',(50.9607809287995,-29.6966961073821,
40.0618424270193));
#175387=CARTESIAN_POINT('Ctrl Pts',(50.9607783120157,-29.6966604273304,
40.0618747942791));
#175388=CARTESIAN_POINT('Ctrl Pts',(50.9607757022532,-29.6966247415591,
40.0619071564124));
#175389=CARTESIAN_POINT('Ctrl Pts',(50.9607730995135,-29.6965890500697,
40.0619395134161));
#175390=CARTESIAN_POINT('Ctrl Pts',(50.9602549766184,-29.6894840070026,
40.0683807661799));
#175391=CARTESIAN_POINT('Ctrl Pts',(50.9600390146967,-29.6821247070255,
40.0746073439084));
#175392=CARTESIAN_POINT('Ctrl Pts',(50.960124721527,-29.6745516564558,40.0805869293669));
#175393=CARTESIAN_POINT('Ctrl Pts',(50.960294812667,-29.6595224131519,40.092453830807));
#175394=CARTESIAN_POINT('Ctrl Pts',(50.9616539500924,-29.643650250636,40.1033475319609));
#175395=CARTESIAN_POINT('Ctrl Pts',(50.9642038006262,-29.6272454573768,
40.1130129263075));
#175396=CARTESIAN_POINT('Ctrl Pts',(50.9661161885265,-29.6149418624324,
40.1202619720674));
#175397=CARTESIAN_POINT('Ctrl Pts',(50.9686983518507,-29.6023386622823,
40.1268200947266));
#175398=CARTESIAN_POINT('Ctrl Pts',(50.9719510035829,-29.5895667656373,
40.1325796782703));
#175399=CARTESIAN_POINT('Ctrl Pts',(50.9731707479825,-29.5847773043955,
40.1347395220992));
#175400=CARTESIAN_POINT('Ctrl Pts',(50.9744847799797,-29.5799641203062,
40.1367870714852));
#175401=CARTESIAN_POINT('Ctrl Pts',(50.9758931378754,-29.57513411717,40.1387166518767));
#175402=CARTESIAN_POINT('Ctrl Pts',(50.9808223905104,-29.5582291061934,
40.1454701832469));
#175403=CARTESIAN_POINT('Ctrl Pts',(50.9869071309995,-29.5411180593587,
40.1507785912492));
#175404=CARTESIAN_POINT('Ctrl Pts',(50.9941490417486,-29.5240970004169,
40.1543986087265));
#175405=CARTESIAN_POINT('Ctrl Pts',(50.9977699971231,-29.515586470946,40.1562086174652));
#175406=CARTESIAN_POINT('Ctrl Pts',(51.0016802459462,-29.5070984389556,
40.1575965292115));
#175407=CARTESIAN_POINT('Ctrl Pts',(51.005880002284,-29.4986699095565,40.1585319382567));
#175408=CARTESIAN_POINT('Ctrl Pts',(51.0079798804529,-29.4944556448569,
40.1589996427793));
#175409=CARTESIAN_POINT('Ctrl Pts',(51.0101521355228,-29.4902562558175,
40.159354221642));
#175410=CARTESIAN_POINT('Ctrl Pts',(51.0123967945051,-29.4860763682211,
40.159591874311));
#175411=CARTESIAN_POINT('Ctrl Pts',(51.0146414534875,-29.4818964806248,
40.1598295269801));
#175412=CARTESIAN_POINT('Ctrl Pts',(51.0169585178538,-29.4777360953216,
40.1599502506895));
#175413=CARTESIAN_POINT('Ctrl Pts',(51.0193480105327,-29.4735998357338,
40.1599502534424));
#175414=CARTESIAN_POINT('',(51.0345602039887,-29.4472515437736,40.1599502534424));
#175415=CARTESIAN_POINT('Origin',(5.71420591410065E-15,5.21864079991075E-15,
40.1599502534424));
#175416=CARTESIAN_POINT('',(51.3482501200165,-29.2799753962463,39.8576902534424));
#175417=CARTESIAN_POINT('Ctrl Pts',(51.0345602039887,-29.4472515437736,
40.1599502534424));
#175418=CARTESIAN_POINT('Ctrl Pts',(51.0364642604675,-29.4439516646699,
40.1599502448875));
#175419=CARTESIAN_POINT('Ctrl Pts',(51.0384038328688,-29.4406842975233,
40.1598743450437));
#175420=CARTESIAN_POINT('Ctrl Pts',(51.0403770101285,-29.4374505691485,
40.1597243308499));
#175421=CARTESIAN_POINT('Ctrl Pts',(51.0520264994549,-29.4183588813631,
40.1588386583936));
#175422=CARTESIAN_POINT('Ctrl Pts',(51.0648472300504,-29.4004365818696,
40.1553722553598));
#175423=CARTESIAN_POINT('Ctrl Pts',(51.0784429877935,-29.3839216347767,
40.1496902177739));
#175424=CARTESIAN_POINT('Ctrl Pts',(51.0835219102983,-29.3777522003075,
40.1475675976806));
#175425=CARTESIAN_POINT('Ctrl Pts',(51.0887089685294,-29.371778749049,40.1451361443075));
#175426=CARTESIAN_POINT('Ctrl Pts',(51.0939835922269,-29.3660122232358,
40.1424159447501));
#175427=CARTESIAN_POINT('Ctrl Pts',(51.0980991182406,-29.3615128905148,
40.1402935085949));
#175428=CARTESIAN_POINT('Ctrl Pts',(51.1022679285261,-29.3571400387134,
40.1379949176048));
#175429=CARTESIAN_POINT('Ctrl Pts',(51.1064802178293,-29.3528993717244,
40.1355293609261));
#175430=CARTESIAN_POINT('Ctrl Pts',(51.1212232303906,-29.3380570372629,
40.1268999125508));
#175431=CARTESIAN_POINT('Ctrl Pts',(51.1364988531343,-29.3248339623427,
40.1162251288835));
#175432=CARTESIAN_POINT('Ctrl Pts',(51.1518867653713,-29.3134747466759,
40.1038990521418));
#175433=CARTESIAN_POINT('Ctrl Pts',(51.1595807214898,-29.3077951388425,
40.0977360137709));
#175434=CARTESIAN_POINT('Ctrl Pts',(51.1673027515571,-29.3025814967139,
40.0911601532641));
#175435=CARTESIAN_POINT('Ctrl Pts',(51.1750003199402,-29.2978643977774,
40.084220729064));
#175436=CARTESIAN_POINT('Ctrl Pts',(51.1826650006752,-29.2931674525157,
40.0773109533619));
#175437=CARTESIAN_POINT('Ctrl Pts',(51.1903053811865,-29.2889625693101,
40.0700409753048));
#175438=CARTESIAN_POINT('Ctrl Pts',(51.1978697380629,-29.2852806784149,
40.0624586415899));
#175439=CARTESIAN_POINT('Ctrl Pts',(51.1979021952408,-29.2852648801402,
40.0624261072769));
#175440=CARTESIAN_POINT('Ctrl Pts',(51.1979346509235,-29.2852490909584,
40.0623935677889));
#175441=CARTESIAN_POINT('Ctrl Pts',(51.1979671051091,-29.2852333108688,
40.0623610231288));
#175442=CARTESIAN_POINT('Ctrl Pts',(51.2132718752132,-29.2777917239328,
40.0470135870247));
#175443=CARTESIAN_POINT('Ctrl Pts',(51.228210313038,-29.2723555974564,40.0305755292122));
#175444=CARTESIAN_POINT('Ctrl Pts',(51.2426536914375,-29.2687791125368,
40.0133447567384));
#175445=CARTESIAN_POINT('Ctrl Pts',(51.2576224915239,-29.265072522133,39.995487162666));
#175446=CARTESIAN_POINT('Ctrl Pts',(51.2720604115264,-29.2633635057963,
39.9767767954398));
#175447=CARTESIAN_POINT('Ctrl Pts',(51.2858132466341,-29.263540790607,39.9575197577579));
#175448=CARTESIAN_POINT('Ctrl Pts',(51.2993697979264,-29.2637155451657,
39.9385375612124));
#175449=CARTESIAN_POINT('Ctrl Pts',(51.3122614394758,-29.265723671145,39.9190226977245));
#175450=CARTESIAN_POINT('Ctrl Pts',(51.3243180878321,-29.269501389236,39.899265545203));
#175451=CARTESIAN_POINT('Ctrl Pts',(51.3327241975788,-29.2721352815024,
39.8854905069443));
#175452=CARTESIAN_POINT('Ctrl Pts',(51.3407239614216,-29.2756302808569,
39.8715976051533));
#175453=CARTESIAN_POINT('Ctrl Pts',(51.3482501200165,-29.2799753962463,
39.8576902534424));
#175454=CARTESIAN_POINT('',(51.6568155675427,-29.4581217525674,39.2875012672119));
#175455=CARTESIAN_POINT('',(51.3482501200165,-29.2799753962463,39.8576902534424));
#175456=CARTESIAN_POINT('',(54.1952354911872,-24.4761921430393,39.2875012672119));
#175457=CARTESIAN_POINT('Origin',(5.53234440788222E-15,0.,39.2875012672119));
#175458=CARTESIAN_POINT('',(53.8697418420145,-24.3312692531089,39.8576902534424));
#175459=CARTESIAN_POINT('',(54.1952354911872,-24.4761921430393,39.2875012672119));
#175460=CARTESIAN_POINT('',(53.8206887816836,-23.9791663275014,40.1599502534424));
#175461=CARTESIAN_POINT('Ctrl Pts',(53.8697418420145,-24.3312692531089,
39.8576902534424));
#175462=CARTESIAN_POINT('Ctrl Pts',(53.8585692765391,-24.3262947497603,
39.8772619994026));
#175463=CARTESIAN_POINT('Ctrl Pts',(53.8482286480054,-24.3195865685246,
39.8967644650314));
#175464=CARTESIAN_POINT('Ctrl Pts',(53.8388409929203,-24.3112807320101,
39.9159282835966));
#175465=CARTESIAN_POINT('Ctrl Pts',(53.8292837625023,-24.3028248617567,
39.9354382707079));
#175466=CARTESIAN_POINT('Ctrl Pts',(53.8207133850174,-24.2927127498415,
39.9545987622223));
#175467=CARTESIAN_POINT('Ctrl Pts',(53.8132717929093,-24.2810366187063,
39.9731387498077));
#175468=CARTESIAN_POINT('Ctrl Pts',(53.8061452585171,-24.2698548246904,
39.9908938023878));
#175469=CARTESIAN_POINT('Ctrl Pts',(53.8000534013066,-24.2572379736713,
40.0080810365982));
#175470=CARTESIAN_POINT('Ctrl Pts',(53.7951438030611,-24.2432286115827,
40.0244542742322));
#175471=CARTESIAN_POINT('Ctrl Pts',(53.7912388700622,-24.2320860256563,
40.0374770090346));
#175472=CARTESIAN_POINT('Ctrl Pts',(53.7880821478325,-24.2200617420654,
40.0499848769972));
#175473=CARTESIAN_POINT('Ctrl Pts',(53.7857624469883,-24.2071623814823,
40.0618424270193));
#175474=CARTESIAN_POINT('Ctrl Pts',(53.7857561149585,-24.207127170418,40.0618747942791));
#175475=CARTESIAN_POINT('Ctrl Pts',(53.7857497893137,-24.2070919529316,
40.0619071564124));
#175476=CARTESIAN_POINT('Ctrl Pts',(53.7857434700555,-24.2070567290242,
40.0619395134162));
#175477=CARTESIAN_POINT('Ctrl Pts',(53.7844855062586,-24.2000447667165,
40.0683807661799));
#175478=CARTESIAN_POINT('Ctrl Pts',(53.7835014710816,-24.1927483559225,
40.0746073439084));
#175479=CARTESIAN_POINT('Ctrl Pts',(53.7827951090625,-24.1852078325129,
40.0805869293669));
#175480=CARTESIAN_POINT('Ctrl Pts',(53.7813932847188,-24.1702431416109,
40.092453830807));
#175481=CARTESIAN_POINT('Ctrl Pts',(53.7810858838907,-24.1543158599156,
40.1033475319609));
#175482=CARTESIAN_POINT('Ctrl Pts',(53.7819069982469,-24.1377344018724,
40.1130129263075));
#175483=CARTESIAN_POINT('Ctrl Pts',(53.782522834014,-24.1252983083401,40.1202619720674));
#175484=CARTESIAN_POINT('Ctrl Pts',(53.7837734588334,-24.1124942402749,
40.1268200947266));
#175485=CARTESIAN_POINT('Ctrl Pts',(53.7856732654698,-24.099452314729,40.1325796782703));
#175486=CARTESIAN_POINT('Ctrl Pts',(53.7863856929585,-24.0945615926493,
40.1347395220992));
#175487=CARTESIAN_POINT('Ctrl Pts',(53.7871894118146,-24.0896374219408,
40.1367870714852));
#175488=CARTESIAN_POINT('Ctrl Pts',(53.788085181773,-24.0846866645806,40.1387166518767));
#175489=CARTESIAN_POINT('Ctrl Pts',(53.7912203766273,-24.0673590138199,
40.1454701832468));
#175490=CARTESIAN_POINT('Ctrl Pts',(53.7954831928409,-24.0497056745174,
40.1507785912492));
#175491=CARTESIAN_POINT('Ctrl Pts',(53.8009062465108,-24.0320208729156,
40.1543986087265));
#175492=CARTESIAN_POINT('Ctrl Pts',(53.8036177733457,-24.0231784721148,
40.1562086174652));
#175493=CARTESIAN_POINT('Ctrl Pts',(53.8066193604764,-24.0143282061514,
40.1575965292115));
#175494=CARTESIAN_POINT('Ctrl Pts',(53.8099150888839,-24.005506855042,40.1585319382567));
#175495=CARTESIAN_POINT('Ctrl Pts',(53.8115629530877,-24.0010961794874,
40.1589996427793));
#175496=CARTESIAN_POINT('Ctrl Pts',(53.813284352634,-23.9966927326563,40.159354221642));
#175497=CARTESIAN_POINT('Ctrl Pts',(53.8150797979125,-23.9923011121675,
40.159591874311));
#175498=CARTESIAN_POINT('Ctrl Pts',(53.816875243191,-23.9879094916788,40.1598295269801));
#175499=CARTESIAN_POINT('Ctrl Pts',(53.818744735754,-23.9835296982241,40.1599502506895));
#175500=CARTESIAN_POINT('Ctrl Pts',(53.8206887816836,-23.9791663275014,
40.1599502534424));
#175501=CARTESIAN_POINT('',(53.8330634946837,-23.9513722670365,40.1599502534424));
#175502=CARTESIAN_POINT('Origin',(5.71744365443249E-15,5.22499522310014E-15,
40.1599502534424));
#175503=CARTESIAN_POINT('',(54.1275498658873,-23.7522229508829,39.8576902534424));
#175504=CARTESIAN_POINT('Ctrl Pts',(53.8330634946837,-23.9513722670365,
40.1599502534424));
#175505=CARTESIAN_POINT('Ctrl Pts',(53.8346121892503,-23.9478914369182,
40.1599502448875));
#175506=CARTESIAN_POINT('Ctrl Pts',(53.8361996036043,-23.9444392282281,
40.1598743450437));
#175507=CARTESIAN_POINT('Ctrl Pts',(53.8378239549348,-23.941016961369,40.1597243308498));
#175508=CARTESIAN_POINT('Ctrl Pts',(53.8474140023521,-23.9208121566345,
40.1588386583938));
#175509=CARTESIAN_POINT('Ctrl Pts',(53.8582911092169,-23.90164790611,40.1553722553614));
#175510=CARTESIAN_POINT('Ctrl Pts',(53.8700861059327,-23.8838022859651,
40.1496902177779));
#175511=CARTESIAN_POINT('Ctrl Pts',(53.8744923240669,-23.8771357563345,
40.1475675976837));
#175512=CARTESIAN_POINT('Ctrl Pts',(53.8790265713726,-23.8706528330371,
40.1451361443092));
#175513=CARTESIAN_POINT('Ctrl Pts',(53.8836695340509,-23.8643665485423,
40.1424159447501));
#175514=CARTESIAN_POINT('Ctrl Pts',(53.8872922064474,-23.8594616740269,
40.1402935085949));
#175515=CARTESIAN_POINT('Ctrl Pts',(53.8909810920751,-23.8546770178324,
40.1379949176048));
#175516=CARTESIAN_POINT('Ctrl Pts',(53.8947270356132,-23.8500192775332,
40.1355293609261));
#175517=CARTESIAN_POINT('Ctrl Pts',(53.9078378379964,-23.8337171864859,
40.1268999125509));
#175518=CARTESIAN_POINT('Ctrl Pts',(53.9216475915794,-23.8189698115828,
40.1162251288835));
#175519=CARTESIAN_POINT('Ctrl Pts',(53.9357638458656,-23.8060643480688,
40.1038990521418));
#175520=CARTESIAN_POINT('Ctrl Pts',(53.9428219730086,-23.7996116163119,
40.097736013771));
#175521=CARTESIAN_POINT('Ctrl Pts',(53.9499567269876,-23.7936193631242,
40.0911601532641));
#175522=CARTESIAN_POINT('Ctrl Pts',(53.9571190561826,-23.7881234899552,
40.084220729064));
#175523=CARTESIAN_POINT('Ctrl Pts',(53.9642507845244,-23.7826510977524,
40.0773109533618));
#175524=CARTESIAN_POINT('Ctrl Pts',(53.9714097802521,-23.7776706121034,
40.0700409753047));
#175525=CARTESIAN_POINT('Ctrl Pts',(53.9785478363929,-23.7732182003918,
40.0624586415899));
#175526=CARTESIAN_POINT('Ctrl Pts',(53.9785784643976,-23.7731990959628,
40.0624261072769));
#175527=CARTESIAN_POINT('Ctrl Pts',(53.9786090918658,-23.7731800007332,
40.0623935677888));
#175528=CARTESIAN_POINT('Ctrl Pts',(53.9786397187954,-23.7731609147024,
40.0623610231288));
#175529=CARTESIAN_POINT('Ctrl Pts',(53.9930827901212,-23.7641603094583,
40.0470135870242));
#175530=CARTESIAN_POINT('Ctrl Pts',(54.0073711636744,-23.757192470702,40.0305755292112));
#175531=CARTESIAN_POINT('Ctrl Pts',(54.0213615752636,-23.7521258339925,
40.0133447567369));
#175532=CARTESIAN_POINT('Ctrl Pts',(54.0358609304984,-23.7468748830087,
39.9954871626638));
#175533=CARTESIAN_POINT('Ctrl Pts',(54.0500411172136,-23.7436660552518,
39.976776795437));
#175534=CARTESIAN_POINT('Ctrl Pts',(54.0637371441607,-23.7424048061586,
39.9575197577545));
#175535=CARTESIAN_POINT('Ctrl Pts',(54.0772376980724,-23.74116155792,39.9385375612083));
#175536=CARTESIAN_POINT('Ctrl Pts',(54.0902686241836,-23.7418111396953,
39.9190226977197));
#175537=CARTESIAN_POINT('Ctrl Pts',(54.1026541040257,-23.7443079001268,
39.8992655451974));
#175538=CARTESIAN_POINT('Ctrl Pts',(54.1112894809334,-23.7460486859219,
39.8854905069405));
#175539=CARTESIAN_POINT('Ctrl Pts',(54.1196107481433,-23.7486883362829,
39.8715976051514));
#175540=CARTESIAN_POINT('Ctrl Pts',(54.1275498658873,-23.7522229508829,
39.8576902534424));
#175541=CARTESIAN_POINT('',(54.4530463244692,-23.8971395307769,39.2875012672119));
#175542=CARTESIAN_POINT('',(54.1275498658873,-23.7522229508828,39.8576902534424));
#175543=CARTESIAN_POINT('',(56.4568070719811,-18.6771643191711,39.2875012672119));
#175544=CARTESIAN_POINT('Origin',(5.53234440788222E-15,0.,39.2875012672119));
#175545=CARTESIAN_POINT('',(56.1179479440988,-18.5670586829466,39.8576902534424));
#175546=CARTESIAN_POINT('',(56.4568070719811,-18.677164319171,39.2875012672119));
#175547=CARTESIAN_POINT('',(56.0323588238391,-18.2220120550218,40.1599502534424));
#175548=CARTESIAN_POINT('Ctrl Pts',(56.1179479440988,-18.5670586829466,
39.8576902534424));
#175549=CARTESIAN_POINT('Ctrl Pts',(56.1063166059129,-18.563279281547,39.877261999407));
#175550=CARTESIAN_POINT('Ctrl Pts',(56.095331428546,-18.5576887384383,39.8967644650402));
#175551=CARTESIAN_POINT('Ctrl Pts',(56.0851270036887,-18.5504096793227,
39.9159282836095));
#175552=CARTESIAN_POINT('Ctrl Pts',(56.0747382496537,-18.5429991338175,
39.9354382707253));
#175553=CARTESIAN_POINT('Ctrl Pts',(56.0651578180728,-18.5338382654942,
39.9545987622439));
#175554=CARTESIAN_POINT('Ctrl Pts',(56.0565365037393,-18.5230039556103,
39.9731387498331));
#175555=CARTESIAN_POINT('Ctrl Pts',(56.0482801935019,-18.5126283423164,
39.990893802417));
#175556=CARTESIAN_POINT('Ctrl Pts',(56.0409028880736,-18.5007173801951,
40.008081036631));
#175557=CARTESIAN_POINT('Ctrl Pts',(56.0345558080305,-18.4872979556121,
40.0244542742679));
#175558=CARTESIAN_POINT('Ctrl Pts',(56.0295075492851,-18.4766245865907,
40.0374770090574));
#175559=CARTESIAN_POINT('Ctrl Pts',(56.0251112400292,-18.4649961406168,
40.049984877008));
#175560=CARTESIAN_POINT('Ctrl Pts',(56.0214558964133,-18.4524099188566,
40.0618424270193));
#175561=CARTESIAN_POINT('Ctrl Pts',(56.0214459185126,-18.4523755625596,
40.0618747942791));
#175562=CARTESIAN_POINT('Ctrl Pts',(56.0214359462907,-18.4523411992081,
40.0619071564124));
#175563=CARTESIAN_POINT('Ctrl Pts',(56.0214259797492,-18.4523068288034,
40.0619395134161));
#175564=CARTESIAN_POINT('Ctrl Pts',(56.019441957565,-18.4454647717814,40.0683807661799));
#175565=CARTESIAN_POINT('Ctrl Pts',(56.017700630428,-18.438311191174,40.0746073439084));
#175566=CARTESIAN_POINT('Ctrl Pts',(56.0162099386098,-18.430885810477,40.0805869293668));
#175567=CARTESIAN_POINT('Ctrl Pts',(56.0132515574632,-18.4161496282619,
40.092453830807));
#175568=CARTESIAN_POINT('Ctrl Pts',(56.0112809863294,-18.4003417300184,
40.1033475319609));
#175569=CARTESIAN_POINT('Ctrl Pts',(56.0103643682072,-18.3837652771156,
40.1130129263075));
#175570=CARTESIAN_POINT('Ctrl Pts',(56.0096769046155,-18.3713329374384,
40.1202619720674));
#175571=CARTESIAN_POINT('Ctrl Pts',(56.0095822888229,-18.3584682855073,
40.1268200947266));
#175572=CARTESIAN_POINT('Ctrl Pts',(56.0101084356844,-18.345299221126,40.1325796782703));
#175573=CARTESIAN_POINT('Ctrl Pts',(56.0103057407575,-18.340360821983,40.1347395220992));
#175574=CARTESIAN_POINT('Ctrl Pts',(56.0105903407606,-18.3353796148998,
40.1367870714852));
#175575=CARTESIAN_POINT('Ctrl Pts',(56.0109637085386,-18.3303623448493,
40.1387166518767));
#175576=CARTESIAN_POINT('Ctrl Pts',(56.0122704957614,-18.3128018996723,
40.1454701832469));
#175577=CARTESIAN_POINT('Ctrl Pts',(56.0146646833929,-18.2947996815816,
40.1507785912491));
#175578=CARTESIAN_POINT('Ctrl Pts',(56.0182094638727,-18.2766448957071,
40.1543986087265));
#175579=CARTESIAN_POINT('Ctrl Pts',(56.0199818541126,-18.2675675027699,
40.1562086174652));
#175580=CARTESIAN_POINT('Ctrl Pts',(56.0220418935343,-18.2584519681993,
40.1575965292115));
#175581=CARTESIAN_POINT('Ctrl Pts',(56.0243974853213,-18.2493344439485,
40.1585319382567));
#175582=CARTESIAN_POINT('Ctrl Pts',(56.0255752812149,-18.2447756818231,
40.1589996427793));
#175583=CARTESIAN_POINT('Ctrl Pts',(56.0268269652241,-18.2402164222853,
40.159354221642));
#175584=CARTESIAN_POINT('Ctrl Pts',(56.0281535255245,-18.2356611844172,
40.159591874311));
#175585=CARTESIAN_POINT('Ctrl Pts',(56.029480085825,-18.2311059465492,40.1598295269801));
#175586=CARTESIAN_POINT('Ctrl Pts',(56.0308815240329,-18.2265547308766,
40.1599502506895));
#175587=CARTESIAN_POINT('Ctrl Pts',(56.0323588238391,-18.2220120550218,
40.1599502534424));
#175588=CARTESIAN_POINT('',(56.0417604764383,-18.193076743595,40.1599502534424));
#175589=CARTESIAN_POINT('Origin',(5.71999943999309E-15,5.23165327211576E-15,
40.1599502534424));
#175590=CARTESIAN_POINT('',(56.3138168485095,-17.9642361803973,39.8576902534424));
#175591=CARTESIAN_POINT('Ctrl Pts',(56.0417604764383,-18.193076743595,40.1599502534424));
#175592=CARTESIAN_POINT('Ctrl Pts',(56.0429368412708,-18.1894530991651,
40.1599502448875));
#175593=CARTESIAN_POINT('Ctrl Pts',(56.0441547055336,-18.1858538720524,
40.1598743450437));
#175594=CARTESIAN_POINT('Ctrl Pts',(56.0454124342019,-18.1822805617809,
40.1597243308499));
#175595=CARTESIAN_POINT('Ctrl Pts',(56.0528379691473,-18.1611840081594,
40.1588386583937));
#175596=CARTESIAN_POINT('Ctrl Pts',(56.0616522804266,-18.1409877741371,
40.1553722553607));
#175597=CARTESIAN_POINT('Ctrl Pts',(56.0715172876677,-18.1220070012839,
40.1496902177761));
#175598=CARTESIAN_POINT('Ctrl Pts',(56.0752025259794,-18.1149164163918,
40.1475675976823));
#175599=CARTESIAN_POINT('Ctrl Pts',(56.0790342841932,-18.1079950493255,
40.1451361443084));
#175600=CARTESIAN_POINT('Ctrl Pts',(56.0829947165771,-18.101257880003,40.1424159447501));
#175601=CARTESIAN_POINT('Ctrl Pts',(56.0860848445996,-18.096001202525,40.1402935085949));
#175602=CARTESIAN_POINT('Ctrl Pts',(56.0892533893665,-18.0908571636319,
40.1379949176048));
#175603=CARTESIAN_POINT('Ctrl Pts',(56.0924919457982,-18.0858333811998,
40.1355293609261));
#175604=CARTESIAN_POINT('Ctrl Pts',(56.103826893309,-18.0682501426877,40.1268999125509));
#175605=CARTESIAN_POINT('Ctrl Pts',(56.1160194751811,-18.0521400431272,
40.1162251288835));
#175606=CARTESIAN_POINT('Ctrl Pts',(56.1287094108803,-18.0378297267251,
40.1038990521418));
#175607=CARTESIAN_POINT('Ctrl Pts',(56.13505437873,-18.0306745685241,40.097736013771));
#175608=CARTESIAN_POINT('Ctrl Pts',(56.1415236867628,-18.0239693566571,
40.0911601532641));
#175609=CARTESIAN_POINT('Ctrl Pts',(56.1480723047925,-18.0177549231922,
40.084220729064));
#175610=CARTESIAN_POINT('Ctrl Pts',(56.1545929440329,-18.0115670407224,
40.0773109533618));
#175611=CARTESIAN_POINT('Ctrl Pts',(56.1611921195217,-18.005865519873,40.0700409753047));
#175612=CARTESIAN_POINT('Ctrl Pts',(56.1678256688901,-18.0006913688995,
40.0624586415899));
#175613=CARTESIAN_POINT('Ctrl Pts',(56.1678541321547,-18.0006691676283,
40.0624261072769));
#175614=CARTESIAN_POINT('Ctrl Pts',(56.1678825958474,-18.0006469755621,
40.0623935677888));
#175615=CARTESIAN_POINT('Ctrl Pts',(56.167911059966,-18.0006247927008,40.0623610231288));
#175616=CARTESIAN_POINT('Ctrl Pts',(56.1813341912004,-17.9901637816641,
40.0470135870252));
#175617=CARTESIAN_POINT('Ctrl Pts',(56.1948159540698,-17.9817405717279,
40.0305755292134));
#175618=CARTESIAN_POINT('Ctrl Pts',(56.2082001169704,-17.9752392943607,
40.0133447567403));
#175619=CARTESIAN_POINT('Ctrl Pts',(56.2220711693822,-17.9685015133149,
39.9954871626685));
#175620=CARTESIAN_POINT('Ctrl Pts',(56.2358382617157,-17.963828030726,39.9767767954431));
#175621=CARTESIAN_POINT('Ctrl Pts',(56.2493274239639,-17.9611420662373,
39.957519757762));
#175622=CARTESIAN_POINT('Ctrl Pts',(56.2626240656001,-17.9584944364886,
39.938537561217));
#175623=CARTESIAN_POINT('Ctrl Pts',(56.2756515067187,-17.9577783571049,
39.9190226977296));
#175624=CARTESIAN_POINT('Ctrl Pts',(56.2882301201368,-17.9589668048461,
39.8992655452086));
#175625=CARTESIAN_POINT('Ctrl Pts',(56.2970001532129,-17.9597954117562,
39.885490506948));
#175626=CARTESIAN_POINT('Ctrl Pts',(56.3055517542485,-17.9615507925628,
39.8715976051552));
#175627=CARTESIAN_POINT('Ctrl Pts',(56.3138168485095,-17.9642361803973,
39.8576902534424));
#175628=CARTESIAN_POINT('',(56.6526781108323,-18.0743352474892,39.2875012672119));
#175629=CARTESIAN_POINT('',(56.3138168485095,-17.9642361803973,39.8576902534424));
#175630=CARTESIAN_POINT('',(58.099826060148,-12.6735055745741,39.2875012672119));
#175631=CARTESIAN_POINT('Origin',(5.53234440788222E-15,0.,39.2875012672119));
#175632=CARTESIAN_POINT('',(57.751314065072,-12.5994235324472,39.8576902534424));
#175633=CARTESIAN_POINT('',(58.099826060148,-12.6735055745741,39.2875012672119));
#175634=CARTESIAN_POINT('',(57.6301266171957,-12.2652136052661,40.1599502534424));
#175635=CARTESIAN_POINT('Ctrl Pts',(57.751314065072,-12.5994235324472,39.8576902534424));
#175636=CARTESIAN_POINT('Ctrl Pts',(57.7393513895544,-12.5968806409106,
39.8772619994052));
#175637=CARTESIAN_POINT('Ctrl Pts',(57.7278420192595,-12.5924689870915,
39.8967644650367));
#175638=CARTESIAN_POINT('Ctrl Pts',(57.7169326264468,-12.5862964562731,
39.9159282836043));
#175639=CARTESIAN_POINT('Ctrl Pts',(57.7058261701605,-12.580012427007,39.9354382707184));
#175640=CARTESIAN_POINT('Ctrl Pts',(57.695340649699,-12.5719031706707,39.9545987622355));
#175641=CARTESIAN_POINT('Ctrl Pts',(57.6856340700653,-12.5620293850099,
39.9731387498233));
#175642=CARTESIAN_POINT('Ctrl Pts',(57.6763384418466,-12.5525736298339,
39.9908938024062));
#175643=CARTESIAN_POINT('Ctrl Pts',(57.667756515503,-12.5414990556102,40.0080810366192));
#175644=CARTESIAN_POINT('Ctrl Pts',(57.660041493599,-12.528816594564,40.0244542742554));
#175645=CARTESIAN_POINT('Ctrl Pts',(57.6539052188793,-12.5187293821012,
40.0374770090494));
#175646=CARTESIAN_POINT('Ctrl Pts',(57.6483174894756,-12.5076241774183,
40.0499848770042));
#175647=CARTESIAN_POINT('Ctrl Pts',(57.643366551794,-12.4954889917448,40.0618424270193));
#175648=CARTESIAN_POINT('Ctrl Pts',(57.6433530373424,-12.4954558666298,
40.0618747942791));
#175649=CARTESIAN_POINT('Ctrl Pts',(57.643339527801,-12.4954227339055,40.0619071564124));
#175650=CARTESIAN_POINT('Ctrl Pts',(57.6433260231716,-12.4953895935727,
40.0619395134161));
#175651=CARTESIAN_POINT('Ctrl Pts',(57.6406376799625,-12.4887924048449,
40.0683807661799));
#175652=CARTESIAN_POINT('Ctrl Pts',(57.63815813921,-12.4818600305503,40.0746073439084));
#175653=CARTESIAN_POINT('Ctrl Pts',(57.6358994499241,-12.4746311465906,
40.0805869293669));
#175654=CARTESIAN_POINT('Ctrl Pts',(57.6314169246176,-12.4602849257587,
40.092453830807));
#175655=CARTESIAN_POINT('Ctrl Pts',(57.6278047731677,-12.444769605608,40.1033475319609));
#175656=CARTESIAN_POINT('Ctrl Pts',(57.6251604652272,-12.4283797729324,
40.1130129263075));
#175657=CARTESIAN_POINT('Ctrl Pts',(57.6231772342717,-12.4160873984256,
40.1202619720674));
#175658=CARTESIAN_POINT('Ctrl Pts',(57.6217384144975,-12.4033031104472,
40.1268200947266));
#175659=CARTESIAN_POINT('Ctrl Pts',(57.620885137009,-12.3901511902556,40.1325796782703));
#175660=CARTESIAN_POINT('Ctrl Pts',(57.6205651579508,-12.3852192201837,
40.1347395220992));
#175661=CARTESIAN_POINT('Ctrl Pts',(57.6203275209637,-12.3802355518732,
40.1367870714852));
#175662=CARTESIAN_POINT('Ctrl Pts',(57.6201743958657,-12.3752067393928,
40.1387166518767));
#175663=CARTESIAN_POINT('Ctrl Pts',(57.6196384580227,-12.3576058957117,
40.1454701832469));
#175664=CARTESIAN_POINT('Ctrl Pts',(57.6201377858514,-12.3394520349014,
40.1507785912492));
#175665=CARTESIAN_POINT('Ctrl Pts',(57.6217654557845,-12.3210261723874,
40.1543986087265));
#175666=CARTESIAN_POINT('Ctrl Pts',(57.622579290751,-12.3118132411303,40.1562086174652));
#175667=CARTESIAN_POINT('Ctrl Pts',(57.6236752122407,-12.3025323096568,
40.1575965292115));
#175668=CARTESIAN_POINT('Ctrl Pts',(57.6250648590507,-12.2932185057683,
40.1585319382567));
#175669=CARTESIAN_POINT('Ctrl Pts',(57.6257596824557,-12.2885616038241,
40.1589996427793));
#175670=CARTESIAN_POINT('Ctrl Pts',(57.6265279372158,-12.2838964837811,
40.159354221642));
#175671=CARTESIAN_POINT('Ctrl Pts',(57.627371078466,-12.279227536673,40.159591874311));
#175672=CARTESIAN_POINT('Ctrl Pts',(57.6282142197162,-12.274558589565,40.1598295269801));
#175673=CARTESIAN_POINT('Ctrl Pts',(57.6291322491186,-12.2698858157459,
40.1599502506895));
#175674=CARTESIAN_POINT('Ctrl Pts',(57.6301266171957,-12.2652136052661,
40.1599502534424));
#175675=CARTESIAN_POINT('',(57.6364522029207,-12.2354540642045,40.1599502534424));
#175676=CARTESIAN_POINT('Origin',(5.72184526906101E-15,5.23854199997932E-15,
40.1599502534424));
#175677=CARTESIAN_POINT('',(57.8830978693156,-11.9794294790612,39.8576902534424));
#175678=CARTESIAN_POINT('Ctrl Pts',(57.6364522029207,-12.2354540642045,
40.1599502534424));
#175679=CARTESIAN_POINT('Ctrl Pts',(57.6372433495199,-12.2317273068698,
40.1599502448874));
#175680=CARTESIAN_POINT('Ctrl Pts',(57.6380783205158,-12.2280204952199,
40.1598743450437));
#175681=CARTESIAN_POINT('Ctrl Pts',(57.6389556465834,-12.2243352914711,
40.1597243308498));
#175682=CARTESIAN_POINT('Ctrl Pts',(57.6441353133399,-12.2025781272258,
40.1588386583939));
#175683=CARTESIAN_POINT('Ctrl Pts',(57.6507902575918,-12.1815711838785,
40.1553722553622));
#175684=CARTESIAN_POINT('Ctrl Pts',(57.6586171922707,-12.161663215642,40.14969021778));
#175685=CARTESIAN_POINT('Ctrl Pts',(57.6615410745205,-12.1542262614136,
40.1475675976853));
#175686=CARTESIAN_POINT('Ctrl Pts',(57.6646283621005,-12.1469422825181,
40.1451361443101));
#175687=CARTESIAN_POINT('Ctrl Pts',(57.6678628728673,-12.1398280421987,
40.1424159447501));
#175688=CARTESIAN_POINT('Ctrl Pts',(57.6703866004265,-12.1342771550164,
40.1402935085949));
#175689=CARTESIAN_POINT('Ctrl Pts',(57.6730000890933,-12.1288300925913,
40.1379949176047));
#175690=CARTESIAN_POINT('Ctrl Pts',(57.6756957761165,-12.1234953096381,
40.1355293609261));
#175691=CARTESIAN_POINT('Ctrl Pts',(57.6851306806979,-12.1048235693018,
40.1268999125508));
#175692=CARTESIAN_POINT('Ctrl Pts',(57.6955725063806,-12.087527250706,40.1162251288835));
#175693=CARTESIAN_POINT('Ctrl Pts',(57.7066970899019,-12.0719688682368,
40.1038990521418));
#175694=CARTESIAN_POINT('Ctrl Pts',(57.7122593816626,-12.0641896770022,
40.0977360137709));
#175695=CARTESIAN_POINT('Ctrl Pts',(57.7179923646568,-12.0568449701604,
40.0911601532641));
#175696=CARTESIAN_POINT('Ctrl Pts',(57.7238555234916,-12.0499800630331,
40.084220729064));
#175697=CARTESIAN_POINT('Ctrl Pts',(57.7296936321425,-12.0431444860316,
40.0773109533618));
#175698=CARTESIAN_POINT('Ctrl Pts',(57.7356606854448,-12.0367843970373,
40.0700409753048));
#175699=CARTESIAN_POINT('Ctrl Pts',(57.7417170494857,-12.0309451958827,
40.0624586415899));
#175700=CARTESIAN_POINT('Ctrl Pts',(57.7417430361609,-12.0309201410111,
40.0624261072769));
#175701=CARTESIAN_POINT('Ctrl Pts',(57.7417690242238,-12.0308950952493,
40.0623935677888));
#175702=CARTESIAN_POINT('Ctrl Pts',(57.7417950136727,-12.0308700585974,
40.0623610231288));
#175703=CARTESIAN_POINT('Ctrl Pts',(57.7540511381846,-12.0190632547909,
40.0470135870217));
#175704=CARTESIAN_POINT('Ctrl Pts',(57.7665785813589,-12.0092769601233,
40.0305755292058));
#175705=CARTESIAN_POINT('Ctrl Pts',(57.7792098558853,-12.0014122714526,
40.0133447567283));
#175706=CARTESIAN_POINT('Ctrl Pts',(57.7923006313251,-11.993261480883,39.9954871626521));
#175707=CARTESIAN_POINT('Ctrl Pts',(57.8055037941362,-11.9871745471154,
39.9767767954219));
#175708=CARTESIAN_POINT('Ctrl Pts',(57.8186383016047,-11.9830932952215,
39.9575197577359));
#175709=CARTESIAN_POINT('Ctrl Pts',(57.8315853501805,-11.9790702919497,
39.9385375611865));
#175710=CARTESIAN_POINT('Ctrl Pts',(57.8444665749385,-11.9769963969252,
39.9190226976948));
#175711=CARTESIAN_POINT('Ctrl Pts',(57.8571005080145,-11.9768635110972,
39.8992655451694));
#175712=CARTESIAN_POINT('Ctrl Pts',(57.8659091109301,-11.9767708607337,
39.8854905069217));
#175713=CARTESIAN_POINT('Ctrl Pts',(57.8745973526502,-11.9776227396658,
39.871597605142));
#175714=CARTESIAN_POINT('Ctrl Pts',(57.8830978693156,-11.9794294790612,
39.8576902534424));
#175715=CARTESIAN_POINT('',(58.2316113004781,-12.0535047649322,39.2875012672119));
#175716=CARTESIAN_POINT('',(57.8830978693156,-11.9794294790612,39.8576902534424));
#175717=CARTESIAN_POINT('',(59.1062911958296,-6.53099325080055,39.2875012672119));
#175718=CARTESIAN_POINT('Origin',(5.53234440788222E-15,0.,39.2875012672119));
#175719=CARTESIAN_POINT('',(58.7519447039088,-6.4937464611274,39.8576902534424));
#175720=CARTESIAN_POINT('',(59.1062911958296,-6.53099325080055,39.2875012672119));
#175721=CARTESIAN_POINT('',(58.5964866834551,-6.1740349085902,40.1599502534424));
#175722=CARTESIAN_POINT('Ctrl Pts',(58.7519447039088,-6.49374646112741,
39.8576902534424));
#175723=CARTESIAN_POINT('Ctrl Pts',(58.7397817566352,-6.49246793990524,
39.8772619994045));
#175724=CARTESIAN_POINT('Ctrl Pts',(58.7278742924813,-6.48928351037763,
39.8967644650353));
#175725=CARTESIAN_POINT('Ctrl Pts',(58.7163794573033,-6.48428513539508,
39.9159282836023));
#175726=CARTESIAN_POINT('Ctrl Pts',(58.7046769834247,-6.47919647150708,
39.9354382707158));
#175727=CARTESIAN_POINT('Ctrl Pts',(58.6934012556386,-6.47222767386624,
39.9545987622323));
#175728=CARTESIAN_POINT('Ctrl Pts',(58.6827157580223,-6.4634225916897,39.9731387498196));
#175729=CARTESIAN_POINT('Ctrl Pts',(58.6724826566703,-6.4549902938632,39.9908938024019));
#175730=CARTESIAN_POINT('Ctrl Pts',(58.6627901347925,-6.44487344288915,
40.0080810366144));
#175731=CARTESIAN_POINT('Ctrl Pts',(58.6537916984223,-6.43306689707603,
40.0244542742501));
#175732=CARTESIAN_POINT('Ctrl Pts',(58.6466346380391,-6.42367635878418,
40.037477009046));
#175733=CARTESIAN_POINT('Ctrl Pts',(58.639916708821,-6.413216066341,40.0499848770026));
#175734=CARTESIAN_POINT('Ctrl Pts',(58.6337244205833,-6.40166487239037,
40.0618424270193));
#175735=CARTESIAN_POINT('Ctrl Pts',(58.6337075176478,-6.40163334138309,
40.0618747942791));
#175736=CARTESIAN_POINT('Ctrl Pts',(58.6336906188004,-6.40160180229485,
40.0619071564124));
#175737=CARTESIAN_POINT('Ctrl Pts',(58.6336737240427,-6.40157025512642,
40.0619395134161));
#175738=CARTESIAN_POINT('Ctrl Pts',(58.6303105138594,-6.39529021487321,
40.0683807661799));
#175739=CARTESIAN_POINT('Ctrl Pts',(58.6271199258587,-6.38865499943471,
40.0746073439084));
#175740=CARTESIAN_POINT('Ctrl Pts',(58.6241179857776,-6.38170181337784,
40.0805869293669));
#175741=CARTESIAN_POINT('Ctrl Pts',(58.6181604277966,-6.36790273412649,
40.092453830807));
#175742=CARTESIAN_POINT('Ctrl Pts',(58.6129462715178,-6.35284998116321,
40.1033475319609));
#175743=CARTESIAN_POINT('Ctrl Pts',(58.60860324535,-6.33682633915125,40.1130129263075));
#175744=CARTESIAN_POINT('Ctrl Pts',(58.6053459757242,-6.32480860764228,
40.1202619720674));
#175745=CARTESIAN_POINT('Ctrl Pts',(58.6025787159788,-6.31224475095104,
40.1268200947266));
#175746=CARTESIAN_POINT('Ctrl Pts',(58.600355362827,-6.2992540701389,40.1325796782703));
#175747=CARTESIAN_POINT('Ctrl Pts',(58.5995216053951,-6.29438256483434,
40.1347395220992));
#175748=CARTESIAN_POINT('Ctrl Pts',(58.5987643350184,-6.28945103740937,
40.1367870714852));
#175749=CARTESIAN_POINT('Ctrl Pts',(58.5980863947151,-6.28446577922116,
40.1387166518766));
#175750=CARTESIAN_POINT('Ctrl Pts',(58.5957136036535,-6.26701737556243,
40.1454701832468));
#175751=CARTESIAN_POINT('Ctrl Pts',(58.5943126009392,-6.24891076953056,
40.1507785912491));
#175752=CARTESIAN_POINT('Ctrl Pts',(58.5940053272331,-6.23041570798245,
40.1543986087265));
#175753=CARTESIAN_POINT('Ctrl Pts',(58.59385169038,-6.2211681772084,40.1562086174652));
#175754=CARTESIAN_POINT('Ctrl Pts',(58.5939714867925,-6.21182353265943,
40.1575965292115));
#175755=CARTESIAN_POINT('Ctrl Pts',(58.5943799633642,-6.20241549311763,
40.1585319382567));
#175756=CARTESIAN_POINT('Ctrl Pts',(58.5945842016501,-6.19771147334672,
40.1589996427793));
#175757=CARTESIAN_POINT('Ctrl Pts',(58.5948606100012,-6.19299160482992,
40.159354221642));
#175758=CARTESIAN_POINT('Ctrl Pts',(58.5952110945691,-6.18826010244349,
40.159591874311));
#175759=CARTESIAN_POINT('Ctrl Pts',(58.595561579137,-6.18352860005705,40.1598295269801));
#175760=CARTESIAN_POINT('Ctrl Pts',(58.5959861416119,-6.17878546397913,
40.1599502506895));
#175761=CARTESIAN_POINT('Ctrl Pts',(58.5964866834551,-6.1740349085902,40.1599502534424));
#175762=CARTESIAN_POINT('',(58.5996668978648,-6.14377718965322,40.1599502534424));
#175763=CARTESIAN_POINT('Origin',(5.72296091834672E-15,5.2455859323468E-15,
40.1599502534424));
#175764=CARTESIAN_POINT('',(58.8181995570485,-5.86337364149581,39.8576902534424));
#175765=CARTESIAN_POINT('Ctrl Pts',(58.5996668978648,-6.14377718965322,
40.1599502534424));
#175766=CARTESIAN_POINT('Ctrl Pts',(58.600064158263,-6.13998815054686,40.1599502448875));
#175767=CARTESIAN_POINT('Ctrl Pts',(58.6005070878751,-6.13621436696404,
40.1598743450437));
#175768=CARTESIAN_POINT('Ctrl Pts',(58.600994399174,-6.13245764560126,40.1597243308498));
#175769=CARTESIAN_POINT('Ctrl Pts',(58.6038714482307,-6.11027824676979,
40.1588386583938));
#175770=CARTESIAN_POINT('Ctrl Pts',(58.6082941124962,-6.08869075055824,
40.1553722553616));
#175771=CARTESIAN_POINT('Ctrl Pts',(58.6139972210823,-6.0680737027988,40.1496902177783));
#175772=CARTESIAN_POINT('Ctrl Pts',(58.6161277126018,-6.06037186006759,
40.147567597684));
#175773=CARTESIAN_POINT('Ctrl Pts',(58.6184367045765,-6.05280507414621,
40.1451361443094));
#175774=CARTESIAN_POINT('Ctrl Pts',(58.6209098557463,-6.04539170794176,
40.1424159447501));
#175775=CARTESIAN_POINT('Ctrl Pts',(58.6228395323549,-6.03960742773678,
40.1402935085949));
#175776=CARTESIAN_POINT('Ctrl Pts',(58.6248693309927,-6.03391702093548,
40.1379949176048));
#175777=CARTESIAN_POINT('Ctrl Pts',(58.6269926140964,-6.02832968645946,
40.1355293609261));
#175778=CARTESIAN_POINT('Ctrl Pts',(58.6344241049594,-6.0087740157934,40.1268999125508));
#175779=CARTESIAN_POINT('Ctrl Pts',(58.6430007716254,-5.99048098024828,
40.1162251288835));
#175780=CARTESIAN_POINT('Ctrl Pts',(58.6524381197038,-5.97384499260622,
40.1038990521418));
#175781=CARTESIAN_POINT('Ctrl Pts',(58.657156793743,-5.9655269987852,40.0977360137709));
#175782=CARTESIAN_POINT('Ctrl Pts',(58.6620906399372,-5.95762326711356,
40.0911601532641));
#175783=CARTESIAN_POINT('Ctrl Pts',(58.667204101582,-5.95018309968293,40.084220729064));
#175784=CARTESIAN_POINT('Ctrl Pts',(58.6722957161033,-5.94277472016181,
40.0773109533618));
#175785=CARTESIAN_POINT('Ctrl Pts',(58.6775652709345,-5.93582574548853,
40.0700409753048));
#175786=CARTESIAN_POINT('Ctrl Pts',(58.682978094856,-5.92938546966269,40.0624586415899));
#175787=CARTESIAN_POINT('Ctrl Pts',(58.6830013202262,-5.92935783569705,
40.0624261072769));
#175788=CARTESIAN_POINT('Ctrl Pts',(58.6830245479289,-5.92933021064629,
40.0623935677888));
#175789=CARTESIAN_POINT('Ctrl Pts',(58.6830477779621,-5.92930259451062,
40.0623610231288));
#175790=CARTESIAN_POINT('Ctrl Pts',(58.6940026150818,-5.91627935575194,
40.0470135870241));
#175791=CARTESIAN_POINT('Ctrl Pts',(58.7054384852671,-5.90523719704834,
40.030575529211));
#175792=CARTESIAN_POINT('Ctrl Pts',(58.7171784805271,-5.89609526425064,
40.0133447567366));
#175793=CARTESIAN_POINT('Ctrl Pts',(58.7293455537148,-5.8866207659257,39.9954871626633));
#175794=CARTESIAN_POINT('Ctrl Pts',(58.7418401303837,-5.87918707069946,
39.9767767954363));
#175795=CARTESIAN_POINT('Ctrl Pts',(58.7544760786554,-5.87375524644868,
39.9575197577536));
#175796=CARTESIAN_POINT('Ctrl Pts',(58.7669316835929,-5.86840094651774,
39.938537561207));
#175797=CARTESIAN_POINT('Ctrl Pts',(58.7795255625923,-5.86499195787722,
39.9190226977181));
#175798=CARTESIAN_POINT('Ctrl Pts',(58.792076395308,-5.86353919440062,39.8992655451955));
#175799=CARTESIAN_POINT('Ctrl Pts',(58.8008270591807,-5.86252630185729,
39.8854905069393));
#175800=CARTESIAN_POINT('Ctrl Pts',(58.8095567514049,-5.86246534555135,
39.8715976051508));
#175801=CARTESIAN_POINT('Ctrl Pts',(58.8181995570485,-5.86337364149584,
39.8576902534424));
#175802=CARTESIAN_POINT('',(59.1725467709677,-5.90061356181257,39.2875012672119));
#175803=CARTESIAN_POINT('',(58.8181995570485,-5.8633736414958,39.8576902534424));
#175804=CARTESIAN_POINT('',(59.4651754363832,-0.316925998273047,39.2875012672119));
#175805=CARTESIAN_POINT('Origin',(5.53234440788222E-15,0.,39.2875012672119));
#175806=CARTESIAN_POINT('',(59.1088767419348,-0.316922544675689,39.8576902534424));
#175807=CARTESIAN_POINT('',(59.4651754363832,-0.316925998273047,39.2875012672119));
#175808=CARTESIAN_POINT('',(58.9208513795073,-0.0152121934559198,40.1599502534424));
#175809=CARTESIAN_POINT('Ctrl Pts',(59.1088767419348,-0.316922544675689,
39.8576902534424));
#175810=CARTESIAN_POINT('Ctrl Pts',(59.0966467826998,-0.316922401513862,
39.8772619994055));
#175811=CARTESIAN_POINT('Ctrl Pts',(59.0844716853548,-0.315000085553629,
39.8967644650373));
#175812=CARTESIAN_POINT('Ctrl Pts',(59.0725173476303,-0.311230629648508,
39.9159282836053));
#175813=CARTESIAN_POINT('Ctrl Pts',(59.0603470709112,-0.307393083604294,
39.9354382707198));
#175814=CARTESIAN_POINT('Ctrl Pts',(59.0484046750329,-0.301641096263203,
39.9545987622372));
#175815=CARTESIAN_POINT('Ctrl Pts',(59.0368573319812,-0.294001187892417,
39.9731387498253));
#175816=CARTESIAN_POINT('Ctrl Pts',(59.0257988734949,-0.286684733433703,
39.9908938024085));
#175817=CARTESIAN_POINT('Ctrl Pts',(59.0151019493803,-0.277636448043934,
40.0080810366218));
#175818=CARTESIAN_POINT('Ctrl Pts',(59.0049186872952,-0.266835172448542,
40.0244542742581));
#175819=CARTESIAN_POINT('Ctrl Pts',(58.9968192555025,-0.258244193032669,
40.0374770090511));
#175820=CARTESIAN_POINT('Ctrl Pts',(58.9890447295109,-0.248543417985227,
40.049984877005));
#175821=CARTESIAN_POINT('Ctrl Pts',(58.981678934725,-0.237702773059495,
40.0618424270192));
#175822=CARTESIAN_POINT('Ctrl Pts',(58.9816588284979,-0.237673181620236,
40.0618747942791));
#175823=CARTESIAN_POINT('Ctrl Pts',(58.9816387254916,-0.237643581716976,
40.0619071564124));
#175824=CARTESIAN_POINT('Ctrl Pts',(58.9816186257082,-0.237613973350289,
40.0619395134161));
#175825=CARTESIAN_POINT('Ctrl Pts',(58.9776173965852,-0.231719887006783,
40.0683807661799));
#175826=CARTESIAN_POINT('Ctrl Pts',(58.9737507180862,-0.225454527233356,
40.0746073439084));
#175827=CARTESIAN_POINT('Ctrl Pts',(58.9700384170936,-0.218853219640725,
40.0805869293669));
#175828=CARTESIAN_POINT('Ctrl Pts',(58.9626710986899,-0.205752467569922,
40.092453830807));
#175829=CARTESIAN_POINT('Ctrl Pts',(58.9559120649696,-0.191327202905425,
40.1033475319609));
#175830=CARTESIAN_POINT('Ctrl Pts',(58.9499179036781,-0.175845309932244,
40.1130129263075));
#175831=CARTESIAN_POINT('Ctrl Pts',(58.9454222827095,-0.164233890202358,
40.1202619720674));
#175832=CARTESIAN_POINT('Ctrl Pts',(58.9413569016699,-0.152028117041295,
40.1268200947266));
#175833=CARTESIAN_POINT('Ctrl Pts',(58.9377878323772,-0.139341004226136,
40.1325796782703));
#175834=CARTESIAN_POINT('Ctrl Pts',(58.9364494313924,-0.134583336920451,
40.1347395220992));
#175835=CARTESIAN_POINT('Ctrl Pts',(58.9351808244388,-0.12975798122746,
40.1367870714852));
#175836=CARTESIAN_POINT('Ctrl Pts',(58.933985496586,-0.124870896863315,
40.1387166518767));
#175837=CARTESIAN_POINT('Ctrl Pts',(58.9298018491012,-0.107766101588806,
40.1454701832469));
#175838=CARTESIAN_POINT('Ctrl Pts',(58.9265158655229,-0.0899051301000603,
40.1507785912492));
#175839=CARTESIAN_POINT('Ctrl Pts',(58.9242770147326,-0.0715435052825847,
40.1543986087265));
#175840=CARTESIAN_POINT('Ctrl Pts',(58.9231575893375,-0.0623626928738469,
40.1562086174652));
#175841=CARTESIAN_POINT('Ctrl Pts',(58.9222999481582,-0.0530567171305711,
40.1575965292115));
#175842=CARTESIAN_POINT('Ctrl Pts',(58.9217227791368,-0.043657518385426,
40.1585319382567));
#175843=CARTESIAN_POINT('Ctrl Pts',(58.9214341946262,-0.0389579190128535,
40.1589996427793));
#175844=CARTESIAN_POINT('Ctrl Pts',(58.9212157281805,-0.0342350138894578,
40.159354221642));
#175845=CARTESIAN_POINT('Ctrl Pts',(58.9210697160839,-0.0294927955548823,
40.159591874311));
#175846=CARTESIAN_POINT('Ctrl Pts',(58.9209237039872,-0.0247505772203069,
40.1598295269801));
#175847=CARTESIAN_POINT('Ctrl Pts',(58.9208501479391,-0.0199890456750397,
40.1599502506895));
#175848=CARTESIAN_POINT('Ctrl Pts',(58.9208513795073,-0.0152121934559204,
40.1599502534424));
#175849=CARTESIAN_POINT('',(58.9208533432504,-7.21572344498422E-15,40.1599502534424));
#175850=CARTESIAN_POINT('Origin',(4.7062627014205E-16,0.,40.1599502534424));
#175851=CARTESIAN_POINT('',(58.6605641730809,-7.18384721507414E-15,40.5765));
#175852=CARTESIAN_POINT('',(58.9208513795073,0.0152121934559198,40.1599502534424));
#175853=CARTESIAN_POINT('Origin',(4.7062627014205E-16,0.,40.1599502534424));
#175854=CARTESIAN_POINT('',(59.1088767419348,0.316922544675676,39.8576902534424));
#175855=CARTESIAN_POINT('Ctrl Pts',(58.9208513795073,0.0152121934559198,
40.1599502534424));
#175856=CARTESIAN_POINT('Ctrl Pts',(58.9208504012364,0.0190220008285439,
40.1599502448875));
#175857=CARTESIAN_POINT('Ctrl Pts',(58.9208964366351,0.0228214099817244,
40.1598743450437));
#175858=CARTESIAN_POINT('Ctrl Pts',(58.9209883940807,0.0266084895330077,
40.1597243308498));
#175859=CARTESIAN_POINT('Ctrl Pts',(58.9215313038857,0.0489671208154066,
40.1588386583937));
#175860=CARTESIAN_POINT('Ctrl Pts',(58.9236732325291,0.0708986527648728,
40.155372255361));
#175861=CARTESIAN_POINT('Ctrl Pts',(58.9271900305707,0.0919988953573648,
40.149690217777));
#175862=CARTESIAN_POINT('Ctrl Pts',(58.9285037892496,0.0998812435910838,
40.147567597683));
#175863=CARTESIAN_POINT('Ctrl Pts',(58.93000918782,0.107647933248606,40.1451361443088));
#175864=CARTESIAN_POINT('Ctrl Pts',(58.9316938830317,0.115279202946934,
40.1424159447501));
#175865=CARTESIAN_POINT('Ctrl Pts',(58.933008366749,0.121233502390237,40.1402935085949));
#175866=CARTESIAN_POINT('Ctrl Pts',(58.9344322364591,0.127104908280027,
40.1379949176047));
#175867=CARTESIAN_POINT('Ctrl Pts',(58.9359598525093,0.132883578273087,
40.1355293609261));
#175868=CARTESIAN_POINT('Ctrl Pts',(58.9413065086849,0.153108923248799,
40.1268999125508));
#175869=CARTESIAN_POINT('Ctrl Pts',(58.9479240485795,0.172198253417729,
40.1162251288835));
#175870=CARTESIAN_POINT('Ctrl Pts',(58.9555707636545,0.189729578870784,
40.1038990521418));
#175871=CARTESIAN_POINT('Ctrl Pts',(58.959394121192,0.198495241597312,40.0977360137709));
#175872=CARTESIAN_POINT('Ctrl Pts',(58.9634747743348,0.206871403160556,
40.0911601532641));
#175873=CARTESIAN_POINT('Ctrl Pts',(58.9677825146337,0.214805314863219,
40.084220729064));
#175874=CARTESIAN_POINT('Ctrl Pts',(58.9720718502312,0.222705329147635,
40.0773109533618));
#175875=CARTESIAN_POINT('Ctrl Pts',(58.9765861722458,0.230167055079184,
40.0700409753048));
#175876=CARTESIAN_POINT('Ctrl Pts',(58.9812961520165,0.237137844566655,
40.0624586415899));
#175877=CARTESIAN_POINT('Ctrl Pts',(58.9813163616197,0.237167754862796,
40.0624261072769));
#175878=CARTESIAN_POINT('Ctrl Pts',(58.9813365744745,0.237197656536702,
40.0623935677888));
#175879=CARTESIAN_POINT('Ctrl Pts',(58.9813567905789,0.237227549587952,
40.0623610231288));
#175880=CARTESIAN_POINT('Ctrl Pts',(58.9908903168209,0.251324537972177,
40.0470135870234));
#175881=CARTESIAN_POINT('Ctrl Pts',(59.0011093202327,0.263501580512099,
40.0305755292095));
#175882=CARTESIAN_POINT('Ctrl Pts',(59.0118294103843,0.27382059650901,40.0133447567343));
#175883=CARTESIAN_POINT('Ctrl Pts',(59.0229394763223,0.284514998003889,
39.9954871626602));
#175884=CARTESIAN_POINT('Ctrl Pts',(59.0345885736552,0.293214009568411,
39.9767767954322));
#175885=CARTESIAN_POINT('Ctrl Pts',(59.046587520639,0.299936893972332,39.9575197577486));
#175886=CARTESIAN_POINT('Ctrl Pts',(59.0584152157263,0.306563827731132,
39.9385375612012));
#175887=CARTESIAN_POINT('Ctrl Pts',(59.0705837677954,0.311270560393325,
39.9190226977114));
#175888=CARTESIAN_POINT('Ctrl Pts',(59.0829139906031,0.314027284735693,
39.899265545188));
#175889=CARTESIAN_POINT('Ctrl Pts',(59.0915108413209,0.315949321994159,
39.8854905069342));
#175890=CARTESIAN_POINT('Ctrl Pts',(59.1001863397071,0.316922445687698,
39.8715976051483));
#175891=CARTESIAN_POINT('Ctrl Pts',(59.1088767419348,0.316922544675652,
39.8576902534424));
#175892=CARTESIAN_POINT('',(59.4651754363832,0.316925998273047,39.2875012672119));
#175893=CARTESIAN_POINT('',(59.1088767419348,0.316922544675689,39.8576902534424));
#175894=CARTESIAN_POINT('',(59.1725467709678,5.90061356181176,39.2875012672119));
#175895=CARTESIAN_POINT('Origin',(5.53234440788222E-15,0.,39.2875012672119));
#175896=CARTESIAN_POINT('',(58.8181995570486,5.863373641495,39.8576902534424));
#175897=CARTESIAN_POINT('',(59.1725467709678,5.90061356181176,39.2875012672119));
#175898=CARTESIAN_POINT('',(58.5996668978649,6.14377718965242,40.1599502534424));
#175899=CARTESIAN_POINT('Ctrl Pts',(58.8181995570486,5.863373641495,39.8576902534424));
#175900=CARTESIAN_POINT('Ctrl Pts',(58.806036579845,5.86209540502784,39.877261999406));
#175901=CARTESIAN_POINT('Ctrl Pts',(58.7937272422237,5.86273454612455,39.8967644650383));
#175902=CARTESIAN_POINT('Ctrl Pts',(58.7814443761786,5.86523378400424,39.9159282836067));
#175903=CARTESIAN_POINT('Ctrl Pts',(58.7689396367178,5.86777816724686,39.9354382707217));
#175904=CARTESIAN_POINT('Ctrl Pts',(58.7564614161358,5.87225032431083,39.9545987622396));
#175905=CARTESIAN_POINT('Ctrl Pts',(58.7441787427557,5.87864135444053,39.9731387498282));
#175906=CARTESIAN_POINT('Ctrl Pts',(58.7324160859207,5.88476180492487,39.9908938024117));
#175907=CARTESIAN_POINT('Ctrl Pts',(58.7208319573083,5.8926423898216,40.0080810366254));
#175908=CARTESIAN_POINT('Ctrl Pts',(58.7095754394589,5.90232005416288,40.024454274262));
#175909=CARTESIAN_POINT('Ctrl Pts',(58.7006223753257,5.91001735013546,40.0374770090537));
#175910=CARTESIAN_POINT('Ctrl Pts',(58.6918764318935,5.91885232406688,40.0499848770062));
#175911=CARTESIAN_POINT('Ctrl Pts',(58.6834178317481,5.92886364759471,40.0618424270193));
#175912=CARTESIAN_POINT('Ctrl Pts',(58.6833947425173,5.92889097525594,40.0618747942791));
#175913=CARTESIAN_POINT('Ctrl Pts',(58.6833716556051,5.92891831167149,40.0619071564124));
#175914=CARTESIAN_POINT('Ctrl Pts',(58.6833485710133,5.92894565684097,40.0619395134161));
#175915=CARTESIAN_POINT('Ctrl Pts',(58.6787531612542,5.93438921243137,40.0683807661799));
#175916=CARTESIAN_POINT('Ctrl Pts',(58.6742527563957,5.94021607194697,40.0746073439084));
#175917=CARTESIAN_POINT('Ctrl Pts',(58.6698707672382,5.94639317576796,40.0805869293669));
#175918=CARTESIAN_POINT('Ctrl Pts',(58.6611744062939,5.95865206607701,40.092453830807));
#175919=CARTESIAN_POINT('Ctrl Pts',(58.6529445485199,5.97229179622438,40.1033475319609));
#175920=CARTESIAN_POINT('Ctrl Pts',(58.6453649253902,5.98706231729958,40.1130129263075));
#175921=CARTESIAN_POINT('Ctrl Pts',(58.6396802080429,5.99814020810598,40.1202619720674));
#175922=CARTESIAN_POINT('Ctrl Pts',(58.6343612468745,6.00985416873189,40.1268200947266));
#175923=CARTESIAN_POINT('Ctrl Pts',(58.629485564911,6.02209871088711,40.1325796782703));
#175924=CARTESIAN_POINT('Ctrl Pts',(58.6276571841746,6.02669041419532,40.1347395220992));
#175925=CARTESIAN_POINT('Ctrl Pts',(58.6258911397673,6.03135673054958,40.1367870714852));
#175926=CARTESIAN_POINT('Ctrl Pts',(58.6241915206271,6.03609209717068,40.1387166518767));
#175927=CARTESIAN_POINT('Ctrl Pts',(58.6182428536364,6.05266588034453,40.1454701832469));
#175928=CARTESIAN_POINT('Ctrl Pts',(58.6131078911178,6.07008552874888,40.1507785912492));
#175929=CARTESIAN_POINT('Ctrl Pts',(58.6089619925611,6.0881125430318,40.1543986087265));
#175930=CARTESIAN_POINT('Ctrl Pts',(58.6068890432828,6.09712605017327,40.1562086174652));
#175931=CARTESIAN_POINT('Ctrl Pts',(58.6050633610079,6.10629139889321,40.1575965292115));
#175932=CARTESIAN_POINT('Ctrl Pts',(58.6035068699781,6.11557877725333,40.1585319382567));
#175933=CARTESIAN_POINT('Ctrl Pts',(58.6027286244632,6.12022246643339,40.1589996427793));
#175934=CARTESIAN_POINT('Ctrl Pts',(58.6020176767849,6.12489666302651,40.159354221642));
#175935=CARTESIAN_POINT('Ctrl Pts',(58.6013767677628,6.12959764057279,40.159591874311));
#175936=CARTESIAN_POINT('Ctrl Pts',(58.6007358587407,6.13429861811906,40.1598295269801));
#175937=CARTESIAN_POINT('Ctrl Pts',(58.6001649900651,6.13902637679564,40.1599502506895));
#175938=CARTESIAN_POINT('Ctrl Pts',(58.5996668978649,6.14377718965242,40.1599502534424));
#175939=CARTESIAN_POINT('',(58.5964866834552,6.17403490858941,40.1599502534424));
#175940=CARTESIAN_POINT('Origin',(5.72296091834672E-15,5.25982985649545E-15,
40.1599502534424));
#175941=CARTESIAN_POINT('',(58.7519447039089,6.49374646112659,39.8576902534424));
#175942=CARTESIAN_POINT('Ctrl Pts',(58.5964866834552,6.17403490858941,40.1599502534424));
#175943=CARTESIAN_POINT('Ctrl Pts',(58.5960874772333,6.17782374318146,40.1599502448875));
#175944=CARTESIAN_POINT('Ctrl Pts',(58.5957361140452,6.18160715078324,40.1598743450437));
#175945=CARTESIAN_POINT('Ctrl Pts',(58.5954317101325,6.18538309648697,40.1597243308499));
#175946=CARTESIAN_POINT('Ctrl Pts',(58.5936345324522,6.20767599437318,40.1588386583938));
#175947=CARTESIAN_POINT('Ctrl Pts',(58.5934722580545,6.22971127560327,40.1553722553617));
#175948=CARTESIAN_POINT('Ctrl Pts',(58.5947642147753,6.25106353435202,40.1496902177787));
#175949=CARTESIAN_POINT('Ctrl Pts',(58.5952468467988,6.25904002743534,40.1475675976843));
#175950=CARTESIAN_POINT('Ctrl Pts',(58.595932158504,6.26692152735556,40.1451361443095));
#175951=CARTESIAN_POINT('Ctrl Pts',(58.5968099398849,6.27468709076361,40.1424159447501));
#175952=CARTESIAN_POINT('Ctrl Pts',(58.5974948289522,6.28074617289452,40.1402935085949));
#175953=CARTESIAN_POINT('Ctrl Pts',(58.5982971695202,6.2867342495212,40.1379949176048));
#175954=CARTESIAN_POINT('Ctrl Pts',(58.5992123816357,6.29264094271359,40.1355293609261));
#175955=CARTESIAN_POINT('Ctrl Pts',(58.6024156240399,6.31331436888697,40.1268999125508));
#175956=CARTESIAN_POINT('Ctrl Pts',(58.6070015340113,6.33299084698369,40.1162251288835));
#175957=CARTESIAN_POINT('Ctrl Pts',(58.6127738370723,6.35122543337742,40.1038990521418));
#175958=CARTESIAN_POINT('Ctrl Pts',(58.6156599886029,6.36034272657428,40.097736013771));
#175959=CARTESIAN_POINT('Ctrl Pts',(58.6188427402045,6.36909954705021,40.0911601532641));
#175960=CARTESIAN_POINT('Ctrl Pts',(58.6222975626533,6.37744027742802,40.084220729064));
#175961=CARTESIAN_POINT('Ctrl Pts',(58.6257376244687,6.38574537226605,40.0773109533618));
#175962=CARTESIAN_POINT('Ctrl Pts',(58.62944725381,6.3936380972251,40.0700409753048));
#175963=CARTESIAN_POINT('Ctrl Pts',(58.6334027859058,6.40106302694584,40.0624586415899));
#175964=CARTESIAN_POINT('Ctrl Pts',(58.6334197583214,6.40109488586902,40.0624261072769));
#175965=CARTESIAN_POINT('Ctrl Pts',(58.6334367348721,6.40112673655708,40.0623935677888));
#175966=CARTESIAN_POINT('Ctrl Pts',(58.6334537155558,6.40115857900939,40.0623610231288));
#175967=CARTESIAN_POINT('Ctrl Pts',(58.6414614796113,6.41617486746432,40.047013587023));
#175968=CARTESIAN_POINT('Ctrl Pts',(58.6503516547097,6.42935337961424,40.0305755292085));
#175969=CARTESIAN_POINT('Ctrl Pts',(58.6599343882014,6.44073642151171,40.0133447567327));
#175970=CARTESIAN_POINT('Ctrl Pts',(58.6698657226823,6.45253355607577,39.995487162658));
#175971=CARTESIAN_POINT('Ctrl Pts',(58.6805417107307,6.46240257578753,39.9767767954295));
#175972=CARTESIAN_POINT('Ctrl Pts',(58.6917721934523,6.47034286301631,39.9575197577452));
#175973=CARTESIAN_POINT('Ctrl Pts',(58.7028423919867,6.47816982453002,39.9385375611974));
#175974=CARTESIAN_POINT('Ctrl Pts',(58.7144522959225,6.48412273326606,39.9190226977072));
#175975=CARTESIAN_POINT('Ctrl Pts',(58.7264268163207,6.48815321522562,39.8992655451833));
#175976=CARTESIAN_POINT('Ctrl Pts',(58.7347756649889,6.49096333895681,39.885490506931));
#175977=CARTESIAN_POINT('Ctrl Pts',(58.743301918962,6.49283796829098,39.8715976051467));
#175978=CARTESIAN_POINT('Ctrl Pts',(58.7519447039089,6.49374646112657,39.8576902534424));
#175979=CARTESIAN_POINT('',(59.1062911958297,6.53099325079975,39.2875012672119));
#175980=CARTESIAN_POINT('',(58.7519447039089,6.49374646112661,39.8576902534424));
#175981=CARTESIAN_POINT('',(58.2316113004783,12.0535047649314,39.2875012672119));
#175982=CARTESIAN_POINT('Origin',(5.53234440788222E-15,0.,39.2875012672119));
#175983=CARTESIAN_POINT('',(57.8830978693157,11.9794294790605,39.8576902534424));
#175984=CARTESIAN_POINT('',(58.2316113004783,12.0535047649314,39.2875012672119));
#175985=CARTESIAN_POINT('',(57.6364522029208,12.2354540642037,40.1599502534424));
#175986=CARTESIAN_POINT('Ctrl Pts',(57.8830978693157,11.9794294790605,39.8576902534424));
#175987=CARTESIAN_POINT('Ctrl Pts',(57.8711351342687,11.9768868675908,39.8772619994041));
#175988=CARTESIAN_POINT('Ctrl Pts',(57.8588264200514,11.9762358312602,39.8967644650345));
#175989=CARTESIAN_POINT('Ctrl Pts',(57.8463495993381,11.9774374689406,39.9159282836011));
#175990=CARTESIAN_POINT('Ctrl Pts',(57.8336474016793,11.9786608125857,39.9354382707143));
#175991=CARTESIAN_POINT('Ctrl Pts',(57.8207700703912,11.9818041414828,39.9545987622304));
#175992=CARTESIAN_POINT('Ctrl Pts',(57.8078866382242,11.9868762719063,39.9731387498174));
#175993=CARTESIAN_POINT('Ctrl Pts',(57.7955486571716,11.9917336614784,39.9908938023995));
#175994=CARTESIAN_POINT('Ctrl Pts',(57.7832042422,11.9983602045428,40.0080810366118));
#175995=CARTESIAN_POINT('Ctrl Pts',(57.7709977973527,12.0068082271118,40.0244542742474));
#175996=CARTESIAN_POINT('Ctrl Pts',(57.7612891925185,12.0135275064579,40.0374770090443));
#175997=CARTESIAN_POINT('Ctrl Pts',(57.7516676540279,12.0213998814534,40.0499848770018));
#175998=CARTESIAN_POINT('Ctrl Pts',(57.7422089227119,12.0304721974322,40.0618424270192));
#175999=CARTESIAN_POINT('Ctrl Pts',(57.7421831034479,12.0304969619079,40.0618747942791));
#176000=CARTESIAN_POINT('Ctrl Pts',(57.7421572855747,12.0305217353322,40.0619071564124));
#176001=CARTESIAN_POINT('Ctrl Pts',(57.7421314690942,12.0305465177051,40.0619395134161));
#176002=CARTESIAN_POINT('Ctrl Pts',(57.73699222697,12.0354799018082,40.0683807661799));
#176003=CARTESIAN_POINT('Ctrl Pts',(57.7319074031293,12.0408044207737,40.0746073439084));
#176004=CARTESIAN_POINT('Ctrl Pts',(57.726903735797,12.046489643181,40.0805869293669));
#176005=CARTESIAN_POINT('Ctrl Pts',(57.7169736114626,12.0577723607607,40.092453830807));
#176006=CARTESIAN_POINT('Ctrl Pts',(57.7073630976789,12.0704771166532,40.1033475319609));
#176007=CARTESIAN_POINT('Ctrl Pts',(57.6982810566481,12.0843744369106,40.1130129263075));
#176008=CARTESIAN_POINT('Ctrl Pts',(57.691469525875,12.0947974271036,40.1202619720674));
#176009=CARTESIAN_POINT('Ctrl Pts',(57.6849552602294,12.1058912345904,40.1268200947266));
#176010=CARTESIAN_POINT('Ctrl Pts',(57.6788263845869,12.1175590523195,40.1325796782703));
#176011=CARTESIAN_POINT('Ctrl Pts',(57.676528056221,12.1219344839679,40.1347395220992));
#176012=CARTESIAN_POINT('Ctrl Pts',(57.6742839235121,12.126390635845,40.1367870714852));
#176013=CARTESIAN_POINT('Ctrl Pts',(57.6720986344674,12.1309224030554,40.1387166518767));
#176014=CARTESIAN_POINT('Ctrl Pts',(57.6644501228112,12.1467835882919,40.1454701832469));
#176015=CARTESIAN_POINT('Ctrl Pts',(57.6575224410762,12.1635710602986,40.1507785912492));
#176016=CARTESIAN_POINT('Ctrl Pts',(57.6515149180853,12.1810659563061,40.1543986087265));
#176017=CARTESIAN_POINT('Ctrl Pts',(57.6485111565899,12.1898134043099,40.1562086174652));
#176018=CARTESIAN_POINT('Ctrl Pts',(57.6457374357766,12.1987377085279,40.1575965292115));
#176019=CARTESIAN_POINT('Ctrl Pts',(57.6432186759797,12.2078115120422,40.1585319382567));
#176020=CARTESIAN_POINT('Ctrl Pts',(57.6419592960813,12.2123484137993,40.1589996427793));
#176021=CARTESIAN_POINT('Ctrl Pts',(57.6407636564618,12.2169226903862,40.159354221642));
#176022=CARTESIAN_POINT('Ctrl Pts',(57.6396348724477,12.2215309222504,40.159591874311));
#176023=CARTESIAN_POINT('Ctrl Pts',(57.6385060884335,12.2261391541146,40.1598295269801));
#176024=CARTESIAN_POINT('Ctrl Pts',(57.6374441616871,12.2307813416091,40.1599502506895));
#176025=CARTESIAN_POINT('Ctrl Pts',(57.6364522029208,12.2354540642037,40.1599502534424));
#176026=CARTESIAN_POINT('',(57.6301266171959,12.2652136052653,40.1599502534424));
#176027=CARTESIAN_POINT('Origin',(5.72184526906101E-15,5.26687378886292E-15,
40.1599502534424));
#176028=CARTESIAN_POINT('',(57.7513140650722,12.5994235324464,39.8576902534424));
#176029=CARTESIAN_POINT('Ctrl Pts',(57.6301266171959,12.2652136052653,40.1599502534424));
#176030=CARTESIAN_POINT('Ctrl Pts',(57.6293335568101,12.2689399558122,40.1599502448875));
#176031=CARTESIAN_POINT('Ctrl Pts',(57.6285886446437,12.2726659100571,40.1598743450437));
#176032=CARTESIAN_POINT('Ctrl Pts',(57.6278912144857,12.276389351862,40.1597243308498));
#176033=CARTESIAN_POINT('Ctrl Pts',(57.6237736395748,12.2983722707006,40.1588386583938));
#176034=CARTESIAN_POINT('Ctrl Pts',(57.6213089400485,12.3202698780618,40.1553722553615));
#176035=CARTESIAN_POINT('Ctrl Pts',(57.620361900501,12.3416402131543,40.1496902177781));
#176036=CARTESIAN_POINT('Ctrl Pts',(57.6200081180517,12.349623458957,40.1475675976839));
#176037=CARTESIAN_POINT('Ctrl Pts',(57.6198658344727,12.3575334177747,40.1451361443093));
#176038=CARTESIAN_POINT('Ctrl Pts',(57.6199270848659,12.365348193752,40.1424159447501));
#176039=CARTESIAN_POINT('Ctrl Pts',(57.6199748754953,12.3714456739988,40.1402935085949));
#176040=CARTESIAN_POINT('Ctrl Pts',(57.62014689631,12.3774848147417,40.1379949176047));
#176041=CARTESIAN_POINT('Ctrl Pts',(57.6204396772353,12.3834548161668,40.1355293609261));
#176042=CARTESIAN_POINT('Ctrl Pts',(57.6214644104742,12.4043498211545,40.1268999125508));
#176043=CARTESIAN_POINT('Ctrl Pts',(57.6239684463329,12.4243978675674,40.1162251288835));
#176044=CARTESIAN_POINT('Ctrl Pts',(57.6278030948198,12.4431359329574,40.1038990521418));
#176045=CARTESIAN_POINT('Ctrl Pts',(57.6297204190632,12.4525049656524,40.0977360137709));
#176046=CARTESIAN_POINT('Ctrl Pts',(57.6319703982311,12.4615465034834,40.0911601532641));
#176047=CARTESIAN_POINT('Ctrl Pts',(57.6345344510721,12.470202669749,40.084220729064));
#176048=CARTESIAN_POINT('Ctrl Pts',(57.6370875490682,12.4788218527836,40.0773109533618));
#176049=CARTESIAN_POINT('Ctrl Pts',(57.6399518422609,12.4870591024238,40.0700409753048));
#176050=CARTESIAN_POINT('Ctrl Pts',(57.6431095890444,12.4948568232941,40.0624586415899));
#176051=CARTESIAN_POINT('Ctrl Pts',(57.6431231383191,12.4948902817913,40.0624261072769));
#176052=CARTESIAN_POINT('Ctrl Pts',(57.6431366925669,12.4949237325307,40.0623935677888));
#176053=CARTESIAN_POINT('Ctrl Pts',(57.6431502517861,12.4949571755115,40.0623610231288));
#176054=CARTESIAN_POINT('Ctrl Pts',(57.6495445189161,12.5107282424382,40.0470135870228));
#176055=CARTESIAN_POINT('Ctrl Pts',(57.657008463082,12.524763837661,40.0305755292082));
#176056=CARTESIAN_POINT('Ctrl Pts',(57.6653488494803,12.5370861904698,40.0133447567321));
#176057=CARTESIAN_POINT('Ctrl Pts',(57.673992642725,12.549856806228,39.9954871626571));
#176058=CARTESIAN_POINT('Ctrl Pts',(57.6835785531295,12.5607877070418,39.9767767954283));
#176059=CARTESIAN_POINT('Ctrl Pts',(57.69391752807,12.569858401647,39.9575197577437));
#176060=CARTESIAN_POINT('Ctrl Pts',(57.7041089426397,12.5787996370875,39.9385375611954));
#176061=CARTESIAN_POINT('Ctrl Pts',(57.7150329979052,12.5859335005837,39.9190226977048));
#176062=CARTESIAN_POINT('Ctrl Pts',(57.7265206205425,12.591193581357,39.8992655451805));
#176063=CARTESIAN_POINT('Ctrl Pts',(57.7345299954284,12.5948610032573,39.8854905069291));
#176064=CARTESIAN_POINT('Ctrl Pts',(57.742813589566,12.5976165994009,39.8715976051458));
#176065=CARTESIAN_POINT('Ctrl Pts',(57.7513140650722,12.5994235324464,39.8576902534424));
#176066=CARTESIAN_POINT('',(58.0998260601482,12.6735055745733,39.2875012672119));
#176067=CARTESIAN_POINT('',(57.7513140650722,12.5994235324464,39.8576902534424));
#176068=CARTESIAN_POINT('',(56.6526781108326,18.0743352474884,39.2875012672119));
#176069=CARTESIAN_POINT('Origin',(5.53234440788222E-15,0.,39.2875012672119));
#176070=CARTESIAN_POINT('',(56.3138168485097,17.9642361803965,39.8576902534424));
#176071=CARTESIAN_POINT('',(56.6526781108326,18.0743352474884,39.2875012672119));
#176072=CARTESIAN_POINT('',(56.0417604764386,18.1930767435942,40.1599502534424));
#176073=CARTESIAN_POINT('Ctrl Pts',(56.3138168485097,17.9642361803965,39.8576902534424));
#176074=CARTESIAN_POINT('Ctrl Pts',(56.302185421847,17.9604570513077,39.8772619994036));
#176075=CARTESIAN_POINT('Ctrl Pts',(56.2900121878815,17.9585229704403,39.8967644650334));
#176076=CARTESIAN_POINT('Ctrl Pts',(56.2774781111578,17.9584138425281,39.9159282835995));
#176077=CARTESIAN_POINT('Ctrl Pts',(56.2647176232359,17.9583027433672,39.935438270712));
#176078=CARTESIAN_POINT('Ctrl Pts',(56.2515822679773,17.9600828051289,39.9545987622276));
#176079=CARTESIAN_POINT('Ctrl Pts',(56.2382392306015,17.9637804645249,39.9731387498141));
#176080=CARTESIAN_POINT('Ctrl Pts',(56.225461102833,17.9673215746091,39.9908938023957));
#176081=CARTESIAN_POINT('Ctrl Pts',(56.2124916494954,17.9726214740499,40.0080810366076));
#176082=CARTESIAN_POINT('Ctrl Pts',(56.1994690140138,17.9797472965448,40.0244542742428));
#176083=CARTESIAN_POINT('Ctrl Pts',(56.1891112379872,17.9854149414322,40.0374770090413));
#176084=CARTESIAN_POINT('Ctrl Pts',(56.1787195200293,17.9922384661018,40.0499848770004));
#176085=CARTESIAN_POINT('Ctrl Pts',(56.1683642893845,18.0002723763365,40.0618424270192));
#176086=CARTESIAN_POINT('Ctrl Pts',(56.1683360229685,18.0002943063017,40.0618747942791));
#176087=CARTESIAN_POINT('Ctrl Pts',(56.1683077570003,18.000316245312,40.0619071564124));
#176088=CARTESIAN_POINT('Ctrl Pts',(56.1682794914818,18.0003381933675,40.0619395134161));
#176089=CARTESIAN_POINT('Ctrl Pts',(56.1626527236048,18.0047073547947,40.0683807661799));
#176090=CARTESIAN_POINT('Ctrl Pts',(56.157039191176,18.0094711966661,40.0746073439084));
#176091=CARTESIAN_POINT('Ctrl Pts',(56.1514686668953,18.0146022491732,40.0805869293669));
#176092=CARTESIAN_POINT('Ctrl Pts',(56.1404135756909,18.0247851782088,40.092453830807));
#176093=CARTESIAN_POINT('Ctrl Pts',(56.1295277006976,18.0364157638821,40.1033475319609));
#176094=CARTESIAN_POINT('Ctrl Pts',(56.1190427465078,18.0492876213728,40.1130129263075));
#176095=CARTESIAN_POINT('Ctrl Pts',(56.1111790308655,18.0589415144907,40.1202619720674));
#176096=CARTESIAN_POINT('Ctrl Pts',(56.1035408324003,18.0692936227621,40.1268200947266));
#176097=CARTESIAN_POINT('Ctrl Pts',(56.096225912323,18.0802568810124,40.1325796782703));
#176098=CARTESIAN_POINT('Ctrl Pts',(56.0934828172939,18.0843681028563,40.1347395220992));
#176099=CARTESIAN_POINT('Ctrl Pts',(56.090785183471,18.0885652677237,40.1367870714852));
#176100=CARTESIAN_POINT('Ctrl Pts',(56.088138167006,18.0928437845335,40.1387166518767));
#176101=CARTESIAN_POINT('Ctrl Pts',(56.0788736093786,18.107818593368,40.1454701832469));
#176102=CARTESIAN_POINT('Ctrl Pts',(56.0702291095579,18.1237899619208,40.1507785912492));
#176103=CARTESIAN_POINT('Ctrl Pts',(56.0624257818119,18.1405610619111,40.1543986087265));
#176104=CARTESIAN_POINT('Ctrl Pts',(56.0585241179389,18.1489466119063,40.1562086174652));
#176105=CARTESIAN_POINT('Ctrl Pts',(56.0548327480527,18.157532095078,40.1575965292115));
#176106=CARTESIAN_POINT('Ctrl Pts',(56.0513793155483,18.1662929092563,40.1585319382567));
#176107=CARTESIAN_POINT('Ctrl Pts',(56.049652599296,18.1706733163454,40.1589996427793));
#176108=CARTESIAN_POINT('Ctrl Pts',(56.0479853674133,18.1750975561945,40.159354221642));
#176109=CARTESIAN_POINT('Ctrl Pts',(56.0463810756009,18.179562553624,40.159591874311));
#176110=CARTESIAN_POINT('Ctrl Pts',(56.0447767837886,18.1840275510536,40.1598295269801));
#176111=CARTESIAN_POINT('Ctrl Pts',(56.043235433663,18.1885333065883,40.1599502506895));
#176112=CARTESIAN_POINT('Ctrl Pts',(56.0417604764386,18.1930767435942,40.1599502534424));
#176113=CARTESIAN_POINT('',(56.0323588238394,18.222012055021,40.1599502534424));
#176114=CARTESIAN_POINT('Origin',(5.71999943999309E-15,5.27376251672649E-15,
40.1599502534424));
#176115=CARTESIAN_POINT('',(56.1179479440991,18.5670586829459,39.8576902534424));
#176116=CARTESIAN_POINT('Ctrl Pts',(56.0323588238394,18.222012055021,40.1599502534424));
#176117=CARTESIAN_POINT('Ctrl Pts',(56.031180598225,18.2256350948462,40.1599502448875));
#176118=CARTESIAN_POINT('Ctrl Pts',(56.030050298494,18.2292627734,40.1598743450437));
#176119=CARTESIAN_POINT('Ctrl Pts',(56.0289674832815,18.2328929164984,40.1597243308499));
#176120=CARTESIAN_POINT('Ctrl Pts',(56.0225746241526,18.2543250068291,40.1588386583938));
#176121=CARTESIAN_POINT('Ctrl Pts',(56.0178345032616,18.2758450255515,40.1553722553616));
#176122=CARTESIAN_POINT('Ctrl Pts',(56.0146588434091,18.2969992991233,40.1496902177785));
#176123=CARTESIAN_POINT('Ctrl Pts',(56.0134725226012,18.3049018315349,40.1475675976842));
#176124=CARTESIAN_POINT('Ctrl Pts',(56.0125042026268,18.3127535860873,40.1451361443095));
#176125=CARTESIAN_POINT('Ctrl Pts',(56.0117482509602,18.3205319543142,40.1424159447501));
#176126=CARTESIAN_POINT('Ctrl Pts',(56.0111584195475,18.3266010274072,40.1402935085949));
#176127=CARTESIAN_POINT('Ctrl Pts',(56.0106982359128,18.3326250661767,40.1379949176047));
#176128=CARTESIAN_POINT('Ctrl Pts',(56.010365377879,18.3385929672495,40.1355293609261));
#176129=CARTESIAN_POINT('Ctrl Pts',(56.0092003747606,18.3594806210043,40.1268999125508));
#176130=CARTESIAN_POINT('Ctrl Pts',(56.0095951017658,18.3796805851416,40.1162251288835));
#176131=CARTESIAN_POINT('Ctrl Pts',(56.0114500824673,18.3987168313623,40.1038990521418));
#176132=CARTESIAN_POINT('Ctrl Pts',(56.012377572818,18.4082349544727,40.0977360137709));
#176133=CARTESIAN_POINT('Ctrl Pts',(56.0136701283095,18.4174621486782,40.0911601532641));
#176134=CARTESIAN_POINT('Ctrl Pts',(56.0153153192432,18.4263389120624,40.084220729064));
#176135=CARTESIAN_POINT('Ctrl Pts',(56.0169534811442,18.4351777497207,40.0773109533618));
#176136=CARTESIAN_POINT('Ctrl Pts',(56.0189410563926,18.4436692750113,40.0700409753048));
#176137=CARTESIAN_POINT('Ctrl Pts',(56.0212664209293,18.4517543535694,40.0624586415899));
#176138=CARTESIAN_POINT('Ctrl Pts',(56.0212763986143,18.4517890450622,40.0624261072769));
#176139=CARTESIAN_POINT('Ctrl Pts',(56.0212863820562,18.4518237293597,40.0623935677888));
#176140=CARTESIAN_POINT('Ctrl Pts',(56.0212963712531,18.4518584064607,40.0623610231288));
#176141=CARTESIAN_POINT('Ctrl Pts',(56.0260070845284,18.4682114607482,40.047013587024));
#176142=CARTESIAN_POINT('Ctrl Pts',(56.031963021227,18.4829503621244,40.0305755292107));
#176143=CARTESIAN_POINT('Ctrl Pts',(56.0389696815123,18.4960770195677,40.0133447567361));
#176144=CARTESIAN_POINT('Ctrl Pts',(56.0462312303122,18.5096811989804,39.9954871626627));
#176145=CARTESIAN_POINT('Ctrl Pts',(56.0546220378314,18.5215542196589,39.9767767954356));
#176146=CARTESIAN_POINT('Ctrl Pts',(56.0639562290165,18.531655941212,39.9575197577527));
#176147=CARTESIAN_POINT('Ctrl Pts',(56.0731572003495,18.5416134885325,39.9385375612061));
#176148=CARTESIAN_POINT('Ctrl Pts',(56.0832757207076,18.5498501466877,39.9190226977172));
#176149=CARTESIAN_POINT('Ctrl Pts',(56.0941505847851,18.5562821957293,39.8992655451945));
#176150=CARTESIAN_POINT('Ctrl Pts',(56.1017327335043,18.5607667347594,39.8854905069386));
#176151=CARTESIAN_POINT('Ctrl Pts',(56.1096829110188,18.564373106826,39.8715976051505));
#176152=CARTESIAN_POINT('Ctrl Pts',(56.1179479440991,18.5670586829458,39.8576902534424));
#176153=CARTESIAN_POINT('',(56.4568070719814,18.6771643191703,39.2875012672119));
#176154=CARTESIAN_POINT('',(56.1179479440991,18.5670586829459,39.8576902534424));
#176155=CARTESIAN_POINT('',(54.4530463244696,23.8971395307762,39.2875012672119));
#176156=CARTESIAN_POINT('Origin',(5.53234440788222E-15,0.,39.2875012672119));
#176157=CARTESIAN_POINT('',(54.1275498658877,23.7522229508821,39.8576902534424));
#176158=CARTESIAN_POINT('',(54.4530463244695,23.8971395307762,39.2875012672119));
#176159=CARTESIAN_POINT('',(53.8330634946841,23.9513722670358,40.1599502534424));
#176160=CARTESIAN_POINT('Ctrl Pts',(54.1275498658877,23.7522229508821,39.8576902534424));
#176161=CARTESIAN_POINT('Ctrl Pts',(54.1163771839515,23.7472487091024,39.8772619994067));
#176162=CARTESIAN_POINT('Ctrl Pts',(54.1044728027344,23.7440527738927,39.8967644650396));
#176163=CARTESIAN_POINT('Ctrl Pts',(54.0920187959652,23.7426340760165,39.9159282836086));
#176164=CARTESIAN_POINT('Ctrl Pts',(54.0793398243537,23.7411897512758,39.9354382707242));
#176165=CARTESIAN_POINT('Ctrl Pts',(54.0660903588227,23.7415870431742,39.9545987622426));
#176166=CARTESIAN_POINT('Ctrl Pts',(54.052433905345,23.7438697192144,39.9731387498317));
#176167=CARTESIAN_POINT('Ctrl Pts',(54.0393556306996,23.7460557526694,39.9908938024159));
#176168=CARTESIAN_POINT('Ctrl Pts',(54.0259032350379,23.7499709416819,40.0080810366301));
#176169=CARTESIAN_POINT('Ctrl Pts',(54.0122070876386,23.7556964921038,40.0244542742672));
#176170=CARTESIAN_POINT('Ctrl Pts',(54.001313622389,23.7602504066272,40.0374770090569));
#176171=CARTESIAN_POINT('Ctrl Pts',(53.9902655788085,23.765950321003,40.0499848770078));
#176172=CARTESIAN_POINT('Ctrl Pts',(53.9791273029166,23.7728578042865,40.0618424270193));
#176173=CARTESIAN_POINT('Ctrl Pts',(53.9790968990415,23.7728766594721,40.0618747942791));
#176174=CARTESIAN_POINT('Ctrl Pts',(53.9790664946662,23.7728955236999,40.0619071564124));
#176175=CARTESIAN_POINT('Ctrl Pts',(53.9790360897926,23.7729143969704,40.0619395134161));
#176176=CARTESIAN_POINT('Ctrl Pts',(53.972983444209,23.7766714662748,40.0683807661799));
#176177=CARTESIAN_POINT('Ctrl Pts',(53.9669027062282,23.7808224374038,40.0746073439084));
#176178=CARTESIAN_POINT('Ctrl Pts',(53.9608263568289,23.7853431031257,40.0805869293668));
#176179=CARTESIAN_POINT('Ctrl Pts',(53.9487674206471,23.7943146773157,40.092453830807));
#176180=CARTESIAN_POINT('Ctrl Pts',(53.9367254523687,23.8047436656394,40.1033475319609));
#176181=CARTESIAN_POINT('Ctrl Pts',(53.9249524603721,23.816449033599,40.1130129263075));
#176182=CARTESIAN_POINT('Ctrl Pts',(53.9161227163747,23.8252280595687,40.1202619720674));
#176183=CARTESIAN_POINT('Ctrl Pts',(53.9074442707907,23.8347250487601,40.1268200947266));
#176184=CARTESIAN_POINT('Ctrl Pts',(53.8990234500736,23.84486363178,40.1325796782703));
#176185=CARTESIAN_POINT('Ctrl Pts',(53.8958656423047,23.8486656004125,40.1347395220992));
#176186=CARTESIAN_POINT('Ctrl Pts',(53.8927440632084,23.8525577932536,40.1367870714852));
#176187=CARTESIAN_POINT('Ctrl Pts',(53.8896643205894,23.8565361833374,40.1387166518767));
#176188=CARTESIAN_POINT('Ctrl Pts',(53.8788852214228,23.8704605486305,40.1454701832469));
#176189=CARTESIAN_POINT('Ctrl Pts',(53.8686186144656,23.8854408280733,40.1507785912491));
#176190=CARTESIAN_POINT('Ctrl Pts',(53.8591049768561,23.9013043843655,40.1543986087265));
#176191=CARTESIAN_POINT('Ctrl Pts',(53.8543481580514,23.9092361625115,40.1562086174652));
#176192=CARTESIAN_POINT('Ctrl Pts',(53.8497795825134,23.9173887602865,40.1575965292115));
#176193=CARTESIAN_POINT('Ctrl Pts',(53.8454293138304,23.9257405998154,40.1585319382567));
#176194=CARTESIAN_POINT('Ctrl Pts',(53.843254179489,23.9299165195798,40.1589996427793));
#176195=CARTESIAN_POINT('Ctrl Pts',(53.8411336218844,23.9341422497935,40.159354221642));
#176196=CARTESIAN_POINT('Ctrl Pts',(53.8390713992307,23.9384150933421,40.159591874311));
#176197=CARTESIAN_POINT('Ctrl Pts',(53.8370091765769,23.9426879368908,40.1598295269801));
#176198=CARTESIAN_POINT('Ctrl Pts',(53.8350052904266,23.9470078944653,40.1599502506895));
#176199=CARTESIAN_POINT('Ctrl Pts',(53.8330634946841,23.9513722670358,40.1599502534424));
#176200=CARTESIAN_POINT('',(53.8206887816839,23.9791663275007,40.1599502534424));
#176201=CARTESIAN_POINT('Origin',(5.71744365443249E-15,5.28042056574211E-15,
40.1599502534424));
#176202=CARTESIAN_POINT('',(53.8697418420148,24.3312692531081,39.8576902534424));
#176203=CARTESIAN_POINT('Ctrl Pts',(53.8206887816839,23.9791663275007,40.1599502534424));
#176204=CARTESIAN_POINT('Ctrl Pts',(53.8191382997274,23.9826463618218,40.1599502448875));
#176205=CARTESIAN_POINT('Ctrl Pts',(53.8176349962322,23.986136019079,40.1598743450437));
#176206=CARTESIAN_POINT('Ctrl Pts',(53.8161786595152,23.9896330908635,40.1597243308499));
#176207=CARTESIAN_POINT('Ctrl Pts',(53.8075805576712,24.010279538219,40.1588386583939));
#176208=CARTESIAN_POINT('Ctrl Pts',(53.8006169491721,24.0311861904735,40.1553722553621));
#176209=CARTESIAN_POINT('Ctrl Pts',(53.7952474622087,24.0518926318757,40.1496902177796));
#176210=CARTESIAN_POINT('Ctrl Pts',(53.7932416006211,24.0596278690982,40.147567597685));
#176211=CARTESIAN_POINT('Ctrl Pts',(53.7914578533671,24.06733539392,40.1451361443099));
#176212=CARTESIAN_POINT('Ctrl Pts',(53.7898929820051,24.0749921329672,40.1424159447501));
#176213=CARTESIAN_POINT('Ctrl Pts',(53.7886719908667,24.0809663048716,40.1402935085949));
#176214=CARTESIAN_POINT('Ctrl Pts',(53.7875846446509,24.0869092410382,40.1379949176048));
#176215=CARTESIAN_POINT('Ctrl Pts',(53.7866297945202,24.0928096561858,40.1355293609261));
#176216=CARTESIAN_POINT('Ctrl Pts',(53.7832878190625,24.1134611092021,40.1268999125508));
#176217=CARTESIAN_POINT('Ctrl Pts',(53.7815689125025,24.1335916760296,40.1162251288835));
#176218=CARTESIAN_POINT('Ctrl Pts',(53.7814239018617,24.1527175379838,40.1038990521418));
#176219=CARTESIAN_POINT('Ctrl Pts',(53.7813513965413,24.1622804689609,40.0977360137709));
#176220=CARTESIAN_POINT('Ctrl Pts',(53.7816723668481,24.1715922244704,40.0911601532641));
#176221=CARTESIAN_POINT('Ctrl Pts',(53.7823806708184,24.1805923292961,40.084220729064));
#176222=CARTESIAN_POINT('Ctrl Pts',(53.7830859485795,24.1895539814229,40.0773109533618));
#176223=CARTESIAN_POINT('Ctrl Pts',(53.7841750295933,24.1982067474358,40.0700409753048));
#176224=CARTESIAN_POINT('Ctrl Pts',(53.7856425347027,24.2064906018692,40.0624586415899));
#176225=CARTESIAN_POINT('Ctrl Pts',(53.7856488314805,24.2065261462705,40.0624261072769));
#176226=CARTESIAN_POINT('Ctrl Pts',(53.7856551347357,24.2065616841176,40.0623935677888));
#176227=CARTESIAN_POINT('Ctrl Pts',(53.7856614444667,24.2065972154092,40.0623610231288));
#176228=CARTESIAN_POINT('Ctrl Pts',(53.7886369923277,24.2233530895755,40.0470135870225));
#176229=CARTESIAN_POINT('Ctrl Pts',(53.7930196670713,24.2386338146195,40.0305755292075));
#176230=CARTESIAN_POINT('Ctrl Pts',(53.7986158348088,24.2524209582933,40.013344756731));
#176231=CARTESIAN_POINT('Ctrl Pts',(53.8044155801174,24.2667096511258,39.9954871626558));
#176232=CARTESIAN_POINT('Ctrl Pts',(53.8115193533103,24.279394708371,39.9767767954267));
#176233=CARTESIAN_POINT('Ctrl Pts',(53.8197464933903,24.2904167802974,39.9575197577417));
#176234=CARTESIAN_POINT('Ctrl Pts',(53.8278562137214,24.3012815425261,39.9385375611934));
#176235=CARTESIAN_POINT('Ctrl Pts',(53.837058338548,24.3105307527896,39.9190226977027));
#176236=CARTESIAN_POINT('Ctrl Pts',(53.8472012967816,24.3180642992234,39.8992655451783));
#176237=CARTESIAN_POINT('Ctrl Pts',(53.8542731477211,24.3233168218307,39.8854905069277));
#176238=CARTESIAN_POINT('Ctrl Pts',(53.8618028047985,24.32773445765,39.871597605145));
#176239=CARTESIAN_POINT('Ctrl Pts',(53.8697418420148,24.3312692531081,39.8576902534424));
#176240=CARTESIAN_POINT('',(54.1952354911875,24.4761921430385,39.2875012672119));
#176241=CARTESIAN_POINT('',(53.8697418420148,24.3312692531081,39.8576902534424));
#176242=CARTESIAN_POINT('',(51.6568155675431,29.4581217525667,39.2875012672119));
#176243=CARTESIAN_POINT('Origin',(5.53234440788222E-15,0.,39.2875012672119));
#176244=CARTESIAN_POINT('',(51.3482501200169,29.2799753962456,39.8576902534424));
#176245=CARTESIAN_POINT('',(51.6568155675431,29.4581217525667,39.2875012672119));
#176246=CARTESIAN_POINT('',(51.0345602039891,29.4472515437729,40.1599502534424));
#176247=CARTESIAN_POINT('Ctrl Pts',(51.3482501200169,29.2799753962456,39.8576902534424));
#176248=CARTESIAN_POINT('Ctrl Pts',(51.3376585930516,29.2738605406101,39.8772619994048));
#176249=CARTESIAN_POINT('Ctrl Pts',(51.3261534914777,29.2694377663934,39.8967644650358));
#176250=CARTESIAN_POINT('Ctrl Pts',(51.3139160033709,29.2667250421034,39.915928283603));
#176251=CARTESIAN_POINT('Ctrl Pts',(51.3014574615395,29.2639633161063,39.9354382707168));
#176252=CARTESIAN_POINT('Ctrl Pts',(51.2882390496569,29.2629734853266,39.9545987622334));
#176253=CARTESIAN_POINT('Ctrl Pts',(51.2744188030431,29.2638161685321,39.9731387498209));
#176254=CARTESIAN_POINT('Ctrl Pts',(51.2611836698386,29.2646231747156,39.9908938024034));
#176255=CARTESIAN_POINT('Ctrl Pts',(51.2473957191187,29.267110757666,40.0080810366162));
#176256=CARTESIAN_POINT('Ctrl Pts',(51.2331761176627,29.2713733056818,40.0244542742521));
#176257=CARTESIAN_POINT('Ctrl Pts',(51.2218663142644,29.2747635962031,40.0374770090473));
#176258=CARTESIAN_POINT('Ctrl Pts',(51.2102829897278,29.2792774508353,40.0499848770032));
#176259=CARTESIAN_POINT('Ctrl Pts',(51.1984837018595,29.2849828273423,40.0618424270193));
#176260=CARTESIAN_POINT('Ctrl Pts',(51.1984514936364,29.2849984011669,40.0618747942791));
#176261=CARTESIAN_POINT('Ctrl Pts',(51.1984192839706,29.2850139839319,40.0619071564124));
#176262=CARTESIAN_POINT('Ctrl Pts',(51.1983870728642,29.2850295756379,40.0619395134161));
#176263=CARTESIAN_POINT('Ctrl Pts',(51.1919748636256,29.288133389582,40.0683807661799));
#176264=CARTESIAN_POINT('Ctrl Pts',(51.1854935419305,29.2916260110601,40.0746073439084));
#176265=CARTESIAN_POINT('Ctrl Pts',(51.1789779411681,29.2954867606373,40.0805869293669));
#176266=CARTESIAN_POINT('Ctrl Pts',(51.1660472802373,29.3031486855374,40.092453830807));
#176267=CARTESIAN_POINT('Ctrl Pts',(51.1529811529982,29.312261814333,40.1033475319609));
#176268=CARTESIAN_POINT('Ctrl Pts',(51.1400491105588,29.3226724463007,40.1130129263075));
#176269=CARTESIAN_POINT('Ctrl Pts',(51.1303500787293,29.3304804202765,40.1202619720674));
#176270=CARTESIAN_POINT('Ctrl Pts',(51.1207264688924,29.339018239387,40.1268200947266));
#176271=CARTESIAN_POINT('Ctrl Pts',(51.1112920078095,29.3482210667393,40.1325796782703));
#176272=CARTESIAN_POINT('Ctrl Pts',(51.1077540849034,29.3516721269964,40.1347395220992));
#176273=CARTESIAN_POINT('Ctrl Pts',(51.1042427612076,29.355216704132,40.1367870714852));
#176274=CARTESIAN_POINT('Ctrl Pts',(51.1007640347392,29.3588513794154,40.1387166518767));
#176275=CARTESIAN_POINT('Ctrl Pts',(51.0885884920996,29.3715727429072,40.1454701832469));
#176276=CARTESIAN_POINT('Ctrl Pts',(51.0768122611,29.3853978061636,40.1507785912491));
#176277=CARTESIAN_POINT('Ctrl Pts',(51.0656925470316,29.4001800143151,40.1543986087265));
#176278=CARTESIAN_POINT('Ctrl Pts',(51.0601326899974,29.4075711183909,40.1562086174652));
#176279=CARTESIAN_POINT('Ctrl Pts',(51.0547369630771,29.4152015092019,40.1575965292115));
#176280=CARTESIAN_POINT('Ctrl Pts',(51.0495375206698,29.4230528695798,40.1585319382567));
#176281=CARTESIAN_POINT('Ctrl Pts',(51.0469377994662,29.4269785497687,40.1589996427792));
#176282=CARTESIAN_POINT('Ctrl Pts',(51.0443871494127,29.4309594723624,40.159354221642));
#176283=CARTESIAN_POINT('Ctrl Pts',(51.0418895900604,29.4349933478621,40.159591874311));
#176284=CARTESIAN_POINT('Ctrl Pts',(51.0393920307082,29.4390272233619,40.1598295269801));
#176285=CARTESIAN_POINT('Ctrl Pts',(51.0369475635293,29.4431140526169,40.1599502506895));
#176286=CARTESIAN_POINT('Ctrl Pts',(51.0345602039891,29.4472515437729,40.1599502534424));
#176287=CARTESIAN_POINT('',(51.0193480105331,29.4735998357331,40.1599502534424));
#176288=CARTESIAN_POINT('Origin',(5.71420591410065E-15,5.28677498893149E-15,
40.1599502534424));
#176289=CARTESIAN_POINT('',(51.0313275753413,29.8289013456879,39.8576902534424));
#176290=CARTESIAN_POINT('Ctrl Pts',(51.0193480105331,29.4735998357331,40.1599502534424));
#176291=CARTESIAN_POINT('Ctrl Pts',(51.0174422596394,29.4768987365659,40.1599502448875));
#176292=CARTESIAN_POINT('Ctrl Pts',(51.0155824228875,29.4802121391113,40.1598743450437));
#176293=CARTESIAN_POINT('Ctrl Pts',(51.0137685205959,29.4835378249316,40.1597243308499));
#176294=CARTESIAN_POINT('Ctrl Pts',(51.0030593786379,29.5031724225183,40.1588386583937));
#176295=CARTESIAN_POINT('Ctrl Pts',(50.9939485772815,29.5232366506519,40.1553722553611));
#176296=CARTESIAN_POINT('Ctrl Pts',(50.9864440924293,29.5432683957836,40.1496902177772));
#176297=CARTESIAN_POINT('Ctrl Pts',(50.9836406667027,29.5507515889351,40.1475675976832));
#176298=CARTESIAN_POINT('Ctrl Pts',(50.9810610352787,29.5582304387673,40.1451361443089));
#176299=CARTESIAN_POINT('Ctrl Pts',(50.9787043892804,29.5656816597952,40.1424159447501));
#176300=CARTESIAN_POINT('Ctrl Pts',(50.9768656158508,29.5714954762335,40.1402935085949));
#176301=CARTESIAN_POINT('Ctrl Pts',(50.9751630202465,29.5772921977451,40.1379949176048));
#176302=CARTESIAN_POINT('Ctrl Pts',(50.9735966395567,29.5830604807842,40.1355293609261));
#176303=CARTESIAN_POINT('Ctrl Pts',(50.9681143071422,29.6032494714213,40.1268999125509));
#176304=CARTESIAN_POINT('Ctrl Pts',(50.964300599717,29.6230900862361,40.1162251288835));
#176305=CARTESIAN_POINT('Ctrl Pts',(50.9621571865009,29.642096016978,40.1038990521418));
#176306=CARTESIAN_POINT('Ctrl Pts',(50.9610854798929,29.6515989823489,40.0977360137709));
#176307=CARTESIAN_POINT('Ctrl Pts',(50.960431348397,29.6608932776203,40.0911601532641));
#176308=CARTESIAN_POINT('Ctrl Pts',(50.9601950050774,29.6699181168556,40.084220729064));
#176309=CARTESIAN_POINT('Ctrl Pts',(50.959959671528,29.678904397715,40.0773109533618));
#176310=CARTESIAN_POINT('Ctrl Pts',(50.9601383261077,29.6876236029351,40.0700409753048));
#176311=CARTESIAN_POINT('Ctrl Pts',(50.9607318934967,29.696015473601,40.0624586415899));
#176312=CARTESIAN_POINT('Ctrl Pts',(50.9607344403784,29.6960514814789,40.0624261072769));
#176313=CARTESIAN_POINT('Ctrl Pts',(50.9607369943872,29.6960874835155,40.0623935677888));
#176314=CARTESIAN_POINT('Ctrl Pts',(50.9607395555215,29.6961234797095,40.0623610231288));
#176315=CARTESIAN_POINT('Ctrl Pts',(50.9619473372426,29.7130985928882,40.0470135870233));
#176316=CARTESIAN_POINT('Ctrl Pts',(50.9647087325287,29.7287537227769,40.0305755292093));
#176317=CARTESIAN_POINT('Ctrl Pts',(50.9688330949324,29.7430502978482,40.0133447567338));
#176318=CARTESIAN_POINT('Ctrl Pts',(50.9731074935251,29.7578669541901,39.9954871626596));
#176319=CARTESIAN_POINT('Ctrl Pts',(50.9788464019642,29.7712250678592,39.9767767954316));
#176320=CARTESIAN_POINT('Ctrl Pts',(50.9858763526689,29.7830467300316,39.9575197577479));
#176321=CARTESIAN_POINT('Ctrl Pts',(50.9928059702033,29.7946996705595,39.9385375612006));
#176322=CARTESIAN_POINT('Ctrl Pts',(51.0009908790913,29.8048600966483,39.919022697711));
#176323=CARTESIAN_POINT('Ctrl Pts',(51.0102908031059,29.8134126013637,39.8992655451877));
#176324=CARTESIAN_POINT('Ctrl Pts',(51.0167748755908,29.8193755598154,39.885490506934));
#176325=CARTESIAN_POINT('Ctrl Pts',(51.023801515737,29.8245560588481,39.8715976051482));
#176326=CARTESIAN_POINT('Ctrl Pts',(51.0313275753413,29.8289013456879,39.8576902534424));
#176327=CARTESIAN_POINT('',(51.3398895692701,30.0070536838151,39.2875012672119));
#176328=CARTESIAN_POINT('',(51.0313275753413,29.8289013456879,39.8576902534424));
#176329=CARTESIAN_POINT('',(48.2946219293751,34.6963546279279,39.2875012672119));
#176330=CARTESIAN_POINT('Origin',(5.53234440788222E-15,0.,39.2875012672119));
#176331=CARTESIAN_POINT('',(48.0063682005191,34.4869303039391,39.8576902534424));
#176332=CARTESIAN_POINT('',(48.2946219293751,34.6963546279279,39.2875012672119));
#176333=CARTESIAN_POINT('',(47.6769115920308,34.6205005703629,40.1599502534424));
#176334=CARTESIAN_POINT('Ctrl Pts',(48.0063682005191,34.4869303039391,39.8576902534424));
#176335=CARTESIAN_POINT('Ctrl Pts',(47.9964738715094,34.4797418300848,39.8772619994052));
#176336=CARTESIAN_POINT('Ctrl Pts',(47.9854941018778,34.4741406737006,39.8967644650366));
#176337=CARTESIAN_POINT('Ctrl Pts',(47.9736072089122,34.470163644172,39.9159282836043));
#176338=CARTESIAN_POINT('Ctrl Pts',(47.9615055952506,34.4661147749665,39.9354382707186));
#176339=CARTESIAN_POINT('Ctrl Pts',(47.9484630607011,34.4637486663026,39.954598762236));
#176340=CARTESIAN_POINT('Ctrl Pts',(47.9346304384632,34.4631421240611,39.973138749824));
#176341=CARTESIAN_POINT('Ctrl Pts',(47.9213834535862,34.4625612612454,39.9908938024074));
#176342=CARTESIAN_POINT('Ctrl Pts',(47.907411011479,34.4635939836562,40.008081036621));
#176343=CARTESIAN_POINT('Ctrl Pts',(47.8928237488929,34.4663468279001,40.0244542742576));
#176344=CARTESIAN_POINT('Ctrl Pts',(47.8812215199242,34.4685363496862,40.0374770090508));
#176345=CARTESIAN_POINT('Ctrl Pts',(47.8692298237649,34.4718146898368,40.0499848770049));
#176346=CARTESIAN_POINT('Ctrl Pts',(47.8568987993932,34.4762554502652,40.0618424270193));
#176347=CARTESIAN_POINT('Ctrl Pts',(47.8568651397022,34.4762675720986,40.0618747942791));
#176348=CARTESIAN_POINT('Ctrl Pts',(47.8568314776419,34.4762797026728,40.0619071564124));
#176349=CARTESIAN_POINT('Ctrl Pts',(47.8567978132142,34.4762918419884,40.0619395134162));
#176350=CARTESIAN_POINT('Ctrl Pts',(47.8500962938269,34.4787083945371,40.0683807661799));
#176351=CARTESIAN_POINT('Ctrl Pts',(47.8432853991343,34.4815044004726,40.0746073439084));
#176352=CARTESIAN_POINT('Ctrl Pts',(47.8364019332942,34.4846629347246,40.0805869293669));
#176353=CARTESIAN_POINT('Ctrl Pts',(47.8227412186415,34.4909312646823,40.092453830807));
#176354=CARTESIAN_POINT('Ctrl Pts',(47.808794087666,34.4986286886037,40.1033475319609));
#176355=CARTESIAN_POINT('Ctrl Pts',(47.7948446809469,34.5076305235171,40.1130129263075));
#176356=CARTESIAN_POINT('Ctrl Pts',(47.7843826259076,34.5143818997022,40.1202619720674));
#176357=CARTESIAN_POINT('Ctrl Pts',(47.7739192901011,34.5218670065989,40.1268200947266));
#176358=CARTESIAN_POINT('Ctrl Pts',(47.7635745545823,34.5300332501813,40.1325796782703));
#176359=CARTESIAN_POINT('Ctrl Pts',(47.7596952787628,34.5330955915247,40.1347395220992));
#176360=CARTESIAN_POINT('Ctrl Pts',(47.7558326812647,34.5362537178259,40.1367870714852));
#176361=CARTESIAN_POINT('Ctrl Pts',(47.751993084602,34.5395048560459,40.1387166518767));
#176362=CARTESIAN_POINT('Ctrl Pts',(47.7385544962824,34.5508838398159,40.1454701832469));
#176363=CARTESIAN_POINT('Ctrl Pts',(47.7253976640916,34.5634022165997,40.1507785912491));
#176364=CARTESIAN_POINT('Ctrl Pts',(47.7127937034786,34.5769411196448,40.1543986087265));
#176365=CARTESIAN_POINT('Ctrl Pts',(47.7064917231721,34.5837105711674,40.1562086174652));
#176366=CARTESIAN_POINT('Ctrl Pts',(47.7003279615829,34.590735154856,40.1575965292115));
#176367=CARTESIAN_POINT('Ctrl Pts',(47.6943363116302,34.5980000149355,40.1585319382567));
#176368=CARTESIAN_POINT('Ctrl Pts',(47.6913404866539,34.6016324449753,40.1589996427793));
#176369=CARTESIAN_POINT('Ctrl Pts',(47.6883876896072,34.605324944128,40.159354221642));
#176370=CARTESIAN_POINT('Ctrl Pts',(47.6854821573394,34.6090756555947,40.159591874311));
#176371=CARTESIAN_POINT('Ctrl Pts',(47.6825766250716,34.6128263670613,40.1598295269801));
#176372=CARTESIAN_POINT('Ctrl Pts',(47.679718358958,34.6166352918404,40.1599502506895));
#176373=CARTESIAN_POINT('Ctrl Pts',(47.6769115920308,34.6205005703629,40.1599502534424));
#176374=CARTESIAN_POINT('',(47.659028586094,34.645114416418,40.1599502534424));
#176375=CARTESIAN_POINT('Origin',(5.71032169235817E-15,5.29275616590442E-15,
40.1599502534424));
#176376=CARTESIAN_POINT('',(47.6338034047604,34.9997217530255,39.8576902534424));
#176377=CARTESIAN_POINT('Ctrl Pts',(47.659028586094,34.645114416418,40.1599502534424));
#176378=CARTESIAN_POINT('Ctrl Pts',(47.6567884460685,34.6481960403145,40.1599502448875));
#176379=CARTESIAN_POINT('Ctrl Pts',(47.6545924528207,34.6512968858165,40.1598743450437));
#176380=CARTESIAN_POINT('Ctrl Pts',(47.6524408584475,34.6544147487629,40.1597243308499));
#176381=CARTESIAN_POINT('Ctrl Pts',(47.6397380079776,34.6728223758169,40.1588386583938));
#176382=CARTESIAN_POINT('Ctrl Pts',(47.6285798336113,34.6918243519436,40.1553722553614));
#176383=CARTESIAN_POINT('Ctrl Pts',(47.6190225715775,34.7109619288094,40.149690217778));
#176384=CARTESIAN_POINT('Ctrl Pts',(47.6154522966294,34.7181110904637,40.1475675976838));
#176385=CARTESIAN_POINT('Ctrl Pts',(47.6121050440158,34.7252793254663,40.1451361443092));
#176386=CARTESIAN_POINT('Ctrl Pts',(47.608982443287,34.732443391342,40.1424159447501));
#176387=CARTESIAN_POINT('Ctrl Pts',(47.6065460335526,34.7380331549247,40.1402935085949));
#176388=CARTESIAN_POINT('Ctrl Pts',(47.6042468425536,34.7436201516872,40.1379949176048));
#176389=CARTESIAN_POINT('Ctrl Pts',(47.6020860928993,34.7491931041019,40.1355293609261));
#176390=CARTESIAN_POINT('Ctrl Pts',(47.5945234691092,34.7686984375535,40.1268999125509));
#176391=CARTESIAN_POINT('Ctrl Pts',(47.5886567445954,34.7880317224279,40.1162251288835));
#176392=CARTESIAN_POINT('Ctrl Pts',(47.5845384124878,34.8067094890029,40.1038990521418));
#176393=CARTESIAN_POINT('Ctrl Pts',(47.582479246434,34.8160483722904,40.097736013771));
#176394=CARTESIAN_POINT('Ctrl Pts',(47.580857179937,34.8252233770798,40.0911601532641));
#176395=CARTESIAN_POINT('Ctrl Pts',(47.5796787787543,34.8341740726974,40.084220729064));
#176396=CARTESIAN_POINT('Ctrl Pts',(47.578505412258,34.8430865267157,40.0773109533619));
#176397=CARTESIAN_POINT('Ctrl Pts',(47.5777716830267,34.851776641706,40.0700409753047));
#176398=CARTESIAN_POINT('Ctrl Pts',(47.5774848094468,34.8601845855133,40.0624586415899));
#176399=CARTESIAN_POINT('Ctrl Pts',(47.5774835785283,34.860220662358,40.0624261072769));
#176400=CARTESIAN_POINT('Ctrl Pts',(47.5774823553084,34.8602567341383,40.0623935677888));
#176401=CARTESIAN_POINT('Ctrl Pts',(47.5774811397857,34.8602928008528,40.0623610231288));
#176402=CARTESIAN_POINT('Ctrl Pts',(47.5769079226579,34.8773011701495,40.0470135870261));
#176403=CARTESIAN_POINT('Ctrl Pts',(47.5780177840617,34.8931591840015,40.0305755292153));
#176404=CARTESIAN_POINT('Ctrl Pts',(47.5806251537534,34.9078085542004,40.0133447567433));
#176405=CARTESIAN_POINT('Ctrl Pts',(47.5833273744242,34.9229908396626,39.9954871626726));
#176406=CARTESIAN_POINT('Ctrl Pts',(47.587638541427,34.9368756554655,39.9767767954483));
#176407=CARTESIAN_POINT('Ctrl Pts',(47.593394281144,34.9493673872784,39.9575197577683));
#176408=CARTESIAN_POINT('Ctrl Pts',(47.5990678735408,34.96168083405,39.938537561224));
#176409=CARTESIAN_POINT('Ctrl Pts',(47.6061458909142,34.9726411562093,39.9190226977374));
#176410=CARTESIAN_POINT('Ctrl Pts',(47.6145008887944,34.982118916175,39.8992655452171));
#176411=CARTESIAN_POINT('Ctrl Pts',(47.6203261419715,34.9887269790548,39.8854905069538));
#176412=CARTESIAN_POINT('Ctrl Pts',(47.626772779849,34.9946135826729,39.8715976051581));
#176413=CARTESIAN_POINT('Ctrl Pts',(47.6338034047604,34.9997217530255,39.8576902534424));
#176414=CARTESIAN_POINT('',(47.9220530736691,35.2091516650522,39.2875012672119));
#176415=CARTESIAN_POINT('',(47.6338034047604,34.9997217530255,39.8576902534424));
#176416=CARTESIAN_POINT('',(44.4033023070494,39.5544469813066,39.2875012672119));
#176417=CARTESIAN_POINT('Origin',(5.53234440788222E-15,0.,39.2875012672119));
#176418=CARTESIAN_POINT('',(44.1385184650381,39.3160391863685,39.8576902534424));
#176419=CARTESIAN_POINT('',(44.4033023070494,39.5544469813066,39.2875012672119));
#176420=CARTESIAN_POINT('',(43.7969047596351,39.4144401478985,40.1599502534424));
#176421=CARTESIAN_POINT('Ctrl Pts',(44.1385184650381,39.3160391863685,39.8576902534424));
#176422=CARTESIAN_POINT('Ctrl Pts',(44.1294297383225,39.3078558527197,39.877261999406));
#176423=CARTESIAN_POINT('Ctrl Pts',(44.1190955972865,39.3011376816095,39.8967644650382));
#176424=CARTESIAN_POINT('Ctrl Pts',(44.1076895347488,39.29593992001,39.9159282836065));
#176425=CARTESIAN_POINT('Ctrl Pts',(44.0960774370686,39.2906482678547,39.9354382707213));
#176426=CARTESIAN_POINT('Ctrl Pts',(44.0833536765903,39.286931804888,39.954598762239));
#176427=CARTESIAN_POINT('Ctrl Pts',(44.0696602318325,39.2848826826029,39.9731387498273));
#176428=CARTESIAN_POINT('Ctrl Pts',(44.0565465320223,39.2829203148425,39.9908938024105));
#176429=CARTESIAN_POINT('Ctrl Pts',(44.0425426835285,39.2824868619904,40.0080810366238));
#176430=CARTESIAN_POINT('Ctrl Pts',(44.0277475809149,39.2836998417242,40.0244542742601));
#176431=CARTESIAN_POINT('Ctrl Pts',(44.0159800428236,39.2846646059163,40.0374770090524));
#176432=CARTESIAN_POINT('Ctrl Pts',(44.0037113585733,39.2866715134049,40.0499848770057));
#176433=CARTESIAN_POINT('Ctrl Pts',(43.9909836989809,39.2897990038547,40.0618424270193));
#176434=CARTESIAN_POINT('Ctrl Pts',(43.9909489566045,39.2898075408878,40.0618747942791));
#176435=CARTESIAN_POINT('Ctrl Pts',(43.9909142109582,39.2898160863659,40.0619071564124));
#176436=CARTESIAN_POINT('Ctrl Pts',(43.9908794620438,39.2898246402901,40.0619395134161));
#176437=CARTESIAN_POINT('Ctrl Pts',(43.9839620557566,39.291527455188,40.0683807661799));
#176438=CARTESIAN_POINT('Ctrl Pts',(43.976896209654,39.2935962119547,40.0746073439084));
#176439=CARTESIAN_POINT('Ctrl Pts',(43.9697202954285,39.2960179253194,40.0805869293669));
#176440=CARTESIAN_POINT('Ctrl Pts',(43.9554791967022,39.3008239832,40.092453830807));
#176441=CARTESIAN_POINT('Ctrl Pts',(43.9408038696759,39.3070213676599,40.1033475319609));
#176442=CARTESIAN_POINT('Ctrl Pts',(43.9259899312964,39.3145157795319,40.1130129263075));
#176443=CARTESIAN_POINT('Ctrl Pts',(43.9148794775117,39.3201365884359,40.1202619720674));
#176444=CARTESIAN_POINT('Ctrl Pts',(43.9036910542322,39.3264869747214,40.1268200947266));
#176445=CARTESIAN_POINT('Ctrl Pts',(43.8925493833646,39.3335271634603,40.1325796782703));
#176446=CARTESIAN_POINT('Ctrl Pts',(43.8883712567893,39.3361672342374,40.1347395220992));
#176447=CARTESIAN_POINT('Ctrl Pts',(43.8841997049153,39.3389043086116,40.1367870714852));
#176448=CARTESIAN_POINT('Ctrl Pts',(43.8800413054829,39.3417362896176,40.1387166518767));
#176449=CARTESIAN_POINT('Ctrl Pts',(43.8654869074692,39.3516482231383,40.1454701832469));
#176450=CARTESIAN_POINT('Ctrl Pts',(43.851093623094,39.362722759494,40.1507785912492));
#176451=CARTESIAN_POINT('Ctrl Pts',(43.8371435075663,39.3748700223776,40.1543986087265));
#176452=CARTESIAN_POINT('Ctrl Pts',(43.8301684498025,39.3809436538194,40.1562086174652));
#176453=CARTESIAN_POINT('Ctrl Pts',(43.8233041850061,39.3872854675767,40.1575965292115));
#176454=CARTESIAN_POINT('Ctrl Pts',(43.8165859732789,39.3938842320306,40.1585319382567));
#176455=CARTESIAN_POINT('Ctrl Pts',(43.8132268674153,39.3971836142575,40.1589996427793));
#176456=CARTESIAN_POINT('Ctrl Pts',(43.8099042748376,39.4005472341759,40.159354221642));
#176457=CARTESIAN_POINT('Ctrl Pts',(43.8066226032738,39.4039736880298,40.159591874311));
#176458=CARTESIAN_POINT('Ctrl Pts',(43.8033409317101,39.4074001418836,40.1598295269801));
#176459=CARTESIAN_POINT('Ctrl Pts',(43.8001001824235,39.4108894308098,40.1599502506895));
#176460=CARTESIAN_POINT('Ctrl Pts',(43.7969047596351,39.4144401478985,40.1599502534424));
#176461=CARTESIAN_POINT('',(43.7765468711727,39.4370498736003,40.1599502534424));
#176462=CARTESIAN_POINT('Origin',(5.7058335455513E-15,5.29829856563434E-15,
40.1599502534424));
#176463=CARTESIAN_POINT('',(43.7143933160628,39.7870778846742,39.8576902534424));
#176464=CARTESIAN_POINT('Ctrl Pts',(43.7765468711727,39.4370498736003,40.1599502534424));
#176465=CARTESIAN_POINT('Ctrl Pts',(43.7739968854584,39.4398804576443,40.1599502448875));
#176466=CARTESIAN_POINT('Ctrl Pts',(43.7714887954763,39.4427347725906,40.1598743450437));
#176467=CARTESIAN_POINT('Ctrl Pts',(43.7690230823397,39.4456106527042,40.1597243308499));
#176468=CARTESIAN_POINT('Ctrl Pts',(43.7544656984424,39.4625896314159,40.1588386583936));
#176469=CARTESIAN_POINT('Ctrl Pts',(43.7413824023569,39.4803211659136,40.15537225536));
#176470=CARTESIAN_POINT('Ctrl Pts',(43.7298770745023,39.4983548992213,40.1496902177745));
#176471=CARTESIAN_POINT('Ctrl Pts',(43.7255790670151,39.5050917016626,40.1475675976811));
#176472=CARTESIAN_POINT('Ctrl Pts',(43.7215008664148,39.5118707851483,40.1451361443077));
#176473=CARTESIAN_POINT('Ctrl Pts',(43.7176465228248,39.5186692048623,40.1424159447501));
#176474=CARTESIAN_POINT('Ctrl Pts',(43.7146391706006,39.5239736729698,40.1402935085948));
#176475=CARTESIAN_POINT('Ctrl Pts',(43.7117685746245,39.5292897326775,40.1379949176047));
#176476=CARTESIAN_POINT('Ctrl Pts',(43.7090371296311,39.534606296035,40.1355293609261));
#176477=CARTESIAN_POINT('Ctrl Pts',(43.6994770721542,39.5532142677859,40.1268999125508));
#176478=CARTESIAN_POINT('Ctrl Pts',(43.6916216076134,39.5718284032051,40.1162251288835));
#176479=CARTESIAN_POINT('Ctrl Pts',(43.6855734779227,39.5899733680941,40.1038990521418));
#176480=CARTESIAN_POINT('Ctrl Pts',(43.6825494130773,39.5990458505386,40.0977360137709));
#176481=CARTESIAN_POINT('Ctrl Pts',(43.6799771832791,39.6080010415734,40.0911601532641));
#176482=CARTESIAN_POINT('Ctrl Pts',(43.6778696350433,39.6167795278792,40.084220729064));
#176483=CARTESIAN_POINT('Ctrl Pts',(43.675771091249,39.6255205083452,40.0773109533618));
#176484=CARTESIAN_POINT('Ctrl Pts',(43.6741330170976,39.6340863223872,40.0700409753048));
#176485=CARTESIAN_POINT('Ctrl Pts',(43.6729688455957,39.6424182201442,40.0624586415899));
#176486=CARTESIAN_POINT('Ctrl Pts',(43.6729638503632,39.6424539706901,40.0624261072769));
#176487=CARTESIAN_POINT('Ctrl Pts',(43.6729588633165,39.6424897170041,40.0623935677889));
#176488=CARTESIAN_POINT('Ctrl Pts',(43.6729538844543,39.6425254590847,40.0623610231289));
#176489=CARTESIAN_POINT('Ctrl Pts',(43.6706059487643,39.6593807372514,40.0470135870242));
#176490=CARTESIAN_POINT('Ctrl Pts',(43.670052116413,39.6752678913532,40.0305755292112));
#176491=CARTESIAN_POINT('Ctrl Pts',(43.6711139265065,39.690109555118,40.0133447567368));
#176492=CARTESIAN_POINT('Ctrl Pts',(43.672214363162,39.7054911294078,39.9954871626635));
#176493=CARTESIAN_POINT('Ctrl Pts',(43.6750505546831,39.7197505224001,39.9767767954365));
#176494=CARTESIAN_POINT('Ctrl Pts',(43.6794690223272,39.7327754618278,39.9575197577537));
#176495=CARTESIAN_POINT('Ctrl Pts',(43.6838244285239,39.7456145061448,39.938537561207));
#176496=CARTESIAN_POINT('Ctrl Pts',(43.6897180061469,39.7572546407921,39.919022697718));
#176497=CARTESIAN_POINT('Ctrl Pts',(43.697036538792,39.7675538156862,39.8992655451953));
#176498=CARTESIAN_POINT('Ctrl Pts',(43.7021391499628,39.7747345836643,39.8854905069391));
#176499=CARTESIAN_POINT('Ctrl Pts',(43.7079351548507,39.7812627969986,39.8715976051507));
#176500=CARTESIAN_POINT('Ctrl Pts',(43.7143933160628,39.7870778846742,39.8576902534424));
#176501=CARTESIAN_POINT('',(43.9791725362587,40.0254908126583,39.2875012672119));
#176502=CARTESIAN_POINT('',(43.7143933160628,39.7870778846742,39.8576902534424));
#176503=CARTESIAN_POINT('',(40.0254908126594,43.9791725362578,39.2875012672119));
#176504=CARTESIAN_POINT('Origin',(5.53234440788222E-15,0.,39.2875012672119));
#176505=CARTESIAN_POINT('',(39.7870778846752,43.7143933160618,39.8576902534424));
#176506=CARTESIAN_POINT('',(40.0254908126594,43.9791725362578,39.2875012672119));
#176507=CARTESIAN_POINT('',(39.4370498736014,43.7765468711718,40.1599502534424));
#176508=CARTESIAN_POINT('Ctrl Pts',(39.7870778846752,43.7143933160618,39.8576902534424));
#176509=CARTESIAN_POINT('Ctrl Pts',(39.7788943382462,43.7053047809343,39.8772619994062));
#176510=CARTESIAN_POINT('Ctrl Pts',(39.7693190488181,43.6975432007866,39.8967644650386));
#176511=CARTESIAN_POINT('Ctrl Pts',(39.7585187839167,43.69118165488,39.9159282836071));
#176512=CARTESIAN_POINT('Ctrl Pts',(39.7475234267904,43.684705196223,39.9354382707221));
#176513=CARTESIAN_POINT('Ctrl Pts',(39.7352578445659,43.6796790972996,39.9545987622399));
#176514=CARTESIAN_POINT('Ctrl Pts',(39.7218536055345,43.6762098455834,39.9731387498284));
#176515=CARTESIAN_POINT('Ctrl Pts',(39.7090168672302,43.67288747299,39.9908938024117));
#176516=CARTESIAN_POINT('Ctrl Pts',(39.6951350414442,43.6709925938752,40.008081036625));
#176517=CARTESIAN_POINT('Ctrl Pts',(39.680294197043,43.670652419439,40.0244542742614));
#176518=CARTESIAN_POINT('Ctrl Pts',(39.6684902774386,43.6703818558789,40.0374770090532));
#176519=CARTESIAN_POINT('Ctrl Pts',(39.656079023369,43.6710953426073,40.049984877006));
#176520=CARTESIAN_POINT('Ctrl Pts',(39.6430941754573,43.6728752976389,40.0618424270193));
#176521=CARTESIAN_POINT('Ctrl Pts',(39.6430587310404,43.672880156338,40.0618747942791));
#176522=CARTESIAN_POINT('Ctrl Pts',(39.6430232824887,43.6728850230941,40.0619071564124));
#176523=CARTESIAN_POINT('Ctrl Pts',(39.642987829804,43.6728898979084,40.0619395134161));
#176524=CARTESIAN_POINT('Ctrl Pts',(39.6359303251676,43.6738603187591,40.0683807661799));
#176525=CARTESIAN_POINT('Ctrl Pts',(39.6286869425436,43.675179160625,40.0746073439084));
#176526=CARTESIAN_POINT('Ctrl Pts',(39.6212972007506,43.676837520304,40.0805869293668));
#176527=CARTESIAN_POINT('Ctrl Pts',(39.6066317464086,43.6801286499315,40.092453830807));
#176528=CARTESIAN_POINT('Ctrl Pts',(39.5913890092854,43.6847580950889,40.1033475319609));
#176529=CARTESIAN_POINT('Ctrl Pts',(39.5758728438542,43.6906629735748,40.1130129263075));
#176530=CARTESIAN_POINT('Ctrl Pts',(39.5642357197808,43.6950916324392,40.1202619720674));
#176531=CARTESIAN_POINT('Ctrl Pts',(39.5524447917351,43.7002377219523,40.1268200947266));
#176532=CARTESIAN_POINT('Ctrl Pts',(39.5406282559963,43.7060747220667,40.1325796782703));
#176533=CARTESIAN_POINT('Ctrl Pts',(39.5361970550943,43.7082635971095,40.1347395220992));
#176534=CARTESIAN_POINT('Ctrl Pts',(39.5317622532398,43.7105496315971,40.1367870714852));
#176535=CARTESIAN_POINT('Ctrl Pts',(39.527330611332,43.7129314276125,40.1387166518767));
#176536=CARTESIAN_POINT('Ctrl Pts',(39.5118198646546,43.7212677136662,40.1454701832469));
#176537=CARTESIAN_POINT('Ctrl Pts',(39.4963478239305,43.7307770746558,40.1507785912492));
#176538=CARTESIAN_POINT('Ctrl Pts',(39.4812043938732,43.7413996094238,40.1543986087265));
#176539=CARTESIAN_POINT('Ctrl Pts',(39.4736326788445,43.7467108768079,40.1562086174652));
#176540=CARTESIAN_POINT('Ctrl Pts',(39.4661431171625,43.7523004383952,40.1575965292115));
#176541=CARTESIAN_POINT('Ctrl Pts',(39.4587719497942,43.7581608097792,40.1585319382567));
#176542=CARTESIAN_POINT('Ctrl Pts',(39.4550863661101,43.7610909954712,40.1589996427793));
#176543=CARTESIAN_POINT('Ctrl Pts',(39.4514303810211,43.7640888836316,40.159354221642));
#176544=CARTESIAN_POINT('Ctrl Pts',(39.4478085248418,43.7671535389272,40.159591874311));
#176545=CARTESIAN_POINT('Ctrl Pts',(39.4441866686624,43.7702181942228,40.1598295269801));
#176546=CARTESIAN_POINT('Ctrl Pts',(39.4405989425301,43.7733496179164,40.1599502506895));
#176547=CARTESIAN_POINT('Ctrl Pts',(39.4370498736014,43.7765468711718,40.1599502534424));
#176548=CARTESIAN_POINT('',(39.4144401478995,43.7969047596342,40.1599502534424));
#176549=CARTESIAN_POINT('Origin',(5.70079064675565E-15,5.30334146442998E-15,
40.1599502534424));
#176550=CARTESIAN_POINT('',(39.3160391863695,44.1385184650371,39.8576902534424));
#176551=CARTESIAN_POINT('Ctrl Pts',(39.4144401478995,43.7969047596342,40.1599502534424));
#176552=CARTESIAN_POINT('Ctrl Pts',(39.4116082546735,43.7994532913546,40.1599502448875));
#176553=CARTESIAN_POINT('Ctrl Pts',(39.4088155471156,43.8020298032734,40.1598743450437));
#176554=CARTESIAN_POINT('Ctrl Pts',(39.4060627300848,43.8046321918097,40.1597243308499));
#176555=CARTESIAN_POINT('Ctrl Pts',(39.3898103065136,43.8199964969255,40.1588386583939));
#176556=CARTESIAN_POINT('Ctrl Pts',(39.3749452320458,43.8362633193808,40.1553722553627));
#176557=CARTESIAN_POINT('Ctrl Pts',(39.3616178931555,43.8529956277635,40.1496902177812));
#176558=CARTESIAN_POINT('Ctrl Pts',(39.3566392429908,43.8592462611849,40.1475675976862));
#176559=CARTESIAN_POINT('Ctrl Pts',(39.3518747760156,43.865561920107,40.1451361443106));
#176560=CARTESIAN_POINT('Ctrl Pts',(39.347330918553,43.8719202087608,40.1424159447501));
#176561=CARTESIAN_POINT('Ctrl Pts',(39.3437855730191,43.8768812645304,40.1402935085949));
#176562=CARTESIAN_POINT('Ctrl Pts',(39.3403750229164,43.8818681433209,40.1379949176048));
#176563=CARTESIAN_POINT('Ctrl Pts',(39.3371028088668,43.8868700682403,40.1355293609261));
#176564=CARTESIAN_POINT('Ctrl Pts',(39.3256500596934,43.9043768054582,40.1268999125508));
#176565=CARTESIAN_POINT('Ctrl Pts',(39.3158919212388,43.9220678510592,40.1162251288835));
#176566=CARTESIAN_POINT('Ctrl Pts',(39.3079802585394,43.9394812142298,40.1038990521418));
#176567=CARTESIAN_POINT('Ctrl Pts',(39.3040244271897,43.948187895815,40.0977360137709));
#176568=CARTESIAN_POINT('Ctrl Pts',(39.3005302159784,43.9568251581485,40.0911601532641));
#176569=CARTESIAN_POINT('Ctrl Pts',(39.297516611429,43.9653352562094,40.084220729064));
#176570=CARTESIAN_POINT('Ctrl Pts',(39.2945158824216,43.9738089951119,40.0773109533619));
#176571=CARTESIAN_POINT('Ctrl Pts',(39.2919914104334,43.9821566593546,40.0700409753047));
#176572=CARTESIAN_POINT('Ctrl Pts',(39.2899626959162,43.9903212250458,40.0624586415899));
#176573=CARTESIAN_POINT('Ctrl Pts',(39.2899539910984,43.9903562576025,40.0624261072769));
#176574=CARTESIAN_POINT('Ctrl Pts',(39.289945294864,43.9903912868061,40.0623935677888));
#176575=CARTESIAN_POINT('Ctrl Pts',(39.2899366072118,43.990426312655,40.0623610231288));
#176576=CARTESIAN_POINT('Ctrl Pts',(39.2858396774346,44.0069438297345,40.0470135870245));
#176577=CARTESIAN_POINT('Ctrl Pts',(39.2836282192308,44.0226860610988,40.0305755292119));
#176578=CARTESIAN_POINT('Ctrl Pts',(39.2831328363119,44.0375574100537,40.013344756738));
#176579=CARTESIAN_POINT('Ctrl Pts',(39.282619432337,44.0529697494221,39.9954871626652));
#176580=CARTESIAN_POINT('Ctrl Pts',(39.2839495744675,44.0674474907085,39.9767767954388));
#176581=CARTESIAN_POINT('Ctrl Pts',(39.2869823603807,44.0808629337877,39.9575197577567));
#176582=CARTESIAN_POINT('Ctrl Pts',(39.2899718616341,44.094086908393,39.9385375612105));
#176583=CARTESIAN_POINT('Ctrl Pts',(39.294616428235,44.1062793237767,39.919022697722));
#176584=CARTESIAN_POINT('Ctrl Pts',(39.3008183122675,44.1172870736838,39.8992655451998));
#176585=CARTESIAN_POINT('Ctrl Pts',(39.3051423761588,44.1249618727689,39.8854905069421));
#176586=CARTESIAN_POINT('Ctrl Pts',(39.3102242458182,44.1320601713525,39.8715976051522));
#176587=CARTESIAN_POINT('Ctrl Pts',(39.3160391863696,44.1385184650371,39.8576902534424));
#176588=CARTESIAN_POINT('',(39.5544469813076,44.4033023070484,39.2875012672119));
#176589=CARTESIAN_POINT('',(39.3160391863695,44.1385184650371,39.8576902534424));
#176590=CARTESIAN_POINT('',(35.2091516650533,47.9220530736683,39.2875012672119));
#176591=CARTESIAN_POINT('Origin',(5.53234440788222E-15,0.,39.2875012672119));
#176592=CARTESIAN_POINT('',(34.9997217530266,47.6338034047596,39.8576902534424));
#176593=CARTESIAN_POINT('',(35.2091516650533,47.9220530736683,39.2875012672119));
#176594=CARTESIAN_POINT('',(34.6451144164191,47.6590285860932,40.1599502534424));
#176595=CARTESIAN_POINT('Ctrl Pts',(34.9997217530266,47.6338034047596,39.8576902534424));
#176596=CARTESIAN_POINT('Ctrl Pts',(34.9925330475319,47.6239092440465,39.8772619994051));
#176597=CARTESIAN_POINT('Ctrl Pts',(34.9838215185872,47.6151892923581,39.8967644650364));
#176598=CARTESIAN_POINT('Ctrl Pts',(34.9737453812853,47.6077336605728,39.915928283604));
#176599=CARTESIAN_POINT('Ctrl Pts',(34.9634872321473,47.6001433528506,39.9354382707181));
#176600=CARTESIAN_POINT('Ctrl Pts',(34.951814212463,47.5938626849621,39.9545987622351));
#176601=CARTESIAN_POINT('Ctrl Pts',(34.9388460388069,47.5890113136625,39.9731387498229));
#176602=CARTESIAN_POINT('Ctrl Pts',(34.9264269040003,47.5843653368455,39.9908938024059));
#176603=CARTESIAN_POINT('Ctrl Pts',(34.9128191931108,47.5810297921597,40.008081036619));
#176604=CARTESIAN_POINT('Ctrl Pts',(34.8980952063197,47.5791401905755,40.0244542742552));
#176605=CARTESIAN_POINT('Ctrl Pts',(34.8863842314135,47.5776372636136,40.0374770090492));
#176606=CARTESIAN_POINT('Ctrl Pts',(34.8739663878191,47.5770495124717,40.0499848770041));
#176607=CARTESIAN_POINT('Ctrl Pts',(34.8608666162967,47.5774624305256,40.0618424270192));
#176608=CARTESIAN_POINT('Ctrl Pts',(34.8608308581757,47.5774635576577,40.0618747942791));
#176609=CARTESIAN_POINT('Ctrl Pts',(34.8607950951003,47.5774646923706,40.0619071564124));
#176610=CARTESIAN_POINT('Ctrl Pts',(34.8607593270722,47.5774658346655,40.0619395134161));
#176611=CARTESIAN_POINT('Ctrl Pts',(34.8536390475845,47.5776932293351,40.0683807661799));
#176612=CARTESIAN_POINT('Ctrl Pts',(34.8462974884548,47.5782477067928,40.0746073439084));
#176613=CARTESIAN_POINT('Ctrl Pts',(34.8387748826518,47.5791245434503,40.0805869293669));
#176614=CARTESIAN_POINT('Ctrl Pts',(34.8238457504807,47.5808646865199,40.092453830807));
#176615=CARTESIAN_POINT('Ctrl Pts',(34.8082026058783,47.5838754712048,40.1033475319609));
#176616=CARTESIAN_POINT('Ctrl Pts',(34.7921542117509,47.5881261212202,40.1130129263075));
#176617=CARTESIAN_POINT('Ctrl Pts',(34.7801179161553,47.5913141087317,40.1202619720674));
#176618=CARTESIAN_POINT('Ctrl Pts',(34.7678536672185,47.595199519839,40.1268200947266));
#176619=CARTESIAN_POINT('Ctrl Pts',(34.7554917310469,47.599769379934,40.1325796782703));
#176620=CARTESIAN_POINT('Ctrl Pts',(34.7508560049825,47.6014830774696,40.1347395220992));
#176621=CARTESIAN_POINT('Ctrl Pts',(34.7462065417646,47.6032930257984,40.1367870714852));
#176622=CARTESIAN_POINT('Ctrl Pts',(34.7415502113776,47.6051985413675,40.1387166518767));
#176623=CARTESIAN_POINT('Ctrl Pts',(34.7252530550228,47.6118678458597,40.1454701832469));
#176624=CARTESIAN_POINT('Ctrl Pts',(34.7088717728658,47.6197078449343,40.1507785912492));
#176625=CARTESIAN_POINT('Ctrl Pts',(34.6927009428675,47.628689268873,40.1543986087265));
#176626=CARTESIAN_POINT('Ctrl Pts',(34.6846155278684,47.6331799808423,40.1562086174652));
#176627=CARTESIAN_POINT('Ctrl Pts',(34.6765827265058,47.6379560498532,40.1575965292115));
#176628=CARTESIAN_POINT('Ctrl Pts',(34.6686393635487,47.6430138207121,40.1585319382567));
#176629=CARTESIAN_POINT('Ctrl Pts',(34.6646676820701,47.6455427061416,40.1589996427793));
#176630=CARTESIAN_POINT('Ctrl Pts',(34.6607183602076,47.6481420170538,40.159354221642));
#176631=CARTESIAN_POINT('Ctrl Pts',(34.6567960012268,47.6508112967865,40.159591874311));
#176632=CARTESIAN_POINT('Ctrl Pts',(34.6528736422461,47.6534805765192,40.1598295269801));
#176633=CARTESIAN_POINT('Ctrl Pts',(34.6489782471464,47.6562198264468,40.1599502506894));
#176634=CARTESIAN_POINT('Ctrl Pts',(34.6451144164191,47.6590285860932,40.1599502534424));
#176635=CARTESIAN_POINT('',(34.620500570364,47.67691159203,40.1599502534424));
#176636=CARTESIAN_POINT('Origin',(5.69524824702573E-15,5.30782961123685E-15,
40.1599502534424));
#176637=CARTESIAN_POINT('',(34.4869303039402,48.0063682005183,39.8576902534424));
#176638=CARTESIAN_POINT('Ctrl Pts',(34.620500570364,47.67691159203,40.1599502534424));
#176639=CARTESIAN_POINT('Ctrl Pts',(34.617417796441,47.6791501491799,40.1599502448875));
#176640=CARTESIAN_POINT('Ctrl Pts',(34.614371068796,47.6814206292675,40.1598743450437));
#176641=CARTESIAN_POINT('Ctrl Pts',(34.6113613083103,47.6837210139132,40.1597243308499));
#176642=CARTESIAN_POINT('Ctrl Pts',(34.5935919100098,47.6973023109002,40.1588386583938));
#176643=CARTESIAN_POINT('Ctrl Pts',(34.5771079220191,47.7119261986124,40.1553722553615));
#176644=CARTESIAN_POINT('Ctrl Pts',(34.5621045892013,47.7271737594084,40.1496902177782));
#176645=CARTESIAN_POINT('Ctrl Pts',(34.5564998435001,47.7328697405523,40.1475675976839));
#176646=CARTESIAN_POINT('Ctrl Pts',(34.5511013106546,47.73865277922,40.1451361443093));
#176647=CARTESIAN_POINT('Ctrl Pts',(34.5459177227791,47.7445012740626,40.1424159447501));
#176648=CARTESIAN_POINT('Ctrl Pts',(34.5418732274832,47.7490645631293,40.1402935085949));
#176649=CARTESIAN_POINT('Ctrl Pts',(34.5379600899543,47.7536676237148,40.1379949176048));
#176650=CARTESIAN_POINT('Ctrl Pts',(34.5341829579105,47.75830010806,40.1355293609261));
#176651=CARTESIAN_POINT('Ctrl Pts',(34.5209629957571,47.7745138032684,40.1268999125509));
#176652=CARTESIAN_POINT('Ctrl Pts',(34.5094090955958,47.7910879322535,40.1162251288835));
#176653=CARTESIAN_POINT('Ctrl Pts',(34.4997205817199,47.8075789092548,40.1038990521418));
#176654=CARTESIAN_POINT('Ctrl Pts',(34.494876324782,47.8158243977555,40.097736013771));
#176655=CARTESIAN_POINT('Ctrl Pts',(34.4904984154667,47.8240490997338,40.0911601532641));
#176656=CARTESIAN_POINT('Ctrl Pts',(34.4866117722857,47.8321975711347,40.084220729064));
#176657=CARTESIAN_POINT('Ctrl Pts',(34.4827417346802,47.840311228417,40.0773109533618));
#176658=CARTESIAN_POINT('Ctrl Pts',(34.4793585234985,47.8483492841041,40.0700409753047));
#176659=CARTESIAN_POINT('Ctrl Pts',(34.4764874929868,47.8562570650393,40.0624586415899));
#176660=CARTESIAN_POINT('Ctrl Pts',(34.4764751739556,47.8562909957828,40.0624261072769));
#176661=CARTESIAN_POINT('Ctrl Pts',(34.4764628638112,47.8563249240887,40.0623935677888));
#176662=CARTESIAN_POINT('Ctrl Pts',(34.4764505625528,47.8563588499554,40.0623610231288));
#176663=CARTESIAN_POINT('Ctrl Pts',(34.4706495255091,47.8723576365719,40.0470135870269));
#176664=CARTESIAN_POINT('Ctrl Pts',(34.4668046706522,47.8877824700158,40.0305755292169));
#176665=CARTESIAN_POINT('Ctrl Pts',(34.4647575222394,47.9025205705478,40.0133447567459));
#176666=CARTESIAN_POINT('Ctrl Pts',(34.4626359025954,47.9177948141779,39.9954871626762));
#176667=CARTESIAN_POINT('Ctrl Pts',(34.462445422019,47.9323322825936,39.9767767954531));
#176668=CARTESIAN_POINT('Ctrl Pts',(34.4640592983631,47.9459912469213,39.9575197577743));
#176669=CARTESIAN_POINT('Ctrl Pts',(34.4656501410707,47.9594552671806,39.9385375612313));
#176670=CARTESIAN_POINT('Ctrl Pts',(34.4689948098043,47.9720663806451,39.9190226977461));
#176671=CARTESIAN_POINT('Ctrl Pts',(34.4740120960831,47.983662102353,39.8992655452271));
#176672=CARTESIAN_POINT('Ctrl Pts',(34.477510237347,47.9917468458453,39.8854905069605));
#176673=CARTESIAN_POINT('Ctrl Pts',(34.4818222937524,47.9993374592379,39.8715976051615));
#176674=CARTESIAN_POINT('Ctrl Pts',(34.4869303039402,48.0063682005183,39.8576902534424));
#176675=CARTESIAN_POINT('',(34.6963546279291,48.2946219293742,39.2875012672119));
#176676=CARTESIAN_POINT('',(34.4869303039402,48.0063682005183,39.8576902534424));
#176677=CARTESIAN_POINT('',(30.0070536838164,51.3398895692693,39.2875012672119));
#176678=CARTESIAN_POINT('Origin',(5.53234440788222E-15,0.,39.2875012672119));
#176679=CARTESIAN_POINT('',(29.8289013456892,51.0313275753405,39.8576902534424));
#176680=CARTESIAN_POINT('',(30.0070536838164,51.3398895692693,39.2875012672119));
#176681=CARTESIAN_POINT('',(29.4735998357344,51.0193480105324,40.1599502534424));
#176682=CARTESIAN_POINT('Ctrl Pts',(29.8289013456892,51.0313275753405,39.8576902534424));
#176683=CARTESIAN_POINT('Ctrl Pts',(29.82278624209,51.020736191537,39.8772619994049));
#176684=CARTESIAN_POINT('Ctrl Pts',(29.8150339189622,51.0111534059232,39.896764465036));
#176685=CARTESIAN_POINT('Ctrl Pts',(29.8057923055281,51.0026853737211,39.9159282836033));
#176686=CARTESIAN_POINT('Ctrl Pts',(29.7963837548065,50.9940643779337,39.935438270717));
#176687=CARTESIAN_POINT('Ctrl Pts',(29.7854311897083,50.9865979533917,39.9545987622337));
#176688=CARTESIAN_POINT('Ctrl Pts',(29.7730411634515,50.9804176151481,39.9731387498212));
#176689=CARTESIAN_POINT('Ctrl Pts',(29.7611756987822,50.9744989364018,39.9908938024036));
#176690=CARTESIAN_POINT('Ctrl Pts',(29.7479911917175,50.969759271071,40.0080810366163));
#176691=CARTESIAN_POINT('Ctrl Pts',(29.7335453816171,50.9663409452095,40.0244542742521));
#176692=CARTESIAN_POINT('Ctrl Pts',(29.7220556593017,50.963622121228,40.0374770090473));
#176693=CARTESIAN_POINT('Ctrl Pts',(29.7097672786766,50.9617395717401,40.0499848770032));
#176694=CARTESIAN_POINT('Ctrl Pts',(29.6966961073826,50.9607809287992,40.0618424270192));
#176695=CARTESIAN_POINT('Ctrl Pts',(29.6966604273309,50.9607783120154,40.0618747942791));
#176696=CARTESIAN_POINT('Ctrl Pts',(29.6966247415596,50.9607757022529,40.0619071564124));
#176697=CARTESIAN_POINT('Ctrl Pts',(29.6965890500702,50.9607730995132,40.0619395134161));
#176698=CARTESIAN_POINT('Ctrl Pts',(29.6894840070031,50.9602549766181,40.0683807661799));
#176699=CARTESIAN_POINT('Ctrl Pts',(29.682124707026,50.9600390146964,40.0746073439084));
#176700=CARTESIAN_POINT('Ctrl Pts',(29.6745516564563,50.9601247215267,40.0805869293668));
#176701=CARTESIAN_POINT('Ctrl Pts',(29.6595224131525,50.9602948126666,40.092453830807));
#176702=CARTESIAN_POINT('Ctrl Pts',(29.6436502506365,50.9616539500921,40.1033475319609));
#176703=CARTESIAN_POINT('Ctrl Pts',(29.6272454573773,50.9642038006258,40.1130129263075));
#176704=CARTESIAN_POINT('Ctrl Pts',(29.6149418624329,50.9661161885262,40.1202619720674));
#176705=CARTESIAN_POINT('Ctrl Pts',(29.6023386622828,50.9686983518504,40.1268200947266));
#176706=CARTESIAN_POINT('Ctrl Pts',(29.5895667656379,50.9719510035826,40.1325796782703));
#176707=CARTESIAN_POINT('Ctrl Pts',(29.584777304396,50.9731707479822,40.1347395220992));
#176708=CARTESIAN_POINT('Ctrl Pts',(29.5799641203068,50.9744847799794,40.1367870714852));
#176709=CARTESIAN_POINT('Ctrl Pts',(29.5751341171706,50.9758931378751,40.1387166518767));
#176710=CARTESIAN_POINT('Ctrl Pts',(29.5582291061939,50.9808223905101,40.1454701832469));
#176711=CARTESIAN_POINT('Ctrl Pts',(29.5411180593592,50.9869071309992,40.1507785912492));
#176712=CARTESIAN_POINT('Ctrl Pts',(29.5240970004174,50.9941490417483,40.1543986087265));
#176713=CARTESIAN_POINT('Ctrl Pts',(29.5155864709465,50.9977699971228,40.1562086174652));
#176714=CARTESIAN_POINT('Ctrl Pts',(29.5070984389562,51.0016802459459,40.1575965292115));
#176715=CARTESIAN_POINT('Ctrl Pts',(29.498669909557,51.0058800022837,40.1585319382567));
#176716=CARTESIAN_POINT('Ctrl Pts',(29.4944556448574,51.0079798804526,40.1589996427793));
#176717=CARTESIAN_POINT('Ctrl Pts',(29.490256255818,51.0101521355225,40.159354221642));
#176718=CARTESIAN_POINT('Ctrl Pts',(29.4860763682217,51.0123967945048,40.159591874311));
#176719=CARTESIAN_POINT('Ctrl Pts',(29.4818964806253,51.0146414534872,40.1598295269801));
#176720=CARTESIAN_POINT('Ctrl Pts',(29.4777360953222,51.0169585178535,40.1599502506895));
#176721=CARTESIAN_POINT('Ctrl Pts',(29.4735998357344,51.0193480105324,40.1599502534424));
#176722=CARTESIAN_POINT('',(29.4472515437741,51.0345602039883,40.1599502534424));
#176723=CARTESIAN_POINT('Origin',(5.68926707005281E-15,5.31171383297933E-15,
40.1599502534424));
#176724=CARTESIAN_POINT('',(29.2799753962469,51.3482501200162,39.8576902534424));
#176725=CARTESIAN_POINT('Ctrl Pts',(29.4472515437741,51.0345602039883,40.1599502534424));
#176726=CARTESIAN_POINT('Ctrl Pts',(29.4439516646705,51.0364642604672,40.1599502448875));
#176727=CARTESIAN_POINT('Ctrl Pts',(29.4406842975238,51.0384038328685,40.1598743450437));
#176728=CARTESIAN_POINT('Ctrl Pts',(29.4374505691491,51.0403770101281,40.1597243308499));
#176729=CARTESIAN_POINT('Ctrl Pts',(29.4183588813694,51.052026499451,40.1588386583938));
#176730=CARTESIAN_POINT('Ctrl Pts',(29.4004365818809,51.0648472300424,40.1553722553619));
#176731=CARTESIAN_POINT('Ctrl Pts',(29.3839216347922,51.0784429877809,40.149690217779));
#176732=CARTESIAN_POINT('Ctrl Pts',(29.3777522003177,51.0835219102896,40.1475675976846));
#176733=CARTESIAN_POINT('Ctrl Pts',(29.3717787490543,51.0887089685248,40.1451361443097));
#176734=CARTESIAN_POINT('Ctrl Pts',(29.3660122232364,51.0939835922265,40.1424159447501));
#176735=CARTESIAN_POINT('Ctrl Pts',(29.3615128905155,51.0980991182402,40.1402935085949));
#176736=CARTESIAN_POINT('Ctrl Pts',(29.357140038714,51.1022679285257,40.1379949176048));
#176737=CARTESIAN_POINT('Ctrl Pts',(29.352899371725,51.1064802178289,40.1355293609261));
#176738=CARTESIAN_POINT('Ctrl Pts',(29.3380570372635,51.1212232303902,40.1268999125509));
#176739=CARTESIAN_POINT('Ctrl Pts',(29.3248339623433,51.136498853134,40.1162251288835));
#176740=CARTESIAN_POINT('Ctrl Pts',(29.3134747466765,51.151886765371,40.1038990521418));
#176741=CARTESIAN_POINT('Ctrl Pts',(29.307795138843,51.1595807214895,40.097736013771));
#176742=CARTESIAN_POINT('Ctrl Pts',(29.3025814967144,51.1673027515568,40.0911601532641));
#176743=CARTESIAN_POINT('Ctrl Pts',(29.297864397778,51.1750003199398,40.084220729064));
#176744=CARTESIAN_POINT('Ctrl Pts',(29.2931674525162,51.1826650006749,40.0773109533618));
#176745=CARTESIAN_POINT('Ctrl Pts',(29.2889625693107,51.1903053811861,40.0700409753048));
#176746=CARTESIAN_POINT('Ctrl Pts',(29.2852806784154,51.1978697380626,40.0624586415899));
#176747=CARTESIAN_POINT('Ctrl Pts',(29.2852648801407,51.1979021952405,40.0624261072769));
#176748=CARTESIAN_POINT('Ctrl Pts',(29.2852490909589,51.1979346509232,40.0623935677889));
#176749=CARTESIAN_POINT('Ctrl Pts',(29.2852333108693,51.1979671051088,40.0623610231288));
#176750=CARTESIAN_POINT('Ctrl Pts',(29.2777917239323,51.2132718752149,40.0470135870226));
#176751=CARTESIAN_POINT('Ctrl Pts',(29.2723555974555,51.2282103130417,40.0305755292077));
#176752=CARTESIAN_POINT('Ctrl Pts',(29.2687791125359,51.242653691443,40.0133447567315));
#176753=CARTESIAN_POINT('Ctrl Pts',(29.2650725221321,51.2576224915312,39.9954871626564));
#176754=CARTESIAN_POINT('Ctrl Pts',(29.263363505796,51.2720604115355,39.9767767954275));
#176755=CARTESIAN_POINT('Ctrl Pts',(29.2635407906077,51.2858132466446,39.9575197577428));
#176756=CARTESIAN_POINT('Ctrl Pts',(29.2637155451674,51.2993697979382,39.9385375611947));
#176757=CARTESIAN_POINT('Ctrl Pts',(29.2657236711482,51.3122614394886,39.9190226977042));
#176758=CARTESIAN_POINT('Ctrl Pts',(29.2695013892409,51.3243180878457,39.8992655451801));
#176759=CARTESIAN_POINT('Ctrl Pts',(29.2721352815069,51.3327241975874,39.8854905069289));
#176760=CARTESIAN_POINT('Ctrl Pts',(29.2756302808599,51.3407239614254,39.8715976051456));
#176761=CARTESIAN_POINT('Ctrl Pts',(29.2799753962468,51.3482501200162,39.8576902534424));
#176762=CARTESIAN_POINT('',(29.458121752568,51.6568155675424,39.2875012672119));
#176763=CARTESIAN_POINT('',(29.2799753962469,51.3482501200162,39.8576902534424));
#176764=CARTESIAN_POINT('',(24.4761921430398,54.1952354911869,39.2875012672119));
#176765=CARTESIAN_POINT('Origin',(5.53234440788222E-15,0.,39.2875012672119));
#176766=CARTESIAN_POINT('',(24.3312692531094,53.8697418420142,39.8576902534424));
#176767=CARTESIAN_POINT('',(24.4761921430398,54.1952354911869,39.2875012672119));
#176768=CARTESIAN_POINT('',(23.979166327502,53.8206887816833,40.1599502534424));
#176769=CARTESIAN_POINT('Ctrl Pts',(24.3312692531094,53.8697418420142,39.8576902534424));
#176770=CARTESIAN_POINT('Ctrl Pts',(24.3262947497605,53.8585692765376,39.8772619994046));
#176771=CARTESIAN_POINT('Ctrl Pts',(24.3195865685239,53.8482286480028,39.8967644650355));
#176772=CARTESIAN_POINT('Ctrl Pts',(24.3112807320083,53.8388409929169,39.9159282836026));
#176773=CARTESIAN_POINT('Ctrl Pts',(24.3028248617536,53.8292837624981,39.9354382707161));
#176774=CARTESIAN_POINT('Ctrl Pts',(24.2927127498367,53.8207133850125,39.9545987622325));
#176775=CARTESIAN_POINT('Ctrl Pts',(24.2810366186995,53.8132717929041,39.9731387498198));
#176776=CARTESIAN_POINT('Ctrl Pts',(24.2698548246814,53.8061452585114,39.9908938024019));
#176777=CARTESIAN_POINT('Ctrl Pts',(24.2572379736598,53.8000534013008,40.0080810366143));
#176778=CARTESIAN_POINT('Ctrl Pts',(24.2432286115683,53.7951438030556,40.0244542742498));
#176779=CARTESIAN_POINT('Ctrl Pts',(24.2320860256461,53.791238870059,40.0374770090458));
#176780=CARTESIAN_POINT('Ctrl Pts',(24.2200617420602,53.7880821478312,40.0499848770025));
#176781=CARTESIAN_POINT('Ctrl Pts',(24.2071623814828,53.785762446988,40.0618424270193));
#176782=CARTESIAN_POINT('Ctrl Pts',(24.2071271704186,53.7857561149582,40.0618747942791));
#176783=CARTESIAN_POINT('Ctrl Pts',(24.2070919529321,53.7857497893135,40.0619071564124));
#176784=CARTESIAN_POINT('Ctrl Pts',(24.2070567290248,53.7857434700553,40.0619395134161));
#176785=CARTESIAN_POINT('Ctrl Pts',(24.2000447667171,53.7844855062584,40.0683807661799));
#176786=CARTESIAN_POINT('Ctrl Pts',(24.192748355923,53.7835014710813,40.0746073439084));
#176787=CARTESIAN_POINT('Ctrl Pts',(24.1852078325135,53.7827951090623,40.0805869293669));
#176788=CARTESIAN_POINT('Ctrl Pts',(24.1702431416115,53.7813932847186,40.092453830807));
#176789=CARTESIAN_POINT('Ctrl Pts',(24.1543158599161,53.7810858838905,40.1033475319609));
#176790=CARTESIAN_POINT('Ctrl Pts',(24.137734401873,53.7819069982466,40.1130129263075));
#176791=CARTESIAN_POINT('Ctrl Pts',(24.1252983083407,53.7825228340137,40.1202619720674));
#176792=CARTESIAN_POINT('Ctrl Pts',(24.1124942402755,53.7837734588331,40.1268200947266));
#176793=CARTESIAN_POINT('Ctrl Pts',(24.0994523147296,53.7856732654695,40.1325796782703));
#176794=CARTESIAN_POINT('Ctrl Pts',(24.0945615926499,53.7863856929582,40.1347395220992));
#176795=CARTESIAN_POINT('Ctrl Pts',(24.0896374219413,53.7871894118144,40.1367870714852));
#176796=CARTESIAN_POINT('Ctrl Pts',(24.0846866645811,53.7880851817728,40.1387166518767));
#176797=CARTESIAN_POINT('Ctrl Pts',(24.0673590138204,53.7912203766271,40.1454701832469));
#176798=CARTESIAN_POINT('Ctrl Pts',(24.0497056745179,53.7954831928406,40.1507785912491));
#176799=CARTESIAN_POINT('Ctrl Pts',(24.0320208729162,53.8009062465105,40.1543986087265));
#176800=CARTESIAN_POINT('Ctrl Pts',(24.0231784721154,53.8036177733455,40.1562086174652));
#176801=CARTESIAN_POINT('Ctrl Pts',(24.0143282061519,53.8066193604762,40.1575965292115));
#176802=CARTESIAN_POINT('Ctrl Pts',(24.0055068550426,53.8099150888837,40.1585319382567));
#176803=CARTESIAN_POINT('Ctrl Pts',(24.0010961794879,53.8115629530874,40.1589996427793));
#176804=CARTESIAN_POINT('Ctrl Pts',(23.9966927326568,53.8132843526338,40.159354221642));
#176805=CARTESIAN_POINT('Ctrl Pts',(23.9923011121681,53.8150797979123,40.159591874311));
#176806=CARTESIAN_POINT('Ctrl Pts',(23.9879094916794,53.8168752431908,40.1598295269801));
#176807=CARTESIAN_POINT('Ctrl Pts',(23.9835296982247,53.8187447357538,40.1599502506895));
#176808=CARTESIAN_POINT('Ctrl Pts',(23.979166327502,53.8206887816833,40.1599502534424));
#176809=CARTESIAN_POINT('',(23.9513722670371,53.8330634946835,40.1599502534424));
#176810=CARTESIAN_POINT('Origin',(5.68291264686342E-15,5.31495157331118E-15,
40.1599502534424));
#176811=CARTESIAN_POINT('',(23.7522229508834,54.1275498658871,39.8576902534424));
#176812=CARTESIAN_POINT('Ctrl Pts',(23.9513722670371,53.8330634946835,40.1599502534424));
#176813=CARTESIAN_POINT('Ctrl Pts',(23.9478914369187,53.8346121892501,40.1599502448875));
#176814=CARTESIAN_POINT('Ctrl Pts',(23.9444392282286,53.8361996036041,40.1598743450437));
#176815=CARTESIAN_POINT('Ctrl Pts',(23.9410169613696,53.8378239549346,40.1597243308499));
#176816=CARTESIAN_POINT('Ctrl Pts',(23.9208121566336,53.8474140023525,40.1588386583937));
#176817=CARTESIAN_POINT('Ctrl Pts',(23.9016479061078,53.8582911092182,40.1553722553609));
#176818=CARTESIAN_POINT('Ctrl Pts',(23.8838022859618,53.8700861059349,40.1496902177767));
#176819=CARTESIAN_POINT('Ctrl Pts',(23.8771357563326,53.8744923240684,40.1475675976828));
#176820=CARTESIAN_POINT('Ctrl Pts',(23.8706528330364,53.8790265713733,40.1451361443087));
#176821=CARTESIAN_POINT('Ctrl Pts',(23.8643665485428,53.8836695340507,40.1424159447501));
#176822=CARTESIAN_POINT('Ctrl Pts',(23.8594616740274,53.8872922064472,40.1402935085949));
#176823=CARTESIAN_POINT('Ctrl Pts',(23.8546770178329,53.8909810920749,40.1379949176048));
#176824=CARTESIAN_POINT('Ctrl Pts',(23.8500192775337,53.894727035613,40.1355293609261));
#176825=CARTESIAN_POINT('Ctrl Pts',(23.8337171864864,53.9078378379962,40.1268999125508));
#176826=CARTESIAN_POINT('Ctrl Pts',(23.8189698115833,53.9216475915792,40.1162251288835));
#176827=CARTESIAN_POINT('Ctrl Pts',(23.8060643480694,53.9357638458653,40.1038990521418));
#176828=CARTESIAN_POINT('Ctrl Pts',(23.7996116163124,53.9428219730084,40.0977360137709));
#176829=CARTESIAN_POINT('Ctrl Pts',(23.7936193631247,53.9499567269873,40.0911601532641));
#176830=CARTESIAN_POINT('Ctrl Pts',(23.7881234899558,53.9571190561824,40.084220729064));
#176831=CARTESIAN_POINT('Ctrl Pts',(23.7826510977529,53.9642507845242,40.0773109533618));
#176832=CARTESIAN_POINT('Ctrl Pts',(23.7776706121039,53.9714097802518,40.0700409753047));
#176833=CARTESIAN_POINT('Ctrl Pts',(23.7732182003924,53.9785478363927,40.0624586415899));
#176834=CARTESIAN_POINT('Ctrl Pts',(23.7731990959634,53.9785784643974,40.0624261072769));
#176835=CARTESIAN_POINT('Ctrl Pts',(23.7731800007337,53.9786090918655,40.0623935677888));
#176836=CARTESIAN_POINT('Ctrl Pts',(23.7731609147029,53.9786397187951,40.0623610231288));
#176837=CARTESIAN_POINT('Ctrl Pts',(23.7641603094588,53.9930827901211,40.0470135870241));
#176838=CARTESIAN_POINT('Ctrl Pts',(23.7571924707025,54.0073711636743,40.0305755292109));
#176839=CARTESIAN_POINT('Ctrl Pts',(23.7521258339929,54.0213615752637,40.0133447567365));
#176840=CARTESIAN_POINT('Ctrl Pts',(23.7468748830091,54.0358609304986,39.9954871626633));
#176841=CARTESIAN_POINT('Ctrl Pts',(23.7436660552522,54.0500411172139,39.9767767954363));
#176842=CARTESIAN_POINT('Ctrl Pts',(23.7424048061591,54.0637371441611,39.9575197577536));
#176843=CARTESIAN_POINT('Ctrl Pts',(23.7411615579205,54.0772376980728,39.9385375612074));
#176844=CARTESIAN_POINT('Ctrl Pts',(23.7418111396958,54.090268624184,39.9190226977187));
#176845=CARTESIAN_POINT('Ctrl Pts',(23.7443079001274,54.1026541040261,39.8992655451964));
#176846=CARTESIAN_POINT('Ctrl Pts',(23.7460486859225,54.1112894809336,39.8854905069398));
#176847=CARTESIAN_POINT('Ctrl Pts',(23.7486883362836,54.1196107481433,39.8715976051511));
#176848=CARTESIAN_POINT('Ctrl Pts',(23.7522229508834,54.1275498658871,39.8576902534424));
#176849=CARTESIAN_POINT('',(23.8971395307774,54.453046324469,39.2875012672119));
#176850=CARTESIAN_POINT('',(23.7522229508834,54.1275498658871,39.8576902534424));
#176851=CARTESIAN_POINT('',(18.6771643191716,56.4568070719809,39.2875012672119));
#176852=CARTESIAN_POINT('Origin',(5.53234440788222E-15,0.,39.2875012672119));
#176853=CARTESIAN_POINT('',(18.5670586829472,56.1179479440986,39.8576902534424));
#176854=CARTESIAN_POINT('',(18.6771643191716,56.4568070719809,39.2875012672119));
#176855=CARTESIAN_POINT('',(18.2220120550223,56.0323588238389,40.1599502534424));
#176856=CARTESIAN_POINT('Ctrl Pts',(18.5670586829472,56.1179479440986,39.8576902534424));
#176857=CARTESIAN_POINT('Ctrl Pts',(18.5632792815478,56.106316605913,39.8772619994065));
#176858=CARTESIAN_POINT('Ctrl Pts',(18.5576887384393,56.0953314285463,39.8967644650392));
#176859=CARTESIAN_POINT('Ctrl Pts',(18.5504096793239,56.0851270036893,39.915928283608));
#176860=CARTESIAN_POINT('Ctrl Pts',(18.5429991338191,56.0747382496544,39.9354382707233));
#176861=CARTESIAN_POINT('Ctrl Pts',(18.5338382654961,56.0651578180737,39.9545987622415));
#176862=CARTESIAN_POINT('Ctrl Pts',(18.5230039556125,56.0565365037403,39.9731387498304));
#176863=CARTESIAN_POINT('Ctrl Pts',(18.512628342319,56.048280193503,39.990893802414));
#176864=CARTESIAN_POINT('Ctrl Pts',(18.5007173801981,56.0409028880748,40.0080810366277));
#176865=CARTESIAN_POINT('Ctrl Pts',(18.4872979556155,56.0345558080316,40.0244542742644));
#176866=CARTESIAN_POINT('Ctrl Pts',(18.4766245865934,56.0295075492857,40.0374770090551));
#176867=CARTESIAN_POINT('Ctrl Pts',(18.4649961406185,56.0251112400293,40.049984877007));
#176868=CARTESIAN_POINT('Ctrl Pts',(18.4524099188571,56.0214558964132,40.0618424270193));
#176869=CARTESIAN_POINT('Ctrl Pts',(18.4523755625601,56.0214459185124,40.0618747942791));
#176870=CARTESIAN_POINT('Ctrl Pts',(18.4523411992087,56.0214359462905,40.0619071564124));
#176871=CARTESIAN_POINT('Ctrl Pts',(18.4523068288039,56.021425979749,40.0619395134162));
#176872=CARTESIAN_POINT('Ctrl Pts',(18.445464771782,56.0194419575648,40.0683807661799));
#176873=CARTESIAN_POINT('Ctrl Pts',(18.4383111911745,56.0177006304278,40.0746073439084));
#176874=CARTESIAN_POINT('Ctrl Pts',(18.4308858104775,56.0162099386096,40.0805869293669));
#176875=CARTESIAN_POINT('Ctrl Pts',(18.4161496282625,56.0132515574631,40.092453830807));
#176876=CARTESIAN_POINT('Ctrl Pts',(18.4003417300189,56.0112809863292,40.1033475319609));
#176877=CARTESIAN_POINT('Ctrl Pts',(18.3837652771161,56.010364368207,40.1130129263075));
#176878=CARTESIAN_POINT('Ctrl Pts',(18.371332937439,56.0096769046154,40.1202619720674));
#176879=CARTESIAN_POINT('Ctrl Pts',(18.3584682855079,56.0095822888227,40.1268200947266));
#176880=CARTESIAN_POINT('Ctrl Pts',(18.3452992211265,56.0101084356842,40.1325796782703));
#176881=CARTESIAN_POINT('Ctrl Pts',(18.3403608219835,56.0103057407573,40.1347395220992));
#176882=CARTESIAN_POINT('Ctrl Pts',(18.3353796149004,56.0105903407604,40.1367870714852));
#176883=CARTESIAN_POINT('Ctrl Pts',(18.3303623448498,56.0109637085384,40.1387166518767));
#176884=CARTESIAN_POINT('Ctrl Pts',(18.3128018996728,56.0122704957612,40.1454701832468));
#176885=CARTESIAN_POINT('Ctrl Pts',(18.2947996815822,56.0146646833927,40.1507785912492));
#176886=CARTESIAN_POINT('Ctrl Pts',(18.2766448957077,56.0182094638725,40.1543986087265));
#176887=CARTESIAN_POINT('Ctrl Pts',(18.2675675027704,56.0199818541124,40.1562086174652));
#176888=CARTESIAN_POINT('Ctrl Pts',(18.2584519681998,56.0220418935341,40.1575965292115));
#176889=CARTESIAN_POINT('Ctrl Pts',(18.2493344439491,56.0243974853212,40.1585319382567));
#176890=CARTESIAN_POINT('Ctrl Pts',(18.2447756818237,56.0255752812147,40.1589996427793));
#176891=CARTESIAN_POINT('Ctrl Pts',(18.2402164222858,56.0268269652239,40.159354221642));
#176892=CARTESIAN_POINT('Ctrl Pts',(18.2356611844178,56.0281535255243,40.159591874311));
#176893=CARTESIAN_POINT('Ctrl Pts',(18.2311059465498,56.0294800858248,40.1598295269801));
#176894=CARTESIAN_POINT('Ctrl Pts',(18.2265547308772,56.0308815240327,40.1599502506895));
#176895=CARTESIAN_POINT('Ctrl Pts',(18.2220120550223,56.0323588238389,40.1599502534424));
#176896=CARTESIAN_POINT('',(18.1930767435955,56.0417604764381,40.1599502534424));
#176897=CARTESIAN_POINT('Origin',(5.6762545978478E-15,5.31750735887178E-15,
40.1599502534424));
#176898=CARTESIAN_POINT('',(17.9642361803979,56.3138168485093,39.8576902534424));
#176899=CARTESIAN_POINT('Ctrl Pts',(18.1930767435955,56.0417604764381,40.1599502534424));
#176900=CARTESIAN_POINT('Ctrl Pts',(18.1894530991656,56.0429368412706,40.1599502448875));
#176901=CARTESIAN_POINT('Ctrl Pts',(18.185853872053,56.0441547055335,40.1598743450437));
#176902=CARTESIAN_POINT('Ctrl Pts',(18.1822805617814,56.0454124342017,40.1597243308498));
#176903=CARTESIAN_POINT('Ctrl Pts',(18.1611840081625,56.0528379691462,40.1588386583938));
#176904=CARTESIAN_POINT('Ctrl Pts',(18.1409877741425,56.0616522804243,40.1553722553615));
#176905=CARTESIAN_POINT('Ctrl Pts',(18.1220070012914,56.071517287664,40.1496902177782));
#176906=CARTESIAN_POINT('Ctrl Pts',(18.1149164163968,56.0752025259768,40.1475675976839));
#176907=CARTESIAN_POINT('Ctrl Pts',(18.1079950493283,56.0790342841917,40.1451361443093));
#176908=CARTESIAN_POINT('Ctrl Pts',(18.1012578800035,56.0829947165769,40.1424159447501));
#176909=CARTESIAN_POINT('Ctrl Pts',(18.0960012025255,56.0860848445994,40.1402935085949));
#176910=CARTESIAN_POINT('Ctrl Pts',(18.0908571636324,56.0892533893664,40.1379949176048));
#176911=CARTESIAN_POINT('Ctrl Pts',(18.0858333812004,56.0924919457981,40.1355293609261));
#176912=CARTESIAN_POINT('Ctrl Pts',(18.0682501426882,56.1038268933088,40.1268999125509));
#176913=CARTESIAN_POINT('Ctrl Pts',(18.0521400431277,56.1160194751809,40.1162251288835));
#176914=CARTESIAN_POINT('Ctrl Pts',(18.0378297267256,56.1287094108802,40.1038990521418));
#176915=CARTESIAN_POINT('Ctrl Pts',(18.0306745685246,56.1350543787298,40.0977360137709));
#176916=CARTESIAN_POINT('Ctrl Pts',(18.0239693566576,56.1415236867627,40.0911601532641));
#176917=CARTESIAN_POINT('Ctrl Pts',(18.0177549231928,56.1480723047924,40.084220729064));
#176918=CARTESIAN_POINT('Ctrl Pts',(18.011567040723,56.1545929440327,40.0773109533618));
#176919=CARTESIAN_POINT('Ctrl Pts',(18.0058655198736,56.1611921195215,40.0700409753047));
#176920=CARTESIAN_POINT('Ctrl Pts',(18.0006913689001,56.1678256688899,40.0624586415899));
#176921=CARTESIAN_POINT('Ctrl Pts',(18.0006691676289,56.1678541321546,40.0624261072769));
#176922=CARTESIAN_POINT('Ctrl Pts',(18.0006469755627,56.1678825958472,40.0623935677888));
#176923=CARTESIAN_POINT('Ctrl Pts',(18.0006247927013,56.1679110599659,40.0623610231288));
#176924=CARTESIAN_POINT('Ctrl Pts',(17.9901637816636,56.1813341912017,40.0470135870236));
#176925=CARTESIAN_POINT('Ctrl Pts',(17.9817405717267,56.1948159540725,40.0305755292099));
#176926=CARTESIAN_POINT('Ctrl Pts',(17.9752392943591,56.2082001169745,40.0133447567349));
#176927=CARTESIAN_POINT('Ctrl Pts',(17.9685015133131,56.2220711693878,39.995487162661));
#176928=CARTESIAN_POINT('Ctrl Pts',(17.9638280307243,56.2358382617226,39.9767767954334));
#176929=CARTESIAN_POINT('Ctrl Pts',(17.9611420662362,56.2493274239721,39.95751975775));
#176930=CARTESIAN_POINT('Ctrl Pts',(17.958494436488,56.2626240656095,39.938537561203));
#176931=CARTESIAN_POINT('Ctrl Pts',(17.9577783571053,56.2756515067291,39.9190226977136));
#176932=CARTESIAN_POINT('Ctrl Pts',(17.9589668048477,56.2882301201481,39.8992655451906));
#176933=CARTESIAN_POINT('Ctrl Pts',(17.9597954117583,56.2970001532202,39.8854905069359));
#176934=CARTESIAN_POINT('Ctrl Pts',(17.9615507925645,56.305551754252,39.8715976051492));
#176935=CARTESIAN_POINT('Ctrl Pts',(17.9642361803979,56.3138168485093,39.8576902534424));
#176936=CARTESIAN_POINT('',(18.0743352474898,56.6526781108321,39.2875012672119));
#176937=CARTESIAN_POINT('',(17.9642361803979,56.3138168485093,39.8576902534424));
#176938=CARTESIAN_POINT('',(12.6735055745747,58.0998260601478,39.2875012672119));
#176939=CARTESIAN_POINT('Origin',(5.53234440788222E-15,0.,39.2875012672119));
#176940=CARTESIAN_POINT('',(12.5994235324478,57.7513140650719,39.8576902534424));
#176941=CARTESIAN_POINT('',(12.6735055745747,58.0998260601478,39.2875012672119));
#176942=CARTESIAN_POINT('',(12.2652136052667,57.6301266171956,40.1599502534424));
#176943=CARTESIAN_POINT('Ctrl Pts',(12.5994235324478,57.7513140650719,39.8576902534424));
#176944=CARTESIAN_POINT('Ctrl Pts',(12.5968806409115,57.739351389555,39.8772619994039));
#176945=CARTESIAN_POINT('Ctrl Pts',(12.5924689870928,57.7278420192608,39.8967644650342));
#176946=CARTESIAN_POINT('Ctrl Pts',(12.5862964562751,57.7169326264487,39.9159282836006));
#176947=CARTESIAN_POINT('Ctrl Pts',(12.5800124270096,57.7058261701631,39.9354382707136));
#176948=CARTESIAN_POINT('Ctrl Pts',(12.571903170674,57.695340649702,39.9545987622296));
#176949=CARTESIAN_POINT('Ctrl Pts',(12.5620293850143,57.6856340700687,39.9731387498165));
#176950=CARTESIAN_POINT('Ctrl Pts',(12.5525736298391,57.6763384418503,39.9908938023985));
#176951=CARTESIAN_POINT('Ctrl Pts',(12.5414990556166,57.6677565155071,40.0080810366108));
#176952=CARTESIAN_POINT('Ctrl Pts',(12.5288165945717,57.6600414936031,40.0244542742463));
#176953=CARTESIAN_POINT('Ctrl Pts',(12.518729382107,57.6539052188818,40.0374770090436));
#176954=CARTESIAN_POINT('Ctrl Pts',(12.5076241774218,57.6483174894766,40.0499848770015));
#176955=CARTESIAN_POINT('Ctrl Pts',(12.4954889917454,57.6433665517939,40.0618424270192));
#176956=CARTESIAN_POINT('Ctrl Pts',(12.4954558666304,57.6433530373422,40.0618747942791));
#176957=CARTESIAN_POINT('Ctrl Pts',(12.4954227339061,57.6433395278008,40.0619071564124));
#176958=CARTESIAN_POINT('Ctrl Pts',(12.4953895935733,57.6433260231715,40.0619395134161));
#176959=CARTESIAN_POINT('Ctrl Pts',(12.4887924048456,57.6406376799624,40.0683807661799));
#176960=CARTESIAN_POINT('Ctrl Pts',(12.4818600305509,57.6381581392098,40.0746073439084));
#176961=CARTESIAN_POINT('Ctrl Pts',(12.4746311465912,57.6358994499239,40.0805869293669));
#176962=CARTESIAN_POINT('Ctrl Pts',(12.4602849257593,57.6314169246175,40.092453830807));
#176963=CARTESIAN_POINT('Ctrl Pts',(12.4447696056087,57.6278047731676,40.1033475319609));
#176964=CARTESIAN_POINT('Ctrl Pts',(12.428379772933,57.625160465227,40.1130129263075));
#176965=CARTESIAN_POINT('Ctrl Pts',(12.4160873984262,57.6231772342716,40.1202619720674));
#176966=CARTESIAN_POINT('Ctrl Pts',(12.4033031104478,57.6217384144973,40.1268200947266));
#176967=CARTESIAN_POINT('Ctrl Pts',(12.3901511902562,57.6208851370088,40.1325796782703));
#176968=CARTESIAN_POINT('Ctrl Pts',(12.3852192201843,57.6205651579506,40.1347395220992));
#176969=CARTESIAN_POINT('Ctrl Pts',(12.3802355518738,57.6203275209636,40.1367870714852));
#176970=CARTESIAN_POINT('Ctrl Pts',(12.3752067393935,57.6201743958656,40.1387166518767));
#176971=CARTESIAN_POINT('Ctrl Pts',(12.3576058957123,57.6196384580226,40.1454701832469));
#176972=CARTESIAN_POINT('Ctrl Pts',(12.339452034902,57.6201377858513,40.1507785912492));
#176973=CARTESIAN_POINT('Ctrl Pts',(12.321026172388,57.6217654557844,40.1543986087265));
#176974=CARTESIAN_POINT('Ctrl Pts',(12.3118132411309,57.6225792907509,40.1562086174652));
#176975=CARTESIAN_POINT('Ctrl Pts',(12.3025323096575,57.6236752122406,40.1575965292115));
#176976=CARTESIAN_POINT('Ctrl Pts',(12.293218505769,57.6250648590506,40.1585319382567));
#176977=CARTESIAN_POINT('Ctrl Pts',(12.2885616038247,57.6257596824556,40.1589996427793));
#176978=CARTESIAN_POINT('Ctrl Pts',(12.2838964837817,57.6265279372157,40.159354221642));
#176979=CARTESIAN_POINT('Ctrl Pts',(12.2792275366736,57.6273710784659,40.159591874311));
#176980=CARTESIAN_POINT('Ctrl Pts',(12.2745585895656,57.628214219716,40.1598295269801));
#176981=CARTESIAN_POINT('Ctrl Pts',(12.2698858157465,57.6291322491185,40.1599502506895));
#176982=CARTESIAN_POINT('Ctrl Pts',(12.2652136052667,57.6301266171956,40.1599502534424));
#176983=CARTESIAN_POINT('',(12.2354540642051,57.6364522029206,40.1599502534424));
#176984=CARTESIAN_POINT('Origin',(5.66936586998424E-15,5.3193531879397E-15,
40.1599502534424));
#176985=CARTESIAN_POINT('',(11.9794294790618,57.8830978693155,39.8576902534424));
#176986=CARTESIAN_POINT('Ctrl Pts',(12.2354540642051,57.6364522029206,40.1599502534424));
#176987=CARTESIAN_POINT('Ctrl Pts',(12.2317273068703,57.6372433495198,40.1599502448875));
#176988=CARTESIAN_POINT('Ctrl Pts',(12.2280204952205,57.6380783205157,40.1598743450437));
#176989=CARTESIAN_POINT('Ctrl Pts',(12.2243352914717,57.6389556465833,40.1597243308499));
#176990=CARTESIAN_POINT('Ctrl Pts',(12.202578127225,57.6441353133401,40.1588386583938));
#176991=CARTESIAN_POINT('Ctrl Pts',(12.1815711838763,57.6507902575925,40.1553722553618));
#176992=CARTESIAN_POINT('Ctrl Pts',(12.1616632156387,57.6586171922721,40.1496902177789));
#176993=CARTESIAN_POINT('Ctrl Pts',(12.1542262614116,57.6615410745215,40.1475675976844));
#176994=CARTESIAN_POINT('Ctrl Pts',(12.1469422825174,57.664628362101,40.1451361443096));
#176995=CARTESIAN_POINT('Ctrl Pts',(12.1398280421993,57.6678628728672,40.1424159447501));
#176996=CARTESIAN_POINT('Ctrl Pts',(12.134277155017,57.6703866004264,40.1402935085949));
#176997=CARTESIAN_POINT('Ctrl Pts',(12.1288300925919,57.6730000890931,40.1379949176047));
#176998=CARTESIAN_POINT('Ctrl Pts',(12.1234953096386,57.6756957761164,40.1355293609261));
#176999=CARTESIAN_POINT('Ctrl Pts',(12.1048235693023,57.6851306806978,40.1268999125508));
#177000=CARTESIAN_POINT('Ctrl Pts',(12.0875272507065,57.6955725063805,40.1162251288835));
#177001=CARTESIAN_POINT('Ctrl Pts',(12.0719688682374,57.7066970899018,40.1038990521418));
#177002=CARTESIAN_POINT('Ctrl Pts',(12.0641896770028,57.7122593816625,40.0977360137709));
#177003=CARTESIAN_POINT('Ctrl Pts',(12.0568449701609,57.7179923646567,40.0911601532641));
#177004=CARTESIAN_POINT('Ctrl Pts',(12.0499800630337,57.7238555234915,40.084220729064));
#177005=CARTESIAN_POINT('Ctrl Pts',(12.0431444860322,57.7296936321424,40.0773109533619));
#177006=CARTESIAN_POINT('Ctrl Pts',(12.0367843970379,57.7356606854447,40.0700409753048));
#177007=CARTESIAN_POINT('Ctrl Pts',(12.0309451958833,57.7417170494856,40.0624586415899));
#177008=CARTESIAN_POINT('Ctrl Pts',(12.0309201410117,57.7417430361607,40.0624261072769));
#177009=CARTESIAN_POINT('Ctrl Pts',(12.0308950952499,57.7417690242237,40.0623935677889));
#177010=CARTESIAN_POINT('Ctrl Pts',(12.030870058598,57.7417950136726,40.0623610231289));
#177011=CARTESIAN_POINT('Ctrl Pts',(12.0190632547928,57.7540511381831,40.0470135870234));
#177012=CARTESIAN_POINT('Ctrl Pts',(12.0092769601261,57.766578581356,40.0305755292094));
#177013=CARTESIAN_POINT('Ctrl Pts',(12.0014122714559,57.7792098558809,40.0133447567341));
#177014=CARTESIAN_POINT('Ctrl Pts',(11.9932614808867,57.7923006313193,39.99548716266));
#177015=CARTESIAN_POINT('Ctrl Pts',(11.9871745471191,57.805503794129,39.976776795432));
#177016=CARTESIAN_POINT('Ctrl Pts',(11.9830932952248,57.8186383015961,39.9575197577483));
#177017=CARTESIAN_POINT('Ctrl Pts',(11.9790702919525,57.8315853501707,39.9385375612009));
#177018=CARTESIAN_POINT('Ctrl Pts',(11.9769963969272,57.8444665749276,39.9190226977112));
#177019=CARTESIAN_POINT('Ctrl Pts',(11.976863511098,57.8571005080025,39.8992655451878));
#177020=CARTESIAN_POINT('Ctrl Pts',(11.9767708607335,57.8659091109222,39.8854905069341));
#177021=CARTESIAN_POINT('Ctrl Pts',(11.9776227396656,57.8745973526463,39.8715976051482));
#177022=CARTESIAN_POINT('Ctrl Pts',(11.9794294790618,57.8830978693154,39.8576902534424));
#177023=CARTESIAN_POINT('',(12.0535047649328,58.231611300478,39.2875012672119));
#177024=CARTESIAN_POINT('',(11.9794294790618,57.8830978693155,39.8576902534424));
#177025=CARTESIAN_POINT('',(6.53099325080115,59.1062911958296,39.2875012672119));
#177026=CARTESIAN_POINT('Origin',(5.53234440788222E-15,0.,39.2875012672119));
#177027=CARTESIAN_POINT('',(6.493746461128,58.7519447039088,39.8576902534424));
#177028=CARTESIAN_POINT('',(6.53099325080115,59.1062911958296,39.2875012672119));
#177029=CARTESIAN_POINT('',(6.17403490859079,58.596486683455,40.1599502534424));
#177030=CARTESIAN_POINT('Ctrl Pts',(6.493746461128,58.7519447039088,39.8576902534424));
#177031=CARTESIAN_POINT('Ctrl Pts',(6.49246793990594,58.7397817566363,39.8772619994027));
#177032=CARTESIAN_POINT('Ctrl Pts',(6.48928351037877,58.7278742924834,39.8967644650317));
#177033=CARTESIAN_POINT('Ctrl Pts',(6.484285135397,58.7163794573064,39.915928283597));
#177034=CARTESIAN_POINT('Ctrl Pts',(6.47919647150981,58.7046769834289,39.9354382707087));
#177035=CARTESIAN_POINT('Ctrl Pts',(6.47222767387013,58.6934012556437,39.9545987622235));
#177036=CARTESIAN_POINT('Ctrl Pts',(6.4634225916951,58.6827157580282,39.9731387498093));
#177037=CARTESIAN_POINT('Ctrl Pts',(6.45499029387005,58.672482656677,39.9908938023901));
#177038=CARTESIAN_POINT('Ctrl Pts',(6.4448734428978,58.6627901347998,40.0080810366013));
#177039=CARTESIAN_POINT('Ctrl Pts',(6.4330668970868,58.65379169843,40.024454274236));
#177040=CARTESIAN_POINT('Ctrl Pts',(6.42367635879233,58.6466346380439,40.0374770090369));
#177041=CARTESIAN_POINT('Ctrl Pts',(6.41321606634576,58.6399167088232,40.0499848769983));
#177042=CARTESIAN_POINT('Ctrl Pts',(6.40166487239094,58.6337244205832,40.0618424270192));
#177043=CARTESIAN_POINT('Ctrl Pts',(6.40163334138366,58.6337075176478,40.0618747942791));
#177044=CARTESIAN_POINT('Ctrl Pts',(6.40160180229542,58.6336906188003,40.0619071564124));
#177045=CARTESIAN_POINT('Ctrl Pts',(6.40157025512699,58.6336737240427,40.0619395134161));
#177046=CARTESIAN_POINT('Ctrl Pts',(6.39529021487377,58.6303105138593,40.0683807661799));
#177047=CARTESIAN_POINT('Ctrl Pts',(6.38865499943531,58.6271199258587,40.0746073439084));
#177048=CARTESIAN_POINT('Ctrl Pts',(6.38170181337843,58.6241179857776,40.0805869293669));
#177049=CARTESIAN_POINT('Ctrl Pts',(6.36790273412708,58.6181604277965,40.092453830807));
#177050=CARTESIAN_POINT('Ctrl Pts',(6.3528499811638,58.6129462715177,40.1033475319609));
#177051=CARTESIAN_POINT('Ctrl Pts',(6.33682633915184,58.6086032453499,40.1130129263075));
#177052=CARTESIAN_POINT('Ctrl Pts',(6.32480860764288,58.6053459757241,40.1202619720674));
#177053=CARTESIAN_POINT('Ctrl Pts',(6.31224475095164,58.6025787159787,40.1268200947266));
#177054=CARTESIAN_POINT('Ctrl Pts',(6.29925407013949,58.6003553628269,40.1325796782703));
#177055=CARTESIAN_POINT('Ctrl Pts',(6.29438256483494,58.599521605395,40.1347395220992));
#177056=CARTESIAN_POINT('Ctrl Pts',(6.28945103740996,58.5987643350183,40.1367870714852));
#177057=CARTESIAN_POINT('Ctrl Pts',(6.28446577922175,58.598086394715,40.1387166518767));
#177058=CARTESIAN_POINT('Ctrl Pts',(6.26701737556302,58.5957136036534,40.1454701832469));
#177059=CARTESIAN_POINT('Ctrl Pts',(6.24891076953115,58.5943126009391,40.1507785912491));
#177060=CARTESIAN_POINT('Ctrl Pts',(6.23041570798304,58.594005327233,40.1543986087265));
#177061=CARTESIAN_POINT('Ctrl Pts',(6.22116817720899,58.59385169038,40.1562086174652));
#177062=CARTESIAN_POINT('Ctrl Pts',(6.21182353266002,58.5939714867924,40.1575965292115));
#177063=CARTESIAN_POINT('Ctrl Pts',(6.20241549311822,58.5943799633642,40.1585319382567));
#177064=CARTESIAN_POINT('Ctrl Pts',(6.19771147334731,58.59458420165,40.1589996427793));
#177065=CARTESIAN_POINT('Ctrl Pts',(6.19299160483051,58.5948606100011,40.159354221642));
#177066=CARTESIAN_POINT('Ctrl Pts',(6.18826010244408,58.595211094569,40.159591874311));
#177067=CARTESIAN_POINT('Ctrl Pts',(6.18352860005764,58.5955615791369,40.1598295269801));
#177068=CARTESIAN_POINT('Ctrl Pts',(6.17878546397972,58.5959861416118,40.1599502506895));
#177069=CARTESIAN_POINT('Ctrl Pts',(6.17403490859079,58.596486683455,40.1599502534424));
#177070=CARTESIAN_POINT('',(6.14377718965381,58.5996668978648,40.1599502534424));
#177071=CARTESIAN_POINT('Origin',(5.66232193761676E-15,5.32046883722541E-15,
40.1599502534424));
#177072=CARTESIAN_POINT('',(5.86337364149639,58.8181995570484,39.8576902534424));
#177073=CARTESIAN_POINT('Ctrl Pts',(6.14377718965381,58.5996668978648,40.1599502534424));
#177074=CARTESIAN_POINT('Ctrl Pts',(6.13998815054745,58.6000641582629,40.1599502448875));
#177075=CARTESIAN_POINT('Ctrl Pts',(6.13621436696463,58.600507087875,40.1598743450437));
#177076=CARTESIAN_POINT('Ctrl Pts',(6.13245764560186,58.6009943991739,40.1597243308499));
#177077=CARTESIAN_POINT('Ctrl Pts',(6.11027824677019,58.6038714482306,40.1588386583938));
#177078=CARTESIAN_POINT('Ctrl Pts',(6.08869075055846,58.6082941124962,40.1553722553615));
#177079=CARTESIAN_POINT('Ctrl Pts',(6.06807370279885,58.6139972210824,40.1496902177782));
#177080=CARTESIAN_POINT('Ctrl Pts',(6.06037186006783,58.6161277126019,40.1475675976839));
#177081=CARTESIAN_POINT('Ctrl Pts',(6.05280507414665,58.6184367045764,40.1451361443093));
#177082=CARTESIAN_POINT('Ctrl Pts',(6.04539170794238,58.6209098557462,40.1424159447501));
#177083=CARTESIAN_POINT('Ctrl Pts',(6.0396074277374,58.6228395323549,40.1402935085949));
#177084=CARTESIAN_POINT('Ctrl Pts',(6.0339170209361,58.6248693309926,40.1379949176048));
#177085=CARTESIAN_POINT('Ctrl Pts',(6.02832968646008,58.6269926140963,40.1355293609261));
#177086=CARTESIAN_POINT('Ctrl Pts',(6.00877401579401,58.6344241049593,40.1268999125508));
#177087=CARTESIAN_POINT('Ctrl Pts',(5.99048098024888,58.6430007716254,40.1162251288835));
#177088=CARTESIAN_POINT('Ctrl Pts',(5.97384499260683,58.6524381197038,40.1038990521418));
#177089=CARTESIAN_POINT('Ctrl Pts',(5.9655269987858,58.657156793743,40.097736013771));
#177090=CARTESIAN_POINT('Ctrl Pts',(5.95762326711415,58.6620906399372,40.0911601532641));
#177091=CARTESIAN_POINT('Ctrl Pts',(5.95018309968352,58.6672041015819,40.084220729064));
#177092=CARTESIAN_POINT('Ctrl Pts',(5.9427747201624,58.6722957161032,40.0773109533618));
#177093=CARTESIAN_POINT('Ctrl Pts',(5.93582574548912,58.6775652709344,40.0700409753048));
#177094=CARTESIAN_POINT('Ctrl Pts',(5.92938546966327,58.682978094856,40.0624586415899));
#177095=CARTESIAN_POINT('Ctrl Pts',(5.92935783569764,58.6830013202262,40.0624261072769));
#177096=CARTESIAN_POINT('Ctrl Pts',(5.92933021064688,58.6830245479289,40.0623935677889));
#177097=CARTESIAN_POINT('Ctrl Pts',(5.92930259451122,58.683047777962,40.0623610231289));
#177098=CARTESIAN_POINT('Ctrl Pts',(5.91627935575158,58.6940026150826,40.047013587023));
#177099=CARTESIAN_POINT('Ctrl Pts',(5.90523719704731,58.7054384852687,40.0305755292086));
#177100=CARTESIAN_POINT('Ctrl Pts',(5.8960952642492,58.7171784805296,40.0133447567329));
#177101=CARTESIAN_POINT('Ctrl Pts',(5.88662076592385,58.7293455537182,39.9954871626582));
#177102=CARTESIAN_POINT('Ctrl Pts',(5.87918707069749,58.7418401303881,39.9767767954297));
#177103=CARTESIAN_POINT('Ctrl Pts',(5.87375524644688,58.7544760786607,39.9575197577455));
#177104=CARTESIAN_POINT('Ctrl Pts',(5.86840094651616,58.766931683599,39.9385375611976));
#177105=CARTESIAN_POINT('Ctrl Pts',(5.86499195787612,58.7795255625992,39.9190226977074));
#177106=CARTESIAN_POINT('Ctrl Pts',(5.86353919440024,58.7920763953157,39.8992655451834));
#177107=CARTESIAN_POINT('Ctrl Pts',(5.86252630185778,58.8008270591857,39.8854905069311));
#177108=CARTESIAN_POINT('Ctrl Pts',(5.86246534555215,58.8095567514073,39.8715976051467));
#177109=CARTESIAN_POINT('Ctrl Pts',(5.86337364149639,58.8181995570484,39.8576902534424));
#177110=CARTESIAN_POINT('',(5.90061356181316,59.1725467709677,39.2875012672119));
#177111=CARTESIAN_POINT('',(5.86337364149639,58.8181995570484,39.8576902534424));
#177112=CARTESIAN_POINT('',(0.316925998273675,59.4651754363832,39.2875012672119));
#177113=CARTESIAN_POINT('Origin',(5.53234440788222E-15,0.,39.2875012672119));
#177114=CARTESIAN_POINT('',(0.316922544676313,59.1088767419348,39.8576902534424));
#177115=CARTESIAN_POINT('',(0.316925998273675,59.4651754363832,39.2875012672119));
#177116=CARTESIAN_POINT('Ctrl Pts',(0.316922544676314,59.1088767419348,
39.8576902534424));
#177117=CARTESIAN_POINT('Ctrl Pts',(0.316922401514489,59.0966467826992,
39.8772619994065));
#177118=CARTESIAN_POINT('Ctrl Pts',(0.31500008555408,59.0844716853536,39.8967644650393));
#177119=CARTESIAN_POINT('Ctrl Pts',(0.311230629648603,59.0725173476285,
39.9159282836081));
#177120=CARTESIAN_POINT('Ctrl Pts',(0.307393083604025,59.0603470709089,
39.9354382707235));
#177121=CARTESIAN_POINT('Ctrl Pts',(0.301641096262377,59.04840467503,39.9545987622418));
#177122=CARTESIAN_POINT('Ctrl Pts',(0.294001187890843,59.0368573319778,
39.9731387498307));
#177123=CARTESIAN_POINT('Ctrl Pts',(0.2866847334314,59.0257988734911,39.9908938024147));
#177124=CARTESIAN_POINT('Ctrl Pts',(0.27763644804072,59.0151019493759,40.0080810366287));
#177125=CARTESIAN_POINT('Ctrl Pts',(0.266835172444231,59.0049186872905,
40.0244542742656));
#177126=CARTESIAN_POINT('Ctrl Pts',(0.258244193029575,58.9968192554995,
40.0374770090559));
#177127=CARTESIAN_POINT('Ctrl Pts',(0.24854341798377,58.9890447295094,40.0499848770073));
#177128=CARTESIAN_POINT('Ctrl Pts',(0.237702773060119,58.981678934725,40.0618424270193));
#177129=CARTESIAN_POINT('Ctrl Pts',(0.237673181620862,58.9816588284979,
40.0618747942791));
#177130=CARTESIAN_POINT('Ctrl Pts',(0.237643581717602,58.9816387254916,
40.0619071564124));
#177131=CARTESIAN_POINT('Ctrl Pts',(0.237613973350917,58.9816186257082,
40.0619395134161));
#177132=CARTESIAN_POINT('Ctrl Pts',(0.231719887007412,58.9776173965852,
40.0683807661799));
#177133=CARTESIAN_POINT('Ctrl Pts',(0.225454527233989,58.9737507180862,
40.0746073439084));
#177134=CARTESIAN_POINT('Ctrl Pts',(0.218853219641359,58.9700384170936,
40.0805869293669));
#177135=CARTESIAN_POINT('Ctrl Pts',(0.205752467570556,58.9626710986899,
40.092453830807));
#177136=CARTESIAN_POINT('Ctrl Pts',(0.191327202906059,58.9559120649696,
40.1033475319609));
#177137=CARTESIAN_POINT('Ctrl Pts',(0.175845309932877,58.9499179036781,
40.1130129263075));
#177138=CARTESIAN_POINT('Ctrl Pts',(0.16423389020299,58.9454222827095,40.1202619720674));
#177139=CARTESIAN_POINT('Ctrl Pts',(0.152028117041927,58.9413569016699,
40.1268200947266));
#177140=CARTESIAN_POINT('Ctrl Pts',(0.139341004226766,58.9377878323772,
40.1325796782703));
#177141=CARTESIAN_POINT('Ctrl Pts',(0.134583336921081,58.9364494313924,
40.1347395220992));
#177142=CARTESIAN_POINT('Ctrl Pts',(0.12975798122809,58.9351808244388,40.1367870714852));
#177143=CARTESIAN_POINT('Ctrl Pts',(0.124870896863944,58.933985496586,40.1387166518767));
#177144=CARTESIAN_POINT('Ctrl Pts',(0.107766101589435,58.9298018491012,
40.1454701832469));
#177145=CARTESIAN_POINT('Ctrl Pts',(0.0899051301006875,58.9265158655229,
40.1507785912492));
#177146=CARTESIAN_POINT('Ctrl Pts',(0.0715435052832107,58.9242770147326,
40.1543986087265));
#177147=CARTESIAN_POINT('Ctrl Pts',(0.0623626928744723,58.9231575893375,
40.1562086174652));
#177148=CARTESIAN_POINT('Ctrl Pts',(0.053056717131196,58.9222999481582,
40.1575965292115));
#177149=CARTESIAN_POINT('Ctrl Pts',(0.0436575183860504,58.9217227791369,
40.1585319382567));
#177150=CARTESIAN_POINT('Ctrl Pts',(0.0389579190134777,58.9214341946262,
40.1589996427793));
#177151=CARTESIAN_POINT('Ctrl Pts',(0.0342350138900817,58.9212157281805,
40.159354221642));
#177152=CARTESIAN_POINT('Ctrl Pts',(0.029492795555506,58.9210697160839,
40.159591874311));
#177153=CARTESIAN_POINT('Ctrl Pts',(0.0247505772209303,58.9209237039872,
40.1598295269801));
#177154=CARTESIAN_POINT('Ctrl Pts',(0.0199890456756627,58.9208501479391,
40.1599502506895));
#177155=CARTESIAN_POINT('Ctrl Pts',(0.0152121934565431,58.9208513795073,
40.1599502534424));
#177156=CARTESIAN_POINT('',(-0.316922544675064,59.1088767419348,39.8576902534424));
#177157=CARTESIAN_POINT('Ctrl Pts',(-0.015212193455297,58.9208513795073,
40.1599502534424));
#177158=CARTESIAN_POINT('Ctrl Pts',(-0.0190220008279198,58.9208504012364,
40.1599502448875));
#177159=CARTESIAN_POINT('Ctrl Pts',(-0.0228214099810991,58.9208964366351,
40.1598743450437));
#177160=CARTESIAN_POINT('Ctrl Pts',(-0.0266084895323811,58.9209883940807,
40.1597243308499));
#177161=CARTESIAN_POINT('Ctrl Pts',(-0.0489671208125404,58.9215313038856,
40.1588386583938));
#177162=CARTESIAN_POINT('Ctrl Pts',(-0.0708986527598547,58.9236732325286,
40.1553722553617));
#177163=CARTESIAN_POINT('Ctrl Pts',(-0.0919988953503987,58.9271900305696,
40.1496902177787));
#177164=CARTESIAN_POINT('Ctrl Pts',(-0.0998812435862781,58.9285037892488,
40.1475675976843));
#177165=CARTESIAN_POINT('Ctrl Pts',(-0.107647933245904,58.9300091878196,
40.1451361443095));
#177166=CARTESIAN_POINT('Ctrl Pts',(-0.115279202946265,58.9316938830317,
40.1424159447501));
#177167=CARTESIAN_POINT('Ctrl Pts',(-0.12123350238957,58.933008366749,40.1402935085949));
#177168=CARTESIAN_POINT('Ctrl Pts',(-0.127104908279362,58.9344322364591,
40.1379949176048));
#177169=CARTESIAN_POINT('Ctrl Pts',(-0.132883578272425,58.9359598525093,
40.1355293609261));
#177170=CARTESIAN_POINT('Ctrl Pts',(-0.153108923248145,58.9413065086849,
40.1268999125509));
#177171=CARTESIAN_POINT('Ctrl Pts',(-0.172198253417083,58.9479240485795,
40.1162251288835));
#177172=CARTESIAN_POINT('Ctrl Pts',(-0.189729578870145,58.9555707636545,
40.1038990521418));
#177173=CARTESIAN_POINT('Ctrl Pts',(-0.198495241596676,58.959394121192,
40.097736013771));
#177174=CARTESIAN_POINT('Ctrl Pts',(-0.206871403159924,58.9634747743348,
40.0911601532641));
#177175=CARTESIAN_POINT('Ctrl Pts',(-0.214805314862589,58.9677825146336,
40.084220729064));
#177176=CARTESIAN_POINT('Ctrl Pts',(-0.222705329147007,58.9720718502312,
40.0773109533618));
#177177=CARTESIAN_POINT('Ctrl Pts',(-0.230167055078556,58.9765861722458,
40.0700409753047));
#177178=CARTESIAN_POINT('Ctrl Pts',(-0.237137844566028,58.9812961520165,
40.0624586415899));
#177179=CARTESIAN_POINT('Ctrl Pts',(-0.23716775486217,58.9813163616197,
40.0624261072769));
#177180=CARTESIAN_POINT('Ctrl Pts',(-0.237197656536078,58.9813365744745,
40.0623935677888));
#177181=CARTESIAN_POINT('Ctrl Pts',(-0.237227549587329,58.9813567905789,
40.0623610231288));
#177182=CARTESIAN_POINT('Ctrl Pts',(-0.251324537971654,58.990890316821,
40.0470135870233));
#177183=CARTESIAN_POINT('Ctrl Pts',(-0.263501580511648,59.0011093202329,
40.0305755292093));
#177184=CARTESIAN_POINT('Ctrl Pts',(-0.273820596508607,59.0118294103845,
40.0133447567339));
#177185=CARTESIAN_POINT('Ctrl Pts',(-0.284514998003514,59.0229394763226,
39.9954871626597));
#177186=CARTESIAN_POINT('Ctrl Pts',(-0.293214009568045,59.0345885736555,
39.9767767954317));
#177187=CARTESIAN_POINT('Ctrl Pts',(-0.299936893971955,59.0465875206394,
39.9575197577479));
#177188=CARTESIAN_POINT('Ctrl Pts',(-0.306563827730748,59.0584152157268,
39.9385375612004));
#177189=CARTESIAN_POINT('Ctrl Pts',(-0.311270560392914,59.070583767796,
39.9190226977105));
#177190=CARTESIAN_POINT('Ctrl Pts',(-0.314027284735234,59.0829139906038,
39.899265545187));
#177191=CARTESIAN_POINT('Ctrl Pts',(-0.315949321993608,59.0915108413214,
39.8854905069335));
#177192=CARTESIAN_POINT('Ctrl Pts',(-0.316922445687103,59.1001863397073,
39.8715976051479));
#177193=CARTESIAN_POINT('Ctrl Pts',(-0.316922544675064,59.1088767419348,
39.8576902534424));
#177194=CARTESIAN_POINT('',(-0.316925998272418,59.4651754363832,39.2875012672119));
#177195=CARTESIAN_POINT('',(-0.316922544675064,59.1088767419348,39.8576902534424));
#177196=CARTESIAN_POINT('',(-5.90061356181196,59.1725467709678,39.2875012672119));
#177197=CARTESIAN_POINT('Origin',(5.53234440788222E-15,0.,39.2875012672119));
#177198=CARTESIAN_POINT('',(-5.8633736414952,58.8181995570485,39.8576902534424));
#177199=CARTESIAN_POINT('',(-5.90061356181196,59.1725467709678,39.2875012672119));
#177200=CARTESIAN_POINT('',(-6.14377718965262,58.5996668978649,40.1599502534424));
#177201=CARTESIAN_POINT('Ctrl Pts',(-5.8633736414952,58.8181995570485,39.8576902534424));
#177202=CARTESIAN_POINT('Ctrl Pts',(-5.86209540502807,58.8060365798455,
39.8772619994052));
#177203=CARTESIAN_POINT('Ctrl Pts',(-5.86273454612467,58.7937272422247,
39.8967644650367));
#177204=CARTESIAN_POINT('Ctrl Pts',(-5.8652337840041,58.7814443761802,39.9159282836043));
#177205=CARTESIAN_POINT('Ctrl Pts',(-5.86777816724645,58.7689396367198,
39.9354382707185));
#177206=CARTESIAN_POINT('Ctrl Pts',(-5.87225032431001,58.7564614161383,
39.9545987622357));
#177207=CARTESIAN_POINT('Ctrl Pts',(-5.87864135443915,58.7441787427587,
39.9731387498236));
#177208=CARTESIAN_POINT('Ctrl Pts',(-5.88476180492296,58.7324160859241,
39.9908938024066));
#177209=CARTESIAN_POINT('Ctrl Pts',(-5.89264238981903,58.7208319573121,
40.0080810366197));
#177210=CARTESIAN_POINT('Ctrl Pts',(-5.9023200541595,58.709575439463,40.024454274256));
#177211=CARTESIAN_POINT('Ctrl Pts',(-5.91001735013293,58.7006223753283,
40.0374770090498));
#177212=CARTESIAN_POINT('Ctrl Pts',(-5.91885232406554,58.6918764318948,
40.0499848770044));
#177213=CARTESIAN_POINT('Ctrl Pts',(-5.92886364759493,58.6834178317481,
40.0618424270193));
#177214=CARTESIAN_POINT('Ctrl Pts',(-5.92889097525616,58.6833947425173,
40.0618747942791));
#177215=CARTESIAN_POINT('Ctrl Pts',(-5.9289183116717,58.683371655605,40.0619071564124));
#177216=CARTESIAN_POINT('Ctrl Pts',(-5.92894565684118,58.6833485710132,
40.0619395134161));
#177217=CARTESIAN_POINT('Ctrl Pts',(-5.93438921243158,58.6787531612542,
40.0683807661799));
#177218=CARTESIAN_POINT('Ctrl Pts',(-5.94021607194716,58.6742527563957,
40.0746073439084));
#177219=CARTESIAN_POINT('Ctrl Pts',(-5.94639317576815,58.6698707672381,
40.0805869293669));
#177220=CARTESIAN_POINT('Ctrl Pts',(-5.95865206607721,58.6611744062939,
40.092453830807));
#177221=CARTESIAN_POINT('Ctrl Pts',(-5.97229179622457,58.6529445485199,
40.1033475319609));
#177222=CARTESIAN_POINT('Ctrl Pts',(-5.98706231729977,58.6453649253901,
40.1130129263075));
#177223=CARTESIAN_POINT('Ctrl Pts',(-5.99814020810617,58.6396802080428,
40.1202619720675));
#177224=CARTESIAN_POINT('Ctrl Pts',(-6.00985416873208,58.6343612468744,
40.1268200947266));
#177225=CARTESIAN_POINT('Ctrl Pts',(-6.02209871088731,58.6294855649109,
40.1325796782703));
#177226=CARTESIAN_POINT('Ctrl Pts',(-6.02669041419551,58.6276571841746,
40.1347395220992));
#177227=CARTESIAN_POINT('Ctrl Pts',(-6.03135673054978,58.6258911397673,
40.1367870714852));
#177228=CARTESIAN_POINT('Ctrl Pts',(-6.03609209717088,58.6241915206271,
40.1387166518767));
#177229=CARTESIAN_POINT('Ctrl Pts',(-6.05266588034473,58.6182428536364,
40.1454701832469));
#177230=CARTESIAN_POINT('Ctrl Pts',(-6.07008552874908,58.6131078911177,
40.1507785912492));
#177231=CARTESIAN_POINT('Ctrl Pts',(-6.088112543032,58.6089619925611,40.1543986087265));
#177232=CARTESIAN_POINT('Ctrl Pts',(-6.09712605017347,58.6068890432828,
40.1562086174652));
#177233=CARTESIAN_POINT('Ctrl Pts',(-6.10629139889341,58.6050633610079,
40.1575965292115));
#177234=CARTESIAN_POINT('Ctrl Pts',(-6.11557877725353,58.6035068699781,
40.1585319382567));
#177235=CARTESIAN_POINT('Ctrl Pts',(-6.12022246643359,58.6027286244632,
40.1589996427793));
#177236=CARTESIAN_POINT('Ctrl Pts',(-6.12489666302671,58.6020176767849,
40.159354221642));
#177237=CARTESIAN_POINT('Ctrl Pts',(-6.12959764057299,58.6013767677628,
40.159591874311));
#177238=CARTESIAN_POINT('Ctrl Pts',(-6.13429861811926,58.6007358587407,
40.1598295269801));
#177239=CARTESIAN_POINT('Ctrl Pts',(-6.13902637679584,58.6001649900651,
40.1599502506895));
#177240=CARTESIAN_POINT('Ctrl Pts',(-6.14377718965262,58.5996668978649,
40.1599502534424));
#177241=CARTESIAN_POINT('',(-6.17403490858961,58.5964866834551,40.1599502534424));
#177242=CARTESIAN_POINT('Origin',(3.95370119046988E-16,6.77609428042844E-17,
40.1599502534424));
#177243=CARTESIAN_POINT('',(-6.49374646112681,58.7519447039089,39.8576902534424));
#177244=CARTESIAN_POINT('Ctrl Pts',(-6.17403490858961,58.5964866834551,
40.1599502534424));
#177245=CARTESIAN_POINT('Ctrl Pts',(-6.17782374318166,58.5960874772333,
40.1599502448875));
#177246=CARTESIAN_POINT('Ctrl Pts',(-6.18160715078344,58.5957361140451,
40.1598743450437));
#177247=CARTESIAN_POINT('Ctrl Pts',(-6.18538309648717,58.5954317101325,
40.1597243308499));
#177248=CARTESIAN_POINT('Ctrl Pts',(-6.20767599437464,58.5936345324521,
40.1588386583938));
#177249=CARTESIAN_POINT('Ctrl Pts',(-6.22971127560594,58.5934722580544,
40.1553722553613));
#177250=CARTESIAN_POINT('Ctrl Pts',(-6.25106353435582,58.5947642147755,
40.1496902177777));
#177251=CARTESIAN_POINT('Ctrl Pts',(-6.2590400274379,58.595246846799,40.1475675976836));
#177252=CARTESIAN_POINT('Ctrl Pts',(-6.26692152735692,58.5959321585041,
40.1451361443091));
#177253=CARTESIAN_POINT('Ctrl Pts',(-6.2746870907638,58.5968099398849,40.1424159447501));
#177254=CARTESIAN_POINT('Ctrl Pts',(-6.2807461728947,58.5974948289522,40.1402935085949));
#177255=CARTESIAN_POINT('Ctrl Pts',(-6.28673424952138,58.5982971695202,
40.1379949176048));
#177256=CARTESIAN_POINT('Ctrl Pts',(-6.29264094271378,58.5992123816357,
40.1355293609261));
#177257=CARTESIAN_POINT('Ctrl Pts',(-6.31331436888716,58.6024156240399,
40.1268999125509));
#177258=CARTESIAN_POINT('Ctrl Pts',(-6.33299084698388,58.6070015340112,
40.1162251288835));
#177259=CARTESIAN_POINT('Ctrl Pts',(-6.35122543337761,58.6127738370723,
40.1038990521418));
#177260=CARTESIAN_POINT('Ctrl Pts',(-6.36034272657447,58.6156599886029,
40.097736013771));
#177261=CARTESIAN_POINT('Ctrl Pts',(-6.36909954705041,58.6188427402045,
40.0911601532641));
#177262=CARTESIAN_POINT('Ctrl Pts',(-6.37744027742822,58.6222975626533,
40.084220729064));
#177263=CARTESIAN_POINT('Ctrl Pts',(-6.38574537226625,58.6257376244687,
40.0773109533618));
#177264=CARTESIAN_POINT('Ctrl Pts',(-6.3936380972253,58.62944725381,40.0700409753048));
#177265=CARTESIAN_POINT('Ctrl Pts',(-6.40106302694604,58.6334027859058,
40.0624586415899));
#177266=CARTESIAN_POINT('Ctrl Pts',(-6.40109488586922,58.6334197583214,
40.0624261072769));
#177267=CARTESIAN_POINT('Ctrl Pts',(-6.40112673655728,58.633436734872,40.0623935677888));
#177268=CARTESIAN_POINT('Ctrl Pts',(-6.40115857900959,58.6334537155558,
40.0623610231288));
#177269=CARTESIAN_POINT('Ctrl Pts',(-6.41617486746443,58.6414614796112,
40.0470135870231));
#177270=CARTESIAN_POINT('Ctrl Pts',(-6.42935337961428,58.6503516547095,
40.0305755292087));
#177271=CARTESIAN_POINT('Ctrl Pts',(-6.44073642151171,58.6599343882012,
40.013344756733));
#177272=CARTESIAN_POINT('Ctrl Pts',(-6.45253355607573,58.6698657226821,
39.9954871626584));
#177273=CARTESIAN_POINT('Ctrl Pts',(-6.46240257578747,58.6805417107303,
39.97677679543));
#177274=CARTESIAN_POINT('Ctrl Pts',(-6.47034286301626,58.6917721934519,
39.9575197577459));
#177275=CARTESIAN_POINT('Ctrl Pts',(-6.47816982452998,58.7028423919863,
39.9385375611982));
#177276=CARTESIAN_POINT('Ctrl Pts',(-6.48412273326605,58.714452295922,39.9190226977081));
#177277=CARTESIAN_POINT('Ctrl Pts',(-6.48815321522567,58.7264268163201,
39.8992655451843));
#177278=CARTESIAN_POINT('Ctrl Pts',(-6.49096333895696,58.7347756649885,
39.8854905069317));
#177279=CARTESIAN_POINT('Ctrl Pts',(-6.4928379682912,58.7433019189617,39.871597605147));
#177280=CARTESIAN_POINT('Ctrl Pts',(-6.49374646112681,58.7519447039089,
39.8576902534424));
#177281=CARTESIAN_POINT('',(-6.53099325079995,59.1062911958297,39.2875012672119));
#177282=CARTESIAN_POINT('',(-6.49374646112681,58.7519447039089,39.8576902534424));
#177283=CARTESIAN_POINT('',(-12.0535047649316,58.2316113004782,39.2875012672119));
#177284=CARTESIAN_POINT('Origin',(5.53234440788222E-15,0.,39.2875012672119));
#177285=CARTESIAN_POINT('',(-11.9794294790606,57.8830978693157,39.8576902534424));
#177286=CARTESIAN_POINT('',(-12.0535047649316,58.2316113004782,39.2875012672119));
#177287=CARTESIAN_POINT('',(-12.2354540642039,57.6364522029208,40.1599502534424));
#177288=CARTESIAN_POINT('Ctrl Pts',(-11.9794294790606,57.8830978693157,
39.8576902534424));
#177289=CARTESIAN_POINT('Ctrl Pts',(-11.9768868675907,57.8711351342676,
39.877261999406));
#177290=CARTESIAN_POINT('Ctrl Pts',(-11.9762358312602,57.858826420049,39.8967644650382));
#177291=CARTESIAN_POINT('Ctrl Pts',(-11.9774374689411,57.8463495993345,
39.9159282836066));
#177292=CARTESIAN_POINT('Ctrl Pts',(-11.9786608125867,57.8336474016745,
39.9354382707215));
#177293=CARTESIAN_POINT('Ctrl Pts',(-11.9818041414845,57.8207700703852,
39.9545987622393));
#177294=CARTESIAN_POINT('Ctrl Pts',(-11.9868762719092,57.8078866382169,
39.9731387498279));
#177295=CARTESIAN_POINT('Ctrl Pts',(-11.9917336614825,57.7955486571631,
39.9908938024114));
#177296=CARTESIAN_POINT('Ctrl Pts',(-11.9983602045484,57.7832042421904,
40.0080810366251));
#177297=CARTESIAN_POINT('Ctrl Pts',(-12.0068082271193,57.770997797342,40.0244542742617));
#177298=CARTESIAN_POINT('Ctrl Pts',(-12.0135275064638,57.7612891925114,
40.0374770090534));
#177299=CARTESIAN_POINT('Ctrl Pts',(-12.0213998814569,57.7516676540244,
40.0499848770061));
#177300=CARTESIAN_POINT('Ctrl Pts',(-12.0304721974324,57.7422089227119,
40.0618424270193));
#177301=CARTESIAN_POINT('Ctrl Pts',(-12.030496961908,57.7421831034479,40.0618747942791));
#177302=CARTESIAN_POINT('Ctrl Pts',(-12.0305217353323,57.7421572855746,
40.0619071564124));
#177303=CARTESIAN_POINT('Ctrl Pts',(-12.0305465177052,57.7421314690941,
40.0619395134161));
#177304=CARTESIAN_POINT('Ctrl Pts',(-12.0354799018083,57.73699222697,40.0683807661799));
#177305=CARTESIAN_POINT('Ctrl Pts',(-12.0408044207739,57.7319074031293,
40.0746073439084));
#177306=CARTESIAN_POINT('Ctrl Pts',(-12.0464896431811,57.726903735797,40.0805869293669));
#177307=CARTESIAN_POINT('Ctrl Pts',(-12.0577723607609,57.7169736114625,
40.092453830807));
#177308=CARTESIAN_POINT('Ctrl Pts',(-12.0704771166533,57.7073630976789,
40.1033475319609));
#177309=CARTESIAN_POINT('Ctrl Pts',(-12.0843744369107,57.698281056648,40.1130129263075));
#177310=CARTESIAN_POINT('Ctrl Pts',(-12.0947974271037,57.6914695258749,
40.1202619720674));
#177311=CARTESIAN_POINT('Ctrl Pts',(-12.1058912345906,57.6849552602294,
40.1268200947266));
#177312=CARTESIAN_POINT('Ctrl Pts',(-12.1175590523197,57.6788263845869,
40.1325796782703));
#177313=CARTESIAN_POINT('Ctrl Pts',(-12.1219344839681,57.6765280562209,
40.1347395220992));
#177314=CARTESIAN_POINT('Ctrl Pts',(-12.1263906358452,57.674283923512,40.1367870714852));
#177315=CARTESIAN_POINT('Ctrl Pts',(-12.1309224030556,57.6720986344674,
40.1387166518767));
#177316=CARTESIAN_POINT('Ctrl Pts',(-12.146783588292,57.6644501228112,40.1454701832469));
#177317=CARTESIAN_POINT('Ctrl Pts',(-12.1635710602988,57.6575224410761,
40.1507785912492));
#177318=CARTESIAN_POINT('Ctrl Pts',(-12.1810659563062,57.6515149180853,
40.1543986087265));
#177319=CARTESIAN_POINT('Ctrl Pts',(-12.18981340431,57.6485111565899,40.1562086174652));
#177320=CARTESIAN_POINT('Ctrl Pts',(-12.1987377085281,57.6457374357765,
40.1575965292115));
#177321=CARTESIAN_POINT('Ctrl Pts',(-12.2078115120423,57.6432186759797,
40.1585319382567));
#177322=CARTESIAN_POINT('Ctrl Pts',(-12.2123484137995,57.6419592960812,
40.1589996427793));
#177323=CARTESIAN_POINT('Ctrl Pts',(-12.2169226903863,57.6407636564618,
40.159354221642));
#177324=CARTESIAN_POINT('Ctrl Pts',(-12.2215309222505,57.6396348724476,
40.159591874311));
#177325=CARTESIAN_POINT('Ctrl Pts',(-12.2261391541148,57.6385060884334,
40.1598295269801));
#177326=CARTESIAN_POINT('Ctrl Pts',(-12.2307813416093,57.637444161687,40.1599502506895));
#177327=CARTESIAN_POINT('Ctrl Pts',(-12.2354540642039,57.6364522029208,
40.1599502534424));
#177328=CARTESIAN_POINT('',(-12.2652136052655,57.6301266171959,40.1599502534424));
#177329=CARTESIAN_POINT('Origin',(3.88326186679512E-16,6.66452935185788E-17,
40.1599502534424));
#177330=CARTESIAN_POINT('',(-12.5994235324466,57.7513140650721,39.8576902534424));
#177331=CARTESIAN_POINT('Ctrl Pts',(-12.2652136052655,57.6301266171959,
40.1599502534424));
#177332=CARTESIAN_POINT('Ctrl Pts',(-12.2689399558123,57.62933355681,40.1599502448875));
#177333=CARTESIAN_POINT('Ctrl Pts',(-12.2726659100573,57.6285886446436,
40.1598743450437));
#177334=CARTESIAN_POINT('Ctrl Pts',(-12.2763893518622,57.6278912144857,
40.1597243308499));
#177335=CARTESIAN_POINT('Ctrl Pts',(-12.2983722706983,57.6237736395753,
40.1588386583939));
#177336=CARTESIAN_POINT('Ctrl Pts',(-12.3202698780569,57.6213089400491,
40.1553722553623));
#177337=CARTESIAN_POINT('Ctrl Pts',(-12.3416402131471,57.6203619005013,
40.1496902177801));
#177338=CARTESIAN_POINT('Ctrl Pts',(-12.3496234589522,57.6200081180517,
40.1475675976854));
#177339=CARTESIAN_POINT('Ctrl Pts',(-12.3575334177724,57.6198658344726,
40.1451361443101));
#177340=CARTESIAN_POINT('Ctrl Pts',(-12.3653481937521,57.6199270848659,
40.1424159447501));
#177341=CARTESIAN_POINT('Ctrl Pts',(-12.3714456739989,57.6199748754953,
40.1402935085949));
#177342=CARTESIAN_POINT('Ctrl Pts',(-12.3774848147418,57.6201468963099,
40.1379949176048));
#177343=CARTESIAN_POINT('Ctrl Pts',(-12.3834548161669,57.6204396772353,
40.1355293609261));
#177344=CARTESIAN_POINT('Ctrl Pts',(-12.4043498211546,57.6214644104741,
40.1268999125509));
#177345=CARTESIAN_POINT('Ctrl Pts',(-12.4243978675675,57.6239684463328,
40.1162251288835));
#177346=CARTESIAN_POINT('Ctrl Pts',(-12.4431359329575,57.6278030948197,
40.1038990521418));
#177347=CARTESIAN_POINT('Ctrl Pts',(-12.4525049656526,57.6297204190632,
40.0977360137709));
#177348=CARTESIAN_POINT('Ctrl Pts',(-12.4615465034836,57.6319703982311,
40.0911601532641));
#177349=CARTESIAN_POINT('Ctrl Pts',(-12.4702026697491,57.634534451072,40.084220729064));
#177350=CARTESIAN_POINT('Ctrl Pts',(-12.4788218527838,57.6370875490682,
40.0773109533618));
#177351=CARTESIAN_POINT('Ctrl Pts',(-12.487059102424,57.6399518422609,40.0700409753047));
#177352=CARTESIAN_POINT('Ctrl Pts',(-12.4948568232942,57.6431095890444,
40.0624586415899));
#177353=CARTESIAN_POINT('Ctrl Pts',(-12.4948902817914,57.6431231383191,
40.0624261072769));
#177354=CARTESIAN_POINT('Ctrl Pts',(-12.4949237325308,57.6431366925669,
40.0623935677888));
#177355=CARTESIAN_POINT('Ctrl Pts',(-12.4949571755116,57.6431502517861,
40.0623610231288));
#177356=CARTESIAN_POINT('Ctrl Pts',(-12.5107282424363,57.6495445189153,
40.0470135870247));
#177357=CARTESIAN_POINT('Ctrl Pts',(-12.5247638376576,57.6570084630801,
40.0305755292122));
#177358=CARTESIAN_POINT('Ctrl Pts',(-12.5370861904653,57.6653488494772,
40.0133447567385));
#177359=CARTESIAN_POINT('Ctrl Pts',(-12.5498568062223,57.6739926427205,
39.995487162666));
#177360=CARTESIAN_POINT('Ctrl Pts',(-12.5607877070354,57.6835785531235,
39.9767767954399));
#177361=CARTESIAN_POINT('Ctrl Pts',(-12.5698584016403,57.6939175280623,
39.9575197577581));
#177362=CARTESIAN_POINT('Ctrl Pts',(-12.5787996370807,57.7041089426304,
39.9385375612124));
#177363=CARTESIAN_POINT('Ctrl Pts',(-12.5859335005772,57.715032997894,39.9190226977244));
#177364=CARTESIAN_POINT('Ctrl Pts',(-12.5911935813512,57.7265206205295,
39.8992655452027));
#177365=CARTESIAN_POINT('Ctrl Pts',(-12.5948610032545,57.7345299954194,
39.8854905069441));
#177366=CARTESIAN_POINT('Ctrl Pts',(-12.5976165994001,57.7428135895614,
39.8715976051532));
#177367=CARTESIAN_POINT('Ctrl Pts',(-12.5994235324466,57.7513140650721,
39.8576902534424));
#177368=CARTESIAN_POINT('',(-12.6735055745735,58.0998260601481,39.2875012672119));
#177369=CARTESIAN_POINT('',(-12.5994235324466,57.7513140650721,39.8576902534424));
#177370=CARTESIAN_POINT('',(-18.0743352474886,56.6526781108325,39.2875012672119));
#177371=CARTESIAN_POINT('Origin',(5.53234440788222E-15,0.,39.2875012672119));
#177372=CARTESIAN_POINT('',(-17.9642361803967,56.3138168485097,39.8576902534424));
#177373=CARTESIAN_POINT('',(-18.0743352474886,56.6526781108325,39.2875012672119));
#177374=CARTESIAN_POINT('',(-18.1930767435944,56.0417604764385,40.1599502534424));
#177375=CARTESIAN_POINT('Ctrl Pts',(-17.9642361803967,56.3138168485097,
39.8576902534424));
#177376=CARTESIAN_POINT('Ctrl Pts',(-17.9604570513079,56.3021854218463,
39.8772619994045));
#177377=CARTESIAN_POINT('Ctrl Pts',(-17.9585229704406,56.2900121878802,
39.8967644650353));
#177378=CARTESIAN_POINT('Ctrl Pts',(-17.9584138425285,56.2774781111558,
39.9159282836022));
#177379=CARTESIAN_POINT('Ctrl Pts',(-17.9583027433679,56.2647176232334,
39.9354382707156));
#177380=CARTESIAN_POINT('Ctrl Pts',(-17.9600828051299,56.2515822679742,
39.9545987622319));
#177381=CARTESIAN_POINT('Ctrl Pts',(-17.9637804645262,56.2382392305978,
39.973138749819));
#177382=CARTESIAN_POINT('Ctrl Pts',(-17.9673215746108,56.225461102829,39.990893802401));
#177383=CARTESIAN_POINT('Ctrl Pts',(-17.9726214740521,56.212491649491,40.0080810366132));
#177384=CARTESIAN_POINT('Ctrl Pts',(-17.9797472965476,56.199469014009,40.0244542742487));
#177385=CARTESIAN_POINT('Ctrl Pts',(-17.9854149414345,56.189111237984,40.0374770090451));
#177386=CARTESIAN_POINT('Ctrl Pts',(-17.9922384661032,56.1787195200277,
40.0499848770022));
#177387=CARTESIAN_POINT('Ctrl Pts',(-18.0002723763367,56.1683642893844,
40.0618424270193));
#177388=CARTESIAN_POINT('Ctrl Pts',(-18.0002943063019,56.1683360229685,
40.0618747942791));
#177389=CARTESIAN_POINT('Ctrl Pts',(-18.0003162453122,56.1683077570002,
40.0619071564124));
#177390=CARTESIAN_POINT('Ctrl Pts',(-18.0003381933676,56.1682794914817,
40.0619395134161));
#177391=CARTESIAN_POINT('Ctrl Pts',(-18.0047073547949,56.1626527236047,
40.0683807661799));
#177392=CARTESIAN_POINT('Ctrl Pts',(-18.0094711966663,56.1570391911759,
40.0746073439084));
#177393=CARTESIAN_POINT('Ctrl Pts',(-18.0146022491734,56.1514686668952,
40.0805869293669));
#177394=CARTESIAN_POINT('Ctrl Pts',(-18.024785178209,56.1404135756908,40.092453830807));
#177395=CARTESIAN_POINT('Ctrl Pts',(-18.0364157638823,56.1295277006976,
40.1033475319609));
#177396=CARTESIAN_POINT('Ctrl Pts',(-18.049287621373,56.1190427465077,40.1130129263075));
#177397=CARTESIAN_POINT('Ctrl Pts',(-18.0589415144909,56.1111790308654,
40.1202619720674));
#177398=CARTESIAN_POINT('Ctrl Pts',(-18.0692936227623,56.1035408324002,
40.1268200947266));
#177399=CARTESIAN_POINT('Ctrl Pts',(-18.0802568810126,56.0962259123229,
40.1325796782703));
#177400=CARTESIAN_POINT('Ctrl Pts',(-18.0843681028565,56.0934828172939,
40.1347395220992));
#177401=CARTESIAN_POINT('Ctrl Pts',(-18.0885652677239,56.0907851834709,
40.1367870714852));
#177402=CARTESIAN_POINT('Ctrl Pts',(-18.0928437845337,56.088138167006,40.1387166518767));
#177403=CARTESIAN_POINT('Ctrl Pts',(-18.1078185933682,56.0788736093785,
40.1454701832469));
#177404=CARTESIAN_POINT('Ctrl Pts',(-18.1237899619209,56.0702291095579,
40.1507785912491));
#177405=CARTESIAN_POINT('Ctrl Pts',(-18.1405610619113,56.0624257818118,
40.1543986087265));
#177406=CARTESIAN_POINT('Ctrl Pts',(-18.1489466119065,56.0585241179388,
40.1562086174652));
#177407=CARTESIAN_POINT('Ctrl Pts',(-18.1575320950781,56.0548327480527,
40.1575965292115));
#177408=CARTESIAN_POINT('Ctrl Pts',(-18.1662929092565,56.0513793155482,
40.1585319382567));
#177409=CARTESIAN_POINT('Ctrl Pts',(-18.1706733163456,56.0496525992959,
40.1589996427793));
#177410=CARTESIAN_POINT('Ctrl Pts',(-18.1750975561947,56.0479853674133,
40.159354221642));
#177411=CARTESIAN_POINT('Ctrl Pts',(-18.1795625536242,56.0463810756009,
40.1595918743111));
#177412=CARTESIAN_POINT('Ctrl Pts',(-18.1840275510537,56.0447767837885,
40.1598295269801));
#177413=CARTESIAN_POINT('Ctrl Pts',(-18.1885333065885,56.0432354336629,
40.1599502506895));
#177414=CARTESIAN_POINT('Ctrl Pts',(-18.1930767435944,56.0417604764385,
40.1599502534424));
#177415=CARTESIAN_POINT('',(-18.2220120550212,56.0323588238393,40.1599502534424));
#177416=CARTESIAN_POINT('Origin',(3.81437458815951E-16,6.47994644506575E-17,
40.1599502534424));
#177417=CARTESIAN_POINT('',(-18.567058682946,56.117947944099,39.8576902534424));
#177418=CARTESIAN_POINT('Ctrl Pts',(-18.2220120550212,56.0323588238393,
40.1599502534424));
#177419=CARTESIAN_POINT('Ctrl Pts',(-18.2256350948464,56.0311805982249,
40.1599502448875));
#177420=CARTESIAN_POINT('Ctrl Pts',(-18.2292627734001,56.0300502984939,
40.1598743450437));
#177421=CARTESIAN_POINT('Ctrl Pts',(-18.2328929164986,56.0289674832814,
40.1597243308499));
#177422=CARTESIAN_POINT('Ctrl Pts',(-18.2543250068315,56.0225746241519,
40.1588386583937));
#177423=CARTESIAN_POINT('Ctrl Pts',(-18.2758450255561,56.0178345032605,
40.155372255361));
#177424=CARTESIAN_POINT('Ctrl Pts',(-18.2969992991299,56.014658843408,40.1496902177768));
#177425=CARTESIAN_POINT('Ctrl Pts',(-18.3049018315393,56.0134725226006,
40.1475675976829));
#177426=CARTESIAN_POINT('Ctrl Pts',(-18.3127535860896,56.0125042026265,
40.1451361443088));
#177427=CARTESIAN_POINT('Ctrl Pts',(-18.3205319543143,56.0117482509601,
40.1424159447501));
#177428=CARTESIAN_POINT('Ctrl Pts',(-18.3266010274073,56.0111584195474,
40.1402935085949));
#177429=CARTESIAN_POINT('Ctrl Pts',(-18.3326250661768,56.0106982359128,
40.1379949176048));
#177430=CARTESIAN_POINT('Ctrl Pts',(-18.3385929672496,56.0103653778789,
40.1355293609261));
#177431=CARTESIAN_POINT('Ctrl Pts',(-18.3594806210044,56.0092003747605,
40.1268999125509));
#177432=CARTESIAN_POINT('Ctrl Pts',(-18.3796805851417,56.0095951017657,
40.1162251288835));
#177433=CARTESIAN_POINT('Ctrl Pts',(-18.3987168313625,56.0114500824672,
40.1038990521418));
#177434=CARTESIAN_POINT('Ctrl Pts',(-18.4082349544728,56.0123775728179,
40.097736013771));
#177435=CARTESIAN_POINT('Ctrl Pts',(-18.4174621486784,56.0136701283094,
40.0911601532641));
#177436=CARTESIAN_POINT('Ctrl Pts',(-18.4263389120626,56.0153153192431,
40.0842207290641));
#177437=CARTESIAN_POINT('Ctrl Pts',(-18.4351777497209,56.0169534811441,
40.0773109533619));
#177438=CARTESIAN_POINT('Ctrl Pts',(-18.4436692750114,56.0189410563925,
40.0700409753048));
#177439=CARTESIAN_POINT('Ctrl Pts',(-18.4517543535695,56.0212664209292,
40.0624586415899));
#177440=CARTESIAN_POINT('Ctrl Pts',(-18.4517890450624,56.0212763986142,
40.0624261072769));
#177441=CARTESIAN_POINT('Ctrl Pts',(-18.4518237293599,56.0212863820561,
40.0623935677888));
#177442=CARTESIAN_POINT('Ctrl Pts',(-18.4518584064609,56.021296371253,40.0623610231288));
#177443=CARTESIAN_POINT('Ctrl Pts',(-18.4682114607453,56.0260070845275,
40.0470135870268));
#177444=CARTESIAN_POINT('Ctrl Pts',(-18.482950362119,56.0319630212247,40.0305755292168));
#177445=CARTESIAN_POINT('Ctrl Pts',(-18.4960770195605,56.0389696815083,
40.0133447567458));
#177446=CARTESIAN_POINT('Ctrl Pts',(-18.5096811989713,56.0462312303064,
39.9954871626761));
#177447=CARTESIAN_POINT('Ctrl Pts',(-18.5215542196485,56.0546220378234,
39.976776795453));
#177448=CARTESIAN_POINT('Ctrl Pts',(-18.531655941201,56.063956229006,39.9575197577742));
#177449=CARTESIAN_POINT('Ctrl Pts',(-18.541613488521,56.0731572003366,39.9385375612315));
#177450=CARTESIAN_POINT('Ctrl Pts',(-18.5498501466764,56.0832757206921,
39.9190226977465));
#177451=CARTESIAN_POINT('Ctrl Pts',(-18.5562821957188,56.0941505847667,
39.8992655452277));
#177452=CARTESIAN_POINT('Ctrl Pts',(-18.5607667347539,56.1017327334914,
39.8854905069609));
#177453=CARTESIAN_POINT('Ctrl Pts',(-18.5643731068241,56.1096829110121,
39.8715976051617));
#177454=CARTESIAN_POINT('Ctrl Pts',(-18.567058682946,56.117947944099,39.8576902534424));
#177455=CARTESIAN_POINT('',(-18.6771643191705,56.4568070719813,39.2875012672119));
#177456=CARTESIAN_POINT('',(-18.567058682946,56.117947944099,39.8576902534424));
#177457=CARTESIAN_POINT('',(-23.8971395307763,54.4530463244695,39.2875012672119));
#177458=CARTESIAN_POINT('Origin',(5.53234440788222E-15,0.,39.2875012672119));
#177459=CARTESIAN_POINT('',(-23.7522229508823,54.1275498658876,39.8576902534424));
#177460=CARTESIAN_POINT('',(-23.8971395307763,54.4530463244694,39.2875012672119));
#177461=CARTESIAN_POINT('',(-23.951372267036,53.833063494684,40.1599502534424));
#177462=CARTESIAN_POINT('Ctrl Pts',(-23.7522229508823,54.1275498658876,
39.8576902534424));
#177463=CARTESIAN_POINT('Ctrl Pts',(-23.7472487091031,54.1163771839524,
39.8772619994049));
#177464=CARTESIAN_POINT('Ctrl Pts',(-23.7440527738935,54.1044728027364,
39.8967644650361));
#177465=CARTESIAN_POINT('Ctrl Pts',(-23.7426340760171,54.0920187959684,
39.9159282836035));
#177466=CARTESIAN_POINT('Ctrl Pts',(-23.7411897512762,54.0793398243582,
39.9354382707173));
#177467=CARTESIAN_POINT('Ctrl Pts',(-23.7415870431741,54.0660903588286,
39.9545987622342));
#177468=CARTESIAN_POINT('Ctrl Pts',(-23.7438697192134,54.0524339053522,
39.9731387498218));
#177469=CARTESIAN_POINT('Ctrl Pts',(-23.7460557526676,54.0393556307082,
39.9908938024045));
#177470=CARTESIAN_POINT('Ctrl Pts',(-23.7499709416789,54.0259032350479,
40.0080810366174));
#177471=CARTESIAN_POINT('Ctrl Pts',(-23.7556964920992,54.01220708765,40.0244542742534));
#177472=CARTESIAN_POINT('Ctrl Pts',(-23.7602504066234,54.0013136223967,
40.0374770090481));
#177473=CARTESIAN_POINT('Ctrl Pts',(-23.7659503210008,53.9902655788123,
40.0499848770036));
#177474=CARTESIAN_POINT('Ctrl Pts',(-23.7728578042866,53.9791273029165,
40.0618424270192));
#177475=CARTESIAN_POINT('Ctrl Pts',(-23.7728766594722,53.9790968990414,
40.0618747942791));
#177476=CARTESIAN_POINT('Ctrl Pts',(-23.7728955237001,53.9790664946661,
40.0619071564124));
#177477=CARTESIAN_POINT('Ctrl Pts',(-23.7729143969706,53.9790360897925,
40.0619395134161));
#177478=CARTESIAN_POINT('Ctrl Pts',(-23.776671466275,53.9729834442089,40.0683807661799));
#177479=CARTESIAN_POINT('Ctrl Pts',(-23.780822437404,53.966902706228,40.0746073439084));
#177480=CARTESIAN_POINT('Ctrl Pts',(-23.7853431031259,53.9608263568287,
40.0805869293669));
#177481=CARTESIAN_POINT('Ctrl Pts',(-23.7943146773159,53.9487674206469,
40.092453830807));
#177482=CARTESIAN_POINT('Ctrl Pts',(-23.8047436656396,53.9367254523686,
40.1033475319609));
#177483=CARTESIAN_POINT('Ctrl Pts',(-23.8164490335992,53.924952460372,40.1130129263075));
#177484=CARTESIAN_POINT('Ctrl Pts',(-23.8252280595689,53.9161227163746,
40.1202619720674));
#177485=CARTESIAN_POINT('Ctrl Pts',(-23.8347250487603,53.9074442707906,
40.1268200947266));
#177486=CARTESIAN_POINT('Ctrl Pts',(-23.8448636317802,53.8990234500735,
40.1325796782703));
#177487=CARTESIAN_POINT('Ctrl Pts',(-23.8486656004127,53.8958656423046,
40.1347395220992));
#177488=CARTESIAN_POINT('Ctrl Pts',(-23.8525577932538,53.8927440632083,
40.1367870714852));
#177489=CARTESIAN_POINT('Ctrl Pts',(-23.8565361833376,53.8896643205893,
40.1387166518767));
#177490=CARTESIAN_POINT('Ctrl Pts',(-23.8704605486307,53.8788852214227,
40.1454701832469));
#177491=CARTESIAN_POINT('Ctrl Pts',(-23.8854408280735,53.8686186144655,
40.1507785912492));
#177492=CARTESIAN_POINT('Ctrl Pts',(-23.9013043843657,53.859104976856,40.1543986087265));
#177493=CARTESIAN_POINT('Ctrl Pts',(-23.9092361625117,53.8543481580513,
40.1562086174652));
#177494=CARTESIAN_POINT('Ctrl Pts',(-23.9173887602867,53.8497795825133,
40.1575965292115));
#177495=CARTESIAN_POINT('Ctrl Pts',(-23.9257405998156,53.8454293138304,
40.1585319382567));
#177496=CARTESIAN_POINT('Ctrl Pts',(-23.92991651958,53.8432541794889,40.1589996427793));
#177497=CARTESIAN_POINT('Ctrl Pts',(-23.9341422497936,53.8411336218844,
40.159354221642));
#177498=CARTESIAN_POINT('Ctrl Pts',(-23.9384150933423,53.8390713992306,
40.1595918743111));
#177499=CARTESIAN_POINT('Ctrl Pts',(-23.942687936891,53.8370091765768,40.1598295269801));
#177500=CARTESIAN_POINT('Ctrl Pts',(-23.9470078944655,53.8350052904266,
40.1599502506895));
#177501=CARTESIAN_POINT('Ctrl Pts',(-23.951372267036,53.833063494684,40.1599502534424));
#177502=CARTESIAN_POINT('',(-23.9791663275009,53.8206887816838,40.1599502534424));
#177503=CARTESIAN_POINT('Origin',(3.74779409800327E-16,6.22436788900575E-17,
40.1599502534424));
#177504=CARTESIAN_POINT('',(-24.3312692531083,53.8697418420147,39.8576902534424));
#177505=CARTESIAN_POINT('Ctrl Pts',(-23.9791663275009,53.8206887816838,
40.1599502534424));
#177506=CARTESIAN_POINT('Ctrl Pts',(-23.982646361822,53.8191382997274,40.1599502448875));
#177507=CARTESIAN_POINT('Ctrl Pts',(-23.9861360190791,53.8176349962321,
40.1598743450437));
#177508=CARTESIAN_POINT('Ctrl Pts',(-23.9896330908637,53.8161786595151,
40.1597243308499));
#177509=CARTESIAN_POINT('Ctrl Pts',(-24.0102795382188,53.8075805576713,
40.1588386583939));
#177510=CARTESIAN_POINT('Ctrl Pts',(-24.0311861904727,53.8006169491723,
40.1553722553623));
#177511=CARTESIAN_POINT('Ctrl Pts',(-24.0518926318745,53.7952474622089,
40.14969021778));
#177512=CARTESIAN_POINT('Ctrl Pts',(-24.0596278690975,53.7932416006212,
40.1475675976853));
#177513=CARTESIAN_POINT('Ctrl Pts',(-24.0673353939197,53.7914578533671,
40.1451361443101));
#177514=CARTESIAN_POINT('Ctrl Pts',(-24.0749921329673,53.789892982005,40.1424159447501));
#177515=CARTESIAN_POINT('Ctrl Pts',(-24.0809663048717,53.7886719908666,
40.1402935085949));
#177516=CARTESIAN_POINT('Ctrl Pts',(-24.0869092410384,53.7875846446508,
40.1379949176048));
#177517=CARTESIAN_POINT('Ctrl Pts',(-24.0928096561859,53.7866297945201,
40.1355293609261));
#177518=CARTESIAN_POINT('Ctrl Pts',(-24.1134611092023,53.7832878190624,
40.1268999125509));
#177519=CARTESIAN_POINT('Ctrl Pts',(-24.1335916760297,53.7815689125024,
40.1162251288835));
#177520=CARTESIAN_POINT('Ctrl Pts',(-24.152717537984,53.7814239018616,40.1038990521418));
#177521=CARTESIAN_POINT('Ctrl Pts',(-24.1622804689611,53.7813513965412,
40.097736013771));
#177522=CARTESIAN_POINT('Ctrl Pts',(-24.1715922244705,53.781672366848,40.0911601532641));
#177523=CARTESIAN_POINT('Ctrl Pts',(-24.1805923292962,53.7823806708183,
40.084220729064));
#177524=CARTESIAN_POINT('Ctrl Pts',(-24.1895539814231,53.7830859485794,
40.0773109533619));
#177525=CARTESIAN_POINT('Ctrl Pts',(-24.198206747436,53.7841750295932,40.0700409753048));
#177526=CARTESIAN_POINT('Ctrl Pts',(-24.2064906018693,53.7856425347026,
40.0624586415899));
#177527=CARTESIAN_POINT('Ctrl Pts',(-24.2065261462707,53.7856488314804,
40.062426107277));
#177528=CARTESIAN_POINT('Ctrl Pts',(-24.2065616841178,53.7856551347356,
40.0623935677889));
#177529=CARTESIAN_POINT('Ctrl Pts',(-24.2065972154094,53.7856614444666,
40.0623610231289));
#177530=CARTESIAN_POINT('Ctrl Pts',(-24.2233530895771,53.7886369923279,
40.0470135870212));
#177531=CARTESIAN_POINT('Ctrl Pts',(-24.2386338146223,53.793019667072,40.0305755292047));
#177532=CARTESIAN_POINT('Ctrl Pts',(-24.252420958297,53.7986158348102,40.0133447567266));
#177533=CARTESIAN_POINT('Ctrl Pts',(-24.2667096511305,53.8044155801195,
39.9954871626496));
#177534=CARTESIAN_POINT('Ctrl Pts',(-24.2793947083764,53.8115193533133,
39.9767767954186));
#177535=CARTESIAN_POINT('Ctrl Pts',(-24.2904167803032,53.8197464933945,
39.9575197577317));
#177536=CARTESIAN_POINT('Ctrl Pts',(-24.3012815425323,53.8278562137268,
39.9385375611815));
#177537=CARTESIAN_POINT('Ctrl Pts',(-24.3105307527959,53.8370583385547,
39.9190226976888));
#177538=CARTESIAN_POINT('Ctrl Pts',(-24.3180642992295,53.8472012967897,
39.8992655451625));
#177539=CARTESIAN_POINT('Ctrl Pts',(-24.3233168218341,53.8542731477268,
39.885490506917));
#177540=CARTESIAN_POINT('Ctrl Pts',(-24.3277344576514,53.8618028048015,
39.8715976051397));
#177541=CARTESIAN_POINT('Ctrl Pts',(-24.3312692531083,53.8697418420147,
39.8576902534424));
#177542=CARTESIAN_POINT('',(-24.4761921430387,54.1952354911874,39.2875012672119));
#177543=CARTESIAN_POINT('',(-24.3312692531083,53.8697418420147,39.8576902534424));
#177544=CARTESIAN_POINT('',(-29.4581217525669,51.656815567543,39.2875012672119));
#177545=CARTESIAN_POINT('Origin',(5.53234440788222E-15,0.,39.2875012672119));
#177546=CARTESIAN_POINT('',(-29.2799753962458,51.3482501200168,39.8576902534424));
#177547=CARTESIAN_POINT('',(-29.4581217525669,51.656815567543,39.2875012672119));
#177548=CARTESIAN_POINT('',(-29.4472515437731,51.0345602039889,40.1599502534424));
#177549=CARTESIAN_POINT('Ctrl Pts',(-29.2799753962458,51.3482501200168,
39.8576902534424));
#177550=CARTESIAN_POINT('Ctrl Pts',(-29.2738605406099,51.3376585930511,
39.8772619994057));
#177551=CARTESIAN_POINT('Ctrl Pts',(-29.269437766393,51.3261534914766,39.8967644650376));
#177552=CARTESIAN_POINT('Ctrl Pts',(-29.266725042103,51.3139160033692,39.9159282836057));
#177553=CARTESIAN_POINT('Ctrl Pts',(-29.2639633161059,51.3014574615371,
39.9354382707205));
#177554=CARTESIAN_POINT('Ctrl Pts',(-29.2629734853264,51.2882390496537,
39.9545987622381));
#177555=CARTESIAN_POINT('Ctrl Pts',(-29.2638161685324,51.2744188030391,
39.9731387498264));
#177556=CARTESIAN_POINT('Ctrl Pts',(-29.2646231747162,51.2611836698336,
39.99089380241));
#177557=CARTESIAN_POINT('Ctrl Pts',(-29.2671107576673,51.2473957191126,
40.0080810366237));
#177558=CARTESIAN_POINT('Ctrl Pts',(-29.271373305684,51.2331761176555,40.0244542742603));
#177559=CARTESIAN_POINT('Ctrl Pts',(-29.2747635962052,51.2218663142594,
40.0374770090526));
#177560=CARTESIAN_POINT('Ctrl Pts',(-29.2792774508366,51.2102829897252,
40.0499848770057));
#177561=CARTESIAN_POINT('Ctrl Pts',(-29.2849828273425,51.1984837018593,
40.0618424270193));
#177562=CARTESIAN_POINT('Ctrl Pts',(-29.2849984011671,51.1984514936363,
40.0618747942791));
#177563=CARTESIAN_POINT('Ctrl Pts',(-29.2850139839321,51.1984192839705,
40.0619071564124));
#177564=CARTESIAN_POINT('Ctrl Pts',(-29.2850295756381,51.1983870728641,
40.0619395134162));
#177565=CARTESIAN_POINT('Ctrl Pts',(-29.2881333895822,51.1919748636255,
40.0683807661799));
#177566=CARTESIAN_POINT('Ctrl Pts',(-29.2916260110603,51.1854935419304,
40.0746073439084));
#177567=CARTESIAN_POINT('Ctrl Pts',(-29.2954867606374,51.178977941168,40.0805869293669));
#177568=CARTESIAN_POINT('Ctrl Pts',(-29.3031486855376,51.1660472802372,
40.092453830807));
#177569=CARTESIAN_POINT('Ctrl Pts',(-29.3122618143332,51.1529811529981,
40.1033475319609));
#177570=CARTESIAN_POINT('Ctrl Pts',(-29.3226724463009,51.1400491105587,
40.1130129263075));
#177571=CARTESIAN_POINT('Ctrl Pts',(-29.3304804202767,51.1303500787292,
40.1202619720674));
#177572=CARTESIAN_POINT('Ctrl Pts',(-29.3390182393872,51.1207264688923,
40.1268200947266));
#177573=CARTESIAN_POINT('Ctrl Pts',(-29.3482210667394,51.1112920078094,
40.1325796782703));
#177574=CARTESIAN_POINT('Ctrl Pts',(-29.3516721269965,51.1077540849033,
40.1347395220992));
#177575=CARTESIAN_POINT('Ctrl Pts',(-29.3552167041322,51.1042427612075,
40.1367870714852));
#177576=CARTESIAN_POINT('Ctrl Pts',(-29.3588513794155,51.1007640347391,
40.1387166518767));
#177577=CARTESIAN_POINT('Ctrl Pts',(-29.3715727429074,51.0885884920995,
40.1454701832469));
#177578=CARTESIAN_POINT('Ctrl Pts',(-29.3853978061637,51.0768122610999,
40.1507785912492));
#177579=CARTESIAN_POINT('Ctrl Pts',(-29.4001800143153,51.0656925470315,
40.1543986087265));
#177580=CARTESIAN_POINT('Ctrl Pts',(-29.4075711183911,51.0601326899973,
40.1562086174652));
#177581=CARTESIAN_POINT('Ctrl Pts',(-29.4152015092021,51.054736963077,40.1575965292115));
#177582=CARTESIAN_POINT('Ctrl Pts',(-29.42305286958,51.0495375206697,40.1585319382567));
#177583=CARTESIAN_POINT('Ctrl Pts',(-29.4269785497689,51.0469377994661,
40.1589996427793));
#177584=CARTESIAN_POINT('Ctrl Pts',(-29.4309594723626,51.0443871494125,
40.159354221642));
#177585=CARTESIAN_POINT('Ctrl Pts',(-29.4349933478623,51.0418895900603,
40.1595918743111));
#177586=CARTESIAN_POINT('Ctrl Pts',(-29.439027223362,51.0393920307081,40.1598295269801));
#177587=CARTESIAN_POINT('Ctrl Pts',(-29.4431140526171,51.0369475635292,
40.1599502506895));
#177588=CARTESIAN_POINT('Ctrl Pts',(-29.4472515437731,51.034560203989,40.1599502534424));
#177589=CARTESIAN_POINT('',(-29.4735998357333,51.019348010533,40.1599502534424));
#177590=CARTESIAN_POINT('Origin',(3.68424986610945E-16,5.90059385582091E-17,
40.1599502534424));
#177591=CARTESIAN_POINT('',(-29.8289013456881,51.0313275753412,39.8576902534424));
#177592=CARTESIAN_POINT('Ctrl Pts',(-29.4735998357333,51.019348010533,40.1599502534424));
#177593=CARTESIAN_POINT('Ctrl Pts',(-29.476898736566,51.0174422596393,40.1599502448875));
#177594=CARTESIAN_POINT('Ctrl Pts',(-29.4802121391114,51.0155824228874,
40.1598743450438));
#177595=CARTESIAN_POINT('Ctrl Pts',(-29.4835378249318,51.0137685205958,
40.1597243308499));
#177596=CARTESIAN_POINT('Ctrl Pts',(-29.5031724225167,51.0030593786387,
40.1588386583938));
#177597=CARTESIAN_POINT('Ctrl Pts',(-29.5232366506486,50.9939485772829,
40.1553722553617));
#177598=CARTESIAN_POINT('Ctrl Pts',(-29.5432683957785,50.9864440924311,
40.1496902177787));
#177599=CARTESIAN_POINT('Ctrl Pts',(-29.5507515889318,50.9836406667038,
40.1475675976843));
#177600=CARTESIAN_POINT('Ctrl Pts',(-29.5582304387657,50.9810610352791,
40.1451361443096));
#177601=CARTESIAN_POINT('Ctrl Pts',(-29.5656816597953,50.9787043892803,
40.1424159447501));
#177602=CARTESIAN_POINT('Ctrl Pts',(-29.5714954762336,50.9768656158507,
40.1402935085949));
#177603=CARTESIAN_POINT('Ctrl Pts',(-29.5772921977452,50.9751630202464,
40.1379949176048));
#177604=CARTESIAN_POINT('Ctrl Pts',(-29.5830604807844,50.9735966395566,
40.1355293609262));
#177605=CARTESIAN_POINT('Ctrl Pts',(-29.6032494714214,50.9681143071421,
40.1268999125509));
#177606=CARTESIAN_POINT('Ctrl Pts',(-29.6230900862363,50.9643005997169,
40.1162251288835));
#177607=CARTESIAN_POINT('Ctrl Pts',(-29.6420960169782,50.9621571865008,
40.1038990521418));
#177608=CARTESIAN_POINT('Ctrl Pts',(-29.6515989823491,50.9610854798928,
40.097736013771));
#177609=CARTESIAN_POINT('Ctrl Pts',(-29.6608932776205,50.9604313483969,
40.0911601532641));
#177610=CARTESIAN_POINT('Ctrl Pts',(-29.6699181168558,50.9601950050772,
40.084220729064));
#177611=CARTESIAN_POINT('Ctrl Pts',(-29.6789043977152,50.9599596715279,
40.0773109533619));
#177612=CARTESIAN_POINT('Ctrl Pts',(-29.6876236029352,50.9601383261076,
40.0700409753048));
#177613=CARTESIAN_POINT('Ctrl Pts',(-29.6960154736012,50.9607318934966,
40.0624586415899));
#177614=CARTESIAN_POINT('Ctrl Pts',(-29.6960514814791,50.9607344403783,
40.0624261072769));
#177615=CARTESIAN_POINT('Ctrl Pts',(-29.6960874835157,50.9607369943871,
40.0623935677888));
#177616=CARTESIAN_POINT('Ctrl Pts',(-29.6961234797097,50.9607395555214,
40.0623610231288));
#177617=CARTESIAN_POINT('Ctrl Pts',(-29.7130985928884,50.9619473372425,
40.0470135870233));
#177618=CARTESIAN_POINT('Ctrl Pts',(-29.728753722777,50.9647087325286,40.0305755292094));
#177619=CARTESIAN_POINT('Ctrl Pts',(-29.7430502978482,50.9688330949322,
40.013344756734));
#177620=CARTESIAN_POINT('Ctrl Pts',(-29.7578669541901,50.9731074935248,
39.9954871626599));
#177621=CARTESIAN_POINT('Ctrl Pts',(-29.7712250678592,50.9788464019639,
39.9767767954321));
#177622=CARTESIAN_POINT('Ctrl Pts',(-29.7830467300316,50.9858763526685,
39.9575197577485));
#177623=CARTESIAN_POINT('Ctrl Pts',(-29.7946996705594,50.9928059702028,
39.9385375612016));
#177624=CARTESIAN_POINT('Ctrl Pts',(-29.804860096648,51.0009908790906,39.9190226977123));
#177625=CARTESIAN_POINT('Ctrl Pts',(-29.8134126013634,51.010290803105,39.8992655451893));
#177626=CARTESIAN_POINT('Ctrl Pts',(-29.8193755598153,51.0167748755901,
39.8854905069351));
#177627=CARTESIAN_POINT('Ctrl Pts',(-29.8245560588482,51.0238015157365,
39.8715976051487));
#177628=CARTESIAN_POINT('Ctrl Pts',(-29.8289013456881,51.0313275753412,
39.8576902534424));
#177629=CARTESIAN_POINT('',(-30.0070536838153,51.33988956927,39.2875012672119));
#177630=CARTESIAN_POINT('',(-29.8289013456881,51.0313275753412,39.8576902534424));
#177631=CARTESIAN_POINT('',(-34.6963546279281,48.2946219293749,39.2875012672119));
#177632=CARTESIAN_POINT('Origin',(5.53234440788222E-15,0.,39.2875012672119));
#177633=CARTESIAN_POINT('',(-34.4869303039392,48.006368200519,39.8576902534424));
#177634=CARTESIAN_POINT('',(-34.6963546279281,48.2946219293749,39.2875012672119));
#177635=CARTESIAN_POINT('',(-34.620500570363,47.6769115920307,40.1599502534424));
#177636=CARTESIAN_POINT('Ctrl Pts',(-34.4869303039393,48.006368200519,39.8576902534424));
#177637=CARTESIAN_POINT('Ctrl Pts',(-34.4797418300853,47.9964738715094,
39.8772619994048));
#177638=CARTESIAN_POINT('Ctrl Pts',(-34.4741406737012,47.9854941018779,
39.8967644650359));
#177639=CARTESIAN_POINT('Ctrl Pts',(-34.4701636441726,47.9736072089126,
39.9159282836032));
#177640=CARTESIAN_POINT('Ctrl Pts',(-34.4661147749673,47.9615055952513,
39.935438270717));
#177641=CARTESIAN_POINT('Ctrl Pts',(-34.4637486663033,47.9484630607023,
39.9545987622339));
#177642=CARTESIAN_POINT('Ctrl Pts',(-34.4631421240615,47.9346304384649,
39.9731387498215));
#177643=CARTESIAN_POINT('Ctrl Pts',(-34.4625612612457,47.9213834535885,
39.9908938024042));
#177644=CARTESIAN_POINT('Ctrl Pts',(-34.4635939836562,47.907411011482,40.0080810366171));
#177645=CARTESIAN_POINT('Ctrl Pts',(-34.4663468278996,47.8928237488966,
40.0244542742532));
#177646=CARTESIAN_POINT('Ctrl Pts',(-34.4685363496856,47.8812215199268,
40.037477009048));
#177647=CARTESIAN_POINT('Ctrl Pts',(-34.4718146898364,47.8692298237661,
40.0499848770036));
#177648=CARTESIAN_POINT('Ctrl Pts',(-34.4762554502654,47.8568987993931,
40.0618424270193));
#177649=CARTESIAN_POINT('Ctrl Pts',(-34.4762675720988,47.856865139702,40.0618747942791));
#177650=CARTESIAN_POINT('Ctrl Pts',(-34.476279702673,47.8568314776417,40.0619071564124));
#177651=CARTESIAN_POINT('Ctrl Pts',(-34.4762918419885,47.8567978132141,
40.0619395134161));
#177652=CARTESIAN_POINT('Ctrl Pts',(-34.4787083945372,47.8500962938268,
40.0683807661799));
#177653=CARTESIAN_POINT('Ctrl Pts',(-34.4815044004727,47.8432853991342,
40.0746073439084));
#177654=CARTESIAN_POINT('Ctrl Pts',(-34.4846629347248,47.8364019332941,
40.0805869293668));
#177655=CARTESIAN_POINT('Ctrl Pts',(-34.4909312646825,47.8227412186414,
40.092453830807));
#177656=CARTESIAN_POINT('Ctrl Pts',(-34.4986286886039,47.8087940876659,
40.1033475319609));
#177657=CARTESIAN_POINT('Ctrl Pts',(-34.5076305235172,47.7948446809468,
40.1130129263075));
#177658=CARTESIAN_POINT('Ctrl Pts',(-34.5143818997023,47.7843826259075,
40.1202619720674));
#177659=CARTESIAN_POINT('Ctrl Pts',(-34.5218670065991,47.773919290101,40.1268200947266));
#177660=CARTESIAN_POINT('Ctrl Pts',(-34.5300332501814,47.7635745545822,
40.1325796782703));
#177661=CARTESIAN_POINT('Ctrl Pts',(-34.5330955915248,47.7596952787626,
40.1347395220992));
#177662=CARTESIAN_POINT('Ctrl Pts',(-34.5362537178261,47.7558326812646,
40.1367870714852));
#177663=CARTESIAN_POINT('Ctrl Pts',(-34.5395048560461,47.7519930846018,
40.1387166518767));
#177664=CARTESIAN_POINT('Ctrl Pts',(-34.5508838398161,47.7385544962823,
40.1454701832469));
#177665=CARTESIAN_POINT('Ctrl Pts',(-34.5634022165999,47.7253976640915,
40.1507785912492));
#177666=CARTESIAN_POINT('Ctrl Pts',(-34.576941119645,47.7127937034785,40.1543986087265));
#177667=CARTESIAN_POINT('Ctrl Pts',(-34.5837105711675,47.706491723172,40.1562086174652));
#177668=CARTESIAN_POINT('Ctrl Pts',(-34.5907351548561,47.7003279615827,
40.1575965292115));
#177669=CARTESIAN_POINT('Ctrl Pts',(-34.5980000149356,47.6943363116301,
40.1585319382567));
#177670=CARTESIAN_POINT('Ctrl Pts',(-34.6016324449754,47.6913404866538,
40.1589996427793));
#177671=CARTESIAN_POINT('Ctrl Pts',(-34.6053249441282,47.688387689607,40.159354221642));
#177672=CARTESIAN_POINT('Ctrl Pts',(-34.6090756555948,47.6854821573393,
40.159591874311));
#177673=CARTESIAN_POINT('Ctrl Pts',(-34.6128263670615,47.6825766250715,
40.1598295269801));
#177674=CARTESIAN_POINT('Ctrl Pts',(-34.6166352918406,47.6797183589579,
40.1599502506895));
#177675=CARTESIAN_POINT('Ctrl Pts',(-34.620500570363,47.6769115920307,40.1599502534424));
#177676=CARTESIAN_POINT('',(-34.6451144164181,47.6590285860939,40.1599502534424));
#177677=CARTESIAN_POINT('Origin',(3.62443809638016E-16,5.51217168157321E-17,
40.1599502534424));
#177678=CARTESIAN_POINT('',(-34.9997217530256,47.6338034047603,39.8576902534424));
#177679=CARTESIAN_POINT('Ctrl Pts',(-34.6451144164181,47.6590285860939,
40.1599502534424));
#177680=CARTESIAN_POINT('Ctrl Pts',(-34.6481960403147,47.6567884460684,
40.1599502448875));
#177681=CARTESIAN_POINT('Ctrl Pts',(-34.6512968858166,47.6545924528206,
40.1598743450437));
#177682=CARTESIAN_POINT('Ctrl Pts',(-34.654414748763,47.6524408584474,40.1597243308499));
#177683=CARTESIAN_POINT('Ctrl Pts',(-34.672822375821,47.6397380079748,40.1588386583936));
#177684=CARTESIAN_POINT('Ctrl Pts',(-34.6918243519518,47.6285798336065,
40.15537225536));
#177685=CARTESIAN_POINT('Ctrl Pts',(-34.7109619288217,47.6190225715713,
40.1496902177744));
#177686=CARTESIAN_POINT('Ctrl Pts',(-34.718111090472,47.6154522966254,40.147567597681));
#177687=CARTESIAN_POINT('Ctrl Pts',(-34.7252793254705,47.6121050440139,
40.1451361443077));
#177688=CARTESIAN_POINT('Ctrl Pts',(-34.7324433913422,47.6089824432868,
40.1424159447501));
#177689=CARTESIAN_POINT('Ctrl Pts',(-34.7380331549248,47.6065460335525,
40.1402935085949));
#177690=CARTESIAN_POINT('Ctrl Pts',(-34.7436201516873,47.6042468425535,
40.1379949176048));
#177691=CARTESIAN_POINT('Ctrl Pts',(-34.7491931041021,47.6020860928991,
40.1355293609261));
#177692=CARTESIAN_POINT('Ctrl Pts',(-34.7686984375536,47.594523469109,40.1268999125509));
#177693=CARTESIAN_POINT('Ctrl Pts',(-34.788031722428,47.5886567445953,40.1162251288835));
#177694=CARTESIAN_POINT('Ctrl Pts',(-34.806709489003,47.5845384124877,40.1038990521418));
#177695=CARTESIAN_POINT('Ctrl Pts',(-34.8160483722906,47.5824792464339,
40.097736013771));
#177696=CARTESIAN_POINT('Ctrl Pts',(-34.8252233770799,47.5808571799369,
40.0911601532641));
#177697=CARTESIAN_POINT('Ctrl Pts',(-34.8341740726976,47.5796787787542,
40.084220729064));
#177698=CARTESIAN_POINT('Ctrl Pts',(-34.8430865267159,47.5785054122579,
40.0773109533619));
#177699=CARTESIAN_POINT('Ctrl Pts',(-34.8517766417061,47.5777716830265,
40.0700409753048));
#177700=CARTESIAN_POINT('Ctrl Pts',(-34.8601845855135,47.5774848094466,
40.0624586415899));
#177701=CARTESIAN_POINT('Ctrl Pts',(-34.8602206623581,47.5774835785281,
40.0624261072769));
#177702=CARTESIAN_POINT('Ctrl Pts',(-34.8602567341385,47.5774823553082,
40.0623935677889));
#177703=CARTESIAN_POINT('Ctrl Pts',(-34.8602928008529,47.5774811397856,
40.0623610231288));
#177704=CARTESIAN_POINT('Ctrl Pts',(-34.8773011701497,47.5769079226578,
40.0470135870262));
#177705=CARTESIAN_POINT('Ctrl Pts',(-34.8931591840017,47.5780177840616,
40.0305755292153));
#177706=CARTESIAN_POINT('Ctrl Pts',(-34.9078085542006,47.5806251537532,
40.0133447567434));
#177707=CARTESIAN_POINT('Ctrl Pts',(-34.9229908396628,47.583327374424,39.9954871626726));
#177708=CARTESIAN_POINT('Ctrl Pts',(-34.9368756554658,47.5876385414267,
39.9767767954483));
#177709=CARTESIAN_POINT('Ctrl Pts',(-34.9493673872787,47.5933942811437,
39.9575197577683));
#177710=CARTESIAN_POINT('Ctrl Pts',(-34.9616808340502,47.5990678735405,
39.9385375612242));
#177711=CARTESIAN_POINT('Ctrl Pts',(-34.9726411562094,47.6061458909138,
39.9190226977378));
#177712=CARTESIAN_POINT('Ctrl Pts',(-34.9821189161751,47.6145008887939,
39.8992655452176));
#177713=CARTESIAN_POINT('Ctrl Pts',(-34.9887269790549,47.6203261419712,
39.8854905069541));
#177714=CARTESIAN_POINT('Ctrl Pts',(-34.9946135826731,47.6267727798487,
39.8715976051582));
#177715=CARTESIAN_POINT('Ctrl Pts',(-34.9997217530256,47.6338034047603,
39.8576902534424));
#177716=CARTESIAN_POINT('',(-35.2091516650524,47.922053073669,39.2875012672119));
#177717=CARTESIAN_POINT('',(-34.9997217530256,47.6338034047603,39.8576902534424));
#177718=CARTESIAN_POINT('',(-39.5544469813067,44.4033023070493,39.2875012672119));
#177719=CARTESIAN_POINT('Origin',(5.53234440788222E-15,0.,39.2875012672119));
#177720=CARTESIAN_POINT('',(-39.3160391863686,44.1385184650379,39.8576902534424));
#177721=CARTESIAN_POINT('',(-39.5544469813067,44.4033023070493,39.2875012672119));
#177722=CARTESIAN_POINT('',(-39.4144401478986,43.796904759635,40.1599502534424));
#177723=CARTESIAN_POINT('Ctrl Pts',(-39.3160391863686,44.1385184650379,
39.8576902534424));
#177724=CARTESIAN_POINT('Ctrl Pts',(-39.3078558527195,44.1294297383223,
39.8772619994063));
#177725=CARTESIAN_POINT('Ctrl Pts',(-39.3011376816091,44.1190955972862,
39.8967644650388));
#177726=CARTESIAN_POINT('Ctrl Pts',(-39.2959399200096,44.1076895347483,
39.9159282836075));
#177727=CARTESIAN_POINT('Ctrl Pts',(-39.2906482678542,44.0960774370678,
39.9354382707228));
#177728=CARTESIAN_POINT('Ctrl Pts',(-39.2869318048875,44.0833536765891,
39.9545987622409));
#177729=CARTESIAN_POINT('Ctrl Pts',(-39.2848826826026,44.0696602318308,
39.9731387498297));
#177730=CARTESIAN_POINT('Ctrl Pts',(-39.2829203148423,44.0565465320198,
39.9908938024137));
#177731=CARTESIAN_POINT('Ctrl Pts',(-39.2824868619904,44.0425426835252,
40.0080810366277));
#177732=CARTESIAN_POINT('Ctrl Pts',(-39.2836998417246,44.0277475809106,
40.0244542742647));
#177733=CARTESIAN_POINT('Ctrl Pts',(-39.2846646059168,44.0159800428206,
40.0374770090554));
#177734=CARTESIAN_POINT('Ctrl Pts',(-39.2866715134054,44.0037113585717,
40.049984877007));
#177735=CARTESIAN_POINT('Ctrl Pts',(-39.2897990038549,43.9909836989807,
40.0618424270193));
#177736=CARTESIAN_POINT('Ctrl Pts',(-39.2898075408879,43.9909489566044,
40.0618747942791));
#177737=CARTESIAN_POINT('Ctrl Pts',(-39.2898160863661,43.9909142109581,
40.0619071564124));
#177738=CARTESIAN_POINT('Ctrl Pts',(-39.2898246402903,43.9908794620437,
40.0619395134162));
#177739=CARTESIAN_POINT('Ctrl Pts',(-39.2915274551881,43.9839620557564,
40.0683807661799));
#177740=CARTESIAN_POINT('Ctrl Pts',(-39.2935962119549,43.9768962096539,
40.0746073439084));
#177741=CARTESIAN_POINT('Ctrl Pts',(-39.2960179253196,43.9697202954284,
40.0805869293669));
#177742=CARTESIAN_POINT('Ctrl Pts',(-39.3008239832001,43.9554791967021,
40.092453830807));
#177743=CARTESIAN_POINT('Ctrl Pts',(-39.30702136766,43.9408038696758,40.1033475319609));
#177744=CARTESIAN_POINT('Ctrl Pts',(-39.314515779532,43.9259899312962,40.1130129263075));
#177745=CARTESIAN_POINT('Ctrl Pts',(-39.320136588436,43.9148794775116,40.1202619720674));
#177746=CARTESIAN_POINT('Ctrl Pts',(-39.3264869747216,43.9036910542321,
40.1268200947266));
#177747=CARTESIAN_POINT('Ctrl Pts',(-39.3335271634604,43.8925493833645,
40.1325796782703));
#177748=CARTESIAN_POINT('Ctrl Pts',(-39.3361672342375,43.8883712567891,
40.1347395220992));
#177749=CARTESIAN_POINT('Ctrl Pts',(-39.3389043086117,43.8841997049152,
40.1367870714852));
#177750=CARTESIAN_POINT('Ctrl Pts',(-39.3417362896176,43.8800413054828,
40.1387166518767));
#177751=CARTESIAN_POINT('Ctrl Pts',(-39.3516482231384,43.8654869074691,
40.1454701832469));
#177752=CARTESIAN_POINT('Ctrl Pts',(-39.3627227594941,43.8510936230939,
40.1507785912492));
#177753=CARTESIAN_POINT('Ctrl Pts',(-39.3748700223777,43.8371435075662,
40.1543986087265));
#177754=CARTESIAN_POINT('Ctrl Pts',(-39.3809436538195,43.8301684498024,
40.1562086174652));
#177755=CARTESIAN_POINT('Ctrl Pts',(-39.3872854675768,43.823304185006,40.1575965292115));
#177756=CARTESIAN_POINT('Ctrl Pts',(-39.3938842320307,43.8165859732788,
40.1585319382567));
#177757=CARTESIAN_POINT('Ctrl Pts',(-39.3971836142576,43.8132268674151,
40.1589996427793));
#177758=CARTESIAN_POINT('Ctrl Pts',(-39.400547234176,43.8099042748375,40.159354221642));
#177759=CARTESIAN_POINT('Ctrl Pts',(-39.4039736880299,43.8066226032737,
40.1595918743111));
#177760=CARTESIAN_POINT('Ctrl Pts',(-39.4074001418838,43.8033409317099,
40.1598295269801));
#177761=CARTESIAN_POINT('Ctrl Pts',(-39.4108894308099,43.8001001824233,
40.1599502506895));
#177762=CARTESIAN_POINT('Ctrl Pts',(-39.4144401478986,43.796904759635,40.1599502534424));
#177763=CARTESIAN_POINT('',(-39.4370498736004,43.7765468711726,40.1599502534424));
#177764=CARTESIAN_POINT('Origin',(3.56901409908096E-16,5.06335700088602E-17,
40.1599502534424));
#177765=CARTESIAN_POINT('',(-39.7870778846743,43.7143933160627,39.8576902534424));
#177766=CARTESIAN_POINT('Ctrl Pts',(-39.4370498736004,43.7765468711726,
40.1599502534424));
#177767=CARTESIAN_POINT('Ctrl Pts',(-39.4398804576445,43.7739968854583,
40.1599502448875));
#177768=CARTESIAN_POINT('Ctrl Pts',(-39.4427347725908,43.7714887954761,
40.1598743450437));
#177769=CARTESIAN_POINT('Ctrl Pts',(-39.4456106527043,43.7690230823395,
40.1597243308499));
#177770=CARTESIAN_POINT('Ctrl Pts',(-39.4625896314139,43.7544656984441,
40.1588386583937));
#177771=CARTESIAN_POINT('Ctrl Pts',(-39.4803211659092,43.7413824023601,
40.1553722553609));
#177772=CARTESIAN_POINT('Ctrl Pts',(-39.4983548992145,43.7298770745066,
40.1496902177767));
#177773=CARTESIAN_POINT('Ctrl Pts',(-39.505091701658,43.7255790670178,40.1475675976828));
#177774=CARTESIAN_POINT('Ctrl Pts',(-39.511870785146,43.721500866416,40.1451361443087));
#177775=CARTESIAN_POINT('Ctrl Pts',(-39.5186692048623,43.7176465228247,
40.1424159447502));
#177776=CARTESIAN_POINT('Ctrl Pts',(-39.5239736729698,43.7146391706005,
40.1402935085949));
#177777=CARTESIAN_POINT('Ctrl Pts',(-39.5292897326775,43.7117685746245,
40.1379949176048));
#177778=CARTESIAN_POINT('Ctrl Pts',(-39.534606296035,43.7090371296311,40.1355293609261));
#177779=CARTESIAN_POINT('Ctrl Pts',(-39.5532142677859,43.6994770721542,
40.1268999125509));
#177780=CARTESIAN_POINT('Ctrl Pts',(-39.5718284032051,43.6916216076133,
40.1162251288835));
#177781=CARTESIAN_POINT('Ctrl Pts',(-39.5899733680941,43.6855734779225,
40.1038990521418));
#177782=CARTESIAN_POINT('Ctrl Pts',(-39.5990458505387,43.6825494130771,
40.097736013771));
#177783=CARTESIAN_POINT('Ctrl Pts',(-39.6080010415735,43.679977183279,40.0911601532641));
#177784=CARTESIAN_POINT('Ctrl Pts',(-39.6167795278793,43.6778696350432,
40.084220729064));
#177785=CARTESIAN_POINT('Ctrl Pts',(-39.6255205083453,43.6757710912489,
40.0773109533619));
#177786=CARTESIAN_POINT('Ctrl Pts',(-39.6340863223874,43.6741330170974,
40.0700409753048));
#177787=CARTESIAN_POINT('Ctrl Pts',(-39.6424182201444,43.6729688455956,
40.0624586415899));
#177788=CARTESIAN_POINT('Ctrl Pts',(-39.6424539706902,43.6729638503631,
40.0624261072769));
#177789=CARTESIAN_POINT('Ctrl Pts',(-39.6424897170043,43.6729588633163,
40.0623935677889));
#177790=CARTESIAN_POINT('Ctrl Pts',(-39.6425254590848,43.6729538844542,
40.0623610231289));
#177791=CARTESIAN_POINT('Ctrl Pts',(-39.6593807372525,43.6706059487641,
40.0470135870233));
#177792=CARTESIAN_POINT('Ctrl Pts',(-39.6752678913551,43.6700521164128,
40.0305755292093));
#177793=CARTESIAN_POINT('Ctrl Pts',(-39.6901095551207,43.6711139265065,
40.0133447567339));
#177794=CARTESIAN_POINT('Ctrl Pts',(-39.7054911294111,43.6722143631623,
39.9954871626596));
#177795=CARTESIAN_POINT('Ctrl Pts',(-39.719750522404,43.6750505546838,39.9767767954314));
#177796=CARTESIAN_POINT('Ctrl Pts',(-39.7327754618321,43.6794690223284,
39.9575197577475));
#177797=CARTESIAN_POINT('Ctrl Pts',(-39.7456145061495,43.6838244285257,
39.9385375611999));
#177798=CARTESIAN_POINT('Ctrl Pts',(-39.7572546407969,43.6897180061494,
39.9190226977099));
#177799=CARTESIAN_POINT('Ctrl Pts',(-39.7675538156911,43.6970365387953,
39.8992655451861));
#177800=CARTESIAN_POINT('Ctrl Pts',(-39.7747345836673,43.7021391499652,
39.885490506933));
#177801=CARTESIAN_POINT('Ctrl Pts',(-39.7812627970001,43.707935154852,39.8715976051477));
#177802=CARTESIAN_POINT('Ctrl Pts',(-39.7870778846743,43.7143933160627,
39.8576902534424));
#177803=CARTESIAN_POINT('',(-40.0254908126585,43.9791725362586,39.2875012672119));
#177804=CARTESIAN_POINT('',(-39.7870778846743,43.7143933160627,39.8576902534424));
#177805=CARTESIAN_POINT('',(-43.9791725362579,40.0254908126592,39.2875012672119));
#177806=CARTESIAN_POINT('Origin',(5.53234440788222E-15,0.,39.2875012672119));
#177807=CARTESIAN_POINT('',(-43.714393316062,39.7870778846751,39.8576902534424));
#177808=CARTESIAN_POINT('',(-43.9791725362579,40.0254908126592,39.2875012672119));
#177809=CARTESIAN_POINT('',(-43.7765468711719,39.4370498736012,40.1599502534424));
#177810=CARTESIAN_POINT('Ctrl Pts',(-43.714393316062,39.7870778846751,39.8576902534424));
#177811=CARTESIAN_POINT('Ctrl Pts',(-43.7053047809354,39.7788943382471,
39.8772619994039));
#177812=CARTESIAN_POINT('Ctrl Pts',(-43.6975432007884,39.7693190488203,
39.896764465034));
#177813=CARTESIAN_POINT('Ctrl Pts',(-43.6911816548822,39.7585187839205,
39.9159282836004));
#177814=CARTESIAN_POINT('Ctrl Pts',(-43.6847051962256,39.7475234267957,
39.9354382707133));
#177815=CARTESIAN_POINT('Ctrl Pts',(-43.6796790973022,39.7352578445729,
39.9545987622292));
#177816=CARTESIAN_POINT('Ctrl Pts',(-43.6762098455857,39.7218536055436,
39.9731387498159));
#177817=CARTESIAN_POINT('Ctrl Pts',(-43.6728874729921,39.7090168672409,
39.9908938023977));
#177818=CARTESIAN_POINT('Ctrl Pts',(-43.6709925938766,39.6951350414567,
40.0080810366098));
#177819=CARTESIAN_POINT('Ctrl Pts',(-43.6706524194394,39.6802941970576,
40.0244542742451));
#177820=CARTESIAN_POINT('Ctrl Pts',(-43.6703818558784,39.6684902774488,
40.0374770090428));
#177821=CARTESIAN_POINT('Ctrl Pts',(-43.6710953426067,39.6560790233743,
40.0499848770011));
#177822=CARTESIAN_POINT('Ctrl Pts',(-43.6728752976391,39.6430941754572,
40.0618424270193));
#177823=CARTESIAN_POINT('Ctrl Pts',(-43.6728801563381,39.6430587310403,
40.0618747942791));
#177824=CARTESIAN_POINT('Ctrl Pts',(-43.6728850230943,39.6430232824886,
40.0619071564124));
#177825=CARTESIAN_POINT('Ctrl Pts',(-43.6728898979086,39.6429878298038,
40.0619395134161));
#177826=CARTESIAN_POINT('Ctrl Pts',(-43.6738603187593,39.6359303251675,
40.0683807661799));
#177827=CARTESIAN_POINT('Ctrl Pts',(-43.6751791606252,39.6286869425435,
40.0746073439084));
#177828=CARTESIAN_POINT('Ctrl Pts',(-43.6768375203041,39.6212972007505,
40.0805869293669));
#177829=CARTESIAN_POINT('Ctrl Pts',(-43.6801286499317,39.6066317464085,
40.092453830807));
#177830=CARTESIAN_POINT('Ctrl Pts',(-43.684758095089,39.5913890092852,40.1033475319609));
#177831=CARTESIAN_POINT('Ctrl Pts',(-43.6906629735749,39.575872843854,40.1130129263075));
#177832=CARTESIAN_POINT('Ctrl Pts',(-43.6950916324393,39.5642357197806,
40.1202619720674));
#177833=CARTESIAN_POINT('Ctrl Pts',(-43.7002377219525,39.5524447917349,
40.1268200947266));
#177834=CARTESIAN_POINT('Ctrl Pts',(-43.7060747220668,39.5406282559961,
40.1325796782703));
#177835=CARTESIAN_POINT('Ctrl Pts',(-43.7082635971097,39.5361970550941,
40.1347395220992));
#177836=CARTESIAN_POINT('Ctrl Pts',(-43.7105496315973,39.5317622532396,
40.1367870714852));
#177837=CARTESIAN_POINT('Ctrl Pts',(-43.7129314276126,39.5273306113318,
40.1387166518767));
#177838=CARTESIAN_POINT('Ctrl Pts',(-43.7212677136663,39.5118198646544,
40.1454701832469));
#177839=CARTESIAN_POINT('Ctrl Pts',(-43.7307770746559,39.4963478239303,
40.1507785912492));
#177840=CARTESIAN_POINT('Ctrl Pts',(-43.741399609424,39.481204393873,40.1543986087265));
#177841=CARTESIAN_POINT('Ctrl Pts',(-43.746710876808,39.4736326788443,40.1562086174652));
#177842=CARTESIAN_POINT('Ctrl Pts',(-43.7523004383954,39.4661431171624,
40.1575965292115));
#177843=CARTESIAN_POINT('Ctrl Pts',(-43.7581608097794,39.4587719497941,
40.1585319382567));
#177844=CARTESIAN_POINT('Ctrl Pts',(-43.7610909954714,39.4550863661099,
40.1589996427793));
#177845=CARTESIAN_POINT('Ctrl Pts',(-43.7640888836317,39.451430381021,40.159354221642));
#177846=CARTESIAN_POINT('Ctrl Pts',(-43.7671535389273,39.4478085248416,
40.159591874311));
#177847=CARTESIAN_POINT('Ctrl Pts',(-43.7702181942229,39.4441866686622,
40.1598295269801));
#177848=CARTESIAN_POINT('Ctrl Pts',(-43.7733496179165,39.4405989425299,
40.1599502506895));
#177849=CARTESIAN_POINT('Ctrl Pts',(-43.7765468711719,39.4370498736012,
40.1599502534424));
#177850=CARTESIAN_POINT('',(-43.7969047596343,39.4144401478993,40.1599502534424));
#177851=CARTESIAN_POINT('Origin',(3.51858511112452E-16,4.55906712132165E-17,
40.1599502534424));
#177852=CARTESIAN_POINT('',(-44.1385184650372,39.3160391863694,39.8576902534424));
#177853=CARTESIAN_POINT('Ctrl Pts',(-43.7969047596343,39.4144401478993,
40.1599502534424));
#177854=CARTESIAN_POINT('Ctrl Pts',(-43.7994532913547,39.4116082546733,
40.1599502448875));
#177855=CARTESIAN_POINT('Ctrl Pts',(-43.8020298032735,39.4088155471155,
40.1598743450437));
#177856=CARTESIAN_POINT('Ctrl Pts',(-43.8046321918099,39.4060627300846,
40.1597243308499));
#177857=CARTESIAN_POINT('Ctrl Pts',(-43.8199964969272,39.3898103065117,
40.1588386583939));
#177858=CARTESIAN_POINT('Ctrl Pts',(-43.8362633193843,39.3749452320426,
40.1553722553621));
#177859=CARTESIAN_POINT('Ctrl Pts',(-43.8529956277688,39.3616178931512,
40.1496902177795));
#177860=CARTESIAN_POINT('Ctrl Pts',(-43.8592462611885,39.356639242988,40.1475675976849));
#177861=CARTESIAN_POINT('Ctrl Pts',(-43.8655619201088,39.3518747760142,
40.1451361443099));
#177862=CARTESIAN_POINT('Ctrl Pts',(-43.8719202087609,39.3473309185528,
40.1424159447501));
#177863=CARTESIAN_POINT('Ctrl Pts',(-43.8768812645305,39.343785573019,40.1402935085949));
#177864=CARTESIAN_POINT('Ctrl Pts',(-43.881868143321,39.3403750229162,40.1379949176048));
#177865=CARTESIAN_POINT('Ctrl Pts',(-43.8868700682404,39.3371028088667,
40.1355293609261));
#177866=CARTESIAN_POINT('Ctrl Pts',(-43.9043768054583,39.3256500596932,
40.1268999125509));
#177867=CARTESIAN_POINT('Ctrl Pts',(-43.9220678510593,39.3158919212387,
40.1162251288835));
#177868=CARTESIAN_POINT('Ctrl Pts',(-43.9394812142299,39.3079802585393,
40.1038990521418));
#177869=CARTESIAN_POINT('Ctrl Pts',(-43.9481878958152,39.3040244271896,
40.097736013771));
#177870=CARTESIAN_POINT('Ctrl Pts',(-43.9568251581486,39.3005302159783,
40.0911601532641));
#177871=CARTESIAN_POINT('Ctrl Pts',(-43.9653352562096,39.2975166114288,
40.084220729064));
#177872=CARTESIAN_POINT('Ctrl Pts',(-43.973808995112,39.2945158824214,40.0773109533619));
#177873=CARTESIAN_POINT('Ctrl Pts',(-43.9821566593547,39.2919914104332,
40.0700409753048));
#177874=CARTESIAN_POINT('Ctrl Pts',(-43.990321225046,39.289962695916,40.0624586415899));
#177875=CARTESIAN_POINT('Ctrl Pts',(-43.9903562576026,39.2899539910983,
40.0624261072769));
#177876=CARTESIAN_POINT('Ctrl Pts',(-43.9903912868063,39.2899452948638,
40.0623935677888));
#177877=CARTESIAN_POINT('Ctrl Pts',(-43.9904263126551,39.2899366072116,
40.0623610231288));
#177878=CARTESIAN_POINT('Ctrl Pts',(-44.0069438297354,39.2858396774342,
40.0470135870238));
#177879=CARTESIAN_POINT('Ctrl Pts',(-44.0226860611005,39.2836282192304,
40.0305755292104));
#177880=CARTESIAN_POINT('Ctrl Pts',(-44.037557410056,39.2831328363114,40.0133447567356));
#177881=CARTESIAN_POINT('Ctrl Pts',(-44.052969749425,39.2826194323366,39.9954871626623));
#177882=CARTESIAN_POINT('Ctrl Pts',(-44.0674474907118,39.2839495744672,
39.9767767954353));
#177883=CARTESIAN_POINT('Ctrl Pts',(-44.0808629337912,39.2869823603807,
39.9575197577525));
#177884=CARTESIAN_POINT('Ctrl Pts',(-44.0940869083964,39.2899718616342,
39.9385375612064));
#177885=CARTESIAN_POINT('Ctrl Pts',(-44.1062793237798,39.2946164282353,
39.919022697718));
#177886=CARTESIAN_POINT('Ctrl Pts',(-44.1172870736866,39.3008183122681,
39.8992655451958));
#177887=CARTESIAN_POINT('Ctrl Pts',(-44.1249618727708,39.3051423761592,
39.8854905069395));
#177888=CARTESIAN_POINT('Ctrl Pts',(-44.1320601713535,39.3102242458184,
39.8715976051509));
#177889=CARTESIAN_POINT('Ctrl Pts',(-44.1385184650372,39.3160391863694,
39.8576902534424));
#177890=CARTESIAN_POINT('',(-44.4033023070486,39.5544469813075,39.2875012672119));
#177891=CARTESIAN_POINT('',(-44.1385184650372,39.3160391863694,39.8576902534424));
#177892=CARTESIAN_POINT('',(-47.9220530736684,35.2091516650532,39.2875012672119));
#177893=CARTESIAN_POINT('Origin',(5.53234440788222E-15,0.,39.2875012672119));
#177894=CARTESIAN_POINT('',(-47.6338034047597,34.9997217530264,39.8576902534424));
#177895=CARTESIAN_POINT('',(-47.9220530736684,35.2091516650532,39.2875012672119));
#177896=CARTESIAN_POINT('',(-47.6590285860933,34.645114416419,40.1599502534424));
#177897=CARTESIAN_POINT('Ctrl Pts',(-47.6338034047597,34.9997217530264,
39.8576902534424));
#177898=CARTESIAN_POINT('Ctrl Pts',(-47.6239092440465,34.9925330475316,
39.8772619994054));
#177899=CARTESIAN_POINT('Ctrl Pts',(-47.615189292358,34.9838215185866,39.8967644650371));
#177900=CARTESIAN_POINT('Ctrl Pts',(-47.6077336605726,34.9737453812845,
39.9159282836049));
#177901=CARTESIAN_POINT('Ctrl Pts',(-47.6001433528505,34.9634872321464,
39.9354382707192));
#177902=CARTESIAN_POINT('Ctrl Pts',(-47.5938626849619,34.9518142124619,
39.9545987622365));
#177903=CARTESIAN_POINT('Ctrl Pts',(-47.5890113136624,34.9388460388056,
39.9731387498244));
#177904=CARTESIAN_POINT('Ctrl Pts',(-47.5843653368453,34.9264269039989,
39.9908938024073));
#177905=CARTESIAN_POINT('Ctrl Pts',(-47.5810297921596,34.9128191931094,
40.0080810366204));
#177906=CARTESIAN_POINT('Ctrl Pts',(-47.5791401905755,34.8980952063184,
40.0244542742565));
#177907=CARTESIAN_POINT('Ctrl Pts',(-47.5776372636137,34.8863842314125,
40.0374770090501));
#177908=CARTESIAN_POINT('Ctrl Pts',(-47.5770495124718,34.8739663878185,
40.0499848770046));
#177909=CARTESIAN_POINT('Ctrl Pts',(-47.5774624305257,34.8608666162966,
40.0618424270193));
#177910=CARTESIAN_POINT('Ctrl Pts',(-47.5774635576578,34.8608308581755,
40.0618747942791));
#177911=CARTESIAN_POINT('Ctrl Pts',(-47.5774646923707,34.8607950951002,
40.0619071564124));
#177912=CARTESIAN_POINT('Ctrl Pts',(-47.5774658346656,34.860759327072,40.0619395134161));
#177913=CARTESIAN_POINT('Ctrl Pts',(-47.5776932293352,34.8536390475843,
40.0683807661799));
#177914=CARTESIAN_POINT('Ctrl Pts',(-47.5782477067929,34.8462974884547,
40.0746073439084));
#177915=CARTESIAN_POINT('Ctrl Pts',(-47.5791245434504,34.8387748826516,
40.0805869293669));
#177916=CARTESIAN_POINT('Ctrl Pts',(-47.58086468652,34.8238457504806,40.092453830807));
#177917=CARTESIAN_POINT('Ctrl Pts',(-47.5838754712049,34.8082026058781,
40.1033475319609));
#177918=CARTESIAN_POINT('Ctrl Pts',(-47.5881261212203,34.7921542117507,
40.1130129263075));
#177919=CARTESIAN_POINT('Ctrl Pts',(-47.5913141087318,34.7801179161552,
40.1202619720674));
#177920=CARTESIAN_POINT('Ctrl Pts',(-47.5951995198391,34.7678536672184,
40.1268200947266));
#177921=CARTESIAN_POINT('Ctrl Pts',(-47.5997693799341,34.7554917310467,
40.1325796782703));
#177922=CARTESIAN_POINT('Ctrl Pts',(-47.6014830774698,34.7508560049823,
40.1347395220992));
#177923=CARTESIAN_POINT('Ctrl Pts',(-47.6032930257985,34.7462065417645,
40.1367870714852));
#177924=CARTESIAN_POINT('Ctrl Pts',(-47.6051985413677,34.7415502113774,
40.1387166518767));
#177925=CARTESIAN_POINT('Ctrl Pts',(-47.6118678458598,34.7252530550227,
40.1454701832469));
#177926=CARTESIAN_POINT('Ctrl Pts',(-47.6197078449344,34.7088717728656,
40.1507785912492));
#177927=CARTESIAN_POINT('Ctrl Pts',(-47.6286892688731,34.6927009428673,
40.1543986087265));
#177928=CARTESIAN_POINT('Ctrl Pts',(-47.6331799808424,34.6846155278682,
40.1562086174652));
#177929=CARTESIAN_POINT('Ctrl Pts',(-47.6379560498533,34.6765827265057,
40.1575965292115));
#177930=CARTESIAN_POINT('Ctrl Pts',(-47.6430138207122,34.6686393635485,
40.1585319382567));
#177931=CARTESIAN_POINT('Ctrl Pts',(-47.6455427061417,34.66466768207,40.1589996427793));
#177932=CARTESIAN_POINT('Ctrl Pts',(-47.6481420170539,34.6607183602074,
40.159354221642));
#177933=CARTESIAN_POINT('Ctrl Pts',(-47.6508112967866,34.6567960012267,
40.159591874311));
#177934=CARTESIAN_POINT('Ctrl Pts',(-47.6534805765192,34.6528736422459,
40.1598295269801));
#177935=CARTESIAN_POINT('Ctrl Pts',(-47.6562198264469,34.6489782471462,
40.1599502506895));
#177936=CARTESIAN_POINT('Ctrl Pts',(-47.6590285860933,34.645114416419,40.1599502534424));
#177937=CARTESIAN_POINT('',(-47.6769115920301,34.6205005703638,40.1599502534424));
#177938=CARTESIAN_POINT('Origin',(3.4737036430558E-16,4.0048271483298E-17,
40.1599502534424));
#177939=CARTESIAN_POINT('',(-48.0063682005184,34.4869303039401,39.8576902534424));
#177940=CARTESIAN_POINT('Ctrl Pts',(-47.6769115920301,34.6205005703638,
40.1599502534424));
#177941=CARTESIAN_POINT('Ctrl Pts',(-47.67915014918,34.6174177964409,40.1599502448875));
#177942=CARTESIAN_POINT('Ctrl Pts',(-47.6814206292676,34.6143710687958,
40.1598743450437));
#177943=CARTESIAN_POINT('Ctrl Pts',(-47.6837210139133,34.6113613083102,
40.1597243308499));
#177944=CARTESIAN_POINT('Ctrl Pts',(-47.6973023108995,34.5935919100107,
40.1588386583939));
#177945=CARTESIAN_POINT('Ctrl Pts',(-47.7119261986107,34.5771079220209,
40.1553722553619));
#177946=CARTESIAN_POINT('Ctrl Pts',(-47.7271737594057,34.5621045892039,
40.1496902177792));
#177947=CARTESIAN_POINT('Ctrl Pts',(-47.7328697405506,34.5564998435016,
40.1475675976847));
#177948=CARTESIAN_POINT('Ctrl Pts',(-47.7386527792192,34.5511013106553,
40.1451361443098));
#177949=CARTESIAN_POINT('Ctrl Pts',(-47.7445012740627,34.5459177227789,
40.1424159447501));
#177950=CARTESIAN_POINT('Ctrl Pts',(-47.7490645631294,34.5418732274831,
40.1402935085949));
#177951=CARTESIAN_POINT('Ctrl Pts',(-47.7536676237148,34.5379600899542,
40.1379949176048));
#177952=CARTESIAN_POINT('Ctrl Pts',(-47.7583001080601,34.5341829579103,
40.1355293609261));
#177953=CARTESIAN_POINT('Ctrl Pts',(-47.7745138032685,34.520962995757,40.1268999125509));
#177954=CARTESIAN_POINT('Ctrl Pts',(-47.7910879322536,34.5094090955956,
40.1162251288835));
#177955=CARTESIAN_POINT('Ctrl Pts',(-47.8075789092549,34.4997205817197,
40.1038990521418));
#177956=CARTESIAN_POINT('Ctrl Pts',(-47.8158243977556,34.4948763247818,
40.0977360137709));
#177957=CARTESIAN_POINT('Ctrl Pts',(-47.8240490997339,34.4904984154666,
40.0911601532641));
#177958=CARTESIAN_POINT('Ctrl Pts',(-47.8321975711348,34.4866117722856,
40.084220729064));
#177959=CARTESIAN_POINT('Ctrl Pts',(-47.8403112284171,34.4827417346801,
40.0773109533618));
#177960=CARTESIAN_POINT('Ctrl Pts',(-47.8483492841042,34.4793585234984,
40.0700409753048));
#177961=CARTESIAN_POINT('Ctrl Pts',(-47.8562570650395,34.4764874929866,
40.0624586415899));
#177962=CARTESIAN_POINT('Ctrl Pts',(-47.8562909957829,34.4764751739554,
40.0624261072769));
#177963=CARTESIAN_POINT('Ctrl Pts',(-47.8563249240888,34.4764628638111,
40.0623935677888));
#177964=CARTESIAN_POINT('Ctrl Pts',(-47.8563588499555,34.4764505625526,
40.0623610231288));
#177965=CARTESIAN_POINT('Ctrl Pts',(-47.8723576365755,34.4706495255077,
40.0470135870235));
#177966=CARTESIAN_POINT('Ctrl Pts',(-47.8877824700227,34.4668046706503,
40.0305755292097));
#177967=CARTESIAN_POINT('Ctrl Pts',(-47.9025205705575,34.464757522238,40.0133447567346));
#177968=CARTESIAN_POINT('Ctrl Pts',(-47.9177948141909,34.4626359025944,
39.9954871626604));
#177969=CARTESIAN_POINT('Ctrl Pts',(-47.9323322826094,34.4624454220193,
39.9767767954324));
#177970=CARTESIAN_POINT('Ctrl Pts',(-47.9459912469394,34.4640592983654,
39.9575197577486));
#177971=CARTESIAN_POINT('Ctrl Pts',(-47.959455267201,34.465650141075,39.9385375612008));
#177972=CARTESIAN_POINT('Ctrl Pts',(-47.9720663806674,34.4689948098114,
39.9190226977106));
#177973=CARTESIAN_POINT('Ctrl Pts',(-47.9836621023766,34.4740120960936,
39.8992655451867));
#177974=CARTESIAN_POINT('Ctrl Pts',(-47.9917468458601,34.4775102373556,
39.8854905069333));
#177975=CARTESIAN_POINT('Ctrl Pts',(-47.9993374592447,34.4818222937574,
39.8715976051478));
#177976=CARTESIAN_POINT('Ctrl Pts',(-48.0063682005184,34.4869303039401,
39.8576902534424));
#177977=CARTESIAN_POINT('',(-48.2946219293743,34.6963546279289,39.2875012672119));
#177978=CARTESIAN_POINT('',(-48.0063682005184,34.4869303039401,39.8576902534424));
#177979=CARTESIAN_POINT('',(-51.3398895692695,30.0070536838162,39.2875012672119));
#177980=CARTESIAN_POINT('Origin',(5.53234440788222E-15,0.,39.2875012672119));
#177981=CARTESIAN_POINT('',(-51.0313275753406,29.828901345689,39.8576902534424));
#177982=CARTESIAN_POINT('',(-51.3398895692695,30.0070536838162,39.2875012672119));
#177983=CARTESIAN_POINT('',(-51.0193480105325,29.4735998357342,40.1599502534424));
#177984=CARTESIAN_POINT('Ctrl Pts',(-51.0313275753406,29.828901345689,39.8576902534424));
#177985=CARTESIAN_POINT('Ctrl Pts',(-51.020736191538,29.8227862420905,39.8772619994031));
#177986=CARTESIAN_POINT('Ctrl Pts',(-51.0111534059249,29.8150339189635,
39.8967644650325));
#177987=CARTESIAN_POINT('Ctrl Pts',(-51.0026853737234,29.8057923055305,
39.9159282835982));
#177988=CARTESIAN_POINT('Ctrl Pts',(-50.9940643779364,29.79638375481,39.9354382707104));
#177989=CARTESIAN_POINT('Ctrl Pts',(-50.9865979533948,29.7854311897131,
39.9545987622257));
#177990=CARTESIAN_POINT('Ctrl Pts',(-50.9804176151513,29.7730411634577,
39.9731387498119));
#177991=CARTESIAN_POINT('Ctrl Pts',(-50.974498936405,29.7611756987897,39.9908938023933));
#177992=CARTESIAN_POINT('Ctrl Pts',(-50.969759271074,29.7479911917264,40.0080810366051));
#177993=CARTESIAN_POINT('Ctrl Pts',(-50.966340945212,29.7335453816275,40.0244542742402));
#177994=CARTESIAN_POINT('Ctrl Pts',(-50.9636221212293,29.7220556593091,
40.0374770090397));
#177995=CARTESIAN_POINT('Ctrl Pts',(-50.9617395717405,29.7097672786805,
40.0499848769996));
#177996=CARTESIAN_POINT('Ctrl Pts',(-50.9607809287993,29.6966961073824,
40.0618424270193));
#177997=CARTESIAN_POINT('Ctrl Pts',(-50.9607783120155,29.6966604273307,
40.0618747942791));
#177998=CARTESIAN_POINT('Ctrl Pts',(-50.960775702253,29.6966247415594,40.0619071564124));
#177999=CARTESIAN_POINT('Ctrl Pts',(-50.9607730995133,29.69658905007,40.0619395134161));
#178000=CARTESIAN_POINT('Ctrl Pts',(-50.9602549766182,29.6894840070029,
40.0683807661799));
#178001=CARTESIAN_POINT('Ctrl Pts',(-50.9600390146965,29.6821247070258,
40.0746073439084));
#178002=CARTESIAN_POINT('Ctrl Pts',(-50.9601247215268,29.6745516564561,
40.0805869293669));
#178003=CARTESIAN_POINT('Ctrl Pts',(-50.9602948126668,29.6595224131522,
40.092453830807));
#178004=CARTESIAN_POINT('Ctrl Pts',(-50.9616539500922,29.6436502506363,
40.1033475319609));
#178005=CARTESIAN_POINT('Ctrl Pts',(-50.964203800626,29.6272454573771,40.1130129263075));
#178006=CARTESIAN_POINT('Ctrl Pts',(-50.9661161885263,29.6149418624327,
40.1202619720674));
#178007=CARTESIAN_POINT('Ctrl Pts',(-50.9686983518505,29.6023386622826,
40.1268200947266));
#178008=CARTESIAN_POINT('Ctrl Pts',(-50.9719510035827,29.5895667656377,
40.1325796782703));
#178009=CARTESIAN_POINT('Ctrl Pts',(-50.9731707479823,29.5847773043958,
40.1347395220992));
#178010=CARTESIAN_POINT('Ctrl Pts',(-50.9744847799795,29.5799641203066,
40.1367870714852));
#178011=CARTESIAN_POINT('Ctrl Pts',(-50.9758931378752,29.5751341171704,
40.1387166518767));
#178012=CARTESIAN_POINT('Ctrl Pts',(-50.9808223905102,29.5582291061937,
40.1454701832469));
#178013=CARTESIAN_POINT('Ctrl Pts',(-50.9869071309993,29.541118059359,40.1507785912492));
#178014=CARTESIAN_POINT('Ctrl Pts',(-50.9941490417484,29.5240970004172,
40.1543986087265));
#178015=CARTESIAN_POINT('Ctrl Pts',(-50.9977699971229,29.5155864709463,
40.1562086174652));
#178016=CARTESIAN_POINT('Ctrl Pts',(-51.001680245946,29.507098438956,40.1575965292115));
#178017=CARTESIAN_POINT('Ctrl Pts',(-51.0058800022838,29.4986699095568,
40.1585319382567));
#178018=CARTESIAN_POINT('Ctrl Pts',(-51.0079798804527,29.4944556448572,
40.1589996427793));
#178019=CARTESIAN_POINT('Ctrl Pts',(-51.0101521355226,29.4902562558179,
40.159354221642));
#178020=CARTESIAN_POINT('Ctrl Pts',(-51.0123967945049,29.4860763682215,
40.159591874311));
#178021=CARTESIAN_POINT('Ctrl Pts',(-51.0146414534873,29.4818964806251,
40.1598295269801));
#178022=CARTESIAN_POINT('Ctrl Pts',(-51.0169585178536,29.477736095322,40.1599502506896));
#178023=CARTESIAN_POINT('Ctrl Pts',(-51.0193480105325,29.4735998357342,
40.1599502534424));
#178024=CARTESIAN_POINT('',(-51.0345602039884,29.447251543774,40.1599502534424));
#178025=CARTESIAN_POINT('Origin',(3.43486142563102E-16,3.40670945103694E-17,
40.1599502534424));
#178026=CARTESIAN_POINT('',(-51.3482501200163,29.2799753962467,39.8576902534424));
#178027=CARTESIAN_POINT('Ctrl Pts',(-51.0345602039884,29.447251543774,40.1599502534424));
#178028=CARTESIAN_POINT('Ctrl Pts',(-51.0364642604673,29.4439516646703,
40.1599502448875));
#178029=CARTESIAN_POINT('Ctrl Pts',(-51.0384038328686,29.4406842975236,
40.1598743450437));
#178030=CARTESIAN_POINT('Ctrl Pts',(-51.0403770101282,29.4374505691489,
40.1597243308499));
#178031=CARTESIAN_POINT('Ctrl Pts',(-51.0520264994498,29.4183588813712,
40.158838658394));
#178032=CARTESIAN_POINT('Ctrl Pts',(-51.0648472300397,29.4004365818846,
40.1553722553626));
#178033=CARTESIAN_POINT('Ctrl Pts',(-51.0784429877766,29.3839216347975,
40.1496902177808));
#178034=CARTESIAN_POINT('Ctrl Pts',(-51.0835219102867,29.377752200321,40.1475675976859));
#178035=CARTESIAN_POINT('Ctrl Pts',(-51.0887089685234,29.3717787490558,
40.1451361443104));
#178036=CARTESIAN_POINT('Ctrl Pts',(-51.0939835922267,29.3660122232363,
40.14241594475));
#178037=CARTESIAN_POINT('Ctrl Pts',(-51.0980991182404,29.3615128905153,
40.1402935085948));
#178038=CARTESIAN_POINT('Ctrl Pts',(-51.1022679285259,29.3571400387138,
40.1379949176048));
#178039=CARTESIAN_POINT('Ctrl Pts',(-51.1064802178291,29.3528993717248,
40.1355293609261));
#178040=CARTESIAN_POINT('Ctrl Pts',(-51.1212232303903,29.3380570372633,
40.1268999125509));
#178041=CARTESIAN_POINT('Ctrl Pts',(-51.1364988531341,29.3248339623431,
40.1162251288835));
#178042=CARTESIAN_POINT('Ctrl Pts',(-51.1518867653711,29.3134747466763,
40.1038990521418));
#178043=CARTESIAN_POINT('Ctrl Pts',(-51.1595807214896,29.3077951388428,
40.0977360137709));
#178044=CARTESIAN_POINT('Ctrl Pts',(-51.1673027515569,29.3025814967143,
40.0911601532641));
#178045=CARTESIAN_POINT('Ctrl Pts',(-51.1750003199399,29.2978643977778,
40.084220729064));
#178046=CARTESIAN_POINT('Ctrl Pts',(-51.182665000675,29.293167452516,40.0773109533618));
#178047=CARTESIAN_POINT('Ctrl Pts',(-51.1903053811862,29.2889625693105,
40.0700409753047));
#178048=CARTESIAN_POINT('Ctrl Pts',(-51.1978697380627,29.2852806784153,
40.0624586415899));
#178049=CARTESIAN_POINT('Ctrl Pts',(-51.1979021952406,29.2852648801406,
40.0624261072769));
#178050=CARTESIAN_POINT('Ctrl Pts',(-51.1979346509233,29.2852490909588,
40.0623935677888));
#178051=CARTESIAN_POINT('Ctrl Pts',(-51.1979671051088,29.2852333108692,
40.0623610231288));
#178052=CARTESIAN_POINT('Ctrl Pts',(-51.2132718752125,29.2777917239334,
40.0470135870251));
#178053=CARTESIAN_POINT('Ctrl Pts',(-51.228210313037,29.2723555974571,40.030575529213));
#178054=CARTESIAN_POINT('Ctrl Pts',(-51.2426536914361,29.2687791125375,
40.0133447567398));
#178055=CARTESIAN_POINT('Ctrl Pts',(-51.2576224915221,29.2650725221337,
39.9954871626678));
#178056=CARTESIAN_POINT('Ctrl Pts',(-51.2720604115243,29.2633635057969,
39.9767767954423));
#178057=CARTESIAN_POINT('Ctrl Pts',(-51.2858132466317,29.2635407906075,
39.957519757761));
#178058=CARTESIAN_POINT('Ctrl Pts',(-51.2993697979237,29.263715545166,39.9385375612159));
#178059=CARTESIAN_POINT('Ctrl Pts',(-51.312261439473,29.265723671145,39.9190226977285));
#178060=CARTESIAN_POINT('Ctrl Pts',(-51.3243180878291,29.2695013892356,
39.8992655452074));
#178061=CARTESIAN_POINT('Ctrl Pts',(-51.3327241975769,29.2721352815021,
39.8854905069473));
#178062=CARTESIAN_POINT('Ctrl Pts',(-51.3407239614206,29.2756302808568,
39.8715976051548));
#178063=CARTESIAN_POINT('Ctrl Pts',(-51.3482501200163,29.2799753962467,
39.8576902534424));
#178064=CARTESIAN_POINT('',(-51.6568155675425,29.4581217525678,39.2875012672119));
#178065=CARTESIAN_POINT('',(-51.3482501200163,29.2799753962467,39.8576902534424));
#178066=CARTESIAN_POINT('',(-54.195235491187,24.4761921430396,39.2875012672119));
#178067=CARTESIAN_POINT('Origin',(5.53234440788222E-15,0.,39.2875012672119));
#178068=CARTESIAN_POINT('',(-53.8697418420143,24.3312692531092,39.8576902534424));
#178069=CARTESIAN_POINT('',(-54.195235491187,24.4761921430396,39.2875012672119));
#178070=CARTESIAN_POINT('',(-53.8206887816834,23.9791663275018,40.1599502534424));
#178071=CARTESIAN_POINT('Ctrl Pts',(-53.8697418420143,24.3312692531092,
39.8576902534424));
#178072=CARTESIAN_POINT('Ctrl Pts',(-53.8585692765373,24.3262947497602,
39.8772619994052));
#178073=CARTESIAN_POINT('Ctrl Pts',(-53.8482286480022,24.3195865685235,
39.8967644650367));
#178074=CARTESIAN_POINT('Ctrl Pts',(-53.838840992916,24.3112807320075,39.9159282836044));
#178075=CARTESIAN_POINT('Ctrl Pts',(-53.8292837624968,24.3028248617525,
39.9354382707186));
#178076=CARTESIAN_POINT('Ctrl Pts',(-53.8207133850111,24.2927127498351,
39.9545987622357));
#178077=CARTESIAN_POINT('Ctrl Pts',(-53.8132717929025,24.2810366186971,
39.9731387498236));
#178078=CARTESIAN_POINT('Ctrl Pts',(-53.8061452585097,24.2698548246783,
39.9908938024065));
#178079=CARTESIAN_POINT('Ctrl Pts',(-53.800053401299,24.2572379736556,40.0080810366196));
#178080=CARTESIAN_POINT('Ctrl Pts',(-53.7951438030538,24.2432286115631,
40.0244542742558));
#178081=CARTESIAN_POINT('Ctrl Pts',(-53.7912388700581,24.2320860256422,
40.0374770090497));
#178082=CARTESIAN_POINT('Ctrl Pts',(-53.7880821478309,24.220061742058,40.0499848770043));
#178083=CARTESIAN_POINT('Ctrl Pts',(-53.7857624469881,24.2071623814826,
40.0618424270193));
#178084=CARTESIAN_POINT('Ctrl Pts',(-53.7857561149583,24.2071271704184,
40.0618747942791));
#178085=CARTESIAN_POINT('Ctrl Pts',(-53.7857497893135,24.207091952932,40.0619071564124));
#178086=CARTESIAN_POINT('Ctrl Pts',(-53.7857434700554,24.2070567290246,
40.0619395134161));
#178087=CARTESIAN_POINT('Ctrl Pts',(-53.7844855062584,24.2000447667169,
40.0683807661799));
#178088=CARTESIAN_POINT('Ctrl Pts',(-53.7835014710814,24.1927483559228,
40.0746073439084));
#178089=CARTESIAN_POINT('Ctrl Pts',(-53.7827951090624,24.1852078325133,
40.0805869293669));
#178090=CARTESIAN_POINT('Ctrl Pts',(-53.7813932847187,24.1702431416113,
40.092453830807));
#178091=CARTESIAN_POINT('Ctrl Pts',(-53.7810858838905,24.1543158599159,
40.1033475319609));
#178092=CARTESIAN_POINT('Ctrl Pts',(-53.7819069982467,24.1377344018728,
40.1130129263075));
#178093=CARTESIAN_POINT('Ctrl Pts',(-53.7825228340138,24.1252983083405,
40.1202619720674));
#178094=CARTESIAN_POINT('Ctrl Pts',(-53.7837734588332,24.1124942402753,
40.1268200947266));
#178095=CARTESIAN_POINT('Ctrl Pts',(-53.7856732654696,24.0994523147294,
40.1325796782703));
#178096=CARTESIAN_POINT('Ctrl Pts',(-53.7863856929583,24.0945615926497,
40.1347395220992));
#178097=CARTESIAN_POINT('Ctrl Pts',(-53.7871894118144,24.0896374219411,
40.1367870714852));
#178098=CARTESIAN_POINT('Ctrl Pts',(-53.7880851817728,24.0846866645809,
40.1387166518767));
#178099=CARTESIAN_POINT('Ctrl Pts',(-53.7912203766271,24.0673590138202,
40.1454701832469));
#178100=CARTESIAN_POINT('Ctrl Pts',(-53.7954831928407,24.0497056745177,
40.1507785912492));
#178101=CARTESIAN_POINT('Ctrl Pts',(-53.8009062465106,24.032020872916,40.1543986087265));
#178102=CARTESIAN_POINT('Ctrl Pts',(-53.8036177733455,24.0231784721152,
40.1562086174652));
#178103=CARTESIAN_POINT('Ctrl Pts',(-53.8066193604763,24.0143282061517,
40.1575965292115));
#178104=CARTESIAN_POINT('Ctrl Pts',(-53.8099150888837,24.0055068550424,
40.1585319382567));
#178105=CARTESIAN_POINT('Ctrl Pts',(-53.8115629530875,24.0010961794877,
40.1589996427793));
#178106=CARTESIAN_POINT('Ctrl Pts',(-53.8132843526339,23.9966927326566,
40.159354221642));
#178107=CARTESIAN_POINT('Ctrl Pts',(-53.8150797979123,23.9923011121679,
40.159591874311));
#178108=CARTESIAN_POINT('Ctrl Pts',(-53.8168752431908,23.9879094916792,
40.1598295269801));
#178109=CARTESIAN_POINT('Ctrl Pts',(-53.8187447357538,23.9835296982245,
40.1599502506895));
#178110=CARTESIAN_POINT('Ctrl Pts',(-53.8206887816834,23.9791663275018,
40.1599502534424));
#178111=CARTESIAN_POINT('',(-53.8330634946836,23.9513722670369,40.1599502534424));
#178112=CARTESIAN_POINT('Origin',(3.40248402231257E-16,2.77126713209872E-17,
40.1599502534424));
#178113=CARTESIAN_POINT('',(-54.1275498658872,23.7522229508832,39.8576902534424));
#178114=CARTESIAN_POINT('Ctrl Pts',(-53.8330634946836,23.9513722670369,
40.1599502534424));
#178115=CARTESIAN_POINT('Ctrl Pts',(-53.8346121892501,23.9478914369185,
40.1599502448875));
#178116=CARTESIAN_POINT('Ctrl Pts',(-53.8361996036041,23.9444392282284,
40.1598743450437));
#178117=CARTESIAN_POINT('Ctrl Pts',(-53.8378239549346,23.9410169613694,
40.1597243308499));
#178118=CARTESIAN_POINT('Ctrl Pts',(-53.8474140023496,23.9208121566398,
40.158838658394));
#178119=CARTESIAN_POINT('Ctrl Pts',(-53.8582911092114,23.9016479061198,
40.1553722553631));
#178120=CARTESIAN_POINT('Ctrl Pts',(-53.8700861059238,23.8838022859786,
40.1496902177821));
#178121=CARTESIAN_POINT('Ctrl Pts',(-53.8744923240608,23.8771357563434,
40.1475675976869));
#178122=CARTESIAN_POINT('Ctrl Pts',(-53.8790265713694,23.8706528330416,
40.145136144311));
#178123=CARTESIAN_POINT('Ctrl Pts',(-53.8836695340507,23.8643665485426,
40.1424159447501));
#178124=CARTESIAN_POINT('Ctrl Pts',(-53.8872922064473,23.8594616740273,
40.1402935085949));
#178125=CARTESIAN_POINT('Ctrl Pts',(-53.8909810920749,23.8546770178327,
40.1379949176048));
#178126=CARTESIAN_POINT('Ctrl Pts',(-53.894727035613,23.8500192775335,40.1355293609261));
#178127=CARTESIAN_POINT('Ctrl Pts',(-53.9078378379963,23.8337171864862,
40.1268999125509));
#178128=CARTESIAN_POINT('Ctrl Pts',(-53.9216475915793,23.8189698115831,
40.1162251288835));
#178129=CARTESIAN_POINT('Ctrl Pts',(-53.9357638458654,23.8060643480692,
40.1038990521418));
#178130=CARTESIAN_POINT('Ctrl Pts',(-53.9428219730085,23.7996116163122,
40.097736013771));
#178131=CARTESIAN_POINT('Ctrl Pts',(-53.9499567269874,23.7936193631245,
40.0911601532641));
#178132=CARTESIAN_POINT('Ctrl Pts',(-53.9571190561825,23.7881234899556,
40.084220729064));
#178133=CARTESIAN_POINT('Ctrl Pts',(-53.9642507845243,23.7826510977527,
40.0773109533619));
#178134=CARTESIAN_POINT('Ctrl Pts',(-53.9714097802519,23.7776706121038,
40.0700409753048));
#178135=CARTESIAN_POINT('Ctrl Pts',(-53.9785478363928,23.7732182003922,
40.0624586415899));
#178136=CARTESIAN_POINT('Ctrl Pts',(-53.9785784643974,23.7731990959632,
40.0624261072769));
#178137=CARTESIAN_POINT('Ctrl Pts',(-53.9786090918656,23.7731800007335,
40.0623935677888));
#178138=CARTESIAN_POINT('Ctrl Pts',(-53.9786397187952,23.7731609147028,
40.0623610231288));
#178139=CARTESIAN_POINT('Ctrl Pts',(-53.9930827901223,23.764160309458,40.0470135870229));
#178140=CARTESIAN_POINT('Ctrl Pts',(-54.0073711636766,23.7571924707013,
40.0305755292085));
#178141=CARTESIAN_POINT('Ctrl Pts',(-54.0213615752669,23.7521258339916,
40.0133447567326));
#178142=CARTESIAN_POINT('Ctrl Pts',(-54.0358609305028,23.7468748830077,
39.995487162658));
#178143=CARTESIAN_POINT('Ctrl Pts',(-54.050041117219,23.7436660552511,39.9767767954295));
#178144=CARTESIAN_POINT('Ctrl Pts',(-54.0637371441671,23.7424048061585,
39.9575197577452));
#178145=CARTESIAN_POINT('Ctrl Pts',(-54.0772376980797,23.7411615579204,
39.9385375611974));
#178146=CARTESIAN_POINT('Ctrl Pts',(-54.0902686241916,23.7418111396964,
39.9190226977072));
#178147=CARTESIAN_POINT('Ctrl Pts',(-54.1026541040343,23.744307900129,39.8992655451833));
#178148=CARTESIAN_POINT('Ctrl Pts',(-54.1112894809389,23.7460486859241,
39.885490506931));
#178149=CARTESIAN_POINT('Ctrl Pts',(-54.1196107481458,23.7486883362846,
39.8715976051467));
#178150=CARTESIAN_POINT('Ctrl Pts',(-54.1275498658872,23.7522229508832,
39.8576902534424));
#178151=CARTESIAN_POINT('',(-54.4530463244691,23.8971395307772,39.2875012672119));
#178152=CARTESIAN_POINT('',(-54.1275498658872,23.7522229508832,39.8576902534424));
#178153=CARTESIAN_POINT('',(-56.456807071981,18.6771643191714,39.2875012672119));
#178154=CARTESIAN_POINT('Origin',(5.53234440788222E-15,0.,39.2875012672119));
#178155=CARTESIAN_POINT('',(-56.1179479440987,18.567058682947,39.8576902534424));
#178156=CARTESIAN_POINT('',(-56.456807071981,18.6771643191714,39.2875012672119));
#178157=CARTESIAN_POINT('',(-56.032358823839,18.2220120550221,40.1599502534424));
#178158=CARTESIAN_POINT('Ctrl Pts',(-56.1179479440987,18.567058682947,39.8576902534424));
#178159=CARTESIAN_POINT('Ctrl Pts',(-56.1063166059142,18.563279281548,39.8772619994045));
#178160=CARTESIAN_POINT('Ctrl Pts',(-56.0953314285486,18.5576887384402,
39.8967644650353));
#178161=CARTESIAN_POINT('Ctrl Pts',(-56.0851270036924,18.5504096793259,
39.9159282836023));
#178162=CARTESIAN_POINT('Ctrl Pts',(-56.0747382496585,18.5429991338221,
39.9354382707157));
#178163=CARTESIAN_POINT('Ctrl Pts',(-56.0651578180785,18.5338382655006,
39.9545987622321));
#178164=CARTESIAN_POINT('Ctrl Pts',(-56.0565365037455,18.5230039556188,
39.9731387498193));
#178165=CARTESIAN_POINT('Ctrl Pts',(-56.0482801935087,18.5126283423269,
39.9908938024014));
#178166=CARTESIAN_POINT('Ctrl Pts',(-56.0409028880807,18.500717380208,40.0080810366137));
#178167=CARTESIAN_POINT('Ctrl Pts',(-56.0345558080376,18.4872979556277,
40.0244542742492));
#178168=CARTESIAN_POINT('Ctrl Pts',(-56.0295075492892,18.4766245866022,
40.0374770090455));
#178169=CARTESIAN_POINT('Ctrl Pts',(-56.0251112400308,18.4649961406232,
40.0499848770024));
#178170=CARTESIAN_POINT('Ctrl Pts',(-56.0214558964132,18.452409918857,40.0618424270193));
#178171=CARTESIAN_POINT('Ctrl Pts',(-56.0214459185125,18.45237556256,40.0618747942791));
#178172=CARTESIAN_POINT('Ctrl Pts',(-56.0214359462906,18.4523411992085,
40.0619071564124));
#178173=CARTESIAN_POINT('Ctrl Pts',(-56.021425979749,18.4523068288038,40.0619395134161));
#178174=CARTESIAN_POINT('Ctrl Pts',(-56.0194419575649,18.4454647717818,
40.0683807661799));
#178175=CARTESIAN_POINT('Ctrl Pts',(-56.0177006304278,18.4383111911743,
40.0746073439084));
#178176=CARTESIAN_POINT('Ctrl Pts',(-56.0162099386096,18.4308858104773,
40.0805869293669));
#178177=CARTESIAN_POINT('Ctrl Pts',(-56.0132515574631,18.4161496282623,
40.092453830807));
#178178=CARTESIAN_POINT('Ctrl Pts',(-56.0112809863292,18.4003417300187,
40.1033475319609));
#178179=CARTESIAN_POINT('Ctrl Pts',(-56.010364368207,18.3837652771159,40.1130129263075));
#178180=CARTESIAN_POINT('Ctrl Pts',(-56.0096769046154,18.3713329374388,
40.1202619720674));
#178181=CARTESIAN_POINT('Ctrl Pts',(-56.0095822888227,18.3584682855077,
40.1268200947267));
#178182=CARTESIAN_POINT('Ctrl Pts',(-56.0101084356843,18.3452992211263,
40.1325796782703));
#178183=CARTESIAN_POINT('Ctrl Pts',(-56.0103057407573,18.3403608219833,
40.1347395220992));
#178184=CARTESIAN_POINT('Ctrl Pts',(-56.0105903407605,18.3353796149002,
40.1367870714852));
#178185=CARTESIAN_POINT('Ctrl Pts',(-56.0109637085384,18.3303623448496,
40.1387166518767));
#178186=CARTESIAN_POINT('Ctrl Pts',(-56.0122704957612,18.3128018996726,
40.1454701832469));
#178187=CARTESIAN_POINT('Ctrl Pts',(-56.0146646833927,18.294799681582,40.1507785912492));
#178188=CARTESIAN_POINT('Ctrl Pts',(-56.0182094638726,18.2766448957075,
40.1543986087265));
#178189=CARTESIAN_POINT('Ctrl Pts',(-56.0199818541125,18.2675675027702,
40.1562086174652));
#178190=CARTESIAN_POINT('Ctrl Pts',(-56.0220418935342,18.2584519681996,
40.1575965292115));
#178191=CARTESIAN_POINT('Ctrl Pts',(-56.0243974853212,18.2493344439489,
40.1585319382567));
#178192=CARTESIAN_POINT('Ctrl Pts',(-56.0255752812147,18.2447756818235,
40.1589996427793));
#178193=CARTESIAN_POINT('Ctrl Pts',(-56.0268269652239,18.2402164222857,
40.159354221642));
#178194=CARTESIAN_POINT('Ctrl Pts',(-56.0281535255244,18.2356611844176,
40.1595918743111));
#178195=CARTESIAN_POINT('Ctrl Pts',(-56.0294800858248,18.2311059465496,
40.1598295269801));
#178196=CARTESIAN_POINT('Ctrl Pts',(-56.0308815240327,18.226554730877,40.1599502506896));
#178197=CARTESIAN_POINT('Ctrl Pts',(-56.032358823839,18.2220120550221,40.1599502534424));
#178198=CARTESIAN_POINT('',(-56.0417604764382,18.1930767435953,40.1599502534424));
#178199=CARTESIAN_POINT('Origin',(3.37692616670652E-16,2.10546223053637E-17,
40.1599502534424));
#178200=CARTESIAN_POINT('',(-56.3138168485094,17.9642361803977,39.8576902534424));
#178201=CARTESIAN_POINT('Ctrl Pts',(-56.0417604764382,18.1930767435953,
40.1599502534424));
#178202=CARTESIAN_POINT('Ctrl Pts',(-56.0429368412707,18.1894530991654,
40.1599502448875));
#178203=CARTESIAN_POINT('Ctrl Pts',(-56.0441547055335,18.1858538720528,
40.1598743450437));
#178204=CARTESIAN_POINT('Ctrl Pts',(-56.0454124342018,18.1822805617813,
40.1597243308499));
#178205=CARTESIAN_POINT('Ctrl Pts',(-56.0528379691453,18.1611840081651,
40.1588386583939));
#178206=CARTESIAN_POINT('Ctrl Pts',(-56.0616522804221,18.1409877741476,
40.1553722553624));
#178207=CARTESIAN_POINT('Ctrl Pts',(-56.0715172876601,18.1220070012986,
40.1496902177804));
#178208=CARTESIAN_POINT('Ctrl Pts',(-56.0752025259741,18.1149164164015,
40.1475675976856));
#178209=CARTESIAN_POINT('Ctrl Pts',(-56.0790342841904,18.1079950493304,
40.1451361443103));
#178210=CARTESIAN_POINT('Ctrl Pts',(-56.082994716577,18.1012578800034,40.1424159447501));
#178211=CARTESIAN_POINT('Ctrl Pts',(-56.0860848445995,18.0960012025253,
40.1402935085949));
#178212=CARTESIAN_POINT('Ctrl Pts',(-56.0892533893664,18.0908571636322,
40.1379949176048));
#178213=CARTESIAN_POINT('Ctrl Pts',(-56.0924919457981,18.0858333812002,
40.1355293609261));
#178214=CARTESIAN_POINT('Ctrl Pts',(-56.1038268933089,18.068250142688,40.1268999125509));
#178215=CARTESIAN_POINT('Ctrl Pts',(-56.1160194751809,18.0521400431276,
40.1162251288835));
#178216=CARTESIAN_POINT('Ctrl Pts',(-56.1287094108802,18.0378297267255,
40.1038990521418));
#178217=CARTESIAN_POINT('Ctrl Pts',(-56.1350543787298,18.0306745685244,
40.097736013771));
#178218=CARTESIAN_POINT('Ctrl Pts',(-56.1415236867627,18.0239693566574,
40.0911601532641));
#178219=CARTESIAN_POINT('Ctrl Pts',(-56.1480723047924,18.0177549231926,
40.084220729064));
#178220=CARTESIAN_POINT('Ctrl Pts',(-56.1545929440328,18.0115670407228,
40.0773109533618));
#178221=CARTESIAN_POINT('Ctrl Pts',(-56.1611921195216,18.0058655198734,
40.0700409753047));
#178222=CARTESIAN_POINT('Ctrl Pts',(-56.1678256688899,18.0006913688999,
40.0624586415899));
#178223=CARTESIAN_POINT('Ctrl Pts',(-56.1678541321546,18.0006691676287,
40.0624261072769));
#178224=CARTESIAN_POINT('Ctrl Pts',(-56.1678825958473,18.0006469755625,
40.0623935677888));
#178225=CARTESIAN_POINT('Ctrl Pts',(-56.1679110599659,18.0006247927011,
40.0623610231288));
#178226=CARTESIAN_POINT('Ctrl Pts',(-56.1813341912027,17.9901637816626,
40.0470135870225));
#178227=CARTESIAN_POINT('Ctrl Pts',(-56.1948159540745,17.9817405717252,
40.0305755292076));
#178228=CARTESIAN_POINT('Ctrl Pts',(-56.2082001169775,17.9752392943574,
40.0133447567312));
#178229=CARTESIAN_POINT('Ctrl Pts',(-56.2220711693916,17.9685015133111,
39.9954871626562));
#178230=CARTESIAN_POINT('Ctrl Pts',(-56.2358382617272,17.9638280307224,
39.9767767954273));
#178231=CARTESIAN_POINT('Ctrl Pts',(-56.2493274239774,17.9611420662345,
39.9575197577427));
#178232=CARTESIAN_POINT('Ctrl Pts',(-56.2626240656151,17.9584944364867,
39.938537561195));
#178233=CARTESIAN_POINT('Ctrl Pts',(-56.275651506735,17.9577783571046,39.9190226977049));
#178234=CARTESIAN_POINT('Ctrl Pts',(-56.2882301201542,17.9589668048477,
39.8992655451812));
#178235=CARTESIAN_POINT('Ctrl Pts',(-56.2970001532242,17.9597954117587,
39.8854905069296));
#178236=CARTESIAN_POINT('Ctrl Pts',(-56.3055517542539,17.9615507925648,
39.871597605146));
#178237=CARTESIAN_POINT('Ctrl Pts',(-56.3138168485093,17.9642361803977,
39.8576902534424));
#178238=CARTESIAN_POINT('',(-56.6526781108322,18.0743352474896,39.2875012672119));
#178239=CARTESIAN_POINT('',(-56.3138168485094,17.9642361803977,39.8576902534424));
#178240=CARTESIAN_POINT('',(-58.0998260601479,12.6735055745745,39.2875012672119));
#178241=CARTESIAN_POINT('Origin',(5.53234440788222E-15,0.,39.2875012672119));
#178242=CARTESIAN_POINT('',(-57.7513140650719,12.5994235324476,39.8576902534424));
#178243=CARTESIAN_POINT('',(-58.0998260601479,12.6735055745745,39.2875012672119));
#178244=CARTESIAN_POINT('',(-57.6301266171956,12.2652136052665,40.1599502534424));
#178245=CARTESIAN_POINT('Ctrl Pts',(-57.7513140650719,12.5994235324476,
39.8576902534424));
#178246=CARTESIAN_POINT('Ctrl Pts',(-57.7393513895531,12.5968806409109,
39.8772619994072));
#178247=CARTESIAN_POINT('Ctrl Pts',(-57.727842019257,12.5924689870912,39.8967644650405));
#178248=CARTESIAN_POINT('Ctrl Pts',(-57.7169326264434,12.5862964562719,
39.91592828361));
#178249=CARTESIAN_POINT('Ctrl Pts',(-57.7058261701561,12.5800124270049,
39.9354382707261));
#178250=CARTESIAN_POINT('Ctrl Pts',(-57.6953406496936,12.5719031706671,
39.9545987622451));
#178251=CARTESIAN_POINT('Ctrl Pts',(-57.6856340700592,12.5620293850045,
39.9731387498347));
#178252=CARTESIAN_POINT('Ctrl Pts',(-57.6763384418397,12.5525736298267,
39.9908938024193));
#178253=CARTESIAN_POINT('Ctrl Pts',(-57.6677565154956,12.5414990556008,
40.008081036634));
#178254=CARTESIAN_POINT('Ctrl Pts',(-57.6600414935913,12.5288165945521,
40.0244542742715));
#178255=CARTESIAN_POINT('Ctrl Pts',(-57.6539052188746,12.5187293820925,
40.0374770090597));
#178256=CARTESIAN_POINT('Ctrl Pts',(-57.6483174894735,12.5076241774138,
40.0499848770091));
#178257=CARTESIAN_POINT('Ctrl Pts',(-57.6433665517939,12.4954889917452,
40.0618424270193));
#178258=CARTESIAN_POINT('Ctrl Pts',(-57.6433530373423,12.4954558666302,
40.0618747942791));
#178259=CARTESIAN_POINT('Ctrl Pts',(-57.6433395278009,12.4954227339059,
40.0619071564124));
#178260=CARTESIAN_POINT('Ctrl Pts',(-57.6433260231715,12.4953895935731,
40.0619395134162));
#178261=CARTESIAN_POINT('Ctrl Pts',(-57.6406376799624,12.4887924048454,
40.0683807661799));
#178262=CARTESIAN_POINT('Ctrl Pts',(-57.6381581392099,12.4818600305507,
40.0746073439084));
#178263=CARTESIAN_POINT('Ctrl Pts',(-57.635899449924,12.474631146591,40.0805869293669));
#178264=CARTESIAN_POINT('Ctrl Pts',(-57.6314169246175,12.460284925759,40.092453830807));
#178265=CARTESIAN_POINT('Ctrl Pts',(-57.6278047731676,12.4447696056084,
40.1033475319609));
#178266=CARTESIAN_POINT('Ctrl Pts',(-57.6251604652271,12.4283797729328,
40.1130129263075));
#178267=CARTESIAN_POINT('Ctrl Pts',(-57.6231772342716,12.416087398426,40.1202619720674));
#178268=CARTESIAN_POINT('Ctrl Pts',(-57.6217384144973,12.4033031104476,
40.1268200947266));
#178269=CARTESIAN_POINT('Ctrl Pts',(-57.6208851370088,12.390151190256,40.1325796782703));
#178270=CARTESIAN_POINT('Ctrl Pts',(-57.6205651579507,12.3852192201841,
40.1347395220992));
#178271=CARTESIAN_POINT('Ctrl Pts',(-57.6203275209636,12.3802355518736,
40.1367870714852));
#178272=CARTESIAN_POINT('Ctrl Pts',(-57.6201743958656,12.3752067393933,
40.1387166518767));
#178273=CARTESIAN_POINT('Ctrl Pts',(-57.6196384580226,12.3576058957121,
40.1454701832469));
#178274=CARTESIAN_POINT('Ctrl Pts',(-57.6201377858513,12.3394520349018,
40.1507785912492));
#178275=CARTESIAN_POINT('Ctrl Pts',(-57.6217654557844,12.3210261723878,
40.1543986087265));
#178276=CARTESIAN_POINT('Ctrl Pts',(-57.6225792907509,12.3118132411307,
40.1562086174652));
#178277=CARTESIAN_POINT('Ctrl Pts',(-57.6236752122406,12.3025323096572,
40.1575965292115));
#178278=CARTESIAN_POINT('Ctrl Pts',(-57.6250648590506,12.2932185057687,
40.1585319382567));
#178279=CARTESIAN_POINT('Ctrl Pts',(-57.6257596824556,12.2885616038245,
40.1589996427793));
#178280=CARTESIAN_POINT('Ctrl Pts',(-57.6265279372157,12.2838964837814,
40.159354221642));
#178281=CARTESIAN_POINT('Ctrl Pts',(-57.6273710784659,12.2792275366734,
40.159591874311));
#178282=CARTESIAN_POINT('Ctrl Pts',(-57.6282142197161,12.2745585895654,
40.1598295269801));
#178283=CARTESIAN_POINT('Ctrl Pts',(-57.6291322491185,12.2698858157463,
40.1599502506896));
#178284=CARTESIAN_POINT('Ctrl Pts',(-57.6301266171956,12.2652136052665,
40.1599502534424));
#178285=CARTESIAN_POINT('',(-57.6364522029206,12.2354540642049,40.1599502534424));
#178286=CARTESIAN_POINT('Origin',(3.35846787602732E-16,1.4165894441799E-17,
40.1599502534424));
#178287=CARTESIAN_POINT('',(-57.8830978693155,11.9794294790617,39.8576902534424));
#178288=CARTESIAN_POINT('Ctrl Pts',(-57.6364522029206,12.2354540642049,
40.1599502534424));
#178289=CARTESIAN_POINT('Ctrl Pts',(-57.6372433495198,12.2317273068701,
40.1599502448875));
#178290=CARTESIAN_POINT('Ctrl Pts',(-57.6380783205157,12.2280204952203,
40.1598743450438));
#178291=CARTESIAN_POINT('Ctrl Pts',(-57.6389556465833,12.2243352914715,
40.1597243308499));
#178292=CARTESIAN_POINT('Ctrl Pts',(-57.6441353133406,12.2025781272228,
40.1588386583938));
#178293=CARTESIAN_POINT('Ctrl Pts',(-57.6507902575938,12.1815711838723,
40.1553722553612));
#178294=CARTESIAN_POINT('Ctrl Pts',(-57.6586171922743,12.161663215633,40.1496902177773));
#178295=CARTESIAN_POINT('Ctrl Pts',(-57.661541074523,12.1542262614079,40.1475675976833));
#178296=CARTESIAN_POINT('Ctrl Pts',(-57.6646283621018,12.1469422825155,
40.145136144309));
#178297=CARTESIAN_POINT('Ctrl Pts',(-57.6678628728672,12.1398280421991,
40.1424159447501));
#178298=CARTESIAN_POINT('Ctrl Pts',(-57.6703866004264,12.1342771550168,
40.1402935085949));
#178299=CARTESIAN_POINT('Ctrl Pts',(-57.6730000890932,12.1288300925917,
40.1379949176048));
#178300=CARTESIAN_POINT('Ctrl Pts',(-57.6756957761164,12.1234953096385,
40.1355293609261));
#178301=CARTESIAN_POINT('Ctrl Pts',(-57.6851306806978,12.1048235693021,
40.1268999125508));
#178302=CARTESIAN_POINT('Ctrl Pts',(-57.6955725063805,12.0875272507063,
40.1162251288835));
#178303=CARTESIAN_POINT('Ctrl Pts',(-57.7066970899018,12.0719688682372,
40.1038990521418));
#178304=CARTESIAN_POINT('Ctrl Pts',(-57.7122593816625,12.0641896770026,
40.097736013771));
#178305=CARTESIAN_POINT('Ctrl Pts',(-57.7179923646568,12.0568449701607,
40.0911601532641));
#178306=CARTESIAN_POINT('Ctrl Pts',(-57.7238555234915,12.0499800630335,
40.084220729064));
#178307=CARTESIAN_POINT('Ctrl Pts',(-57.7296936321424,12.043144486032,40.0773109533618));
#178308=CARTESIAN_POINT('Ctrl Pts',(-57.7356606854447,12.0367843970377,
40.0700409753048));
#178309=CARTESIAN_POINT('Ctrl Pts',(-57.7417170494856,12.0309451958831,
40.0624586415899));
#178310=CARTESIAN_POINT('Ctrl Pts',(-57.7417430361607,12.0309201410115,
40.0624261072769));
#178311=CARTESIAN_POINT('Ctrl Pts',(-57.7417690242238,12.0308950952497,
40.0623935677889));
#178312=CARTESIAN_POINT('Ctrl Pts',(-57.7417950136726,12.0308700585978,
40.0623610231289));
#178313=CARTESIAN_POINT('Ctrl Pts',(-57.7540511381833,12.0190632547925,
40.0470135870233));
#178314=CARTESIAN_POINT('Ctrl Pts',(-57.7665785813563,12.0092769601257,
40.0305755292092));
#178315=CARTESIAN_POINT('Ctrl Pts',(-57.7792098558813,12.0014122714555,
40.0133447567337));
#178316=CARTESIAN_POINT('Ctrl Pts',(-57.7923006313198,11.9932614808862,
39.9954871626594));
#178317=CARTESIAN_POINT('Ctrl Pts',(-57.8055037941296,11.9871745471185,
39.9767767954313));
#178318=CARTESIAN_POINT('Ctrl Pts',(-57.8186383015968,11.9830932952243,
39.9575197577474));
#178319=CARTESIAN_POINT('Ctrl Pts',(-57.8315853501714,11.9790702919521,
39.9385375612));
#178320=CARTESIAN_POINT('Ctrl Pts',(-57.8444665749283,11.9769963969268,
39.9190226977102));
#178321=CARTESIAN_POINT('Ctrl Pts',(-57.8571005080032,11.9768635110977,
39.8992655451868));
#178322=CARTESIAN_POINT('Ctrl Pts',(-57.8659091109227,11.9767708607333,
39.8854905069334));
#178323=CARTESIAN_POINT('Ctrl Pts',(-57.8745973526466,11.9776227396654,
39.8715976051479));
#178324=CARTESIAN_POINT('Ctrl Pts',(-57.8830978693155,11.9794294790617,
39.8576902534424));
#178325=CARTESIAN_POINT('',(-58.231611300478,12.0535047649326,39.2875012672119));
#178326=CARTESIAN_POINT('',(-57.8830978693155,11.9794294790616,39.8576902534424));
#178327=CARTESIAN_POINT('',(-59.1062911958296,6.53099325080096,39.2875012672119));
#178328=CARTESIAN_POINT('Origin',(5.53234440788222E-15,0.,39.2875012672119));
#178329=CARTESIAN_POINT('',(-58.7519447039088,6.49374646112781,39.8576902534424));
#178330=CARTESIAN_POINT('',(-59.1062911958296,6.53099325080096,39.2875012672119));
#178331=CARTESIAN_POINT('',(-58.596486683455,6.17403490859061,40.1599502534424));
#178332=CARTESIAN_POINT('Ctrl Pts',(-58.7519447039088,6.49374646112781,
39.8576902534424));
#178333=CARTESIAN_POINT('Ctrl Pts',(-58.7397817566348,6.4924679399056,39.8772619994052));
#178334=CARTESIAN_POINT('Ctrl Pts',(-58.7278742924804,6.48928351037781,
39.8967644650367));
#178335=CARTESIAN_POINT('Ctrl Pts',(-58.716379457302,6.48428513539496,39.9159282836043));
#178336=CARTESIAN_POINT('Ctrl Pts',(-58.7046769834231,6.47919647150667,
39.9354382707185));
#178337=CARTESIAN_POINT('Ctrl Pts',(-58.6934012556367,6.47222767386539,
39.9545987622356));
#178338=CARTESIAN_POINT('Ctrl Pts',(-58.6827157580201,6.4634225916883,39.9731387498234));
#178339=CARTESIAN_POINT('Ctrl Pts',(-58.6724826566677,6.45499029386124,
39.9908938024063));
#178340=CARTESIAN_POINT('Ctrl Pts',(-58.6627901347897,6.44487344288651,
40.0080810366194));
#178341=CARTESIAN_POINT('Ctrl Pts',(-58.6537916984193,6.43306689707259,
40.0244542742555));
#178342=CARTESIAN_POINT('Ctrl Pts',(-58.6466346380372,6.42367635878173,
40.0374770090495));
#178343=CARTESIAN_POINT('Ctrl Pts',(-58.6399167088201,6.41321606633983,
40.0499848770043));
#178344=CARTESIAN_POINT('Ctrl Pts',(-58.6337244205832,6.40166487239078,
40.0618424270193));
#178345=CARTESIAN_POINT('Ctrl Pts',(-58.6337075176478,6.4016333413835,40.0618747942791));
#178346=CARTESIAN_POINT('Ctrl Pts',(-58.6336906188003,6.40160180229526,
40.0619071564124));
#178347=CARTESIAN_POINT('Ctrl Pts',(-58.6336737240427,6.40157025512682,
40.0619395134162));
#178348=CARTESIAN_POINT('Ctrl Pts',(-58.6303105138593,6.39529021487361,
40.0683807661799));
#178349=CARTESIAN_POINT('Ctrl Pts',(-58.6271199258587,6.38865499943512,
40.0746073439084));
#178350=CARTESIAN_POINT('Ctrl Pts',(-58.6241179857776,6.38170181337825,
40.0805869293669));
#178351=CARTESIAN_POINT('Ctrl Pts',(-58.6181604277965,6.3679027341269,40.092453830807));
#178352=CARTESIAN_POINT('Ctrl Pts',(-58.6129462715177,6.35284998116362,
40.1033475319609));
#178353=CARTESIAN_POINT('Ctrl Pts',(-58.6086032453499,6.33682633915166,
40.1130129263075));
#178354=CARTESIAN_POINT('Ctrl Pts',(-58.6053459757241,6.3248086076427,40.1202619720674));
#178355=CARTESIAN_POINT('Ctrl Pts',(-58.6025787159787,6.31224475095145,
40.1268200947266));
#178356=CARTESIAN_POINT('Ctrl Pts',(-58.600355362827,6.29925407013931,40.1325796782703));
#178357=CARTESIAN_POINT('Ctrl Pts',(-58.599521605395,6.29438256483475,40.1347395220992));
#178358=CARTESIAN_POINT('Ctrl Pts',(-58.5987643350183,6.28945103740978,
40.1367870714852));
#178359=CARTESIAN_POINT('Ctrl Pts',(-58.598086394715,6.28446577922157,40.1387166518767));
#178360=CARTESIAN_POINT('Ctrl Pts',(-58.5957136036534,6.26701737556284,
40.1454701832469));
#178361=CARTESIAN_POINT('Ctrl Pts',(-58.5943126009392,6.24891076953097,
40.1507785912492));
#178362=CARTESIAN_POINT('Ctrl Pts',(-58.594005327233,6.23041570798286,40.1543986087265));
#178363=CARTESIAN_POINT('Ctrl Pts',(-58.59385169038,6.22116817720881,40.1562086174652));
#178364=CARTESIAN_POINT('Ctrl Pts',(-58.5939714867924,6.21182353265984,
40.1575965292115));
#178365=CARTESIAN_POINT('Ctrl Pts',(-58.5943799633642,6.20241549311804,
40.1585319382567));
#178366=CARTESIAN_POINT('Ctrl Pts',(-58.5945842016501,6.19771147334713,
40.1589996427793));
#178367=CARTESIAN_POINT('Ctrl Pts',(-58.5948606100011,6.19299160483032,
40.159354221642));
#178368=CARTESIAN_POINT('Ctrl Pts',(-58.595211094569,6.18826010244389,40.159591874311));
#178369=CARTESIAN_POINT('Ctrl Pts',(-58.5955615791369,6.18352860005746,
40.1598295269801));
#178370=CARTESIAN_POINT('Ctrl Pts',(-58.5959861416118,6.17878546397953,
40.1599502506895));
#178371=CARTESIAN_POINT('Ctrl Pts',(-58.596486683455,6.17403490859061,40.1599502534424));
#178372=CARTESIAN_POINT('',(-58.5996668978648,6.14377718965363,40.1599502534424));
#178373=CARTESIAN_POINT('Origin',(3.34731138317027E-16,7.12196207432608E-18,
40.1599502534424));
#178374=CARTESIAN_POINT('',(-58.8181995570484,5.86337364149622,39.8576902534424));
#178375=CARTESIAN_POINT('Ctrl Pts',(-58.5996668978648,6.14377718965363,
40.1599502534424));
#178376=CARTESIAN_POINT('Ctrl Pts',(-58.600064158263,6.13998815054726,40.1599502448875));
#178377=CARTESIAN_POINT('Ctrl Pts',(-58.600507087875,6.13621436696444,40.1598743450437));
#178378=CARTESIAN_POINT('Ctrl Pts',(-58.6009943991739,6.13245764560167,
40.1597243308499));
#178379=CARTESIAN_POINT('Ctrl Pts',(-58.6038714482307,6.11027824676932,
40.1588386583938));
#178380=CARTESIAN_POINT('Ctrl Pts',(-58.6082941124965,6.08869075055693,
40.1553722553613));
#178381=CARTESIAN_POINT('Ctrl Pts',(-58.6139972210829,6.06807370279675,
40.1496902177777));
#178382=CARTESIAN_POINT('Ctrl Pts',(-58.6161277126023,6.0603718600664,40.1475675976835));
#178383=CARTESIAN_POINT('Ctrl Pts',(-58.6184367045766,6.05280507414586,
40.1451361443091));
#178384=CARTESIAN_POINT('Ctrl Pts',(-58.6209098557462,6.04539170794222,
40.1424159447501));
#178385=CARTESIAN_POINT('Ctrl Pts',(-58.6228395323549,6.03960742773723,
40.1402935085949));
#178386=CARTESIAN_POINT('Ctrl Pts',(-58.6248693309926,6.03391702093593,
40.1379949176048));
#178387=CARTESIAN_POINT('Ctrl Pts',(-58.6269926140963,6.02832968645991,
40.1355293609261));
#178388=CARTESIAN_POINT('Ctrl Pts',(-58.6344241049593,6.00877401579383,
40.1268999125509));
#178389=CARTESIAN_POINT('Ctrl Pts',(-58.6430007716254,5.9904809802487,40.1162251288835));
#178390=CARTESIAN_POINT('Ctrl Pts',(-58.6524381197038,5.97384499260664,
40.1038990521418));
#178391=CARTESIAN_POINT('Ctrl Pts',(-58.657156793743,5.96552699878561,40.097736013771));
#178392=CARTESIAN_POINT('Ctrl Pts',(-58.6620906399372,5.95762326711397,
40.0911601532641));
#178393=CARTESIAN_POINT('Ctrl Pts',(-58.6672041015819,5.95018309968334,
40.084220729064));
#178394=CARTESIAN_POINT('Ctrl Pts',(-58.6722957161032,5.94277472016222,
40.0773109533619));
#178395=CARTESIAN_POINT('Ctrl Pts',(-58.6775652709344,5.93582574548894,
40.0700409753048));
#178396=CARTESIAN_POINT('Ctrl Pts',(-58.682978094856,5.9293854696631,40.0624586415899));
#178397=CARTESIAN_POINT('Ctrl Pts',(-58.6830013202262,5.92935783569746,
40.0624261072769));
#178398=CARTESIAN_POINT('Ctrl Pts',(-58.6830245479289,5.9293302106467,40.0623935677888));
#178399=CARTESIAN_POINT('Ctrl Pts',(-58.683047777962,5.92930259451103,40.0623610231288));
#178400=CARTESIAN_POINT('Ctrl Pts',(-58.6940026150817,5.91627935575239,
40.0470135870242));
#178401=CARTESIAN_POINT('Ctrl Pts',(-58.7054384852669,5.90523719704883,
40.0305755292111));
#178402=CARTESIAN_POINT('Ctrl Pts',(-58.7171784805269,5.89609526425114,
40.0133447567368));
#178403=CARTESIAN_POINT('Ctrl Pts',(-58.7293455537145,5.88662076592623,
39.9954871626637));
#178404=CARTESIAN_POINT('Ctrl Pts',(-58.7418401303834,5.87918707069999,
39.9767767954368));
#178405=CARTESIAN_POINT('Ctrl Pts',(-58.754476078655,5.87375524644919,39.9575197577541));
#178406=CARTESIAN_POINT('Ctrl Pts',(-58.7669316835925,5.86840094651825,
39.9385375612077));
#178407=CARTESIAN_POINT('Ctrl Pts',(-58.7795255625917,5.86499195787771,
39.919022697719));
#178408=CARTESIAN_POINT('Ctrl Pts',(-58.7920763953073,5.86353919440106,
39.8992655451965));
#178409=CARTESIAN_POINT('Ctrl Pts',(-58.8008270591802,5.86252630185767,
39.8854905069399));
#178410=CARTESIAN_POINT('Ctrl Pts',(-58.8095567514046,5.86246534555171,
39.8715976051512));
#178411=CARTESIAN_POINT('Ctrl Pts',(-58.8181995570484,5.86337364149624,
39.8576902534424));
#178412=CARTESIAN_POINT('',(-59.1725467709677,5.90061356181298,39.2875012672119));
#178413=CARTESIAN_POINT('',(-58.8181995570484,5.8633736414962,39.8576902534424));
#178414=CARTESIAN_POINT('',(-59.4651754363832,0.316925998273044,39.2875012672119));
#178415=CARTESIAN_POINT('Origin',(5.53234440788222E-15,0.,39.2875012672119));
#178416=CARTESIAN_POINT('',(-59.1088767419348,0.316922544675689,39.8576902534424));
#178417=CARTESIAN_POINT('',(-59.4651754363832,0.316925998273047,39.2875012672119));
#178418=CARTESIAN_POINT('Ctrl Pts',(-59.1088767419348,0.316922544675689,
39.8576902534424));
#178419=CARTESIAN_POINT('Ctrl Pts',(-59.096646782701,0.316922401513864,
39.8772619994035));
#178420=CARTESIAN_POINT('Ctrl Pts',(-59.0844716853573,0.315000085554014,
39.8967644650332));
#178421=CARTESIAN_POINT('Ctrl Pts',(-59.0725173476341,0.311230629649666,
39.9159282835992));
#178422=CARTESIAN_POINT('Ctrl Pts',(-59.0603470709162,0.307393083606243,
39.9354382707117));
#178423=CARTESIAN_POINT('Ctrl Pts',(-59.0484046750391,0.30164109626635,
39.9545987622272));
#178424=CARTESIAN_POINT('Ctrl Pts',(-59.0368573319885,0.294001187897179,
39.9731387498136));
#178425=CARTESIAN_POINT('Ctrl Pts',(-59.0257988735033,0.286684733440014,
39.9908938023951));
#178426=CARTESIAN_POINT('Ctrl Pts',(-59.0151019493895,0.27763644805218,
40.0080810366069));
#178427=CARTESIAN_POINT('Ctrl Pts',(-59.0049186873052,0.266835172459114,
40.0244542742421));
#178428=CARTESIAN_POINT('Ctrl Pts',(-58.9968192555089,0.258244193040634,
40.0374770090409));
#178429=CARTESIAN_POINT('Ctrl Pts',(-58.9890447295139,0.248543417989683,
40.0499848770002));
#178430=CARTESIAN_POINT('Ctrl Pts',(-58.981678934725,0.23770277305949,40.0618424270193));
#178431=CARTESIAN_POINT('Ctrl Pts',(-58.9816588284979,0.23767318162023,
40.0618747942791));
#178432=CARTESIAN_POINT('Ctrl Pts',(-58.9816387254916,0.237643581716968,
40.0619071564124));
#178433=CARTESIAN_POINT('Ctrl Pts',(-58.9816186257082,0.23761397335028,
40.0619395134162));
#178434=CARTESIAN_POINT('Ctrl Pts',(-58.9776173965852,0.231719887006775,
40.0683807661799));
#178435=CARTESIAN_POINT('Ctrl Pts',(-58.9737507180862,0.22545452723336,
40.0746073439084));
#178436=CARTESIAN_POINT('Ctrl Pts',(-58.9700384170936,0.218853219640731,
40.0805869293669));
#178437=CARTESIAN_POINT('Ctrl Pts',(-58.9626710986899,0.205752467569928,
40.092453830807));
#178438=CARTESIAN_POINT('Ctrl Pts',(-58.9559120649696,0.191327202905431,
40.1033475319609));
#178439=CARTESIAN_POINT('Ctrl Pts',(-58.9499179036781,0.175845309932249,
40.1130129263075));
#178440=CARTESIAN_POINT('Ctrl Pts',(-58.9454222827095,0.164233890202363,
40.1202619720674));
#178441=CARTESIAN_POINT('Ctrl Pts',(-58.9413569016699,0.1520281170413,40.1268200947267));
#178442=CARTESIAN_POINT('Ctrl Pts',(-58.9377878323772,0.139341004226139,
40.1325796782703));
#178443=CARTESIAN_POINT('Ctrl Pts',(-58.9364494313924,0.134583336920454,
40.1347395220992));
#178444=CARTESIAN_POINT('Ctrl Pts',(-58.9351808244388,0.129757981227463,
40.1367870714852));
#178445=CARTESIAN_POINT('Ctrl Pts',(-58.933985496586,0.124870896863318,
40.1387166518767));
#178446=CARTESIAN_POINT('Ctrl Pts',(-58.9298018491012,0.107766101588809,
40.1454701832469));
#178447=CARTESIAN_POINT('Ctrl Pts',(-58.9265158655229,0.089905130100062,
40.1507785912492));
#178448=CARTESIAN_POINT('Ctrl Pts',(-58.9242770147326,0.0715435052825858,
40.1543986087265));
#178449=CARTESIAN_POINT('Ctrl Pts',(-58.9231575893375,0.0623626928738478,
40.1562086174652));
#178450=CARTESIAN_POINT('Ctrl Pts',(-58.9222999481582,0.0530567171305718,
40.1575965292115));
#178451=CARTESIAN_POINT('Ctrl Pts',(-58.9217227791368,0.0436575183854266,
40.1585319382567));
#178452=CARTESIAN_POINT('Ctrl Pts',(-58.9214341946262,0.038957919012854,
40.1589996427793));
#178453=CARTESIAN_POINT('Ctrl Pts',(-58.9212157281805,0.034235013889458,
40.159354221642));
#178454=CARTESIAN_POINT('Ctrl Pts',(-58.9210697160839,0.0294927955548825,
40.1595918743111));
#178455=CARTESIAN_POINT('Ctrl Pts',(-58.9209237039872,0.024750577220307,
40.1598295269801));
#178456=CARTESIAN_POINT('Ctrl Pts',(-58.9208501479391,0.0199890456750398,
40.1599502506895));
#178457=CARTESIAN_POINT('Ctrl Pts',(-58.9208513795073,0.0152121934559205,
40.1599502534424));
#178458=CARTESIAN_POINT('Origin',(5.49031038273072E-15,0.,38.989));
#178459=CARTESIAN_POINT('',(56.875,6.96517867015057E-15,38.989));
#178460=CARTESIAN_POINT('',(-56.875,-6.96517867015057E-15,38.989));
#178461=CARTESIAN_POINT('Origin',(5.49031038273072E-15,0.,38.989));
#178462=CARTESIAN_POINT('',(-56.875,-6.96517867015057E-15,38.989));
#178463=CARTESIAN_POINT('Origin',(5.49031038273072E-15,0.,38.989));
#178464=CARTESIAN_POINT('Origin',(0.,0.,0.));
#178465=CARTESIAN_POINT('',(56.875,-6.96517867015057E-15,38.6715));
#178466=CARTESIAN_POINT('',(56.875,-6.96517867015057E-15,-8.00896157936366E-15));
#178467=CARTESIAN_POINT('Origin',(5.44560101479317E-15,0.,38.6715));
#178468=CARTESIAN_POINT('Origin',(60.4792282238308,0.,38.989));
#178469=CARTESIAN_POINT('',(60.1802756340597,6.00595296980781,38.989));
#178470=CARTESIAN_POINT('',(60.1803330762808,6.00537737563911,38.9889999997818));
#178471=CARTESIAN_POINT('Origin',(5.49031038273072E-15,0.,38.989));
#178472=CARTESIAN_POINT('',(59.7081718144893,5.95633285891129,38.989));
#178473=CARTESIAN_POINT('',(59.70870646733,5.95638905318924,38.989));
#178474=CARTESIAN_POINT('',(60.0036905223731,0.3175,38.989));
#178475=CARTESIAN_POINT('Origin',(5.49031038273072E-15,0.,38.989));
#178476=CARTESIAN_POINT('',(60.4783948217626,0.317500000025261,38.989));
#178477=CARTESIAN_POINT('',(60.4792282238308,0.3175,38.989));
#178478=CARTESIAN_POINT('',(60.4783917836883,0.318078445377853,38.9889999995776));
#178479=CARTESIAN_POINT('Origin',(5.49031038273072E-15,0.,38.989));
#178480=CARTESIAN_POINT('Origin',(5.49031038273072E-15,0.,38.989));
#178481=CARTESIAN_POINT('Origin',(5.49031038273072E-15,0.,38.989));
#178482=CARTESIAN_POINT('',(60.6410923272405,0.318076890623366,39.2708017080178));
#178483=CARTESIAN_POINT('',(60.3421421673489,6.02238575973002,39.2708017078546));
#178484=CARTESIAN_POINT('Origin',(5.52999282761009E-15,0.,39.2708017080178));
#178485=CARTESIAN_POINT('',(60.3421421670676,6.02238575970194,39.2708017080178));
#178486=CARTESIAN_POINT('',(60.4783917829566,0.318078445374005,38.989));
#178487=CARTESIAN_POINT('Origin',(60.71525,0.,39.3978017080178));
#178488=CARTESIAN_POINT('',(61.0122769227456,0.3175,39.3978017080178));
#178489=CARTESIAN_POINT('',(60.7112330730305,6.06175884541488,39.3978017080178));
#178490=CARTESIAN_POINT('Origin',(5.5478765747851E-15,0.,39.3978017080178));
#178491=CARTESIAN_POINT('',(60.5608532912344,6.04595329344978,39.3978017080178));
#178492=CARTESIAN_POINT('',(60.561380412237,6.04600869609965,39.3978017080178));
#178493=CARTESIAN_POINT('',(60.8610688070707,0.3175,39.3978017080178));
#178494=CARTESIAN_POINT('Origin',(5.5478765747851E-15,0.,39.3978017080178));
#178495=CARTESIAN_POINT('',(60.71525,0.3175,39.3978017080178));
#178496=CARTESIAN_POINT('Origin',(5.5478765747851E-15,0.,39.3978017080178));
#178497=CARTESIAN_POINT('',(61.0917542093525,6.10232411256005,38.9890000005754));
#178498=CARTESIAN_POINT('',(61.0918106390013,6.1017591594455,38.989));
#178499=CARTESIAN_POINT('Origin',(5.49031038273072E-15,0.,38.989));
#178500=CARTESIAN_POINT('',(60.9299448846691,6.08531878138237,39.2708017080178));
#178501=CARTESIAN_POINT('',(61.0917542096815,6.10232411260841,38.989));
#178502=CARTESIAN_POINT('',(61.2322532923707,0.316930737397327,39.2708017081757));
#178503=CARTESIAN_POINT('Origin',(5.52999282761008E-15,0.,39.2708017080178));
#178504=CARTESIAN_POINT('',(61.3949537495049,0.31693224325326,38.9890000005756));
#178505=CARTESIAN_POINT('',(61.2322532920972,0.316930737395914,39.2708017080178));
#178506=CARTESIAN_POINT('',(61.3949508163454,0.3175,38.989));
#178507=CARTESIAN_POINT('Origin',(5.49031038273072E-15,0.,38.989));
#178508=CARTESIAN_POINT('Origin',(5.49031038273072E-15,0.,38.989));
#178509=CARTESIAN_POINT('Origin',(62.2224557307631,0.,38.989));
#178510=CARTESIAN_POINT('',(61.8696548221181,0.3175,38.989));
#178511=CARTESIAN_POINT('',(61.5639141665613,6.15137923967592,38.989));
#178512=CARTESIAN_POINT('Origin',(5.49031038273072E-15,0.,38.989));
#178513=CARTESIAN_POINT('',(61.0923331762718,6.10181408032572,38.989));
#178514=CARTESIAN_POINT('',(62.2224557307631,0.3175,38.989));
#178515=CARTESIAN_POINT('Origin',(5.57972911860581E-15,0.,39.624));
#178516=CARTESIAN_POINT('Origin',(59.7081714060831,5.95632779542214,39.6240070731883));
#178517=CARTESIAN_POINT('Origin',(60.0036895869254,0.317504993060516,39.6240070731883));
#178518=CARTESIAN_POINT('Origin',(5.57972911860581E-15,0.,39.624));
#178519=CARTESIAN_POINT('Origin',(61.6018378049617,6.15533145331002,39.555211759881));
#178520=CARTESIAN_POINT('Origin',(61.9077842377873,0.31753353701155,39.5552135207987));
#178521=CARTESIAN_POINT('Origin',(5.51210908043506E-15,0.,39.1438017080178));
#178522=CARTESIAN_POINT('Origin',(60.7269085901936,6.06344346747426,39.1712173702614));
#178523=CARTESIAN_POINT('Origin',(61.0281367271395,0.31746290747849,39.1711625381338));
#178524=CARTESIAN_POINT('Origin',(5.51210908043507E-15,0.,39.1438017080178));
#178525=CARTESIAN_POINT('Origin',(60.5450849487961,6.04425010054726,39.1711627526728));
#178526=CARTESIAN_POINT('Origin',(60.845302880269,0.317545368445466,39.171217585939));
#178527=CARTESIAN_POINT('Origin',(60.4792282238308,0.,38.989));
#178528=CARTESIAN_POINT('',(58.7584778814678,12.1649068885784,38.989));
#178529=CARTESIAN_POINT('',(59.6417962403144,6.58785426247015,38.989));
#178530=CARTESIAN_POINT('Origin',(5.49031038273072E-15,0.,38.989));
#178531=CARTESIAN_POINT('',(60.1139000598801,6.637474373417,38.989));
#178532=CARTESIAN_POINT('',(59.7852323155142,6.60293000146354,38.989));
#178533=CARTESIAN_POINT('',(60.1138365744453,6.63804933242023,38.9889999995773));
#178534=CARTESIAN_POINT('Origin',(5.49031038273072E-15,0.,38.989));
#178535=CARTESIAN_POINT('',(59.2229260464988,12.2630370254216,38.9889999997818));
#178536=CARTESIAN_POINT('Origin',(5.49031038273072E-15,0.,38.989));
#178537=CARTESIAN_POINT('',(59.2228087529784,12.2636034620781,38.989));
#178538=CARTESIAN_POINT('Origin',(5.49031038273072E-15,0.,38.989));
#178539=CARTESIAN_POINT('',(58.7590037315227,12.165018661458,38.989));
#178540=CARTESIAN_POINT('Origin',(5.49031038273072E-15,0.,38.989));
#178541=CARTESIAN_POINT('',(60.275645989912,6.65505462397314,39.2708017080178));
#178542=CARTESIAN_POINT('',(60.1138365737176,6.63804933233988,38.989));
#178543=CARTESIAN_POINT('',(59.3820708701841,12.2968658914369,39.2708017078546));
#178544=CARTESIAN_POINT('Origin',(5.52999282761009E-15,0.,39.2708017080178));
#178545=CARTESIAN_POINT('',(59.3820708699072,12.2968658913796,39.2708017080178));
#178546=CARTESIAN_POINT('Origin',(60.71525,0.,39.3978017080178));
#178547=CARTESIAN_POINT('',(59.5971203935661,12.3431658574203,39.3978017080178));
#178548=CARTESIAN_POINT('',(60.4944777170595,6.67747469700864,39.3978017080178));
#178549=CARTESIAN_POINT('Origin',(5.5478765747851E-15,0.,39.3978017080178));
#178550=CARTESIAN_POINT('',(60.6448574988555,6.69328024897373,39.3978017080178));
#178551=CARTESIAN_POINT('',(60.0186752706393,6.62746584474012,39.3978017080178));
#178552=CARTESIAN_POINT('',(59.7450242491249,12.3746037924156,39.3978017080178));
#178553=CARTESIAN_POINT('Origin',(5.5478765747851E-15,0.,39.3978017080178));
#178554=CARTESIAN_POINT('',(59.5976388357908,12.343276055717,39.3978017080178));
#178555=CARTESIAN_POINT('Origin',(5.5478765747851E-15,0.,39.3978017080178));
#178556=CARTESIAN_POINT('',(59.9600752506739,12.4208962741579,39.2708017080178));
#178557=CARTESIAN_POINT('',(60.8636883190564,6.71570789672327,39.2708017081757));
#178558=CARTESIAN_POINT('Origin',(5.52999282761008E-15,0.,39.2708017080178));
#178559=CARTESIAN_POINT('',(61.025497328658,6.73271622308714,38.9890000005756));
#178560=CARTESIAN_POINT('',(60.8636883187846,6.71570789669327,39.2708017080178));
#178561=CARTESIAN_POINT('',(61.0254350648263,6.73328056300436,38.989));
#178562=CARTESIAN_POINT('Origin',(5.49031038273072E-15,0.,38.989));
#178563=CARTESIAN_POINT('',(60.119335800013,12.4541661686658,38.989));
#178564=CARTESIAN_POINT('Origin',(5.49031038273072E-15,0.,38.989));
#178565=CARTESIAN_POINT('',(60.1192206258109,12.4547221284036,38.9890000005754));
#178566=CARTESIAN_POINT('Origin',(5.49031038273072E-15,0.,38.989));
#178567=CARTESIAN_POINT('',(60.1192206261331,12.4547221284861,38.989));
#178568=CARTESIAN_POINT('Origin',(62.2224557307631,0.,38.989));
#178569=CARTESIAN_POINT('',(61.4975385923863,6.78290064323477,38.989));
#178570=CARTESIAN_POINT('',(61.5094129706999,6.78414869068668,38.989));
#178571=CARTESIAN_POINT('',(60.5836663843183,12.5528626811439,38.989));
#178572=CARTESIAN_POINT('Origin',(5.49031038273072E-15,0.,38.989));
#178573=CARTESIAN_POINT('',(60.1198497339745,12.4542754087016,38.989));
#178574=CARTESIAN_POINT('Origin',(5.57972911860581E-15,0.,39.624));
#178575=CARTESIAN_POINT('Origin',(59.6417947880742,6.58785913039734,39.6240070731883));
#178576=CARTESIAN_POINT('Origin',(58.7584780045776,12.1649018101376,39.6240070731883));
#178577=CARTESIAN_POINT('Origin',(5.57972911860581E-15,0.,39.624));
#178578=CARTESIAN_POINT('Origin',(61.535455625554,6.78691960575244,39.5552135207993));
#178579=CARTESIAN_POINT('Origin',(60.6209691542404,12.5607573437818,39.5552117598835));
#178580=CARTESIAN_POINT('Origin',(5.51210908043506E-15,0.,39.1438017080178));
#178581=CARTESIAN_POINT('Origin',(60.6606342988042,6.69490116062979,39.1711625381311));
#178582=CARTESIAN_POINT('Origin',(59.7604378032078,12.3779177236587,39.1712173702578));
#178583=CARTESIAN_POINT('Origin',(5.51210908043507E-15,0.,39.1438017080178));
#178584=CARTESIAN_POINT('Origin',(60.4787934153619,6.67587182882045,39.1712175859371));
#178585=CARTESIAN_POINT('Origin',(59.5816164638931,12.3398237541811,39.1711627526761));
#178586=CARTESIAN_POINT('Origin',(60.4792282238308,0.,38.989));
#178587=CARTESIAN_POINT('',(57.1650137687749,18.2401996527038,38.989));
#178588=CARTESIAN_POINT('',(58.6264539577985,12.7860306150444,38.989));
#178589=CARTESIAN_POINT('Origin',(5.49031038273072E-15,0.,38.989));
#178590=CARTESIAN_POINT('',(59.0907848292992,12.8847271885936,38.989));
#178591=CARTESIAN_POINT('',(57.7988642628865,12.6101209950203,38.989));
#178592=CARTESIAN_POINT('',(59.0906615920642,12.8852923618765,38.9889999995768));
#178593=CARTESIAN_POINT('Origin',(5.49031038273072E-15,0.,38.989));
#178594=CARTESIAN_POINT('',(57.6166602457575,18.386340275348,38.9889999997818));
#178595=CARTESIAN_POINT('Origin',(5.49031038273072E-15,0.,38.989));
#178596=CARTESIAN_POINT('',(57.6164843860299,18.3868913484938,38.989));
#178597=CARTESIAN_POINT('Origin',(5.49031038273072E-15,0.,38.989));
#178598=CARTESIAN_POINT('',(57.1655250547209,18.240365779578,38.989));
#178599=CARTESIAN_POINT('Origin',(5.49031038273072E-15,0.,38.989));
#178600=CARTESIAN_POINT('',(59.2498070616281,12.9191181862038,39.2708017080178));
#178601=CARTESIAN_POINT('',(59.0906615913479,12.8852923617204,38.989));
#178602=CARTESIAN_POINT('',(57.7713971780683,18.4366189871525,39.2708017078546));
#178603=CARTESIAN_POINT('Origin',(5.52999282761009E-15,0.,39.2708017080178));
#178604=CARTESIAN_POINT('',(57.771397177799,18.4366189870665,39.2708017080178));
#178605=CARTESIAN_POINT('Origin',(60.71525,0.,39.3978017080178));
#178606=CARTESIAN_POINT('',(57.9804289733666,18.5051441132834,39.3978017080178));
#178607=CARTESIAN_POINT('',(59.4650964698968,12.9642895838863,39.3978017080178));
#178608=CARTESIAN_POINT('Origin',(5.5478765747851E-15,0.,39.3978017080178));
#178609=CARTESIAN_POINT('',(59.6130003254557,12.9957275188816,39.3978017080178));
#178610=CARTESIAN_POINT('',(58.0246834617332,12.6581203474863,39.3978017080178));
#178611=CARTESIAN_POINT('',(58.1242364370959,18.5518699907143,39.3978017080178));
#178612=CARTESIAN_POINT('Origin',(5.5478765747851E-15,0.,39.3978017080178));
#178613=CARTESIAN_POINT('',(57.9809330566519,18.5053078998713,39.3978017080178));
#178614=CARTESIAN_POINT('Origin',(5.5478765747851E-15,0.,39.3978017080178));
#178615=CARTESIAN_POINT('',(58.3332704847798,18.620387828114,39.2708017080178));
#178616=CARTESIAN_POINT('',(59.8282880399729,13.0409063549813,39.2708017081757));
#178617=CARTESIAN_POINT('Origin',(5.52999282761008E-15,0.,39.2708017080178));
#178618=CARTESIAN_POINT('',(59.9874327886719,13.0747351550703,38.9890000005756));
#178619=CARTESIAN_POINT('',(59.8282880397057,13.0409063549231,39.2708017080178));
#178620=CARTESIAN_POINT('',(59.9873118763437,13.0752898951317,38.989));
#178621=CARTESIAN_POINT('Origin',(5.49031038273072E-15,0.,38.989));
#178622=CARTESIAN_POINT('',(58.48818093722,18.6701227271403,38.989));
#178623=CARTESIAN_POINT('Origin',(5.49031038273072E-15,0.,38.989));
#178624=CARTESIAN_POINT('',(58.4880082803372,18.6706636022901,38.9890000005754));
#178625=CARTESIAN_POINT('Origin',(5.49031038273072E-15,0.,38.989));
#178626=CARTESIAN_POINT('',(58.488008280649,18.6706636024058,38.989));
#178627=CARTESIAN_POINT('Origin',(62.2224557307631,0.,38.989));
#178628=CARTESIAN_POINT('',(60.4516424606491,13.1739864076099,38.989));
#178629=CARTESIAN_POINT('',(59.4667368016504,12.9646382471638,38.989));
#178630=CARTESIAN_POINT('',(58.9396512752216,18.8168143322219,38.989));
#178631=CARTESIAN_POINT('Origin',(5.49031038273072E-15,0.,38.989));
#178632=CARTESIAN_POINT('',(58.4886806371044,18.6702850894749,38.989));
#178633=CARTESIAN_POINT('Origin',(5.57972911860581E-15,0.,39.624));
#178634=CARTESIAN_POINT('Origin',(58.626452004677,12.7860353045041,39.6240070731883));
#178635=CARTESIAN_POINT('Origin',(57.165014422052,18.2401946149516,39.6240070731883));
#178636=CARTESIAN_POINT('Origin',(5.57972911860581E-15,0.,39.624));
#178637=CARTESIAN_POINT('Origin',(60.4889316843632,13.1819467630385,39.5552135208047));
#178638=CARTESIAN_POINT('Origin',(58.975924479715,18.8285649482875,39.5552117598805));
#178639=CARTESIAN_POINT('Origin',(5.51210908043506E-15,0.,39.1438017080178));
#178640=CARTESIAN_POINT('Origin',(59.6285212670419,12.9989886756685,39.1711625381368));
#178641=CARTESIAN_POINT('Origin',(58.1392191539782,18.5567769230176,39.1712173702607));
#178642=CARTESIAN_POINT('Origin',(5.51210908043507E-15,0.,39.1438017080178));
#178643=CARTESIAN_POINT('Origin',(59.4496656337923,12.9610560404236,39.1712175859393));
#178644=CARTESIAN_POINT('Origin',(57.9653593207591,18.5001997164918,39.1711627526745));
#178645=CARTESIAN_POINT('Origin',(60.4792282238308,0.,38.989));
#178646=CARTESIAN_POINT('',(54.9452378026832,24.115648972427,38.989));
#178647=CARTESIAN_POINT('',(56.9687879773468,18.8441205405512,38.989));
#178648=CARTESIAN_POINT('Origin',(5.49031038273072E-15,0.,38.989));
#178649=CARTESIAN_POINT('',(57.4202585945868,18.9908122363895,38.989));
#178650=CARTESIAN_POINT('',(54.6058629360818,18.0763596539223,38.989));
#178651=CARTESIAN_POINT('',(57.4200769557624,18.9913614317948,38.9889999995774));
#178652=CARTESIAN_POINT('Origin',(5.49031038273072E-15,0.,38.989));
#178653=CARTESIAN_POINT('',(55.3791342583023,24.3081989336286,38.9889999997818));
#178654=CARTESIAN_POINT('Origin',(5.49031038273072E-15,0.,38.989));
#178655=CARTESIAN_POINT('',(55.3789017591236,24.308728605591,38.989));
#178656=CARTESIAN_POINT('Origin',(5.49031038273072E-15,0.,38.989));
#178657=CARTESIAN_POINT('',(54.9457289227643,24.1158676331751,38.989));
#178658=CARTESIAN_POINT('Origin',(5.49031038273072E-15,0.,38.989));
#178659=CARTESIAN_POINT('',(57.5748148483578,19.041637186087,39.2708017080178));
#178660=CARTESIAN_POINT('',(57.4200769550675,18.991361431565,38.989));
#178661=CARTESIAN_POINT('',(55.5277679690275,24.3743766271344,39.2708017078546));
#178662=CARTESIAN_POINT('Origin',(5.52999282761009E-15,0.,39.2708017080178));
#178663=CARTESIAN_POINT('',(55.5277679687686,24.3743766270207,39.2708017080178));
#178664=CARTESIAN_POINT('Origin',(60.71525,0.,39.3978017080178));
#178665=CARTESIAN_POINT('',(55.7284918401501,24.464376137791,39.3978017080178));
#178666=CARTESIAN_POINT('',(57.7842031819385,19.1090650011308,39.3978017080178));
#178667=CARTESIAN_POINT('Origin',(5.5478765747851E-15,0.,39.3978017080178));
#178668=CARTESIAN_POINT('',(57.9280106456678,19.1557908785618,39.3978017080178));
#178669=CARTESIAN_POINT('',(54.8193466381482,18.1457247135484,39.3978017080178));
#178670=CARTESIAN_POINT('',(55.8666273273836,24.5258780191664,39.3978017080178));
#178671=CARTESIAN_POINT('Origin',(5.5478765747851E-15,0.,39.3978017080178));
#178672=CARTESIAN_POINT('',(55.7289760416541,24.4645917181901,39.3978017080178));
#178673=CARTESIAN_POINT('Origin',(5.5478765747851E-15,0.,39.3978017080178));
#178674=CARTESIAN_POINT('',(56.0673542004329,24.6158705164587,39.2708017080178));
#178675=CARTESIAN_POINT('',(58.1373965172492,19.2232259142291,39.2708017081757));
#178676=CARTESIAN_POINT('Origin',(5.52999282761008E-15,0.,39.2708017080178));
#178677=CARTESIAN_POINT('',(58.2921333818759,19.2735045526302,38.9890000005756));
#178678=CARTESIAN_POINT('',(58.1373965169896,19.2232259141432,39.2708017080178));
#178679=CARTESIAN_POINT('',(58.2919551457919,19.2740436149877,38.989));
#178680=CARTESIAN_POINT('Origin',(5.49031038273072E-15,0.,38.989));
#178681=CARTESIAN_POINT('',(56.2162173246401,24.6815255140419,38.989));
#178682=CARTESIAN_POINT('Origin',(5.49031038273072E-15,0.,38.989));
#178683=CARTESIAN_POINT('',(56.2159890767415,24.6820453786625,38.9890000005754));
#178684=CARTESIAN_POINT('Origin',(5.49031038273072E-15,0.,38.989));
#178685=CARTESIAN_POINT('',(56.2159890770395,24.6820453788101,38.989));
#178686=CARTESIAN_POINT('Origin',(62.2224557307631,0.,38.989));
#178687=CARTESIAN_POINT('',(58.7434254837935,19.4207352200693,38.989));
#178688=CARTESIAN_POINT('',(56.182627028633,18.588681363905,38.989));
#178689=CARTESIAN_POINT('',(56.6498810128385,24.8746050278046,38.989));
#178690=CARTESIAN_POINT('Origin',(5.49031038273072E-15,0.,38.989));
#178691=CARTESIAN_POINT('',(56.2166973156309,24.6817392197998,38.989));
#178692=CARTESIAN_POINT('Origin',(5.57972911860581E-15,0.,39.624));
#178693=CARTESIAN_POINT('Origin',(56.9687855447427,18.8441250001648,39.6240070731883));
#178694=CARTESIAN_POINT('Origin',(54.94523897897,24.1156440305582,39.6240070731883));
#178695=CARTESIAN_POINT('Origin',(5.57972911860581E-15,0.,39.624));
#178696=CARTESIAN_POINT('Origin',(58.77967834952,19.4325497530897,39.5552135208021));
#178697=CARTESIAN_POINT('Origin',(56.6847272350833,24.8900828550895,39.555211759879));
#178698=CARTESIAN_POINT('Origin',(5.51210908043506E-15,0.,39.1438017080178));
#178699=CARTESIAN_POINT('Origin',(57.9431056782062,19.1606565505636,39.1711625381395));
#178700=CARTESIAN_POINT('Origin',(55.8810150532815,24.5323241911521,39.171217370259));
#178701=CARTESIAN_POINT('Origin',(5.51210908043507E-15,0.,39.1438017080178));
#178702=CARTESIAN_POINT('Origin',(57.7691948748958,19.1042362097737,39.1712175859413));
#178703=CARTESIAN_POINT('Origin',(55.7140215708744,24.4578836192922,39.1711627526757));
#178704=CARTESIAN_POINT('Origin',(60.4792282238308,0.,38.989));
#178705=CARTESIAN_POINT('',(52.123470313195,29.7268821954843,38.989));
#178706=CARTESIAN_POINT('',(54.68696003433,24.6957503380301,38.989));
#178707=CARTESIAN_POINT('Origin',(5.49031038273072E-15,0.,38.989));
#178708=CARTESIAN_POINT('',(55.1206239907505,24.8888299712405,38.989));
#178709=CARTESIAN_POINT('',(50.3447265545032,22.7624634345041,38.989));
#178710=CARTESIAN_POINT('',(55.1203859404108,24.8893571716688,38.9889999995774));
#178711=CARTESIAN_POINT('Origin',(5.49031038273072E-15,0.,38.989));
#178712=CARTESIAN_POINT('',(52.5348628870842,29.9637318775748,38.9889999997818));
#178713=CARTESIAN_POINT('Origin',(5.49031038273072E-15,0.,38.989));
#178714=CARTESIAN_POINT('',(52.5345762957642,29.9642343451569,38.989));
#178715=CARTESIAN_POINT('Origin',(5.49031038273072E-15,0.,38.989));
#178716=CARTESIAN_POINT('',(52.123935886597,29.7271509944133,38.989));
#178717=CARTESIAN_POINT('Origin',(5.49031038273072E-15,0.,38.989));
#178718=CARTESIAN_POINT('',(55.2690209153043,24.9555320242408,39.2708017080178));
#178719=CARTESIAN_POINT('',(55.1203859397437,24.8893571713676,38.989));
#178720=CARTESIAN_POINT('',(52.6757649141856,30.0450834961231,39.2708017078546));
#178721=CARTESIAN_POINT('Origin',(5.52999282761009E-15,0.,39.2708017080178));
#178722=CARTESIAN_POINT('',(52.67576491394,30.045083495983,39.2708017080178));
#178723=CARTESIAN_POINT('Origin',(60.71525,0.,39.3978017080178));
#178724=CARTESIAN_POINT('',(52.8659816883963,30.1555713378331,39.3978017080178));
#178725=CARTESIAN_POINT('',(55.470214071797,25.0444775033941,39.3978017080178));
#178726=CARTESIAN_POINT('Origin',(5.5478765747851E-15,0.,39.3978017080178));
#178727=CARTESIAN_POINT('',(55.6083495590305,25.1059793847695,39.3978017080178));
#178728=CARTESIAN_POINT('',(50.5417021396889,22.8501626153342,39.3978017080178));
#178729=CARTESIAN_POINT('',(52.9969317578291,30.2311753956706,39.3978017080178));
#178730=CARTESIAN_POINT('Origin',(5.5478765747851E-15,0.,39.3978017080178));
#178731=CARTESIAN_POINT('',(52.866440703106,30.1558363500993,39.3978017080178));
#178732=CARTESIAN_POINT('Origin',(5.5478765747851E-15,0.,39.3978017080178));
#178733=CARTESIAN_POINT('',(53.1871522506179,30.3416565762229,39.2708017080178));
#178734=CARTESIAN_POINT('',(55.8095395122503,25.1949317876419,39.2708017081757));
#178735=CARTESIAN_POINT('Origin',(5.52999282761008E-15,0.,39.2708017080178));
#178736=CARTESIAN_POINT('',(55.9581731633348,25.2611094010714,38.9890000005756));
#178737=CARTESIAN_POINT('',(55.809539512001,25.1949317875294,39.2708017080178));
#178738=CARTESIAN_POINT('',(55.9579395562869,25.261626879645,38.989));
#178739=CARTESIAN_POINT('Origin',(5.49031038273072E-15,0.,38.989));
#178740=CARTESIAN_POINT('',(53.3283370710516,30.4225123424704,38.989));
#178741=CARTESIAN_POINT('Origin',(5.49031038273072E-15,0.,38.989));
#178742=CARTESIAN_POINT('',(53.328055732869,30.4230055008161,38.9890000005754));
#178743=CARTESIAN_POINT('Origin',(5.49031038273072E-15,0.,38.989));
#178744=CARTESIAN_POINT('',(53.32805573315,30.4230055009941,38.989));
#178745=CARTESIAN_POINT('Origin',(62.2224557307631,0.,38.989));
#178746=CARTESIAN_POINT('',(56.3916032444854,25.4547063934076,38.989));
#178747=CARTESIAN_POINT('',(51.7995637473369,23.4101986852074,38.989));
#178748=CARTESIAN_POINT('',(53.7394427993291,30.6598643453568,38.989));
#178749=CARTESIAN_POINT('Origin',(5.49031038273072E-15,0.,38.989));
#178750=CARTESIAN_POINT('',(53.3287920942672,30.4227750502464,38.989));
#178751=CARTESIAN_POINT('Origin',(5.57972911860581E-15,0.,39.624));
#178752=CARTESIAN_POINT('Origin',(54.6869571488954,24.6957545189371,39.6240070731883));
#178753=CARTESIAN_POINT('Origin',(52.1234719996039,29.7268774036431,39.6240070731883));
#178754=CARTESIAN_POINT('Origin',(5.57972911860581E-15,0.,39.624));
#178755=CARTESIAN_POINT('Origin',(56.4264225582409,25.4702456615226,39.5552135207995));
#178756=CARTESIAN_POINT('Origin',(53.7724802568187,30.6788998055464,39.5552117598838));
#178757=CARTESIAN_POINT('Origin',(5.51210908043506E-15,0.,39.1438017080178));
#178758=CARTESIAN_POINT('Origin',(55.6228532981798,25.1123962626632,39.1711625381312));
#178759=CARTESIAN_POINT('Origin',(53.0105668578091,30.2390901817305,39.1712173702627));
#178760=CARTESIAN_POINT('Origin',(5.51210908043507E-15,0.,39.1438017080178));
#178761=CARTESIAN_POINT('Origin',(55.4557927279734,25.03810636939,39.1712175859376));
#178762=CARTESIAN_POINT('Origin',(52.8522693417516,30.1476018310223,39.1711627526727));
#178763=CARTESIAN_POINT('Origin',(60.4792282238308,0.,38.989));
#178764=CARTESIAN_POINT('',(48.7306271754181,35.0124214764579,38.989));
#178765=CARTESIAN_POINT('',(51.805970313195,30.2768083268874,38.989));
#178766=CARTESIAN_POINT('Origin',(5.49031038273072E-15,0.,38.989));
#178767=CARTESIAN_POINT('',(52.2170762957395,30.5141604766041,38.989));
#178768=CARTESIAN_POINT('',(45.2006711678738,26.4632370872583,38.989));
#178769=CARTESIAN_POINT('',(52.2167844420139,30.5146599059371,38.9889999995774));
#178770=CARTESIAN_POINT('Origin',(5.49031038273072E-15,0.,38.989));
#178771=CARTESIAN_POINT('',(49.1150085644485,35.2909759047562,38.9889999997818));
#178772=CARTESIAN_POINT('Origin',(5.49031038273072E-15,0.,38.989));
#178773=CARTESIAN_POINT('',(49.1146710209415,35.2914456628181,38.989));
#178774=CARTESIAN_POINT('Origin',(5.49031038273072E-15,0.,38.989));
#178775=CARTESIAN_POINT('',(48.7310621012213,35.0127374685504,38.989));
#178776=CARTESIAN_POINT('Origin',(5.49031038273072E-15,0.,38.989));
#178777=CARTESIAN_POINT('',(52.3576880233166,30.5960088312562,39.2708017080178));
#178778=CARTESIAN_POINT('',(52.2167844413819,30.5146599055678,38.989));
#178779=CARTESIAN_POINT('',(49.2466351558313,35.3866101429904,39.2708017078546));
#178780=CARTESIAN_POINT('Origin',(5.52999282761009E-15,0.,39.2708017080178));
#178781=CARTESIAN_POINT('',(49.2466351556017,35.3866101428254,39.2708017080178));
#178782=CARTESIAN_POINT('Origin',(60.71525,0.,39.3978017080178));
#178783=CARTESIAN_POINT('',(49.4242607783465,35.516375787839,39.3978017080178));
#178784=CARTESIAN_POINT('',(52.5484816883963,30.7054974692362,39.3978017080178));
#178785=CARTESIAN_POINT('Origin',(5.5478765747851E-15,0.,39.3978017080178));
#178786=CARTESIAN_POINT('',(52.6794317578291,30.7811015270737,39.3978017080178));
#178787=CARTESIAN_POINT('',(45.3776875000007,26.5654375142627,39.3978017080178));
#178788=CARTESIAN_POINT('',(49.5465907136149,35.6052536882596,39.3978017080178));
#178789=CARTESIAN_POINT('Origin',(5.5478765747851E-15,0.,39.3978017080178));
#178790=CARTESIAN_POINT('',(49.4246895772007,35.5166873284425,39.3978017080178));
#178791=CARTESIAN_POINT('Origin',(5.5478765747851E-15,0.,39.3978017080178));
#178792=CARTESIAN_POINT('',(49.7242207306179,35.7350130971383,39.2708017080178));
#178793=CARTESIAN_POINT('',(52.8702215134581,30.8905967160109,39.2708017081757));
#178794=CARTESIAN_POINT('Origin',(5.52999282761008E-15,0.,39.2708017080178));
#178795=CARTESIAN_POINT('',(53.0111234896157,30.9719482486875,38.9890000005756));
#178796=CARTESIAN_POINT('',(52.870221513222,30.8905967158729,39.2708017080178));
#178797=CARTESIAN_POINT('',(53.0108370710516,30.9724384738736,38.989));
#178798=CARTESIAN_POINT('Origin',(5.49031038273072E-15,0.,38.989));
#178799=CARTESIAN_POINT('',(49.8561803968407,35.8301837593549,38.989));
#178800=CARTESIAN_POINT('Origin',(5.49031038273072E-15,0.,38.989));
#178801=CARTESIAN_POINT('',(49.8558490507741,35.8306448082797,38.9890000005754));
#178802=CARTESIAN_POINT('Origin',(5.49031038273072E-15,0.,38.989));
#178803=CARTESIAN_POINT('',(49.8558490510349,35.830644808486,38.989));
#178804=CARTESIAN_POINT('Origin',(62.2224557307631,0.,38.989));
#178805=CARTESIAN_POINT('',(53.4219427993291,31.2097904767599,38.989));
#178806=CARTESIAN_POINT('',(46.508091798073,27.2180767400479,38.989));
#178807=CARTESIAN_POINT('',(50.2402240048087,36.1092077731522,38.989));
#178808=CARTESIAN_POINT('Origin',(5.49031038273072E-15,0.,38.989));
#178809=CARTESIAN_POINT('',(49.8566054669514,35.8304925908676,38.989));
#178810=CARTESIAN_POINT('Origin',(5.57972911860581E-15,0.,39.624));
#178811=CARTESIAN_POINT('Origin',(51.8059670065433,30.2768121832809,39.6240070731883));
#178812=CARTESIAN_POINT('Origin',(48.7306293534724,35.0124168871446,39.6240070731883));
#178813=CARTESIAN_POINT('Origin',(5.57972911860581E-15,0.,39.624));
#178814=CARTESIAN_POINT('Origin',(53.454947073427,31.2288842284962,39.5552135207965));
#178815=CARTESIAN_POINT('Origin',(50.271090732248,36.1315923097651,39.5552117598796));
#178816=CARTESIAN_POINT('Origin',(5.51210908043506E-15,0.,39.1438017080178));
#178817=CARTESIAN_POINT('Origin',(52.6931852975962,30.7889993062059,39.1711625381385));
#178818=CARTESIAN_POINT('Origin',(49.5593237986654,35.6145503723399,39.1712173702604));
#178819=CARTESIAN_POINT('Origin',(5.51210908043507E-15,0.,39.1438017080178));
#178820=CARTESIAN_POINT('Origin',(52.5348053110498,30.6976537960598,39.1712175859399));
#178821=CARTESIAN_POINT('Origin',(49.4114565896725,35.507016608296,39.171162752673));
#178822=CARTESIAN_POINT('Origin',(60.4792282238308,0.,38.989));
#178823=CARTESIAN_POINT('',(44.8038810887679,39.9143573409152,38.989));
#178824=CARTESIAN_POINT('',(48.3573835402124,35.526147267886,38.989));
#178825=CARTESIAN_POINT('Origin',(5.49031038273072E-15,0.,38.989));
#178826=CARTESIAN_POINT('',(48.7414273857065,35.8051714542874,38.989));
#178827=CARTESIAN_POINT('',(39.3975469582356,29.0164449471018,38.989));
#178828=CARTESIAN_POINT('',(48.7410849262056,35.805637640673,38.9889999995773));
#178829=CARTESIAN_POINT('Origin',(5.49031038273072E-15,0.,38.989));
#178830=CARTESIAN_POINT('',(45.1570399300043,40.2315646148137,38.9889999997818));
#178831=CARTESIAN_POINT('Origin',(5.49031038273072E-15,0.,38.989));
#178832=CARTESIAN_POINT('',(45.1566551325076,40.2319965165876,38.989));
#178833=CARTESIAN_POINT('Origin',(5.49031038273072E-15,0.,38.989));
#178834=CARTESIAN_POINT('',(44.8042806018342,39.9147170640958,38.989));
#178835=CARTESIAN_POINT('Origin',(5.49031038273072E-15,0.,38.989));
#178836=CARTESIAN_POINT('',(48.8727133447948,35.9012693628899,39.2708017080178));
#178837=CARTESIAN_POINT('',(48.7410849256156,35.8056376402395,38.989));
#178838=CARTESIAN_POINT('',(45.2779489571888,40.3404336840068,39.2708017078546));
#178839=CARTESIAN_POINT('Origin',(5.52999282761009E-15,0.,39.2708017080178));
#178840=CARTESIAN_POINT('',(45.2779489569777,40.3404336838187,39.2708017080178));
#178841=CARTESIAN_POINT('Origin',(60.71525,0.,39.3978017080178));
#178842=CARTESIAN_POINT('',(45.4410373245177,40.4880553924338,39.3978017080178));
#178843=CARTESIAN_POINT('',(49.0510171431408,36.0301015792671,39.3978017080178));
#178844=CARTESIAN_POINT('Origin',(5.5478765747851E-15,0.,39.3978017080178));
#178845=CARTESIAN_POINT('',(49.1733470784092,36.1189794796877,39.3978017080178));
#178846=CARTESIAN_POINT('',(39.5520252162596,29.1286799712085,39.3978017080178));
#178847=CARTESIAN_POINT('',(45.5534068532516,40.5892333705617,39.3978017080178));
#178848=CARTESIAN_POINT('Origin',(5.5478765747851E-15,0.,39.3978017080178));
#178849=CARTESIAN_POINT('',(45.4414312095063,40.4884100480706,39.3978017080178));
#178850=CARTESIAN_POINT('Origin',(5.5478765747851E-15,0.,39.3978017080178));
#178851=CARTESIAN_POINT('',(45.7165002428312,40.7368493365292,39.2708017080178));
#178852=CARTESIAN_POINT('',(49.3516463039594,36.2478178024864,39.2708017081757));
#178853=CARTESIAN_POINT('Origin',(5.52999282761008E-15,0.,39.2708017080178));
#178854=CARTESIAN_POINT('',(49.4832728536536,36.3434519499941,38.9890000005756));
#178855=CARTESIAN_POINT('',(49.351646303739,36.2478178023245,39.2708017080178));
#178856=CARTESIAN_POINT('',(49.482936761635,36.343909550783,38.989));
#178857=CARTESIAN_POINT('Origin',(5.49031038273072E-15,0.,38.989));
#178858=CARTESIAN_POINT('',(45.8377889771256,40.8452921850238,38.989));
#178859=CARTESIAN_POINT('Origin',(5.49031038273072E-15,0.,38.989));
#178860=CARTESIAN_POINT('',(45.8374112534718,40.8457160731792,38.9890000005754));
#178861=CARTESIAN_POINT('Origin',(5.49031038273072E-15,0.,38.989));
#178862=CARTESIAN_POINT('',(45.8374112537096,40.8457160734117,38.989));
#178863=CARTESIAN_POINT('Origin',(62.2224557307631,0.,38.989));
#178864=CARTESIAN_POINT('',(49.866980369603,36.6229335645803,38.989));
#178865=CARTESIAN_POINT('',(40.5385041740537,29.8453988870283,38.989));
#178866=CARTESIAN_POINT('',(46.190562802649,41.1629311642475,38.989));
#178867=CARTESIAN_POINT('Origin',(5.49031038273072E-15,0.,38.989));
#178868=CARTESIAN_POINT('',(45.8381794369742,40.8456437566507,38.989));
#178869=CARTESIAN_POINT('Origin',(5.57972911860581E-15,0.,39.624));
#178870=CARTESIAN_POINT('Origin',(48.3573798485719,35.5261507575145,39.6240070731883));
#178871=CARTESIAN_POINT('Origin',(44.8038837346046,39.9143530044112,39.6240070731883));
#178872=CARTESIAN_POINT('Origin',(5.57972911860581E-15,0.,39.624));
#178873=CARTESIAN_POINT('Origin',(49.8978080023047,36.6453726047993,39.5552135208004));
#178874=CARTESIAN_POINT('Origin',(46.2189206177148,41.1884195276092,39.5552117598801));
#178875=CARTESIAN_POINT('Origin',(5.51210908043506E-15,0.,39.1438017080178));
#178876=CARTESIAN_POINT('Origin',(49.18619973213,36.1282716303355,39.1711625381374));
#178877=CARTESIAN_POINT('Origin',(45.5650984170279,40.5998100962455,39.1712173702563));
#178878=CARTESIAN_POINT('Origin',(5.51210908043507E-15,0.,39.1438017080178));
#178879=CARTESIAN_POINT('Origin',(49.0382355735257,36.0208713038458,39.1712175859374));
#178880=CARTESIAN_POINT('Origin',(45.4292815791832,40.4774090812886,39.1711627526757));
#178881=CARTESIAN_POINT('Origin',(60.4792282238308,0.,38.989));
#178882=CARTESIAN_POINT('',(40.3862543050944,44.3789831537291,38.989));
#178883=CARTESIAN_POINT('',(44.37898315373,40.3862543050933,38.989));
#178884=CARTESIAN_POINT('Origin',(5.49031038273072E-15,0.,38.989));
#178885=CARTESIAN_POINT('',(44.7317571974364,40.7038934808038,38.989));
#178886=CARTESIAN_POINT('',(33.1880655373225,30.3099068238763,38.989));
#178887=CARTESIAN_POINT('',(44.731367884218,40.7043213166062,38.9889999995773));
#178888=CARTESIAN_POINT('Origin',(5.49031038273072E-15,0.,38.989));
#178889=CARTESIAN_POINT('',(40.7043213163689,44.7313678839551,38.9889999997818));
#178890=CARTESIAN_POINT('Origin',(5.49031038273072E-15,0.,38.989));
#178891=CARTESIAN_POINT('',(40.7038934808044,44.7317571974349,38.989));
#178892=CARTESIAN_POINT('Origin',(5.49031038273072E-15,0.,38.989));
#178893=CARTESIAN_POINT('',(40.386614028275,44.3793826667954,38.989));
#178894=CARTESIAN_POINT('Origin',(5.49031038273072E-15,0.,38.989));
#178895=CARTESIAN_POINT('',(44.8522789915946,40.8131880745601,39.2708017080178));
#178896=CARTESIAN_POINT('',(44.7313678836765,40.7043213161134,38.989));
#178897=CARTESIAN_POINT('',(40.8131880747515,44.8522789918028,39.2708017078546));
#178898=CARTESIAN_POINT('Origin',(5.52999282761009E-15,0.,39.2708017080178));
#178899=CARTESIAN_POINT('',(40.8131880745612,44.8522789915937,39.2708017080178));
#178900=CARTESIAN_POINT('Origin',(60.71525,0.,39.3978017080178));
#178901=CARTESIAN_POINT('',(40.959952356613,45.0161393894788,39.3978017080178));
#178902=CARTESIAN_POINT('',(45.0161393894798,40.959952356612,39.3978017080178));
#178903=CARTESIAN_POINT('Origin',(5.5478765747851E-15,0.,39.3978017080178));
#178904=CARTESIAN_POINT('',(45.1285089182138,41.0611303347399,39.3978017080178));
#178905=CARTESIAN_POINT('',(33.3184119221875,30.4272712359683,39.3978017080178));
#178906=CARTESIAN_POINT('',(41.0611303347409,45.1285089182128,39.3978017080178));
#178907=CARTESIAN_POINT('Origin',(5.5478765747851E-15,0.,39.3978017080178));
#178908=CARTESIAN_POINT('',(40.9603070122498,45.0165332744675,39.3978017080178));
#178909=CARTESIAN_POINT('Origin',(5.5478765747851E-15,0.,39.3978017080178));
#178910=CARTESIAN_POINT('',(41.2079002115913,45.2923641298552,39.2708017080178));
#178911=CARTESIAN_POINT('',(45.2923641300585,41.2079002117742,39.2708017081757));
#178912=CARTESIAN_POINT('Origin',(5.52999282761008E-15,0.,39.2708017080178));
#178913=CARTESIAN_POINT('',(45.4132731252663,41.3167691863804,38.9890000005756));
#178914=CARTESIAN_POINT('',(45.2923641298562,41.2079002115902,39.2708017080178));
#178915=CARTESIAN_POINT('',(45.4128910420877,41.317189149202,38.989));
#178916=CARTESIAN_POINT('Origin',(5.49031038273072E-15,0.,38.989));
#178917=CARTESIAN_POINT('',(41.3171891492031,45.4128910420867,38.989));
#178918=CARTESIAN_POINT('Origin',(5.49031038273072E-15,0.,38.989));
#178919=CARTESIAN_POINT('',(41.3167691863815,45.4132731252654,38.9890000005754));
#178920=CARTESIAN_POINT('Origin',(5.49031038273072E-15,0.,38.989));
#178921=CARTESIAN_POINT('',(41.3167691865937,45.4132731255215,38.989));
#178922=CARTESIAN_POINT('Origin',(62.2224557307631,0.,38.989));
#178923=CARTESIAN_POINT('',(45.7656648676111,41.6348281284257,38.989));
#178924=CARTESIAN_POINT('',(34.1507877370015,31.1767457860025,38.989));
#178925=CARTESIAN_POINT('',(41.6348281284267,45.7656648676101,38.989));
#178926=CARTESIAN_POINT('Origin',(5.49031038273072E-15,0.,38.989));
#178927=CARTESIAN_POINT('',(41.3175407208299,45.4132815019354,38.989));
#178928=CARTESIAN_POINT('Origin',(5.57972911860581E-15,0.,39.624));
#178929=CARTESIAN_POINT('Origin',(44.3789791175472,40.3862573897239,39.6240070731883));
#178930=CARTESIAN_POINT('Origin',(40.386257389725,44.3789791175462,39.6240070731883));
#178931=CARTESIAN_POINT('Origin',(5.57972911860581E-15,0.,39.624));
#178932=CARTESIAN_POINT('Origin',(45.7939781049223,41.6603666103081,39.5552135208011));
#178933=CARTESIAN_POINT('Origin',(41.6603663369573,45.7939778018841,39.5552117598806));
#178934=CARTESIAN_POINT('Origin',(5.51210908043506E-15,0.,39.1438017080178));
#178935=CARTESIAN_POINT('Origin',(45.1403198695228,41.0717150501545,39.1711625381326));
#178936=CARTESIAN_POINT('Origin',(41.0716522820274,45.1402498046835,39.1712173702617));
#178937=CARTESIAN_POINT('Origin',(5.51210908043507E-15,0.,39.1438017080178));
#178938=CARTESIAN_POINT('Origin',(45.0043926651423,40.949436607778,39.171217585939));
#178939=CARTESIAN_POINT('Origin',(40.9493738530264,45.0043225899457,39.1711627526739));
#178940=CARTESIAN_POINT('Origin',(60.4792282238308,0.,38.989));
#178941=CARTESIAN_POINT('',(35.5261472678871,48.3573835402115,38.989));
#178942=CARTESIAN_POINT('',(39.9143573409162,44.803881088767,38.989));
#178943=CARTESIAN_POINT('Origin',(5.49031038273072E-15,0.,38.989));
#178944=CARTESIAN_POINT('',(40.2319965165892,45.1566551325071,38.989));
#178945=CARTESIAN_POINT('',(26.8427652369017,30.2864073093063,38.989));
#178946=CARTESIAN_POINT('',(40.2315646150503,45.1570399302677,38.9889999995773));
#178947=CARTESIAN_POINT('Origin',(5.49031038273072E-15,0.,38.989));
#178948=CARTESIAN_POINT('',(35.8056376404645,48.7410849259194,38.9889999997818));
#178949=CARTESIAN_POINT('Origin',(5.49031038273072E-15,0.,38.989));
#178950=CARTESIAN_POINT('',(35.8051714542882,48.7414273857052,38.989));
#178951=CARTESIAN_POINT('Origin',(5.49031038273072E-15,0.,38.989));
#178952=CARTESIAN_POINT('',(35.5264632599797,48.3578184660147,38.989));
#178953=CARTESIAN_POINT('Origin',(5.49031038273072E-15,0.,38.989));
#178954=CARTESIAN_POINT('',(40.3404336838198,45.2779489569768,39.2708017080178));
#178955=CARTESIAN_POINT('',(40.2315646145633,45.1570399297211,38.989));
#178956=CARTESIAN_POINT('',(35.9012693630584,48.8727133450218,39.2708017078546));
#178957=CARTESIAN_POINT('Origin',(5.52999282761009E-15,0.,39.2708017080178));
#178958=CARTESIAN_POINT('',(35.901269362891,48.8727133447939,39.2708017080178));
#178959=CARTESIAN_POINT('Origin',(60.71525,0.,39.3978017080178));
#178960=CARTESIAN_POINT('',(36.0301015792682,49.0510171431399,39.3978017080178));
#178961=CARTESIAN_POINT('',(40.4880553924349,45.4410373245167,39.3978017080178));
#178962=CARTESIAN_POINT('Origin',(5.5478765747851E-15,0.,39.3978017080178));
#178963=CARTESIAN_POINT('',(40.5892333705628,45.5534068532507,39.3978017080178));
#178964=CARTESIAN_POINT('',(26.948440628206,30.4037717213983,39.3978017080178));
#178965=CARTESIAN_POINT('',(36.1189794796889,49.1733470784083,39.3978017080178));
#178966=CARTESIAN_POINT('Origin',(5.5478765747851E-15,0.,39.3978017080178));
#178967=CARTESIAN_POINT('',(36.0304131198717,49.0514459419941,39.3978017080178));
#178968=CARTESIAN_POINT('Origin',(5.5478765747851E-15,0.,39.3978017080178));
#178969=CARTESIAN_POINT('',(36.2478178023256,49.3516463037381,39.2708017080178));
#178970=CARTESIAN_POINT('',(40.7368493367122,45.7165002430344,39.2708017081757));
#178971=CARTESIAN_POINT('Origin',(5.52999282761008E-15,0.,39.2708017080178));
#178972=CARTESIAN_POINT('',(40.8457160731802,45.8374112534707,38.9890000005756));
#178973=CARTESIAN_POINT('',(40.7368493365303,45.7165002428302,39.2708017080178));
#178974=CARTESIAN_POINT('',(40.8452921850249,45.8377889771246,38.989));
#178975=CARTESIAN_POINT('Origin',(5.49031038273072E-15,0.,38.989));
#178976=CARTESIAN_POINT('',(36.3439095507841,49.4829367616342,38.989));
#178977=CARTESIAN_POINT('Origin',(5.49031038273072E-15,0.,38.989));
#178978=CARTESIAN_POINT('',(36.3434519499953,49.4832728536528,38.9890000005754));
#178979=CARTESIAN_POINT('Origin',(5.49031038273072E-15,0.,38.989));
#178980=CARTESIAN_POINT('',(36.3434519501796,49.4832728539297,38.989));
#178981=CARTESIAN_POINT('Origin',(62.2224557307631,0.,38.989));
#178982=CARTESIAN_POINT('',(41.1629311642486,46.190562802648,38.989));
#178983=CARTESIAN_POINT('',(27.6232705441551,31.1532462714325,38.989));
#178984=CARTESIAN_POINT('',(36.6229335645815,49.8669803696022,38.989));
#178985=CARTESIAN_POINT('Origin',(5.49031038273072E-15,0.,38.989));
#178986=CARTESIAN_POINT('',(36.3442183822969,49.4833618317448,38.989));
#178987=CARTESIAN_POINT('Origin',(5.57972911860581E-15,0.,39.624));
#178988=CARTESIAN_POINT('Origin',(39.9143530044124,44.8038837346035,39.6240070731883));
#178989=CARTESIAN_POINT('Origin',(35.5261507575157,48.357379848571,39.6240070731883));
#178990=CARTESIAN_POINT('Origin',(5.57972911860581E-15,0.,39.624));
#178991=CARTESIAN_POINT('Origin',(41.1884198004163,46.2189209212438,39.5552135207988));
#178992=CARTESIAN_POINT('Origin',(36.6453723646245,49.8978076723501,39.5552117598822));
#178993=CARTESIAN_POINT('Origin',(5.51210908043506E-15,0.,39.1438017080178));
#178994=CARTESIAN_POINT('Origin',(40.5998732162095,45.5651681650781,39.1711625381354));
#178995=CARTESIAN_POINT('Origin',(36.1282165298278,49.1861234900562,39.1712173702643));
#178996=CARTESIAN_POINT('Origin',(5.51210908043507E-15,0.,39.1438017080178));
#178997=CARTESIAN_POINT('Origin',(40.4774722129479,45.4293513150122,39.1712175859383));
#178998=CARTESIAN_POINT('Origin',(36.0208162177228,49.0381593225517,39.1711627526726));
#178999=CARTESIAN_POINT('Origin',(60.4792282238308,0.,38.989));
#179000=CARTESIAN_POINT('',(30.2768083268887,51.8059703131943,38.989));
#179001=CARTESIAN_POINT('',(35.012421476459,48.7306271754172,38.989));
#179002=CARTESIAN_POINT('Origin',(5.49031038273072E-15,0.,38.989));
#179003=CARTESIAN_POINT('',(35.2914456628196,49.1146710209411,38.989));
#179004=CARTESIAN_POINT('',(20.6381965522797,28.9462038689911,38.989));
#179005=CARTESIAN_POINT('',(35.2909759049641,49.1150085647353,38.9889999995772));
#179006=CARTESIAN_POINT('Origin',(5.49031038273072E-15,0.,38.989));
#179007=CARTESIAN_POINT('',(30.5146599057598,52.2167844417075,38.9889999997818));
#179008=CARTESIAN_POINT('Origin',(5.49031038273072E-15,0.,38.989));
#179009=CARTESIAN_POINT('',(30.5141604766051,52.2170762957381,38.989));
#179010=CARTESIAN_POINT('Origin',(5.49031038273072E-15,0.,38.989));
#179011=CARTESIAN_POINT('',(30.2770771258177,51.8064358865963,38.989));
#179012=CARTESIAN_POINT('Origin',(5.49031038273072E-15,0.,38.989));
#179013=CARTESIAN_POINT('',(35.3866101428265,49.2466351556009,39.2708017080178));
#179014=CARTESIAN_POINT('',(35.2909759045368,49.1150085641407,38.989));
#179015=CARTESIAN_POINT('',(30.5960088314001,52.35768802356,39.2708017078546));
#179016=CARTESIAN_POINT('Origin',(5.52999282761009E-15,0.,39.2708017080178));
#179017=CARTESIAN_POINT('',(30.5960088312575,52.3576880233159,39.2708017080178));
#179018=CARTESIAN_POINT('Origin',(60.71525,0.,39.3978017080178));
#179019=CARTESIAN_POINT('',(30.7054974692375,52.5484816883955,39.3978017080178));
#179020=CARTESIAN_POINT('',(35.5163757878401,49.4242607783457,39.3978017080178));
#179021=CARTESIAN_POINT('Origin',(5.5478765747851E-15,0.,39.3978017080178));
#179022=CARTESIAN_POINT('',(35.6052536882608,49.5465907136141,39.3978017080178));
#179023=CARTESIAN_POINT('',(20.7197400704249,29.0584388930977,39.3978017080178));
#179024=CARTESIAN_POINT('',(30.781101527075,52.6794317578284,39.3978017080178));
#179025=CARTESIAN_POINT('Origin',(5.5478765747851E-15,0.,39.3978017080178));
#179026=CARTESIAN_POINT('',(30.7057624815037,52.5489407031053,39.3978017080178));
#179027=CARTESIAN_POINT('Origin',(5.5478765747851E-15,0.,39.3978017080178));
#179028=CARTESIAN_POINT('',(30.8905967158742,52.8702215132212,39.2708017080178));
#179029=CARTESIAN_POINT('',(35.7350130972991,49.7242207308392,39.2708017081757));
#179030=CARTESIAN_POINT('Origin',(5.52999282761008E-15,0.,39.2708017080178));
#179031=CARTESIAN_POINT('',(35.8306448082808,49.8558490507732,38.9890000005756));
#179032=CARTESIAN_POINT('',(35.7350130971395,49.7242207306171,39.2708017080178));
#179033=CARTESIAN_POINT('',(35.8301837593561,49.8561803968399,38.989));
#179034=CARTESIAN_POINT('Origin',(5.49031038273072E-15,0.,38.989));
#179035=CARTESIAN_POINT('',(30.9724384738749,53.0108370710509,38.989));
#179036=CARTESIAN_POINT('Origin',(5.49031038273072E-15,0.,38.989));
#179037=CARTESIAN_POINT('',(30.9719482486888,53.011123489615,38.9890000005754));
#179038=CARTESIAN_POINT('Origin',(5.49031038273072E-15,0.,38.989));
#179039=CARTESIAN_POINT('',(30.9719482488431,53.0111234899096,38.989));
#179040=CARTESIAN_POINT('Origin',(62.2224557307631,0.,38.989));
#179041=CARTESIAN_POINT('',(36.1092077731534,50.2402240048079,38.989));
#179042=CARTESIAN_POINT('',(21.2404668433939,29.7751578089176,38.989));
#179043=CARTESIAN_POINT('',(31.2097904767612,53.4219427993283,38.989));
#179044=CARTESIAN_POINT('Origin',(5.49031038273072E-15,0.,38.989));
#179045=CARTESIAN_POINT('',(30.9727011816508,53.0112920942664,38.989));
#179046=CARTESIAN_POINT('Origin',(5.57972911860581E-15,0.,39.624));
#179047=CARTESIAN_POINT('Origin',(35.0124168871459,48.7306293534715,39.6240070731883));
#179048=CARTESIAN_POINT('Origin',(30.2768121832823,51.8059670065424,39.6240070731883));
#179049=CARTESIAN_POINT('Origin',(5.57972911860581E-15,0.,39.624));
#179050=CARTESIAN_POINT('Origin',(36.131592549347,50.2710910626322,39.5552135207999));
#179051=CARTESIAN_POINT('Origin',(31.22888402413,53.4549467201701,39.5552117598832));
#179052=CARTESIAN_POINT('Origin',(5.51210908043506E-15,0.,39.1438017080178));
#179053=CARTESIAN_POINT('Origin',(35.6146058558682,49.5593997624593,39.1711625381345));
#179054=CARTESIAN_POINT('Origin',(30.7889524770109,52.6931037136121,39.1712173702631));
#179055=CARTESIAN_POINT('Origin',(5.51210908043507E-15,0.,39.1438017080178));
#179056=CARTESIAN_POINT('Origin',(35.5070721047336,49.411532542537,39.1712175859357));
#179057=CARTESIAN_POINT('Origin',(30.6976069821061,52.5347237197182,39.1711627526718));
#179058=CARTESIAN_POINT('Origin',(60.4792282238308,0.,38.989));
#179059=CARTESIAN_POINT('',(24.6957503380314,54.6869600343295,38.989));
#179060=CARTESIAN_POINT('',(29.7268821954856,52.1234703131943,38.989));
#179061=CARTESIAN_POINT('Origin',(5.49031038273072E-15,0.,38.989));
#179062=CARTESIAN_POINT('',(29.9642343451585,52.534576295764,38.989));
#179063=CARTESIAN_POINT('',(14.8448439902567,26.3470240215575,38.989));
#179064=CARTESIAN_POINT('',(29.9637318777514,52.534862887391,38.9889999995774));
#179065=CARTESIAN_POINT('Origin',(5.49031038273072E-15,0.,38.989));
#179066=CARTESIAN_POINT('',(24.8893571715245,55.1203859400877,38.9889999997818));
#179067=CARTESIAN_POINT('Origin',(5.49031038273072E-15,0.,38.989));
#179068=CARTESIAN_POINT('',(24.8888299712416,55.1206239907494,38.989));
#179069=CARTESIAN_POINT('Origin',(5.49031038273072E-15,0.,38.989));
#179070=CARTESIAN_POINT('',(24.6959689987794,54.6874511544106,38.989));
#179071=CARTESIAN_POINT('Origin',(5.49031038273072E-15,0.,38.989));
#179072=CARTESIAN_POINT('',(30.0450834959843,52.6757649139392,39.2708017080178));
#179073=CARTESIAN_POINT('',(29.9637318773888,52.5348628867551,38.989));
#179074=CARTESIAN_POINT('',(24.9555320243585,55.2690209155614,39.2708017078546));
#179075=CARTESIAN_POINT('Origin',(5.52999282761009E-15,0.,39.2708017080178));
#179076=CARTESIAN_POINT('',(24.9555320242422,55.2690209153037,39.2708017080178));
#179077=CARTESIAN_POINT('Origin',(60.71525,0.,39.3978017080178));
#179078=CARTESIAN_POINT('',(25.0444775033954,55.4702140717964,39.3978017080178));
#179079=CARTESIAN_POINT('',(30.1555713378344,52.8659816883956,39.3978017080178));
#179080=CARTESIAN_POINT('Origin',(5.5478765747851E-15,0.,39.3978017080178));
#179081=CARTESIAN_POINT('',(30.2311753956719,52.9969317578284,39.3978017080178));
#179082=CARTESIAN_POINT('',(14.9038494342991,26.4492244485619,39.3978017080178));
#179083=CARTESIAN_POINT('',(25.1059793847708,55.6083495590299,39.3978017080178));
#179084=CARTESIAN_POINT('Origin',(5.5478765747851E-15,0.,39.3978017080178));
#179085=CARTESIAN_POINT('',(25.0446930837944,55.4706982733004,39.3978017080178));
#179086=CARTESIAN_POINT('Origin',(5.5478765747851E-15,0.,39.3978017080178));
#179087=CARTESIAN_POINT('',(25.1949317875307,55.8095395120004,39.2708017080178));
#179088=CARTESIAN_POINT('',(30.3416565763598,53.1871522508547,39.2708017081757));
#179089=CARTESIAN_POINT('Origin',(5.52999282761008E-15,0.,39.2708017080178));
#179090=CARTESIAN_POINT('',(30.4230055008174,53.3280557328682,38.9890000005756));
#179091=CARTESIAN_POINT('',(30.3416565762242,53.1871522506171,39.2708017080178));
#179092=CARTESIAN_POINT('',(30.4225123424717,53.3283370710509,38.989));
#179093=CARTESIAN_POINT('Origin',(5.49031038273072E-15,0.,38.989));
#179094=CARTESIAN_POINT('',(25.2616268796463,55.9579395562863,38.989));
#179095=CARTESIAN_POINT('Origin',(5.49031038273072E-15,0.,38.989));
#179096=CARTESIAN_POINT('',(25.2611094010728,55.9581731633343,38.9890000005754));
#179097=CARTESIAN_POINT('Origin',(5.49031038273072E-15,0.,38.989));
#179098=CARTESIAN_POINT('',(25.2611094011954,55.9581731636434,38.989));
#179099=CARTESIAN_POINT('Origin',(62.2224557307631,0.,38.989));
#179100=CARTESIAN_POINT('',(30.6598643453581,53.7394427993283,38.989));
#179101=CARTESIAN_POINT('',(15.2806508669898,27.1018636743471,38.989));
#179102=CARTESIAN_POINT('',(25.454706393409,56.3916032444848,38.989));
#179103=CARTESIAN_POINT('Origin',(5.49031038273072E-15,0.,38.989));
#179104=CARTESIAN_POINT('',(25.2618405854041,55.9584195472772,38.989));
#179105=CARTESIAN_POINT('Origin',(5.57972911860581E-15,0.,39.624));
#179106=CARTESIAN_POINT('Origin',(29.7268774036444,52.1234719996031,39.6240070731883));
#179107=CARTESIAN_POINT('Origin',(24.6957545189384,54.6869571488947,39.6240070731883));
#179108=CARTESIAN_POINT('Origin',(5.57972911860581E-15,0.,39.624));
#179109=CARTESIAN_POINT('Origin',(30.6789000092884,53.7724806104368,39.5552135207961));
#179110=CARTESIAN_POINT('Origin',(25.4702454952004,56.4264221855602,39.5552117598815));
#179111=CARTESIAN_POINT('Origin',(5.51210908043506E-15,0.,39.1438017080178));
#179112=CARTESIAN_POINT('Origin',(30.2391374209353,53.0106482050728,39.1711625381366));
#179113=CARTESIAN_POINT('Origin',(25.112358217853,55.6227672661399,39.1712173702603));
#179114=CARTESIAN_POINT('Origin',(5.51210908043507E-15,0.,39.1438017080178));
#179115=CARTESIAN_POINT('Origin',(30.1476490842099,52.8523506794944,39.1712175859362));
#179116=CARTESIAN_POINT('Origin',(25.038068340494,55.4557066902169,39.171162752677));
#179117=CARTESIAN_POINT('Origin',(60.4792282238308,0.,38.989));
#179118=CARTESIAN_POINT('',(18.8441205405526,56.9687879773464,38.989));
#179119=CARTESIAN_POINT('',(24.1156489724283,54.9452378026826,38.989));
#179120=CARTESIAN_POINT('Origin',(5.49031038273072E-15,0.,38.989));
#179121=CARTESIAN_POINT('',(24.3087286055926,55.3789017591236,38.989));
#179122=CARTESIAN_POINT('',(9.71531210235053,22.6015516358801,38.989));
#179123=CARTESIAN_POINT('',(24.3081989337721,55.3791342586255,38.9889999995776));
#179124=CARTESIAN_POINT('Origin',(5.49031038273072E-15,0.,38.989));
#179125=CARTESIAN_POINT('',(18.9913614316851,57.4200769554259,38.9889999997818));
#179126=CARTESIAN_POINT('Origin',(5.49031038273072E-15,0.,38.989));
#179127=CARTESIAN_POINT('',(18.9908122363906,57.4202585945858,38.989));
#179128=CARTESIAN_POINT('Origin',(5.49031038273072E-15,0.,38.989));
#179129=CARTESIAN_POINT('',(18.8442866674268,56.9692992632924,38.989));
#179130=CARTESIAN_POINT('Origin',(5.49031038273072E-15,0.,38.989));
#179131=CARTESIAN_POINT('',(24.374376627022,55.527767968768,39.2708017080178));
#179132=CARTESIAN_POINT('',(24.308198933478,55.3791342579555,38.989));
#179133=CARTESIAN_POINT('',(19.0416371861772,57.5748148486258,39.2708017078546));
#179134=CARTESIAN_POINT('Origin',(5.52999282761009E-15,0.,39.2708017080178));
#179135=CARTESIAN_POINT('',(19.0416371860884,57.5748148483574,39.2708017080178));
#179136=CARTESIAN_POINT('Origin',(60.71525,0.,39.3978017080178));
#179137=CARTESIAN_POINT('',(19.1090650011322,57.7842031819381,39.3978017080178));
#179138=CARTESIAN_POINT('',(24.4643761377923,55.7284918401495,39.3978017080178));
#179139=CARTESIAN_POINT('Origin',(5.5478765747851E-15,0.,39.3978017080178));
#179140=CARTESIAN_POINT('',(24.5258780191677,55.866627327383,39.3978017080178));
#179141=CARTESIAN_POINT('',(9.75435829333414,22.6892508167102,39.3978017080178));
#179142=CARTESIAN_POINT('',(19.1557908785631,57.9280106456674,39.3978017080178));
#179143=CARTESIAN_POINT('Origin',(5.5478765747851E-15,0.,39.3978017080178));
#179144=CARTESIAN_POINT('',(19.1092287877201,57.7847072652234,39.3978017080178));
#179145=CARTESIAN_POINT('Origin',(5.5478765747851E-15,0.,39.3978017080178));
#179146=CARTESIAN_POINT('',(19.2232259141446,58.1373965169891,39.2708017080178));
#179147=CARTESIAN_POINT('',(24.6158705165699,56.0673542006827,39.2708017081757));
#179148=CARTESIAN_POINT('Origin',(5.52999282761008E-15,0.,39.2708017080178));
#179149=CARTESIAN_POINT('',(24.6820453786638,56.2159890767408,38.9890000005756));
#179150=CARTESIAN_POINT('',(24.61587051646,56.0673542004323,39.2708017080178));
#179151=CARTESIAN_POINT('',(24.6815255140433,56.2162173246395,38.989));
#179152=CARTESIAN_POINT('Origin',(5.49031038273072E-15,0.,38.989));
#179153=CARTESIAN_POINT('',(19.2740436149891,58.2919551457914,38.989));
#179154=CARTESIAN_POINT('Origin',(5.49031038273072E-15,0.,38.989));
#179155=CARTESIAN_POINT('',(19.2735045526316,58.2921333818755,38.9890000005754));
#179156=CARTESIAN_POINT('Origin',(5.49031038273072E-15,0.,38.989));
#179157=CARTESIAN_POINT('',(19.2735045527213,58.2921333821957,38.989));
#179158=CARTESIAN_POINT('Origin',(62.2224557307631,0.,38.989));
#179159=CARTESIAN_POINT('',(24.8746050278059,56.6498810128379,38.989));
#179160=CARTESIAN_POINT('',(10.0037024164492,23.2492868865834,38.989));
#179161=CARTESIAN_POINT('',(19.4207352200707,58.743425483793,38.989));
#179162=CARTESIAN_POINT('Origin',(5.49031038273072E-15,0.,38.989));
#179163=CARTESIAN_POINT('',(19.2742059773237,58.2924548456759,38.989));
#179164=CARTESIAN_POINT('Origin',(5.57972911860581E-15,0.,39.624));
#179165=CARTESIAN_POINT('Origin',(24.1156440305597,54.9452389789693,39.6240070731883));
#179166=CARTESIAN_POINT('Origin',(18.8441250001663,56.9687855447422,39.6240070731883));
#179167=CARTESIAN_POINT('Origin',(5.57972911860581E-15,0.,39.624));
#179168=CARTESIAN_POINT('Origin',(24.8900830207503,56.6847276080573,39.5552135207989));
#179169=CARTESIAN_POINT('Origin',(19.4325496266321,58.7796779614968,39.5552117598826));
#179170=CARTESIAN_POINT('Origin',(5.51210908043506E-15,0.,39.1438017080178));
#179171=CARTESIAN_POINT('Origin',(24.5323626684704,55.8811008927563,39.1711625381296));
#179172=CARTESIAN_POINT('Origin',(19.1606277069624,57.9430161406894,39.1712173702622));
#179173=CARTESIAN_POINT('Origin',(5.51210908043507E-15,0.,39.1438017080178));
#179174=CARTESIAN_POINT('Origin',(24.4579221115139,55.7141074023442,39.1712175859374));
#179175=CARTESIAN_POINT('Origin',(19.1042073826023,57.769105333365,39.171162752673));
#179176=CARTESIAN_POINT('Origin',(60.4792282238308,0.,38.989));
#179177=CARTESIAN_POINT('',(12.7860306150458,58.6264539577982,38.989));
#179178=CARTESIAN_POINT('',(18.2401996527051,57.1650137687745,38.989));
#179179=CARTESIAN_POINT('Origin',(5.49031038273072E-15,0.,38.989));
#179180=CARTESIAN_POINT('',(18.3868913484954,57.6164843860301,38.989));
#179181=CARTESIAN_POINT('',(5.47329194811204,17.8725121057138,38.989));
#179182=CARTESIAN_POINT('',(18.3863402754571,57.6166602460946,38.9889999995772));
#179183=CARTESIAN_POINT('Origin',(5.49031038273072E-15,0.,38.989));
#179184=CARTESIAN_POINT('',(12.8852923618023,59.0906615917169,38.9889999997818));
#179185=CARTESIAN_POINT('Origin',(5.49031038273072E-15,0.,38.989));
#179186=CARTESIAN_POINT('',(12.8847271885949,59.0907848292983,38.989));
#179187=CARTESIAN_POINT('Origin',(5.49031038273072E-15,0.,38.989));
#179188=CARTESIAN_POINT('',(12.7861423879254,58.6269798078531,38.989));
#179189=CARTESIAN_POINT('Origin',(5.49031038273072E-15,0.,38.989));
#179190=CARTESIAN_POINT('',(18.4366189870679,57.7713971777985,39.2708017080178));
#179191=CARTESIAN_POINT('',(18.3863402752344,57.6166602453969,38.989));
#179192=CARTESIAN_POINT('',(12.9191181862654,59.249807061904,39.2708017078546));
#179193=CARTESIAN_POINT('Origin',(5.52999282761009E-15,0.,39.2708017080178));
#179194=CARTESIAN_POINT('',(12.9191181862052,59.2498070616278,39.2708017080178));
#179195=CARTESIAN_POINT('Origin',(60.71525,0.,39.3978017080178));
#179196=CARTESIAN_POINT('',(12.9642895838877,59.4650964698965,39.3978017080178));
#179197=CARTESIAN_POINT('',(18.5051441132848,57.9804289733662,39.3978017080178));
#179198=CARTESIAN_POINT('Origin',(5.5478765747851E-15,0.,39.3978017080178));
#179199=CARTESIAN_POINT('',(18.5518699907157,58.1242364370955,39.3978017080178));
#179200=CARTESIAN_POINT('',(5.49583002221492,17.9418771653399,39.3978017080178));
#179201=CARTESIAN_POINT('',(12.995727518883,59.6130003254554,39.3978017080178));
#179202=CARTESIAN_POINT('Origin',(5.5478765747851E-15,0.,39.3978017080178));
#179203=CARTESIAN_POINT('',(12.9643997821844,59.4656149121212,39.3978017080178));
#179204=CARTESIAN_POINT('Origin',(5.5478765747851E-15,0.,39.3978017080178));
#179205=CARTESIAN_POINT('',(13.0409063549245,59.8282880397053,39.2708017080178));
#179206=CARTESIAN_POINT('',(18.6203878281985,58.3332704850399,39.2708017081757));
#179207=CARTESIAN_POINT('Origin',(5.52999282761008E-15,0.,39.2708017080178));
#179208=CARTESIAN_POINT('',(18.6706636022915,58.4880082803367,38.9890000005756));
#179209=CARTESIAN_POINT('',(18.6203878281154,58.3332704847794,39.2708017080178));
#179210=CARTESIAN_POINT('',(18.6701227271417,58.4881809372196,38.989));
#179211=CARTESIAN_POINT('Origin',(5.49031038273072E-15,0.,38.989));
#179212=CARTESIAN_POINT('',(13.0752898951332,59.9873118763434,38.989));
#179213=CARTESIAN_POINT('Origin',(5.49031038273072E-15,0.,38.989));
#179214=CARTESIAN_POINT('',(13.0747351550717,59.9874327886717,38.9890000005754));
#179215=CARTESIAN_POINT('Origin',(5.49031038273072E-15,0.,38.989));
#179216=CARTESIAN_POINT('',(13.0747351551274,59.9874327889996,38.989));
#179217=CARTESIAN_POINT('Origin',(62.2224557307631,0.,38.989));
#179218=CARTESIAN_POINT('',(18.8168143322233,58.9396512752211,38.989));
#179219=CARTESIAN_POINT('',(5.63975536249314,18.3848338156965,38.989));
#179220=CARTESIAN_POINT('',(13.1739864076113,60.4516424606487,38.989));
#179221=CARTESIAN_POINT('Origin',(5.49031038273072E-15,0.,38.989));
#179222=CARTESIAN_POINT('',(13.075399135169,59.9878258103049,38.989));
#179223=CARTESIAN_POINT('Origin',(5.57972911860581E-15,0.,39.624));
#179224=CARTESIAN_POINT('Origin',(18.2401946149532,57.1650144220515,39.6240070731883));
#179225=CARTESIAN_POINT('Origin',(12.7860353045056,58.6264520046766,39.6240070731883));
#179226=CARTESIAN_POINT('Origin',(5.57972911860581E-15,0.,39.624));
#179227=CARTESIAN_POINT('Origin',(18.8285650740585,58.9759248679615,39.5552135207994));
#179228=CARTESIAN_POINT('Origin',(13.1819466778345,60.4889312852505,39.555211759879));
#179229=CARTESIAN_POINT('Origin',(5.51210908043506E-15,0.,39.1438017080178));
#179230=CARTESIAN_POINT('Origin',(18.5568062168849,58.1393085451912,39.1711625381331));
#179231=CARTESIAN_POINT('Origin',(12.9989693492948,59.6284292050442,39.1712173702602));
#179232=CARTESIAN_POINT('Origin',(5.51210908043507E-15,0.,39.1438017080178));
#179233=CARTESIAN_POINT('Origin',(18.5002290260147,57.9654487055675,39.1712175859381));
#179234=CARTESIAN_POINT('Origin',(12.9610367308112,59.4495735695181,39.1711627526717));
#179235=CARTESIAN_POINT('Origin',(60.4792282238308,0.,38.989));
#179236=CARTESIAN_POINT('',(6.58785426247156,59.6417962403142,38.989));
#179237=CARTESIAN_POINT('',(12.1649068885798,58.7584778814675,38.989));
#179238=CARTESIAN_POINT('Origin',(5.49031038273072E-15,0.,38.989));
#179239=CARTESIAN_POINT('',(12.2636034620796,59.2228087529787,38.989));
#179240=CARTESIAN_POINT('',(2.30379013587727,12.3655710936233,38.989));
#179241=CARTESIAN_POINT('',(12.2630370254948,59.2229260468454,38.9889999995773));
#179242=CARTESIAN_POINT('Origin',(5.49031038273072E-15,0.,38.989));
#179243=CARTESIAN_POINT('',(6.63804933238279,60.1138365740932,38.9889999997818));
#179244=CARTESIAN_POINT('Origin',(5.49031038273072E-15,0.,38.989));
#179245=CARTESIAN_POINT('',(6.63747437341838,60.1139000598793,38.989));
#179246=CARTESIAN_POINT('Origin',(5.49031038273072E-15,0.,38.989));
#179247=CARTESIAN_POINT('',(6.58791045674951,59.6423308931549,38.989));
#179248=CARTESIAN_POINT('Origin',(5.49031038273072E-15,0.,38.989));
#179249=CARTESIAN_POINT('',(12.296865891381,59.3820708699069,39.2708017080178));
#179250=CARTESIAN_POINT('',(12.2630370253463,59.2229260461284,38.989));
#179251=CARTESIAN_POINT('',(6.65505462400558,60.2756459901928,39.2708017078546));
#179252=CARTESIAN_POINT('Origin',(5.52999282761009E-15,0.,39.2708017080178));
#179253=CARTESIAN_POINT('',(6.65505462397456,60.2756459899118,39.2708017080178));
#179254=CARTESIAN_POINT('Origin',(60.71525,0.,39.3978017080178));
#179255=CARTESIAN_POINT('',(6.67747469701007,60.4944777170593,39.3978017080178));
#179256=CARTESIAN_POINT('',(12.3431658574217,59.5971203935658,39.3978017080178));
#179257=CARTESIAN_POINT('Origin',(5.5478765747851E-15,0.,39.3978017080178));
#179258=CARTESIAN_POINT('',(12.3746037924171,59.7450242491246,39.3978017080178));
#179259=CARTESIAN_POINT('',(2.31399271319981,12.4135704460892,39.3978017080178));
#179260=CARTESIAN_POINT('',(6.69328024897516,60.6448574988554,39.3978017080178));
#179261=CARTESIAN_POINT('Origin',(5.5478765747851E-15,0.,39.3978017080178));
#179262=CARTESIAN_POINT('',(6.67753009965994,60.4950048380619,39.3978017080178));
#179263=CARTESIAN_POINT('Origin',(5.5478765747851E-15,0.,39.3978017080178));
#179264=CARTESIAN_POINT('',(6.71570789669471,60.8636883187844,39.2708017080178));
#179265=CARTESIAN_POINT('',(12.4208962742148,59.9600752509413,39.2708017081757));
#179266=CARTESIAN_POINT('Origin',(5.52999282761008E-15,0.,39.2708017080178));
#179267=CARTESIAN_POINT('',(12.454722128405,60.1192206258105,38.9890000005756));
#179268=CARTESIAN_POINT('',(12.4208962741593,59.9600752506736,39.2708017080178));
#179269=CARTESIAN_POINT('',(12.4541661686672,60.1193358000127,38.989));
#179270=CARTESIAN_POINT('Origin',(5.49031038273072E-15,0.,38.989));
#179271=CARTESIAN_POINT('',(6.7332805630058,61.0254350648261,38.989));
#179272=CARTESIAN_POINT('Origin',(5.49031038273072E-15,0.,38.989));
#179273=CARTESIAN_POINT('',(6.73271622308859,61.0254973286579,38.9890000005754));
#179274=CARTESIAN_POINT('Origin',(5.49031038273072E-15,0.,38.989));
#179275=CARTESIAN_POINT('',(6.7327162231097,61.0254973289898,38.989));
#179276=CARTESIAN_POINT('Origin',(62.2224557307631,0.,38.989));
#179277=CARTESIAN_POINT('',(12.5528626811454,60.583666384318,38.989));
#179278=CARTESIAN_POINT('',(2.3791451040456,12.7200883457668,38.989));
#179279=CARTESIAN_POINT('',(6.78290064323623,61.4975385923861,38.989));
#179280=CARTESIAN_POINT('Origin',(5.49031038273072E-15,0.,38.989));
#179281=CARTESIAN_POINT('',(6.73333548388602,61.0259576020967,38.989));
#179282=CARTESIAN_POINT('Origin',(5.57972911860581E-15,0.,39.624));
#179283=CARTESIAN_POINT('Origin',(12.1649018101392,58.7584780045773,39.6240070731883));
#179284=CARTESIAN_POINT('Origin',(6.58785913039885,59.6417947880741,39.6240070731883));
#179285=CARTESIAN_POINT('Origin',(5.57972911860581E-15,0.,39.624));
#179286=CARTESIAN_POINT('Origin',(12.5607574282786,60.6209695535089,39.5552135207989));
#179287=CARTESIAN_POINT('Origin',(6.78691956273318,61.5354552197195,39.5552117598775));
#179288=CARTESIAN_POINT('Origin',(5.51210908043506E-15,0.,39.1438017080178));
#179289=CARTESIAN_POINT('Origin',(12.3779375131252,59.7605297667703,39.1711625381316));
#179290=CARTESIAN_POINT('Origin',(6.69489156322753,60.6605407209802,39.1712173702623));
#179291=CARTESIAN_POINT('Origin',(5.51210908043507E-15,0.,39.1438017080178));
#179292=CARTESIAN_POINT('Origin',(12.3398435598877,59.5817084227229,39.171217585937));
#179293=CARTESIAN_POINT('Origin',(6.67586224832399,60.4786998370191,39.1711627526734));
#179294=CARTESIAN_POINT('Origin',(60.4792282238308,0.,38.989));
#179295=CARTESIAN_POINT('',(0.317500000000634,60.0036905223731,38.989));
#179296=CARTESIAN_POINT('',(5.95633285891271,59.7081718144892,38.989));
#179297=CARTESIAN_POINT('Origin',(5.49031038273072E-15,0.,38.989));
#179298=CARTESIAN_POINT('',(6.00595296980932,60.1802756340602,38.989));
#179299=CARTESIAN_POINT('',(0.34504741944992,6.32035708677299,38.989));
#179300=CARTESIAN_POINT('',(6.00537737567573,60.1803330766332,38.9889999995772));
#179301=CARTESIAN_POINT('Origin',(5.49031038273072E-15,0.,38.989));
#179302=CARTESIAN_POINT('',(0.31807844537663,60.4783917833346,38.9889999997818));
#179303=CARTESIAN_POINT('Origin',(5.49031038273072E-15,0.,38.989));
#179304=CARTESIAN_POINT('',(0.317500000025924,60.478394821762,38.989));
#179305=CARTESIAN_POINT('Origin',(5.49031038273072E-15,0.,38.989));
#179306=CARTESIAN_POINT('',(0.317500000000634,60.004228120231,38.989));
#179307=CARTESIAN_POINT('Origin',(5.49031038273072E-15,0.,38.989));
#179308=CARTESIAN_POINT('',(6.02238575970337,60.3421421670675,39.2708017080178));
#179309=CARTESIAN_POINT('',(6.00537737560301,60.1803330759045,38.989));
#179310=CARTESIAN_POINT('',(0.318076890625489,60.6410923275232,39.2708017078546));
#179311=CARTESIAN_POINT('Origin',(5.52999282761009E-15,0.,39.2708017080178));
#179312=CARTESIAN_POINT('',(0.318076890624007,60.6410923272405,39.2708017080178));
#179313=CARTESIAN_POINT('Origin',(60.71525,0.,39.3978017080178));
#179314=CARTESIAN_POINT('',(0.317500000000643,60.8610688070707,39.3978017080178));
#179315=CARTESIAN_POINT('',(6.04595329345123,60.5608532912343,39.3978017080178));
#179316=CARTESIAN_POINT('Origin',(5.5478765747851E-15,0.,39.3978017080178));
#179317=CARTESIAN_POINT('',(6.06175884541631,60.7112330730303,39.3978017080178));
#179318=CARTESIAN_POINT('',(0.347626240494121,6.34489293004957,39.3978017080178));
#179319=CARTESIAN_POINT('',(0.317500000000645,61.0122769227456,39.3978017080178));
#179320=CARTESIAN_POINT('Origin',(5.5478765747851E-15,0.,39.3978017080178));
#179321=CARTESIAN_POINT('',(0.317500000000643,60.8615988316031,39.3978017080178));
#179322=CARTESIAN_POINT('Origin',(5.5478765747851E-15,0.,39.3978017080178));
#179323=CARTESIAN_POINT('',(0.316930737396561,61.2322532920972,39.2708017080178));
#179324=CARTESIAN_POINT('',(6.08531878141099,60.9299448849411,39.2708017081757));
#179325=CARTESIAN_POINT('Origin',(5.52999282761008E-15,0.,39.2708017080178));
#179326=CARTESIAN_POINT('',(6.10232411256148,61.0917542093523,38.9890000005756));
#179327=CARTESIAN_POINT('',(6.08531878138382,60.929944884669,39.2708017080178));
#179328=CARTESIAN_POINT('',(6.10175915944695,61.0918106390011,38.989));
#179329=CARTESIAN_POINT('Origin',(5.49031038273072E-15,0.,38.989));
#179330=CARTESIAN_POINT('',(0.317500000000649,61.3949508163454,38.989));
#179331=CARTESIAN_POINT('Origin',(5.49031038273072E-15,0.,38.989));
#179332=CARTESIAN_POINT('',(0.316932243253905,61.394953749505,38.9890000005754));
#179333=CARTESIAN_POINT('Origin',(5.49031038273072E-15,0.,38.989));
#179334=CARTESIAN_POINT('',(0.316932243240209,61.3949537498373,38.989));
#179335=CARTESIAN_POINT('Origin',(62.2224557307631,0.,38.989));
#179336=CARTESIAN_POINT('',(6.15137923967738,61.5639141665611,38.989));
#179337=CARTESIAN_POINT('',(0.364094271196581,6.50157577599617,38.989));
#179338=CARTESIAN_POINT('',(0.317500000000654,61.8696548221181,38.989));
#179339=CARTESIAN_POINT('Origin',(5.49031038273072E-15,0.,38.989));
#179340=CARTESIAN_POINT('',(0.317500000000649,61.3954762318973,38.989));
#179341=CARTESIAN_POINT('Origin',(5.57972911860581E-15,0.,39.624));
#179342=CARTESIAN_POINT('Origin',(5.95632779542376,59.7081714060829,39.6240070731883));
#179343=CARTESIAN_POINT('Origin',(0.317504993061332,60.0036895869254,39.6240070731883));
#179344=CARTESIAN_POINT('Origin',(5.57972911860581E-15,0.,39.624));
#179345=CARTESIAN_POINT('Origin',(6.15533149561049,61.6018382108738,39.5552135207989));
#179346=CARTESIAN_POINT('Origin',(0.31753353664925,61.907783829676,39.5552117598823));
#179347=CARTESIAN_POINT('Origin',(5.51210908043506E-15,0.,39.1438017080178));
#179348=CARTESIAN_POINT('Origin',(6.06345353572217,60.7270021185324,39.1711625381353));
#179349=CARTESIAN_POINT('Origin',(0.317463144197165,61.0280426587396,39.1712173702592));
#179350=CARTESIAN_POINT('Origin',(5.51210908043507E-15,0.,39.1438017080178));
#179351=CARTESIAN_POINT('Origin',(6.04426018543824,60.545178474123,39.1712175859392));
#179352=CARTESIAN_POINT('Origin',(0.317545622031397,60.845208813123,39.1711627526774));
#179353=CARTESIAN_POINT('Origin',(60.4792282238308,0.,38.989));
#179354=CARTESIAN_POINT('',(-5.9563328589115,59.7081718144893,38.989));
#179355=CARTESIAN_POINT('',(-0.317499999999366,60.0036905223731,38.989));
#179356=CARTESIAN_POINT('Origin',(5.49031038273072E-15,0.,38.989));
#179357=CARTESIAN_POINT('',(-0.317500000024619,60.4783948217626,38.989));
#179358=CARTESIAN_POINT('',(-0.317499999999991,6.36811926168668E-13,38.989));
#179359=CARTESIAN_POINT('',(-0.318078445377217,60.4783917836887,38.9889999995774));
#179360=CARTESIAN_POINT('Origin',(5.49031038273072E-15,0.,38.989));
#179361=CARTESIAN_POINT('',(-6.00537737563932,60.1803330762807,38.9889999997818));
#179362=CARTESIAN_POINT('Origin',(5.49031038273072E-15,0.,38.989));
#179363=CARTESIAN_POINT('',(-6.00595296980802,60.1802756340597,38.989));
#179364=CARTESIAN_POINT('Origin',(5.49031038273072E-15,0.,38.989));
#179365=CARTESIAN_POINT('',(-5.95638905318945,59.7087064673299,38.989));
#179366=CARTESIAN_POINT('Origin',(5.49031038273072E-15,0.,38.989));
#179367=CARTESIAN_POINT('',(-0.318076890622726,60.6410923272405,39.2708017080178));
#179368=CARTESIAN_POINT('',(-0.318078445373366,60.4783917829566,38.989));
#179369=CARTESIAN_POINT('',(-6.02238575973022,60.3421421673489,39.2708017078546));
#179370=CARTESIAN_POINT('Origin',(5.52999282761009E-15,0.,39.2708017080178));
#179371=CARTESIAN_POINT('',(-6.02238575970214,60.3421421670676,39.2708017080178));
#179372=CARTESIAN_POINT('Origin',(60.71525,0.,39.3978017080178));
#179373=CARTESIAN_POINT('',(-6.04595329344999,60.5608532912344,39.3978017080178));
#179374=CARTESIAN_POINT('',(-0.317499999999354,60.8610688070707,39.3978017080178));
#179375=CARTESIAN_POINT('Origin',(5.5478765747851E-15,0.,39.3978017080178));
#179376=CARTESIAN_POINT('',(-0.317499999999355,61.0122769227456,39.3978017080178));
#179377=CARTESIAN_POINT('',(-0.317499999999991,6.39284123049835E-13,39.3978017080178));
#179378=CARTESIAN_POINT('',(-6.06175884541508,60.7112330730304,39.3978017080178));
#179379=CARTESIAN_POINT('Origin',(5.5478765747851E-15,0.,39.3978017080178));
#179380=CARTESIAN_POINT('',(-6.04600869609986,60.561380412237,39.3978017080178));
#179381=CARTESIAN_POINT('Origin',(5.5478765747851E-15,0.,39.3978017080178));
#179382=CARTESIAN_POINT('',(-6.08531878138258,60.9299448846691,39.2708017080178));
#179383=CARTESIAN_POINT('',(-0.316930737396683,61.2322532923707,39.2708017081757));
#179384=CARTESIAN_POINT('Origin',(5.52999282761008E-15,0.,39.2708017080178));
#179385=CARTESIAN_POINT('',(-0.316932243252611,61.3949537495049,38.9890000005756));
#179386=CARTESIAN_POINT('',(-0.316930737395267,61.2322532920972,39.2708017080178));
#179387=CARTESIAN_POINT('',(-0.317499999999355,61.3949508163454,38.989));
#179388=CARTESIAN_POINT('Origin',(5.49031038273072E-15,0.,38.989));
#179389=CARTESIAN_POINT('',(-6.10175915944571,61.0918106390012,38.989));
#179390=CARTESIAN_POINT('Origin',(5.49031038273072E-15,0.,38.989));
#179391=CARTESIAN_POINT('',(-6.10232411256026,61.0917542093525,38.9890000005754));
#179392=CARTESIAN_POINT('Origin',(5.49031038273072E-15,0.,38.989));
#179393=CARTESIAN_POINT('',(-6.10232411260861,61.0917542096815,38.989));
#179394=CARTESIAN_POINT('Origin',(62.2224557307631,0.,38.989));
#179395=CARTESIAN_POINT('',(-0.317499999999346,61.8696548221181,38.989));
#179396=CARTESIAN_POINT('',(-0.317499999999998,6.55071265098105E-13,38.989));
#179397=CARTESIAN_POINT('',(-6.15137923967613,61.5639141665612,38.989));
#179398=CARTESIAN_POINT('Origin',(5.49031038273072E-15,0.,38.989));
#179399=CARTESIAN_POINT('',(-6.10181408032593,61.0923331762718,38.989));
#179400=CARTESIAN_POINT('Origin',(5.57972911860581E-15,0.,39.624));
#179401=CARTESIAN_POINT('Origin',(-0.317504993059919,60.0036895869254,39.6240070731883));
#179402=CARTESIAN_POINT('Origin',(-5.95632779542241,59.7081714060831,39.6240070731883));
#179403=CARTESIAN_POINT('Origin',(5.57972911860581E-15,0.,39.624));
#179404=CARTESIAN_POINT('Origin',(-0.317533537010864,61.9077842377891,39.5552135207949));
#179405=CARTESIAN_POINT('Origin',(-6.15533145331129,61.6018378049591,39.5552117598854));
#179406=CARTESIAN_POINT('Origin',(5.51210908043506E-15,0.,39.1438017080178));
#179407=CARTESIAN_POINT('Origin',(-0.317462907477851,61.0281367271385,39.1711625381323));
#179408=CARTESIAN_POINT('Origin',(-6.06344346747441,60.7269085901931,39.1712173702603));
#179409=CARTESIAN_POINT('Origin',(5.51210908043507E-15,0.,39.1438017080178));
#179410=CARTESIAN_POINT('Origin',(-0.317545368444817,60.8453028802704,39.1712175859369));
#179411=CARTESIAN_POINT('Origin',(-6.04425010054706,60.5450849487948,39.1711627526752));
#179412=CARTESIAN_POINT('Origin',(60.4792282238308,0.,38.989));
#179413=CARTESIAN_POINT('',(-12.1649068885786,58.7584778814678,38.989));
#179414=CARTESIAN_POINT('',(-6.58785426247035,59.6417962403143,38.989));
#179415=CARTESIAN_POINT('Origin',(5.49031038273072E-15,0.,38.989));
#179416=CARTESIAN_POINT('',(-6.63747437341721,60.1139000598801,38.989));
#179417=CARTESIAN_POINT('',(0.345047419449671,-6.32035708677179,38.989));
#179418=CARTESIAN_POINT('',(-6.6380493324205,60.1138365744458,38.988999999577));
#179419=CARTESIAN_POINT('Origin',(5.49031038273072E-15,0.,38.989));
#179420=CARTESIAN_POINT('',(-12.2630370254217,59.2229260464988,38.9889999997818));
#179421=CARTESIAN_POINT('Origin',(5.49031038273072E-15,0.,38.989));
#179422=CARTESIAN_POINT('',(-12.2636034620782,59.2228087529783,38.989));
#179423=CARTESIAN_POINT('Origin',(5.49031038273072E-15,0.,38.989));
#179424=CARTESIAN_POINT('',(-12.1650186614582,58.7590037315227,38.989));
#179425=CARTESIAN_POINT('Origin',(5.49031038273072E-15,0.,38.989));
#179426=CARTESIAN_POINT('',(-6.65505462397334,60.275645989912,39.2708017080178));
#179427=CARTESIAN_POINT('',(-6.63804933234009,60.1138365737176,38.989));
#179428=CARTESIAN_POINT('',(-12.296865891437,59.3820708701841,39.2708017078546));
#179429=CARTESIAN_POINT('Origin',(5.52999282761009E-15,0.,39.2708017080178));
#179430=CARTESIAN_POINT('',(-12.2968658913797,59.3820708699072,39.2708017080178));
#179431=CARTESIAN_POINT('Origin',(60.71525,0.,39.3978017080178));
#179432=CARTESIAN_POINT('',(-12.3431658574205,59.597120393566,39.3978017080178));
#179433=CARTESIAN_POINT('',(-6.67747469700884,60.4944777170594,39.3978017080178));
#179434=CARTESIAN_POINT('Origin',(5.5478765747851E-15,0.,39.3978017080178));
#179435=CARTESIAN_POINT('',(-6.69328024897394,60.6448574988555,39.3978017080178));
#179436=CARTESIAN_POINT('',(0.347626240493851,-6.34489293004837,39.3978017080178));
#179437=CARTESIAN_POINT('',(-12.3746037924158,59.7450242491249,39.3978017080178));
#179438=CARTESIAN_POINT('Origin',(5.5478765747851E-15,0.,39.3978017080178));
#179439=CARTESIAN_POINT('',(-12.3432760557172,59.5976388357908,39.3978017080178));
#179440=CARTESIAN_POINT('Origin',(5.5478765747851E-15,0.,39.3978017080178));
#179441=CARTESIAN_POINT('',(-12.420896274158,59.9600752506738,39.2708017080178));
#179442=CARTESIAN_POINT('',(-6.71570789672347,60.8636883190564,39.2708017081757));
#179443=CARTESIAN_POINT('Origin',(5.52999282761008E-15,0.,39.2708017080178));
#179444=CARTESIAN_POINT('',(-6.73271622308735,61.0254973286579,38.9890000005756));
#179445=CARTESIAN_POINT('',(-6.71570789669348,60.8636883187845,39.2708017080178));
#179446=CARTESIAN_POINT('',(-6.73328056300457,61.0254350648263,38.989));
#179447=CARTESIAN_POINT('Origin',(5.49031038273072E-15,0.,38.989));
#179448=CARTESIAN_POINT('',(-12.4541661686659,60.119335800013,38.989));
#179449=CARTESIAN_POINT('Origin',(5.49031038273072E-15,0.,38.989));
#179450=CARTESIAN_POINT('',(-12.4547221284037,60.1192206258109,38.9890000005754));
#179451=CARTESIAN_POINT('Origin',(5.49031038273072E-15,0.,38.989));
#179452=CARTESIAN_POINT('',(-12.4547221284862,60.119220626133,38.989));
#179453=CARTESIAN_POINT('Origin',(62.2224557307631,0.,38.989));
#179454=CARTESIAN_POINT('',(-6.78290064323498,61.4975385923863,38.989));
#179455=CARTESIAN_POINT('',(0.364094271196325,-6.50157577599494,38.989));
#179456=CARTESIAN_POINT('',(-12.5528626811441,60.5836663843183,38.989));
#179457=CARTESIAN_POINT('Origin',(5.49031038273072E-15,0.,38.989));
#179458=CARTESIAN_POINT('',(-12.4542754087017,60.1198497339745,38.989));
#179459=CARTESIAN_POINT('Origin',(5.57972911860581E-15,0.,39.624));
#179460=CARTESIAN_POINT('Origin',(-6.58785913039747,59.6417947880742,39.6240070731883));
#179461=CARTESIAN_POINT('Origin',(-12.1649018101377,58.7584780045776,39.6240070731883));
#179462=CARTESIAN_POINT('Origin',(5.57972911860581E-15,0.,39.624));
#179463=CARTESIAN_POINT('Origin',(-6.78691960575238,61.5354556255527,39.5552135208018));
#179464=CARTESIAN_POINT('Origin',(-12.5607573437817,60.620969154241,39.5552117598825));
#179465=CARTESIAN_POINT('Origin',(5.51210908043506E-15,0.,39.1438017080178));
#179466=CARTESIAN_POINT('Origin',(-6.69490116062997,60.6606342988039,39.1711625381309));
#179467=CARTESIAN_POINT('Origin',(-12.3779177236594,59.7604378032104,39.1712173702625));
#179468=CARTESIAN_POINT('Origin',(5.51210908043507E-15,0.,39.1438017080178));
#179469=CARTESIAN_POINT('Origin',(-6.67587182882098,60.4787934153615,39.1712175859378));
#179470=CARTESIAN_POINT('Origin',(-12.3398237541834,59.5816164638937,39.1711627526742));
#179471=CARTESIAN_POINT('Origin',(60.4792282238308,0.,38.989));
#179472=CARTESIAN_POINT('',(-18.240199652704,57.1650137687749,38.989));
#179473=CARTESIAN_POINT('',(-12.7860306150445,58.6264539577985,38.989));
#179474=CARTESIAN_POINT('Origin',(5.49031038273072E-15,0.,38.989));
#179475=CARTESIAN_POINT('',(-12.8847271885938,59.0907848292992,38.989));
#179476=CARTESIAN_POINT('',(2.30379013587678,-12.3655710936221,38.989));
#179477=CARTESIAN_POINT('',(-12.8852923618764,59.0906615920626,38.9889999995776));
#179478=CARTESIAN_POINT('Origin',(5.49031038273072E-15,0.,38.989));
#179479=CARTESIAN_POINT('',(-18.3863402753482,57.6166602457574,38.9889999997818));
#179480=CARTESIAN_POINT('Origin',(5.49031038273072E-15,0.,38.989));
#179481=CARTESIAN_POINT('',(-18.386891348494,57.6164843860299,38.989));
#179482=CARTESIAN_POINT('Origin',(5.49031038273072E-15,0.,38.989));
#179483=CARTESIAN_POINT('',(-18.2403657795782,57.1655250547208,38.989));
#179484=CARTESIAN_POINT('Origin',(5.49031038273072E-15,0.,38.989));
#179485=CARTESIAN_POINT('',(-12.9191181862039,59.2498070616281,39.2708017080178));
#179486=CARTESIAN_POINT('',(-12.8852923617205,59.0906615913479,38.989));
#179487=CARTESIAN_POINT('',(-18.4366189871527,57.7713971780682,39.2708017078546));
#179488=CARTESIAN_POINT('Origin',(5.52999282761009E-15,0.,39.2708017080178));
#179489=CARTESIAN_POINT('',(-18.4366189870667,57.7713971777989,39.2708017080178));
#179490=CARTESIAN_POINT('Origin',(60.71525,0.,39.3978017080178));
#179491=CARTESIAN_POINT('',(-18.5051441132836,57.9804289733665,39.3978017080178));
#179492=CARTESIAN_POINT('',(-12.9642895838864,59.4650964698968,39.3978017080178));
#179493=CARTESIAN_POINT('Origin',(5.5478765747851E-15,0.,39.3978017080178));
#179494=CARTESIAN_POINT('',(-12.9957275188818,59.6130003254556,39.3978017080178));
#179495=CARTESIAN_POINT('',(2.31399271319931,-12.4135704460881,39.3978017080178));
#179496=CARTESIAN_POINT('',(-18.5518699907145,58.1242364370958,39.3978017080178));
#179497=CARTESIAN_POINT('Origin',(5.5478765747851E-15,0.,39.3978017080178));
#179498=CARTESIAN_POINT('',(-18.5053078998715,57.9809330566519,39.3978017080178));
#179499=CARTESIAN_POINT('Origin',(5.5478765747851E-15,0.,39.3978017080178));
#179500=CARTESIAN_POINT('',(-18.6203878281142,58.3332704847798,39.2708017080178));
#179501=CARTESIAN_POINT('',(-13.0409063549815,59.8282880399728,39.2708017081757));
#179502=CARTESIAN_POINT('Origin',(5.52999282761008E-15,0.,39.2708017080178));
#179503=CARTESIAN_POINT('',(-13.0747351550704,59.9874327886719,38.9890000005756));
#179504=CARTESIAN_POINT('',(-13.0409063549232,59.8282880397056,39.2708017080178));
#179505=CARTESIAN_POINT('',(-13.0752898951319,59.9873118763437,38.989));
#179506=CARTESIAN_POINT('Origin',(5.49031038273072E-15,0.,38.989));
#179507=CARTESIAN_POINT('',(-18.6701227271405,58.4881809372199,38.989));
#179508=CARTESIAN_POINT('Origin',(5.49031038273072E-15,0.,38.989));
#179509=CARTESIAN_POINT('',(-18.6706636022903,58.4880082803371,38.9890000005754));
#179510=CARTESIAN_POINT('Origin',(5.49031038273072E-15,0.,38.989));
#179511=CARTESIAN_POINT('',(-18.670663602406,58.4880082806489,38.989));
#179512=CARTESIAN_POINT('Origin',(62.2224557307631,0.,38.989));
#179513=CARTESIAN_POINT('',(-13.1739864076101,60.451642460649,38.989));
#179514=CARTESIAN_POINT('',(2.3791451040451,-12.7200883457656,38.989));
#179515=CARTESIAN_POINT('',(-18.8168143322221,58.9396512752215,38.989));
#179516=CARTESIAN_POINT('Origin',(5.49031038273072E-15,0.,38.989));
#179517=CARTESIAN_POINT('',(-18.6702850894751,58.4886806371044,38.989));
#179518=CARTESIAN_POINT('Origin',(5.57972911860581E-15,0.,39.624));
#179519=CARTESIAN_POINT('Origin',(-12.7860353045041,58.626452004677,39.6240070731883));
#179520=CARTESIAN_POINT('Origin',(-18.2401946149518,57.1650144220519,39.6240070731883));
#179521=CARTESIAN_POINT('Origin',(5.57972911860581E-15,0.,39.624));
#179522=CARTESIAN_POINT('Origin',(-13.1819467630411,60.4889316843654,39.5552135207998));
#179523=CARTESIAN_POINT('Origin',(-18.8285649482859,58.9759244797165,39.5552117598789));
#179524=CARTESIAN_POINT('Origin',(5.51210908043506E-15,0.,39.1438017080178));
#179525=CARTESIAN_POINT('Origin',(-12.9989886756678,59.6285212670377,39.1711625381293));
#179526=CARTESIAN_POINT('Origin',(-18.5567769230181,58.1392191539792,39.1712173702626));
#179527=CARTESIAN_POINT('Origin',(5.51210908043507E-15,0.,39.1438017080178));
#179528=CARTESIAN_POINT('Origin',(-12.9610560404226,59.4496656337912,39.1712175859416));
#179529=CARTESIAN_POINT('Origin',(-18.5001997164926,57.9653593207583,39.1711627526753));
#179530=CARTESIAN_POINT('Origin',(60.4792282238308,0.,38.989));
#179531=CARTESIAN_POINT('',(-24.1156489724272,54.9452378026831,38.989));
#179532=CARTESIAN_POINT('',(-18.8441205405514,56.9687879773468,38.989));
#179533=CARTESIAN_POINT('Origin',(5.49031038273072E-15,0.,38.989));
#179534=CARTESIAN_POINT('',(-18.9908122363897,57.4202585945868,38.989));
#179535=CARTESIAN_POINT('',(5.47329194811131,-17.8725121057128,38.989));
#179536=CARTESIAN_POINT('',(-18.9913614317952,57.4200769557627,38.9889999995772));
#179537=CARTESIAN_POINT('Origin',(5.49031038273072E-15,0.,38.989));
#179538=CARTESIAN_POINT('',(-24.3081989336288,55.3791342583022,38.9889999997818));
#179539=CARTESIAN_POINT('Origin',(5.49031038273072E-15,0.,38.989));
#179540=CARTESIAN_POINT('',(-24.3087286055912,55.3789017591235,38.989));
#179541=CARTESIAN_POINT('Origin',(5.49031038273072E-15,0.,38.989));
#179542=CARTESIAN_POINT('',(-24.1158676331753,54.9457289227642,38.989));
#179543=CARTESIAN_POINT('Origin',(5.49031038273072E-15,0.,38.989));
#179544=CARTESIAN_POINT('',(-19.0416371860872,57.5748148483578,39.2708017080178));
#179545=CARTESIAN_POINT('',(-18.9913614315652,57.4200769550674,38.989));
#179546=CARTESIAN_POINT('',(-24.3743766271346,55.5277679690274,39.2708017078546));
#179547=CARTESIAN_POINT('Origin',(5.52999282761009E-15,0.,39.2708017080178));
#179548=CARTESIAN_POINT('',(-24.3743766270209,55.5277679687685,39.2708017080178));
#179549=CARTESIAN_POINT('Origin',(60.71525,0.,39.3978017080178));
#179550=CARTESIAN_POINT('',(-24.4643761377912,55.72849184015,39.3978017080178));
#179551=CARTESIAN_POINT('',(-19.109065001131,57.7842031819385,39.3978017080178));
#179552=CARTESIAN_POINT('Origin',(5.5478765747851E-15,0.,39.3978017080178));
#179553=CARTESIAN_POINT('',(-19.155790878562,57.9280106456677,39.3978017080178));
#179554=CARTESIAN_POINT('',(5.4958300222142,-17.9418771653389,39.3978017080178));
#179555=CARTESIAN_POINT('',(-24.5258780191666,55.8666273273835,39.3978017080178));
#179556=CARTESIAN_POINT('Origin',(5.5478765747851E-15,0.,39.3978017080178));
#179557=CARTESIAN_POINT('',(-24.4645917181903,55.7289760416541,39.3978017080178));
#179558=CARTESIAN_POINT('Origin',(5.5478765747851E-15,0.,39.3978017080178));
#179559=CARTESIAN_POINT('',(-24.6158705164589,56.0673542004328,39.2708017080178));
#179560=CARTESIAN_POINT('',(-19.2232259142293,58.1373965172492,39.2708017081757));
#179561=CARTESIAN_POINT('Origin',(5.52999282761008E-15,0.,39.2708017080178));
#179562=CARTESIAN_POINT('',(-19.2735045526304,58.2921333818758,38.9890000005756));
#179563=CARTESIAN_POINT('',(-19.2232259141434,58.1373965169895,39.2708017080178));
#179564=CARTESIAN_POINT('',(-19.2740436149879,58.2919551457918,38.989));
#179565=CARTESIAN_POINT('Origin',(5.49031038273072E-15,0.,38.989));
#179566=CARTESIAN_POINT('',(-24.6815255140421,56.21621732464,38.989));
#179567=CARTESIAN_POINT('Origin',(5.49031038273072E-15,0.,38.989));
#179568=CARTESIAN_POINT('',(-24.6820453786627,56.2159890767414,38.9890000005754));
#179569=CARTESIAN_POINT('Origin',(5.49031038273072E-15,0.,38.989));
#179570=CARTESIAN_POINT('',(-24.6820453788103,56.2159890770394,38.989));
#179571=CARTESIAN_POINT('Origin',(62.2224557307631,0.,38.989));
#179572=CARTESIAN_POINT('',(-19.4207352200695,58.7434254837934,38.989));
#179573=CARTESIAN_POINT('',(5.6397553624924,-18.3848338156955,38.989));
#179574=CARTESIAN_POINT('',(-24.8746050278048,56.6498810128384,38.989));
#179575=CARTESIAN_POINT('Origin',(5.49031038273072E-15,0.,38.989));
#179576=CARTESIAN_POINT('',(-24.6817392197999,56.2166973156308,38.989));
#179577=CARTESIAN_POINT('Origin',(5.57972911860581E-15,0.,39.624));
#179578=CARTESIAN_POINT('Origin',(-18.8441250001649,56.9687855447426,39.6240070731883));
#179579=CARTESIAN_POINT('Origin',(-24.1156440305584,54.9452389789698,39.6240070731883));
#179580=CARTESIAN_POINT('Origin',(5.57972911860581E-15,0.,39.624));
#179581=CARTESIAN_POINT('Origin',(-19.4325497530907,58.7796783495197,39.5552135208017));
#179582=CARTESIAN_POINT('Origin',(-24.8900828550914,56.6847272350837,39.5552117598772));
#179583=CARTESIAN_POINT('Origin',(5.51210908043506E-15,0.,39.1438017080178));
#179584=CARTESIAN_POINT('Origin',(-19.1606565505623,57.9431056782018,39.1711625381312));
#179585=CARTESIAN_POINT('Origin',(-24.5323241911529,55.8810150532827,39.1712173702612));
#179586=CARTESIAN_POINT('Origin',(5.51210908043507E-15,0.,39.1438017080178));
#179587=CARTESIAN_POINT('Origin',(-19.1042362097708,57.7691948748993,39.1712175859379));
#179588=CARTESIAN_POINT('Origin',(-24.4578836192968,55.7140215708741,39.171162752673));
#179589=CARTESIAN_POINT('Origin',(60.4792282238308,0.,38.989));
#179590=CARTESIAN_POINT('',(-29.7268821954845,52.1234703131949,38.989));
#179591=CARTESIAN_POINT('',(-24.6957503380303,54.6869600343299,38.989));
#179592=CARTESIAN_POINT('Origin',(5.49031038273072E-15,0.,38.989));
#179593=CARTESIAN_POINT('',(-24.8888299712407,55.1206239907504,38.989));
#179594=CARTESIAN_POINT('',(9.71531210234964,-22.6015516358793,38.989));
#179595=CARTESIAN_POINT('',(-24.8893571716693,55.1203859404114,38.988999999577));
#179596=CARTESIAN_POINT('Origin',(5.49031038273072E-15,0.,38.989));
#179597=CARTESIAN_POINT('',(-29.963731877575,52.5348628870841,38.9889999997818));
#179598=CARTESIAN_POINT('Origin',(5.49031038273072E-15,0.,38.989));
#179599=CARTESIAN_POINT('',(-29.964234345157,52.5345762957641,38.989));
#179600=CARTESIAN_POINT('Origin',(5.49031038273072E-15,0.,38.989));
#179601=CARTESIAN_POINT('',(-29.7271509944135,52.1239358865969,38.989));
#179602=CARTESIAN_POINT('Origin',(5.49031038273072E-15,0.,38.989));
#179603=CARTESIAN_POINT('',(-24.955532024241,55.2690209153042,39.2708017080178));
#179604=CARTESIAN_POINT('',(-24.8893571713678,55.1203859397437,38.989));
#179605=CARTESIAN_POINT('',(-30.0450834961232,52.6757649141855,39.2708017078546));
#179606=CARTESIAN_POINT('Origin',(5.52999282761009E-15,0.,39.2708017080178));
#179607=CARTESIAN_POINT('',(-30.0450834959832,52.6757649139399,39.2708017080178));
#179608=CARTESIAN_POINT('Origin',(60.71525,0.,39.3978017080178));
#179609=CARTESIAN_POINT('',(-30.1555713378333,52.8659816883962,39.3978017080178));
#179610=CARTESIAN_POINT('',(-25.0444775033943,55.4702140717969,39.3978017080178));
#179611=CARTESIAN_POINT('Origin',(5.5478765747851E-15,0.,39.3978017080178));
#179612=CARTESIAN_POINT('',(-25.1059793847697,55.6083495590304,39.3978017080178));
#179613=CARTESIAN_POINT('',(9.75435829333326,-22.6892508167094,39.3978017080178));
#179614=CARTESIAN_POINT('',(-30.2311753956707,52.996931757829,39.3978017080178));
#179615=CARTESIAN_POINT('Origin',(5.5478765747851E-15,0.,39.3978017080178));
#179616=CARTESIAN_POINT('',(-30.1558363500995,52.8664407031059,39.3978017080178));
#179617=CARTESIAN_POINT('Origin',(5.5478765747851E-15,0.,39.3978017080178));
#179618=CARTESIAN_POINT('',(-30.3416565762231,53.1871522506178,39.2708017080178));
#179619=CARTESIAN_POINT('',(-25.1949317876421,55.8095395122502,39.2708017081757));
#179620=CARTESIAN_POINT('Origin',(5.52999282761008E-15,0.,39.2708017080178));
#179621=CARTESIAN_POINT('',(-25.2611094010716,55.9581731633347,38.9890000005756));
#179622=CARTESIAN_POINT('',(-25.1949317875296,55.8095395120009,39.2708017080178));
#179623=CARTESIAN_POINT('',(-25.2616268796452,55.9579395562868,38.989));
#179624=CARTESIAN_POINT('Origin',(5.49031038273072E-15,0.,38.989));
#179625=CARTESIAN_POINT('',(-30.4225123424706,53.3283370710515,38.989));
#179626=CARTESIAN_POINT('Origin',(5.49031038273072E-15,0.,38.989));
#179627=CARTESIAN_POINT('',(-30.4230055008163,53.3280557328689,38.9890000005754));
#179628=CARTESIAN_POINT('Origin',(5.49031038273072E-15,0.,38.989));
#179629=CARTESIAN_POINT('',(-30.4230055009943,53.3280557331498,38.989));
#179630=CARTESIAN_POINT('Origin',(62.2224557307631,0.,38.989));
#179631=CARTESIAN_POINT('',(-25.4547063934078,56.3916032444853,38.989));
#179632=CARTESIAN_POINT('',(10.0037024164483,-23.2492868865826,38.989));
#179633=CARTESIAN_POINT('',(-30.659864345357,53.7394427993289,38.989));
#179634=CARTESIAN_POINT('Origin',(5.49031038273072E-15,0.,38.989));
#179635=CARTESIAN_POINT('',(-30.4227750502466,53.328792094267,38.989));
#179636=CARTESIAN_POINT('Origin',(5.57972911860581E-15,0.,39.624));
#179637=CARTESIAN_POINT('Origin',(-24.6957545189371,54.6869571488953,39.6240070731883));
#179638=CARTESIAN_POINT('Origin',(-29.7268774036432,52.1234719996038,39.6240070731883));
#179639=CARTESIAN_POINT('Origin',(5.57972911860581E-15,0.,39.624));
#179640=CARTESIAN_POINT('Origin',(-25.4702456615205,56.4264225582429,39.5552135207977));
#179641=CARTESIAN_POINT('Origin',(-30.6788998055462,53.7724802568187,39.5552117598843));
#179642=CARTESIAN_POINT('Origin',(5.51210908043506E-15,0.,39.1438017080178));
#179643=CARTESIAN_POINT('Origin',(-25.112396262664,55.6228532981809,39.1711625381333));
#179644=CARTESIAN_POINT('Origin',(-30.2390901817291,53.0105668578062,39.1712173702566));
#179645=CARTESIAN_POINT('Origin',(5.51210908043507E-15,0.,39.1438017080178));
#179646=CARTESIAN_POINT('Origin',(-25.0381063693886,55.4557927279736,39.171217585938));
#179647=CARTESIAN_POINT('Origin',(-30.147601831023,52.8522693417483,39.1711627526774));
#179648=CARTESIAN_POINT('Origin',(60.4792282238308,0.,38.989));
#179649=CARTESIAN_POINT('',(-35.0124214764581,48.7306271754179,38.989));
#179650=CARTESIAN_POINT('',(-30.2768083268876,51.8059703131949,38.989));
#179651=CARTESIAN_POINT('Origin',(5.49031038273072E-15,0.,38.989));
#179652=CARTESIAN_POINT('',(-30.5141604766043,52.2170762957393,38.989));
#179653=CARTESIAN_POINT('',(14.8448439902557,-26.3470240215568,38.989));
#179654=CARTESIAN_POINT('',(-30.5146599059373,52.2167844420138,38.9889999995774));
#179655=CARTESIAN_POINT('Origin',(5.49031038273072E-15,0.,38.989));
#179656=CARTESIAN_POINT('',(-35.2909759047564,49.1150085644483,38.9889999997818));
#179657=CARTESIAN_POINT('Origin',(5.49031038273072E-15,0.,38.989));
#179658=CARTESIAN_POINT('',(-35.2914456628182,49.1146710209413,38.989));
#179659=CARTESIAN_POINT('Origin',(5.49031038273072E-15,0.,38.989));
#179660=CARTESIAN_POINT('',(-35.0127374685506,48.7310621012212,38.989));
#179661=CARTESIAN_POINT('Origin',(5.49031038273072E-15,0.,38.989));
#179662=CARTESIAN_POINT('',(-30.5960088312564,52.3576880233165,39.2708017080178));
#179663=CARTESIAN_POINT('',(-30.514659905568,52.2167844413818,38.989));
#179664=CARTESIAN_POINT('',(-35.3866101429905,49.2466351558312,39.2708017078546));
#179665=CARTESIAN_POINT('Origin',(5.52999282761009E-15,0.,39.2708017080178));
#179666=CARTESIAN_POINT('',(-35.3866101428255,49.2466351556016,39.2708017080178));
#179667=CARTESIAN_POINT('Origin',(60.71525,0.,39.3978017080178));
#179668=CARTESIAN_POINT('',(-35.5163757878391,49.4242607783464,39.3978017080178));
#179669=CARTESIAN_POINT('',(-30.7054974692364,52.5484816883962,39.3978017080178));
#179670=CARTESIAN_POINT('Origin',(5.5478765747851E-15,0.,39.3978017080178));
#179671=CARTESIAN_POINT('',(-30.7811015270739,52.679431757829,39.3978017080178));
#179672=CARTESIAN_POINT('',(14.903849434298,-26.4492244485613,39.3978017080178));
#179673=CARTESIAN_POINT('',(-35.6052536882598,49.5465907136148,39.3978017080178));
#179674=CARTESIAN_POINT('Origin',(5.5478765747851E-15,0.,39.3978017080178));
#179675=CARTESIAN_POINT('',(-35.5166873284426,49.4246895772005,39.3978017080178));
#179676=CARTESIAN_POINT('Origin',(5.5478765747851E-15,0.,39.3978017080178));
#179677=CARTESIAN_POINT('',(-35.7350130971385,49.7242207306178,39.2708017080178));
#179678=CARTESIAN_POINT('',(-30.8905967160111,52.870221513458,39.2708017081757));
#179679=CARTESIAN_POINT('Origin',(5.52999282761008E-15,0.,39.2708017080178));
#179680=CARTESIAN_POINT('',(-30.9719482486877,53.0111234896156,38.9890000005756));
#179681=CARTESIAN_POINT('',(-30.8905967158731,52.8702215132219,39.2708017080178));
#179682=CARTESIAN_POINT('',(-30.9724384738737,53.0108370710515,38.989));
#179683=CARTESIAN_POINT('Origin',(5.49031038273072E-15,0.,38.989));
#179684=CARTESIAN_POINT('',(-35.830183759355,49.8561803968406,38.989));
#179685=CARTESIAN_POINT('Origin',(5.49031038273072E-15,0.,38.989));
#179686=CARTESIAN_POINT('',(-35.8306448082798,49.855849050774,38.9890000005754));
#179687=CARTESIAN_POINT('Origin',(5.49031038273072E-15,0.,38.989));
#179688=CARTESIAN_POINT('',(-35.8306448084862,49.8558490510348,38.989));
#179689=CARTESIAN_POINT('Origin',(62.2224557307631,0.,38.989));
#179690=CARTESIAN_POINT('',(-31.2097904767601,53.4219427993289,38.989));
#179691=CARTESIAN_POINT('',(15.2806508669887,-27.1018636743464,38.989));
#179692=CARTESIAN_POINT('',(-36.1092077731524,50.2402240048086,38.989));
#179693=CARTESIAN_POINT('Origin',(5.49031038273072E-15,0.,38.989));
#179694=CARTESIAN_POINT('',(-35.8304925908678,49.8566054669512,38.989));
#179695=CARTESIAN_POINT('Origin',(5.57972911860581E-15,0.,39.624));
#179696=CARTESIAN_POINT('Origin',(-30.2768121832811,51.8059670065432,39.6240070731883));
#179697=CARTESIAN_POINT('Origin',(-35.0124168871447,48.7306293534723,39.6240070731883));
#179698=CARTESIAN_POINT('Origin',(5.57972911860581E-15,0.,39.624));
#179699=CARTESIAN_POINT('Origin',(-31.2288842284945,53.4549470734247,39.5552135208013));
#179700=CARTESIAN_POINT('Origin',(-36.1315923097633,50.2710907322474,39.5552117598819));
#179701=CARTESIAN_POINT('Origin',(5.51210908043506E-15,0.,39.1438017080178));
#179702=CARTESIAN_POINT('Origin',(-30.7889993062062,52.6931852975962,39.1711625381386));
#179703=CARTESIAN_POINT('Origin',(-35.614550372342,49.5593237986677,39.1712173702654));
#179704=CARTESIAN_POINT('Origin',(5.51210908043507E-15,0.,39.1438017080178));
#179705=CARTESIAN_POINT('Origin',(-30.6976537960621,52.5348053110493,39.1712175859384));
#179706=CARTESIAN_POINT('Origin',(-35.5070166083006,49.4114565896685,39.1711627526738));
#179707=CARTESIAN_POINT('Origin',(60.4792282238308,0.,38.989));
#179708=CARTESIAN_POINT('',(-39.9143573409153,44.8038810887678,38.989));
#179709=CARTESIAN_POINT('',(-35.5261472678861,48.3573835402122,38.989));
#179710=CARTESIAN_POINT('Origin',(5.49031038273072E-15,0.,38.989));
#179711=CARTESIAN_POINT('',(-35.8051714542876,48.7414273857064,38.989));
#179712=CARTESIAN_POINT('',(20.6381965522785,-28.9462038689907,38.989));
#179713=CARTESIAN_POINT('',(-35.8056376406732,48.7410849262056,38.9889999995772));
#179714=CARTESIAN_POINT('Origin',(5.49031038273072E-15,0.,38.989));
#179715=CARTESIAN_POINT('',(-40.2315646148138,45.1570399300041,38.9889999997818));
#179716=CARTESIAN_POINT('Origin',(5.49031038273072E-15,0.,38.989));
#179717=CARTESIAN_POINT('',(-40.2319965165878,45.1566551325075,38.989));
#179718=CARTESIAN_POINT('Origin',(5.49031038273072E-15,0.,38.989));
#179719=CARTESIAN_POINT('',(-39.914717064096,44.8042806018341,38.989));
#179720=CARTESIAN_POINT('Origin',(5.49031038273072E-15,0.,38.989));
#179721=CARTESIAN_POINT('',(-35.90126936289,48.8727133447947,39.2708017080178));
#179722=CARTESIAN_POINT('',(-35.8056376402397,48.7410849256154,38.989));
#179723=CARTESIAN_POINT('',(-40.3404336840069,45.2779489571887,39.2708017078546));
#179724=CARTESIAN_POINT('Origin',(5.52999282761009E-15,0.,39.2708017080178));
#179725=CARTESIAN_POINT('',(-40.3404336838189,45.2779489569776,39.2708017080178));
#179726=CARTESIAN_POINT('Origin',(60.71525,0.,39.3978017080178));
#179727=CARTESIAN_POINT('',(-40.4880553924339,45.4410373245175,39.3978017080178));
#179728=CARTESIAN_POINT('',(-36.0301015792672,49.0510171431407,39.3978017080178));
#179729=CARTESIAN_POINT('Origin',(5.5478765747851E-15,0.,39.3978017080178));
#179730=CARTESIAN_POINT('',(-36.1189794796879,49.1733470784091,39.3978017080178));
#179731=CARTESIAN_POINT('',(20.7197400704237,-29.0584388930974,39.3978017080178));
#179732=CARTESIAN_POINT('',(-40.5892333705619,45.5534068532515,39.3978017080178));
#179733=CARTESIAN_POINT('Origin',(5.5478765747851E-15,0.,39.3978017080178));
#179734=CARTESIAN_POINT('',(-40.4884100480707,45.4414312095062,39.3978017080178));
#179735=CARTESIAN_POINT('Origin',(5.5478765747851E-15,0.,39.3978017080178));
#179736=CARTESIAN_POINT('',(-40.7368493365293,45.716500242831,39.2708017080178));
#179737=CARTESIAN_POINT('',(-36.2478178024865,49.3516463039592,39.2708017081757));
#179738=CARTESIAN_POINT('Origin',(5.52999282761008E-15,0.,39.2708017080178));
#179739=CARTESIAN_POINT('',(-36.3434519499943,49.4832728536535,38.9890000005756));
#179740=CARTESIAN_POINT('',(-36.2478178023246,49.3516463037388,39.2708017080178));
#179741=CARTESIAN_POINT('',(-36.3439095507831,49.4829367616349,38.989));
#179742=CARTESIAN_POINT('Origin',(5.49031038273072E-15,0.,38.989));
#179743=CARTESIAN_POINT('',(-40.845292185024,45.8377889771254,38.989));
#179744=CARTESIAN_POINT('Origin',(5.49031038273072E-15,0.,38.989));
#179745=CARTESIAN_POINT('',(-40.8457160731793,45.8374112534716,38.9890000005754));
#179746=CARTESIAN_POINT('Origin',(5.49031038273072E-15,0.,38.989));
#179747=CARTESIAN_POINT('',(-40.8457160734119,45.8374112537094,38.989));
#179748=CARTESIAN_POINT('Origin',(62.2224557307631,0.,38.989));
#179749=CARTESIAN_POINT('',(-36.6229335645805,49.8669803696029,38.989));
#179750=CARTESIAN_POINT('',(21.2404668433927,-29.7751578089171,38.989));
#179751=CARTESIAN_POINT('',(-41.1629311642477,46.1905628026488,38.989));
#179752=CARTESIAN_POINT('Origin',(5.49031038273072E-15,0.,38.989));
#179753=CARTESIAN_POINT('',(-40.8456437566508,45.8381794369741,38.989));
#179754=CARTESIAN_POINT('Origin',(5.57972911860581E-15,0.,39.624));
#179755=CARTESIAN_POINT('Origin',(-35.5261507575146,48.3573798485718,39.6240070731883));
#179756=CARTESIAN_POINT('Origin',(-39.9143530044114,44.8038837346044,39.6240070731883));
#179757=CARTESIAN_POINT('Origin',(5.57972911860581E-15,0.,39.624));
#179758=CARTESIAN_POINT('Origin',(-36.6453726048013,49.8978080023008,39.555213520804));
#179759=CARTESIAN_POINT('Origin',(-41.1884195276088,46.218920617714,39.5552117598819));
#179760=CARTESIAN_POINT('Origin',(5.51210908043506E-15,0.,39.1438017080178));
#179761=CARTESIAN_POINT('Origin',(-36.1282716303341,49.1861997321277,39.1711625381329));
#179762=CARTESIAN_POINT('Origin',(-40.5998100962482,45.5650984170306,39.1712173702632));
#179763=CARTESIAN_POINT('Origin',(5.51210908043507E-15,0.,39.1438017080178));
#179764=CARTESIAN_POINT('Origin',(-36.0208713038459,49.0382355735241,39.1712175859398));
#179765=CARTESIAN_POINT('Origin',(-40.4774090812904,45.4292815791817,39.1711627526756));
#179766=CARTESIAN_POINT('Origin',(60.4792282238308,0.,38.989));
#179767=CARTESIAN_POINT('',(-44.3789831537292,40.3862543050942,38.989));
#179768=CARTESIAN_POINT('',(-40.3862543050934,44.3789831537299,38.989));
#179769=CARTESIAN_POINT('Origin',(5.49031038273072E-15,0.,38.989));
#179770=CARTESIAN_POINT('',(-40.7038934808039,44.7317571974363,38.989));
#179771=CARTESIAN_POINT('',(26.8427652369004,-30.2864073093061,38.989));
#179772=CARTESIAN_POINT('',(-40.7043213166062,44.7313678842177,38.9889999995774));
#179773=CARTESIAN_POINT('Origin',(5.49031038273072E-15,0.,38.989));
#179774=CARTESIAN_POINT('',(-44.7313678839552,40.7043213163687,38.9889999997818));
#179775=CARTESIAN_POINT('Origin',(5.49031038273072E-15,0.,38.989));
#179776=CARTESIAN_POINT('',(-44.7317571974351,40.7038934808043,38.989));
#179777=CARTESIAN_POINT('Origin',(5.49031038273072E-15,0.,38.989));
#179778=CARTESIAN_POINT('',(-44.3793826667955,40.3866140282749,38.989));
#179779=CARTESIAN_POINT('Origin',(5.49031038273072E-15,0.,38.989));
#179780=CARTESIAN_POINT('',(-40.8131880745603,44.8522789915945,39.2708017080178));
#179781=CARTESIAN_POINT('',(-40.7043213161135,44.7313678836763,38.989));
#179782=CARTESIAN_POINT('',(-44.8522789918029,40.8131880747513,39.2708017078546));
#179783=CARTESIAN_POINT('Origin',(5.52999282761009E-15,0.,39.2708017080178));
#179784=CARTESIAN_POINT('',(-44.8522789915938,40.813188074561,39.2708017080178));
#179785=CARTESIAN_POINT('Origin',(60.71525,0.,39.3978017080178));
#179786=CARTESIAN_POINT('',(-45.016139389479,40.9599523566129,39.3978017080178));
#179787=CARTESIAN_POINT('',(-40.9599523566121,45.0161393894797,39.3978017080178));
#179788=CARTESIAN_POINT('Origin',(5.5478765747851E-15,0.,39.3978017080178));
#179789=CARTESIAN_POINT('',(-41.06113033474,45.1285089182136,39.3978017080178));
#179790=CARTESIAN_POINT('',(26.9484406282047,-30.4037717213982,39.3978017080178));
#179791=CARTESIAN_POINT('',(-45.1285089182129,41.0611303347408,39.3978017080178));
#179792=CARTESIAN_POINT('Origin',(5.5478765747851E-15,0.,39.3978017080178));
#179793=CARTESIAN_POINT('',(-45.0165332744676,40.9603070122496,39.3978017080178));
#179794=CARTESIAN_POINT('Origin',(5.5478765747851E-15,0.,39.3978017080178));
#179795=CARTESIAN_POINT('',(-45.2923641298554,41.2079002115911,39.2708017080178));
#179796=CARTESIAN_POINT('',(-41.2079002117744,45.2923641300583,39.2708017081757));
#179797=CARTESIAN_POINT('Origin',(5.52999282761008E-15,0.,39.2708017080178));
#179798=CARTESIAN_POINT('',(-41.3167691863805,45.4132731252661,38.9890000005756));
#179799=CARTESIAN_POINT('',(-41.2079002115903,45.2923641298561,39.2708017080178));
#179800=CARTESIAN_POINT('',(-41.3171891492021,45.4128910420876,38.989));
#179801=CARTESIAN_POINT('Origin',(5.49031038273072E-15,0.,38.989));
#179802=CARTESIAN_POINT('',(-45.4128910420869,41.3171891492029,38.989));
#179803=CARTESIAN_POINT('Origin',(5.49031038273072E-15,0.,38.989));
#179804=CARTESIAN_POINT('',(-45.4132731252655,41.3167691863813,38.9890000005754));
#179805=CARTESIAN_POINT('Origin',(5.49031038273072E-15,0.,38.989));
#179806=CARTESIAN_POINT('',(-45.4132731255216,41.3167691865935,38.989));
#179807=CARTESIAN_POINT('Origin',(62.2224557307631,0.,38.989));
#179808=CARTESIAN_POINT('',(-41.6348281284258,45.765664867611,38.989));
#179809=CARTESIAN_POINT('',(27.6232705441538,-31.1532462714324,38.989));
#179810=CARTESIAN_POINT('',(-45.7656648676103,41.6348281284266,38.989));
#179811=CARTESIAN_POINT('Origin',(5.49031038273072E-15,0.,38.989));
#179812=CARTESIAN_POINT('',(-45.4132815019355,41.3175407208297,38.989));
#179813=CARTESIAN_POINT('Origin',(5.57972911860581E-15,0.,39.624));
#179814=CARTESIAN_POINT('Origin',(-40.3862573897239,44.3789791175472,39.6240070731883));
#179815=CARTESIAN_POINT('Origin',(-44.3789791175464,40.3862573897248,39.6240070731883));
#179816=CARTESIAN_POINT('Origin',(5.57972911860581E-15,0.,39.624));
#179817=CARTESIAN_POINT('Origin',(-41.6603666103049,45.7939781049238,39.5552135208033));
#179818=CARTESIAN_POINT('Origin',(-45.7939778018808,41.6603663369617,39.5552117598793));
#179819=CARTESIAN_POINT('Origin',(5.51210908043506E-15,0.,39.1438017080178));
#179820=CARTESIAN_POINT('Origin',(-41.0717150501544,45.1403198695223,39.1711625381314));
#179821=CARTESIAN_POINT('Origin',(-45.1402498046847,41.0716522820281,39.1712173702639));
#179822=CARTESIAN_POINT('Origin',(5.51210908043507E-15,0.,39.1438017080178));
#179823=CARTESIAN_POINT('Origin',(-40.9494366077754,45.0043926651436,39.1712175859396));
#179824=CARTESIAN_POINT('Origin',(-45.0043225899482,40.9493738530245,39.1711627526731));
#179825=CARTESIAN_POINT('Origin',(60.4792282238308,0.,38.989));
#179826=CARTESIAN_POINT('',(-48.3573835402116,35.526147267887,38.989));
#179827=CARTESIAN_POINT('',(-44.8038810887671,39.9143573409161,38.989));
#179828=CARTESIAN_POINT('Origin',(5.49031038273072E-15,0.,38.989));
#179829=CARTESIAN_POINT('',(-45.1566551325072,40.231996516589,38.989));
#179830=CARTESIAN_POINT('',(33.1880655373213,-30.3099068238764,38.989));
#179831=CARTESIAN_POINT('',(-45.1570399302679,40.2315646150502,38.9889999995773));
#179832=CARTESIAN_POINT('Origin',(5.49031038273072E-15,0.,38.989));
#179833=CARTESIAN_POINT('',(-48.7410849259195,35.8056376404643,38.9889999997818));
#179834=CARTESIAN_POINT('Origin',(5.49031038273072E-15,0.,38.989));
#179835=CARTESIAN_POINT('',(-48.7414273857053,35.8051714542881,38.989));
#179836=CARTESIAN_POINT('Origin',(5.49031038273072E-15,0.,38.989));
#179837=CARTESIAN_POINT('',(-48.3578184660148,35.5264632599795,38.989));
#179838=CARTESIAN_POINT('Origin',(5.49031038273072E-15,0.,38.989));
#179839=CARTESIAN_POINT('',(-45.2779489569769,40.3404336838196,39.2708017080178));
#179840=CARTESIAN_POINT('',(-45.1570399297212,40.2315646145632,38.989));
#179841=CARTESIAN_POINT('',(-48.8727133450219,35.9012693630583,39.2708017078546));
#179842=CARTESIAN_POINT('Origin',(5.52999282761009E-15,0.,39.2708017080178));
#179843=CARTESIAN_POINT('',(-48.8727133447941,35.9012693628909,39.2708017080178));
#179844=CARTESIAN_POINT('Origin',(60.71525,0.,39.3978017080178));
#179845=CARTESIAN_POINT('',(-49.05101714314,36.0301015792681,39.3978017080178));
#179846=CARTESIAN_POINT('',(-45.4410373245168,40.4880553924347,39.3978017080178));
#179847=CARTESIAN_POINT('Origin',(5.5478765747851E-15,0.,39.3978017080178));
#179848=CARTESIAN_POINT('',(-45.5534068532508,40.5892333705626,39.3978017080178));
#179849=CARTESIAN_POINT('',(33.3184119221863,-30.4272712359684,39.3978017080178));
#179850=CARTESIAN_POINT('',(-49.1733470784084,36.1189794796887,39.3978017080178));
#179851=CARTESIAN_POINT('Origin',(5.5478765747851E-15,0.,39.3978017080178));
#179852=CARTESIAN_POINT('',(-49.0514459419942,36.0304131198716,39.3978017080178));
#179853=CARTESIAN_POINT('Origin',(5.5478765747851E-15,0.,39.3978017080178));
#179854=CARTESIAN_POINT('',(-49.3516463037382,36.2478178023255,39.2708017080178));
#179855=CARTESIAN_POINT('',(-45.7165002430345,40.736849336712,39.2708017081757));
#179856=CARTESIAN_POINT('Origin',(5.52999282761008E-15,0.,39.2708017080178));
#179857=CARTESIAN_POINT('',(-45.8374112534709,40.84571607318,38.9890000005756));
#179858=CARTESIAN_POINT('',(-45.7165002428303,40.7368493365301,39.2708017080178));
#179859=CARTESIAN_POINT('',(-45.8377889771247,40.8452921850248,38.989));
#179860=CARTESIAN_POINT('Origin',(5.49031038273072E-15,0.,38.989));
#179861=CARTESIAN_POINT('',(-49.4829367616343,36.343909550784,38.989));
#179862=CARTESIAN_POINT('Origin',(5.49031038273072E-15,0.,38.989));
#179863=CARTESIAN_POINT('',(-49.4832728536529,36.3434519499952,38.9890000005754));
#179864=CARTESIAN_POINT('Origin',(5.49031038273072E-15,0.,38.989));
#179865=CARTESIAN_POINT('',(-49.4832728539298,36.3434519501794,38.989));
#179866=CARTESIAN_POINT('Origin',(62.2224557307631,0.,38.989));
#179867=CARTESIAN_POINT('',(-46.1905628026481,41.1629311642484,38.989));
#179868=CARTESIAN_POINT('',(34.1507877370002,-31.1767457860026,38.989));
#179869=CARTESIAN_POINT('',(-49.8669803696023,36.6229335645814,38.989));
#179870=CARTESIAN_POINT('Origin',(5.49031038273072E-15,0.,38.989));
#179871=CARTESIAN_POINT('',(-49.4833618317449,36.3442183822967,38.989));
#179872=CARTESIAN_POINT('Origin',(5.57972911860581E-15,0.,39.624));
#179873=CARTESIAN_POINT('Origin',(-44.8038837346036,39.9143530044123,39.6240070731883));
#179874=CARTESIAN_POINT('Origin',(-48.3573798485711,35.5261507575156,39.6240070731883));
#179875=CARTESIAN_POINT('Origin',(5.57972911860581E-15,0.,39.624));
#179876=CARTESIAN_POINT('Origin',(-46.2189209212417,41.1884198004172,39.5552135208006));
#179877=CARTESIAN_POINT('Origin',(-49.897807672349,36.6453723646258,39.5552117598824));
#179878=CARTESIAN_POINT('Origin',(5.51210908043506E-15,0.,39.1438017080178));
#179879=CARTESIAN_POINT('Origin',(-45.5651681650772,40.5998732162083,39.1711625381327));
#179880=CARTESIAN_POINT('Origin',(-49.1861234900541,36.1282165298261,39.1712173702595));
#179881=CARTESIAN_POINT('Origin',(5.51210908043507E-15,0.,39.1438017080178));
#179882=CARTESIAN_POINT('Origin',(-45.4293513150125,40.4774722129461,39.1712175859399));
#179883=CARTESIAN_POINT('Origin',(-49.0381593225488,36.0208162177226,39.171162752677));
#179884=CARTESIAN_POINT('Origin',(60.4792282238308,0.,38.989));
#179885=CARTESIAN_POINT('',(-51.8059703131944,30.2768083268885,38.989));
#179886=CARTESIAN_POINT('',(-48.7306271754173,35.0124214764589,38.989));
#179887=CARTESIAN_POINT('Origin',(5.49031038273072E-15,0.,38.989));
#179888=CARTESIAN_POINT('',(-49.1146710209412,35.2914456628195,38.989));
#179889=CARTESIAN_POINT('',(39.3975469582344,-29.0164449471022,38.989));
#179890=CARTESIAN_POINT('',(-49.115008564735,35.2909759049636,38.9889999995775));
#179891=CARTESIAN_POINT('Origin',(5.49031038273072E-15,0.,38.989));
#179892=CARTESIAN_POINT('',(-52.2167844417076,30.5146599057596,38.9889999997818));
#179893=CARTESIAN_POINT('Origin',(5.49031038273072E-15,0.,38.989));
#179894=CARTESIAN_POINT('',(-52.2170762957382,30.5141604766049,38.989));
#179895=CARTESIAN_POINT('Origin',(5.49031038273072E-15,0.,38.989));
#179896=CARTESIAN_POINT('',(-51.8064358865964,30.2770771258175,38.989));
#179897=CARTESIAN_POINT('Origin',(5.49031038273072E-15,0.,38.989));
#179898=CARTESIAN_POINT('',(-49.246635155601,35.3866101428264,39.2708017080178));
#179899=CARTESIAN_POINT('',(-49.1150085641408,35.2909759045367,38.989));
#179900=CARTESIAN_POINT('',(-52.3576880235601,30.5960088313999,39.2708017078546));
#179901=CARTESIAN_POINT('Origin',(5.52999282761009E-15,0.,39.2708017080178));
#179902=CARTESIAN_POINT('',(-52.357688023316,30.5960088312573,39.2708017080178));
#179903=CARTESIAN_POINT('Origin',(60.71525,0.,39.3978017080178));
#179904=CARTESIAN_POINT('',(-52.5484816883957,30.7054974692373,39.3978017080178));
#179905=CARTESIAN_POINT('',(-49.4242607783458,35.51637578784,39.3978017080178));
#179906=CARTESIAN_POINT('Origin',(5.5478765747851E-15,0.,39.3978017080178));
#179907=CARTESIAN_POINT('',(-49.5465907136142,35.6052536882606,39.3978017080178));
#179908=CARTESIAN_POINT('',(39.5520252162584,-29.1286799712089,39.3978017080178));
#179909=CARTESIAN_POINT('',(-52.6794317578285,30.7811015270748,39.3978017080178));
#179910=CARTESIAN_POINT('Origin',(5.5478765747851E-15,0.,39.3978017080178));
#179911=CARTESIAN_POINT('',(-52.5489407031054,30.7057624815036,39.3978017080178));
#179912=CARTESIAN_POINT('Origin',(5.5478765747851E-15,0.,39.3978017080178));
#179913=CARTESIAN_POINT('',(-52.8702215132213,30.8905967158741,39.2708017080178));
#179914=CARTESIAN_POINT('',(-49.7242207308393,35.7350130972989,39.2708017081757));
#179915=CARTESIAN_POINT('Origin',(5.52999282761008E-15,0.,39.2708017080178));
#179916=CARTESIAN_POINT('',(-49.8558490507733,35.8306448082806,38.9890000005756));
#179917=CARTESIAN_POINT('',(-49.7242207306172,35.7350130971393,39.2708017080178));
#179918=CARTESIAN_POINT('',(-49.85618039684,35.8301837593559,38.989));
#179919=CARTESIAN_POINT('Origin',(5.49031038273072E-15,0.,38.989));
#179920=CARTESIAN_POINT('',(-53.010837071051,30.9724384738747,38.989));
#179921=CARTESIAN_POINT('Origin',(5.49031038273072E-15,0.,38.989));
#179922=CARTESIAN_POINT('',(-53.0111234896151,30.9719482486886,38.9890000005754));
#179923=CARTESIAN_POINT('Origin',(5.49031038273072E-15,0.,38.989));
#179924=CARTESIAN_POINT('',(-53.0111234899097,30.9719482488429,38.989));
#179925=CARTESIAN_POINT('Origin',(62.2224557307631,0.,38.989));
#179926=CARTESIAN_POINT('',(-50.240224004808,36.1092077731533,38.989));
#179927=CARTESIAN_POINT('',(40.5385041740525,-29.8453988870287,38.989));
#179928=CARTESIAN_POINT('',(-53.4219427993284,31.209790476761,38.989));
#179929=CARTESIAN_POINT('Origin',(5.49031038273072E-15,0.,38.989));
#179930=CARTESIAN_POINT('',(-53.0112920942665,30.9727011816506,38.989));
#179931=CARTESIAN_POINT('Origin',(5.57972911860581E-15,0.,39.624));
#179932=CARTESIAN_POINT('Origin',(-48.7306293534716,35.0124168871457,39.6240070731883));
#179933=CARTESIAN_POINT('Origin',(-51.8059670065426,30.2768121832821,39.6240070731883));
#179934=CARTESIAN_POINT('Origin',(5.57972911860581E-15,0.,39.624));
#179935=CARTESIAN_POINT('Origin',(-50.2710910626268,36.1315925493537,39.5552135208003));
#179936=CARTESIAN_POINT('Origin',(-53.4549467201713,31.2288840241332,39.5552117598781));
#179937=CARTESIAN_POINT('Origin',(5.51210908043506E-15,0.,39.1438017080178));
#179938=CARTESIAN_POINT('Origin',(-49.5593997624591,35.6146058558679,39.1711625381343));
#179939=CARTESIAN_POINT('Origin',(-52.6931037136118,30.7889524770105,39.171217370262));
#179940=CARTESIAN_POINT('Origin',(5.51210908043507E-15,0.,39.1438017080178));
#179941=CARTESIAN_POINT('Origin',(-49.4115325425356,35.5070721047332,39.1712175859377));
#179942=CARTESIAN_POINT('Origin',(-52.5347237197191,30.697606982104,39.1711627526724));
#179943=CARTESIAN_POINT('Origin',(60.4792282238308,0.,38.989));
#179944=CARTESIAN_POINT('',(-54.6869600343295,24.6957503380312,38.989));
#179945=CARTESIAN_POINT('',(-52.1234703131944,29.7268821954854,38.989));
#179946=CARTESIAN_POINT('Origin',(5.49031038273072E-15,0.,38.989));
#179947=CARTESIAN_POINT('',(-52.5345762957641,29.9642343451583,38.989));
#179948=CARTESIAN_POINT('',(45.2006711678726,-26.4632370872589,38.989));
#179949=CARTESIAN_POINT('',(-52.5348628873914,29.9637318777514,38.9889999995772));
#179950=CARTESIAN_POINT('Origin',(5.49031038273072E-15,0.,38.989));
#179951=CARTESIAN_POINT('',(-55.1203859400878,24.8893571715243,38.9889999997818));
#179952=CARTESIAN_POINT('Origin',(5.49031038273072E-15,0.,38.989));
#179953=CARTESIAN_POINT('',(-55.1206239907494,24.8888299712414,38.989));
#179954=CARTESIAN_POINT('Origin',(5.49031038273072E-15,0.,38.989));
#179955=CARTESIAN_POINT('',(-54.6874511544107,24.6959689987792,38.989));
#179956=CARTESIAN_POINT('Origin',(5.49031038273072E-15,0.,38.989));
#179957=CARTESIAN_POINT('',(-52.6757649139393,30.0450834959841,39.2708017080178));
#179958=CARTESIAN_POINT('',(-52.5348628867552,29.9637318773886,38.989));
#179959=CARTESIAN_POINT('',(-55.2690209155615,24.9555320243583,39.2708017078546));
#179960=CARTESIAN_POINT('Origin',(5.52999282761009E-15,0.,39.2708017080178));
#179961=CARTESIAN_POINT('',(-55.2690209153038,24.9555320242419,39.2708017080178));
#179962=CARTESIAN_POINT('Origin',(60.71525,0.,39.3978017080178));
#179963=CARTESIAN_POINT('',(-55.4702140717965,25.0444775033952,39.3978017080178));
#179964=CARTESIAN_POINT('',(-52.8659816883957,30.1555713378342,39.3978017080178));
#179965=CARTESIAN_POINT('Origin',(5.5478765747851E-15,0.,39.3978017080178));
#179966=CARTESIAN_POINT('',(-52.9969317578285,30.2311753956717,39.3978017080178));
#179967=CARTESIAN_POINT('',(45.3776874999996,-26.5654375142634,39.3978017080178));
#179968=CARTESIAN_POINT('',(-55.6083495590299,25.1059793847706,39.3978017080178));
#179969=CARTESIAN_POINT('Origin',(5.5478765747851E-15,0.,39.3978017080178));
#179970=CARTESIAN_POINT('',(-55.4706982733005,25.0446930837942,39.3978017080178));
#179971=CARTESIAN_POINT('Origin',(5.5478765747851E-15,0.,39.3978017080178));
#179972=CARTESIAN_POINT('',(-55.8095395120005,25.1949317875305,39.2708017080178));
#179973=CARTESIAN_POINT('',(-53.1871522508548,30.3416565763596,39.2708017081757));
#179974=CARTESIAN_POINT('Origin',(5.52999282761008E-15,0.,39.2708017080178));
#179975=CARTESIAN_POINT('',(-53.3280557328683,30.4230055008172,38.9890000005756));
#179976=CARTESIAN_POINT('',(-53.1871522506172,30.3416565762241,39.2708017080178));
#179977=CARTESIAN_POINT('',(-53.328337071051,30.4225123424716,38.989));
#179978=CARTESIAN_POINT('Origin',(5.49031038273072E-15,0.,38.989));
#179979=CARTESIAN_POINT('',(-55.9579395562864,25.2616268796461,38.989));
#179980=CARTESIAN_POINT('Origin',(5.49031038273072E-15,0.,38.989));
#179981=CARTESIAN_POINT('',(-55.9581731633343,25.2611094010726,38.9890000005754));
#179982=CARTESIAN_POINT('Origin',(5.49031038273072E-15,0.,38.989));
#179983=CARTESIAN_POINT('',(-55.9581731636435,25.2611094011952,38.989));
#179984=CARTESIAN_POINT('Origin',(62.2224557307631,0.,38.989));
#179985=CARTESIAN_POINT('',(-53.7394427993284,30.6598643453579,38.989));
#179986=CARTESIAN_POINT('',(46.5080917980719,-27.2180767400485,38.989));
#179987=CARTESIAN_POINT('',(-56.3916032444849,25.4547063934088,38.989));
#179988=CARTESIAN_POINT('Origin',(5.49031038273072E-15,0.,38.989));
#179989=CARTESIAN_POINT('',(-55.9584195472773,25.2618405854039,38.989));
#179990=CARTESIAN_POINT('Origin',(5.57972911860581E-15,0.,39.624));
#179991=CARTESIAN_POINT('Origin',(-52.1234719996032,29.7268774036442,39.6240070731883));
#179992=CARTESIAN_POINT('Origin',(-54.6869571488948,24.6957545189383,39.6240070731883));
#179993=CARTESIAN_POINT('Origin',(5.57972911860581E-15,0.,39.624));
#179994=CARTESIAN_POINT('Origin',(-53.7724806104361,30.6789000092871,39.5552135207983));
#179995=CARTESIAN_POINT('Origin',(-56.4264221855586,25.4702454951994,39.5552117598846));
#179996=CARTESIAN_POINT('Origin',(5.51210908043506E-15,0.,39.1438017080178));
#179997=CARTESIAN_POINT('Origin',(-53.0106482050727,30.239137420935,39.1711625381359));
#179998=CARTESIAN_POINT('Origin',(-55.6227672661403,25.112358217853,39.1712173702612));
#179999=CARTESIAN_POINT('Origin',(5.51210908043507E-15,0.,39.1438017080178));
#180000=CARTESIAN_POINT('Origin',(-52.8523506794951,30.1476490842054,39.1712175859386));
#180001=CARTESIAN_POINT('Origin',(-55.4557066902174,25.0380683404998,39.1711627526719));
#180002=CARTESIAN_POINT('Origin',(60.4792282238308,0.,38.989));
#180003=CARTESIAN_POINT('',(-56.9687879773465,18.8441205405524,38.989));
#180004=CARTESIAN_POINT('',(-54.9452378026827,24.1156489724281,38.989));
#180005=CARTESIAN_POINT('Origin',(5.49031038273072E-15,0.,38.989));
#180006=CARTESIAN_POINT('',(-55.3789017591237,24.3087286055924,38.989));
#180007=CARTESIAN_POINT('',(50.3447265545023,-22.7624634345049,38.989));
#180008=CARTESIAN_POINT('',(-55.3791342586262,24.3081989337722,38.9889999995772));
#180009=CARTESIAN_POINT('Origin',(5.49031038273072E-15,0.,38.989));
#180010=CARTESIAN_POINT('',(-57.420076955426,18.9913614316849,38.9889999997818));
#180011=CARTESIAN_POINT('Origin',(5.49031038273072E-15,0.,38.989));
#180012=CARTESIAN_POINT('',(-57.4202585945858,18.9908122363905,38.989));
#180013=CARTESIAN_POINT('Origin',(5.49031038273072E-15,0.,38.989));
#180014=CARTESIAN_POINT('',(-56.9692992632924,18.8442866674266,38.989));
#180015=CARTESIAN_POINT('Origin',(5.49031038273072E-15,0.,38.989));
#180016=CARTESIAN_POINT('',(-55.5277679687681,24.3743766270218,39.2708017080178));
#180017=CARTESIAN_POINT('',(-55.3791342579556,24.3081989334778,38.989));
#180018=CARTESIAN_POINT('',(-57.5748148486259,19.041637186177,39.2708017078546));
#180019=CARTESIAN_POINT('Origin',(5.52999282761009E-15,0.,39.2708017080178));
#180020=CARTESIAN_POINT('',(-57.5748148483574,19.0416371860882,39.2708017080178));
#180021=CARTESIAN_POINT('Origin',(60.71525,0.,39.3978017080178));
#180022=CARTESIAN_POINT('',(-57.7842031819381,19.109065001132,39.3978017080178));
#180023=CARTESIAN_POINT('',(-55.7284918401496,24.4643761377921,39.3978017080178));
#180024=CARTESIAN_POINT('Origin',(5.5478765747851E-15,0.,39.3978017080178));
#180025=CARTESIAN_POINT('',(-55.8666273273831,24.5258780191675,39.3978017080178));
#180026=CARTESIAN_POINT('',(50.541702139688,-22.850162615335,39.3978017080178));
#180027=CARTESIAN_POINT('',(-57.9280106456674,19.1557908785629,39.3978017080178));
#180028=CARTESIAN_POINT('Origin',(5.5478765747851E-15,0.,39.3978017080178));
#180029=CARTESIAN_POINT('',(-57.7847072652235,19.1092287877199,39.3978017080178));
#180030=CARTESIAN_POINT('Origin',(5.5478765747851E-15,0.,39.3978017080178));
#180031=CARTESIAN_POINT('',(-58.1373965169892,19.2232259141444,39.2708017080178));
#180032=CARTESIAN_POINT('',(-56.0673542006828,24.6158705165698,39.2708017081757));
#180033=CARTESIAN_POINT('Origin',(5.52999282761008E-15,0.,39.2708017080178));
#180034=CARTESIAN_POINT('',(-56.2159890767409,24.6820453786636,38.9890000005756));
#180035=CARTESIAN_POINT('',(-56.0673542004324,24.6158705164598,39.2708017080178));
#180036=CARTESIAN_POINT('',(-56.2162173246396,24.6815255140431,38.989));
#180037=CARTESIAN_POINT('Origin',(5.49031038273072E-15,0.,38.989));
#180038=CARTESIAN_POINT('',(-58.2919551457915,19.2740436149889,38.989));
#180039=CARTESIAN_POINT('Origin',(5.49031038273072E-15,0.,38.989));
#180040=CARTESIAN_POINT('',(-58.2921333818755,19.2735045526314,38.9890000005754));
#180041=CARTESIAN_POINT('Origin',(5.49031038273072E-15,0.,38.989));
#180042=CARTESIAN_POINT('',(-58.2921333821958,19.2735045527211,38.989));
#180043=CARTESIAN_POINT('Origin',(62.2224557307631,0.,38.989));
#180044=CARTESIAN_POINT('',(-56.649881012838,24.8746050278057,38.989));
#180045=CARTESIAN_POINT('',(51.799563747336,-23.4101986852082,38.989));
#180046=CARTESIAN_POINT('',(-58.7434254837931,19.4207352200705,38.989));
#180047=CARTESIAN_POINT('Origin',(5.49031038273072E-15,0.,38.989));
#180048=CARTESIAN_POINT('',(-58.2924548456759,19.2742059773236,38.989));
#180049=CARTESIAN_POINT('Origin',(5.57972911860581E-15,0.,39.624));
#180050=CARTESIAN_POINT('Origin',(-54.9452389789694,24.1156440305594,39.6240070731884));
#180051=CARTESIAN_POINT('Origin',(-56.9687855447422,18.8441250001661,39.6240070731883));
#180052=CARTESIAN_POINT('Origin',(5.57972911860581E-15,0.,39.624));
#180053=CARTESIAN_POINT('Origin',(-56.6847276080567,24.8900830207528,39.5552135207981));
#180054=CARTESIAN_POINT('Origin',(-58.7796779614985,19.4325496266337,39.5552117598791));
#180055=CARTESIAN_POINT('Origin',(5.51210908043506E-15,0.,39.1438017080178));
#180056=CARTESIAN_POINT('Origin',(-55.8811008927611,24.5323626684723,39.1711625381393));
#180057=CARTESIAN_POINT('Origin',(-57.94301614069,19.1606277069624,39.171217370263));
#180058=CARTESIAN_POINT('Origin',(5.51210908043507E-15,0.,39.1438017080178));
#180059=CARTESIAN_POINT('Origin',(-55.7141074023455,24.4579221115113,39.1712175859368));
#180060=CARTESIAN_POINT('Origin',(-57.7691053333631,19.1042073826016,39.1711627526768));
#180061=CARTESIAN_POINT('Origin',(60.4792282238308,0.,38.989));
#180062=CARTESIAN_POINT('',(-58.6264539577983,12.7860306150456,38.989));
#180063=CARTESIAN_POINT('',(-57.1650137687745,18.240199652705,38.989));
#180064=CARTESIAN_POINT('Origin',(5.49031038273072E-15,0.,38.989));
#180065=CARTESIAN_POINT('',(-57.6164843860301,18.3868913484952,38.989));
#180066=CARTESIAN_POINT('',(54.6058629360811,-18.0763596539233,38.989));
#180067=CARTESIAN_POINT('',(-57.616660246095,18.386340275457,38.988999999577));
#180068=CARTESIAN_POINT('Origin',(5.49031038273072E-15,0.,38.989));
#180069=CARTESIAN_POINT('',(-59.090661591717,12.8852923618021,38.9889999997818));
#180070=CARTESIAN_POINT('Origin',(5.49031038273072E-15,0.,38.989));
#180071=CARTESIAN_POINT('',(-59.0907848292983,12.8847271885947,38.989));
#180072=CARTESIAN_POINT('Origin',(5.49031038273072E-15,0.,38.989));
#180073=CARTESIAN_POINT('',(-58.6269798078532,12.7861423879252,38.989));
#180074=CARTESIAN_POINT('Origin',(5.49031038273072E-15,0.,38.989));
#180075=CARTESIAN_POINT('',(-57.7713971777986,18.4366189870677,39.2708017080178));
#180076=CARTESIAN_POINT('',(-57.616660245397,18.3863402752342,38.989));
#180077=CARTESIAN_POINT('',(-59.2498070619041,12.9191181862652,39.2708017078546));
#180078=CARTESIAN_POINT('Origin',(5.52999282761009E-15,0.,39.2708017080178));
#180079=CARTESIAN_POINT('',(-59.2498070616278,12.919118186205,39.2708017080178));
#180080=CARTESIAN_POINT('Origin',(60.71525,0.,39.3978017080178));
#180081=CARTESIAN_POINT('',(-59.4650964698965,12.9642895838875,39.3978017080178));
#180082=CARTESIAN_POINT('',(-57.9804289733662,18.5051441132846,39.3978017080178));
#180083=CARTESIAN_POINT('Origin',(5.5478765747851E-15,0.,39.3978017080178));
#180084=CARTESIAN_POINT('',(-58.1242364370955,18.5518699907155,39.3978017080178));
#180085=CARTESIAN_POINT('',(54.8193466381475,-18.1457247135494,39.3978017080178));
#180086=CARTESIAN_POINT('',(-59.6130003254554,12.9957275188828,39.3978017080178));
#180087=CARTESIAN_POINT('Origin',(5.5478765747851E-15,0.,39.3978017080178));
#180088=CARTESIAN_POINT('',(-59.4656149121213,12.9643997821842,39.3978017080178));
#180089=CARTESIAN_POINT('Origin',(5.5478765747851E-15,0.,39.3978017080178));
#180090=CARTESIAN_POINT('',(-59.8282880397054,13.0409063549243,39.2708017080178));
#180091=CARTESIAN_POINT('',(-58.33327048504,18.6203878281983,39.2708017081757));
#180092=CARTESIAN_POINT('Origin',(5.52999282761008E-15,0.,39.2708017080178));
#180093=CARTESIAN_POINT('',(-58.4880082803367,18.6706636022913,38.9890000005756));
#180094=CARTESIAN_POINT('',(-58.3332704847794,18.6203878281152,39.2708017080178));
#180095=CARTESIAN_POINT('',(-58.4881809372196,18.6701227271415,38.989));
#180096=CARTESIAN_POINT('Origin',(5.49031038273072E-15,0.,38.989));
#180097=CARTESIAN_POINT('',(-59.9873118763435,13.075289895133,38.989));
#180098=CARTESIAN_POINT('Origin',(5.49031038273072E-15,0.,38.989));
#180099=CARTESIAN_POINT('',(-59.9874327886717,13.0747351550715,38.9890000005754));
#180100=CARTESIAN_POINT('Origin',(5.49031038273072E-15,0.,38.989));
#180101=CARTESIAN_POINT('',(-59.9874327889996,13.0747351551272,38.989));
#180102=CARTESIAN_POINT('Origin',(62.2224557307631,0.,38.989));
#180103=CARTESIAN_POINT('',(-58.9396512752212,18.8168143322231,38.989));
#180104=CARTESIAN_POINT('',(56.1826270286323,-18.588681363906,38.989));
#180105=CARTESIAN_POINT('',(-60.4516424606488,13.1739864076111,38.989));
#180106=CARTESIAN_POINT('Origin',(5.49031038273072E-15,0.,38.989));
#180107=CARTESIAN_POINT('',(-59.987825810305,13.0753991351687,38.989));
#180108=CARTESIAN_POINT('Origin',(5.57972911860581E-15,0.,39.624));
#180109=CARTESIAN_POINT('Origin',(-57.1650144220515,18.2401946149529,39.6240070731884));
#180110=CARTESIAN_POINT('Origin',(-58.6264520046767,12.7860353045054,39.6240070731884));
#180111=CARTESIAN_POINT('Origin',(5.57972911860581E-15,0.,39.624));
#180112=CARTESIAN_POINT('Origin',(-58.9759248679604,18.8285650740589,39.5552135208012));
#180113=CARTESIAN_POINT('Origin',(-60.4889312852515,13.1819466778347,39.5552117598777));
#180114=CARTESIAN_POINT('Origin',(5.51210908043506E-15,0.,39.1438017080178));
#180115=CARTESIAN_POINT('Origin',(-58.1393085451906,18.5568062168846,39.1711625381322));
#180116=CARTESIAN_POINT('Origin',(-59.6284292050461,12.998969349295,39.171217370263));
#180117=CARTESIAN_POINT('Origin',(5.51210908043507E-15,0.,39.1438017080178));
#180118=CARTESIAN_POINT('Origin',(-57.9654487055671,18.5002290260152,39.1712175859384));
#180119=CARTESIAN_POINT('Origin',(-59.4495735695152,12.9610367308092,39.1711627526779));
#180120=CARTESIAN_POINT('Origin',(60.4792282238308,0.,38.989));
#180121=CARTESIAN_POINT('',(-59.6417962403142,6.58785426247137,38.989));
#180122=CARTESIAN_POINT('',(-58.7584778814675,12.1649068885796,38.989));
#180123=CARTESIAN_POINT('Origin',(5.49031038273072E-15,0.,38.989));
#180124=CARTESIAN_POINT('',(-59.2228087529787,12.2636034620794,38.989));
#180125=CARTESIAN_POINT('',(57.7988642628859,-12.6101209950214,38.989));
#180126=CARTESIAN_POINT('',(-59.2229260468456,12.2630370254946,38.9889999995771));
#180127=CARTESIAN_POINT('Origin',(5.49031038273072E-15,0.,38.989));
#180128=CARTESIAN_POINT('',(-60.1138365740932,6.6380493323826,38.9889999997818));
#180129=CARTESIAN_POINT('Origin',(5.49031038273072E-15,0.,38.989));
#180130=CARTESIAN_POINT('',(-60.1139000598793,6.63747437341819,38.989));
#180131=CARTESIAN_POINT('Origin',(5.49031038273072E-15,0.,38.989));
#180132=CARTESIAN_POINT('',(-59.6423308931549,6.58791045674932,38.989));
#180133=CARTESIAN_POINT('Origin',(5.49031038273072E-15,0.,38.989));
#180134=CARTESIAN_POINT('',(-59.382070869907,12.2968658913807,39.2708017080178));
#180135=CARTESIAN_POINT('',(-59.2229260461284,12.2630370253461,38.989));
#180136=CARTESIAN_POINT('',(-60.2756459901929,6.6550546240054,39.2708017078546));
#180137=CARTESIAN_POINT('Origin',(5.52999282761009E-15,0.,39.2708017080178));
#180138=CARTESIAN_POINT('',(-60.2756459899118,6.65505462397437,39.2708017080178));
#180139=CARTESIAN_POINT('Origin',(60.71525,0.,39.3978017080178));
#180140=CARTESIAN_POINT('',(-60.4944777170593,6.67747469700988,39.3978017080178));
#180141=CARTESIAN_POINT('',(-59.5971203935658,12.3431658574215,39.3978017080178));
#180142=CARTESIAN_POINT('Origin',(5.5478765747851E-15,0.,39.3978017080178));
#180143=CARTESIAN_POINT('',(-59.7450242491247,12.3746037924168,39.3978017080178));
#180144=CARTESIAN_POINT('',(58.0246834617327,-12.6581203474874,39.3978017080178));
#180145=CARTESIAN_POINT('',(-60.6448574988554,6.69328024897497,39.3978017080178));
#180146=CARTESIAN_POINT('Origin',(5.5478765747851E-15,0.,39.3978017080178));
#180147=CARTESIAN_POINT('',(-60.4950048380619,6.67753009965975,39.3978017080178));
#180148=CARTESIAN_POINT('Origin',(5.5478765747851E-15,0.,39.3978017080178));
#180149=CARTESIAN_POINT('',(-60.8636883187844,6.71570789669452,39.2708017080178));
#180150=CARTESIAN_POINT('',(-59.9600752509414,12.4208962742145,39.2708017081757));
#180151=CARTESIAN_POINT('Origin',(5.52999282761008E-15,0.,39.2708017080178));
#180152=CARTESIAN_POINT('',(-60.1192206258105,12.4547221284048,38.9890000005756));
#180153=CARTESIAN_POINT('',(-59.9600752506736,12.4208962741591,39.2708017080178));
#180154=CARTESIAN_POINT('',(-60.1193358000127,12.454166168667,38.989));
#180155=CARTESIAN_POINT('Origin',(5.49031038273072E-15,0.,38.989));
#180156=CARTESIAN_POINT('',(-61.0254350648262,6.73328056300561,38.989));
#180157=CARTESIAN_POINT('Origin',(5.49031038273072E-15,0.,38.989));
#180158=CARTESIAN_POINT('',(-61.0254973286579,6.7327162230884,38.9890000005754));
#180159=CARTESIAN_POINT('Origin',(5.49031038273072E-15,0.,38.989));
#180160=CARTESIAN_POINT('',(-61.0254973289898,6.73271622310951,38.989));
#180161=CARTESIAN_POINT('Origin',(62.2224557307631,0.,38.989));
#180162=CARTESIAN_POINT('',(-60.5836663843181,12.5528626811452,38.989));
#180163=CARTESIAN_POINT('',(59.4667368016499,-12.964638247165,38.989));
#180164=CARTESIAN_POINT('',(-61.4975385923862,6.78290064323603,38.989));
#180165=CARTESIAN_POINT('Origin',(5.49031038273072E-15,0.,38.989));
#180166=CARTESIAN_POINT('',(-61.0259576020967,6.73333548388583,38.989));
#180167=CARTESIAN_POINT('Origin',(5.57972911860581E-15,0.,39.624));
#180168=CARTESIAN_POINT('Origin',(-58.7584780045773,12.1649018101389,39.6240070731883));
#180169=CARTESIAN_POINT('Origin',(-59.6417947880741,6.58785913039868,39.6240070731883));
#180170=CARTESIAN_POINT('Origin',(5.57972911860581E-15,0.,39.624));
#180171=CARTESIAN_POINT('Origin',(-60.620969553508,12.5607574282799,39.5552135208001));
#180172=CARTESIAN_POINT('Origin',(-61.5354552197157,6.78691956273326,39.5552117598845));
#180173=CARTESIAN_POINT('Origin',(5.51210908043506E-15,0.,39.1438017080178));
#180174=CARTESIAN_POINT('Origin',(-59.7605297667705,12.3779375131251,39.1711625381321));
#180175=CARTESIAN_POINT('Origin',(-60.6605407209825,6.6948915632276,39.1712173702665));
#180176=CARTESIAN_POINT('Origin',(5.51210908043507E-15,0.,39.1438017080178));
#180177=CARTESIAN_POINT('Origin',(-59.5817084227212,12.339843559887,39.17121758594));
#180178=CARTESIAN_POINT('Origin',(-60.4786998370186,6.67586224832373,39.1711627526745));
#180179=CARTESIAN_POINT('Origin',(60.4792282238308,0.,38.989));
#180180=CARTESIAN_POINT('',(-60.003690522373,0.3175,38.989));
#180181=CARTESIAN_POINT('',(-59.7081718144892,5.95633285891252,38.989));
#180182=CARTESIAN_POINT('Origin',(5.49031038273072E-15,0.,38.989));
#180183=CARTESIAN_POINT('',(-60.1802756340603,6.00595296980914,38.989));
#180184=CARTESIAN_POINT('',(59.785232315514,-6.60293000146475,38.989));
#180185=CARTESIAN_POINT('',(-60.1803330766331,6.00537737567553,38.9889999995772));
#180186=CARTESIAN_POINT('Origin',(5.49031038273072E-15,0.,38.989));
#180187=CARTESIAN_POINT('',(-60.4783917833346,0.318078445375988,38.9889999997818));
#180188=CARTESIAN_POINT('Origin',(5.49031038273072E-15,0.,38.989));
#180189=CARTESIAN_POINT('',(-60.478394821762,0.317500000025284,38.989));
#180190=CARTESIAN_POINT('Origin',(5.49031038273072E-15,0.,38.989));
#180191=CARTESIAN_POINT('',(-60.004228120231,0.3175,38.989));
#180192=CARTESIAN_POINT('Origin',(5.49031038273072E-15,0.,38.989));
#180193=CARTESIAN_POINT('',(-60.3421421670675,6.02238575970318,39.2708017080178));
#180194=CARTESIAN_POINT('',(-60.1803330759045,6.00537737560282,38.989));
#180195=CARTESIAN_POINT('',(-60.6410923275232,0.31807689062485,39.2708017078546));
#180196=CARTESIAN_POINT('Origin',(5.52999282761009E-15,0.,39.2708017080178));
#180197=CARTESIAN_POINT('',(-60.6410923272405,0.318076890623367,39.2708017080178));
#180198=CARTESIAN_POINT('Origin',(60.71525,0.,39.3978017080178));
#180199=CARTESIAN_POINT('',(-60.8610688070707,0.3175,39.3978017080178));
#180200=CARTESIAN_POINT('',(-60.5608532912343,6.04595329345103,39.3978017080178));
#180201=CARTESIAN_POINT('Origin',(5.5478765747851E-15,0.,39.3978017080178));
#180202=CARTESIAN_POINT('',(-60.7112330730303,6.06175884541612,39.3978017080178));
#180203=CARTESIAN_POINT('',(60.0186752706391,-6.62746584474133,39.3978017080178));
#180204=CARTESIAN_POINT('',(-61.0122769227456,0.3175,39.3978017080178));
#180205=CARTESIAN_POINT('Origin',(5.5478765747851E-15,0.,39.3978017080178));
#180206=CARTESIAN_POINT('',(-60.8615988316031,0.3175,39.3978017080178));
#180207=CARTESIAN_POINT('Origin',(5.5478765747851E-15,0.,39.3978017080178));
#180208=CARTESIAN_POINT('',(-61.2322532920972,0.316930737395914,39.2708017080178));
#180209=CARTESIAN_POINT('',(-60.9299448849411,6.0853187814108,39.2708017081757));
#180210=CARTESIAN_POINT('Origin',(5.52999282761008E-15,0.,39.2708017080178));
#180211=CARTESIAN_POINT('',(-61.0917542093523,6.10232411256129,38.9890000005756));
#180212=CARTESIAN_POINT('',(-60.929944884669,6.08531878138362,39.2708017080178));
#180213=CARTESIAN_POINT('',(-61.0918106390011,6.10175915944675,38.989));
#180214=CARTESIAN_POINT('Origin',(5.49031038273072E-15,0.,38.989));
#180215=CARTESIAN_POINT('',(-61.3949508163453,0.3175,38.989));
#180216=CARTESIAN_POINT('Origin',(5.49031038273072E-15,0.,38.989));
#180217=CARTESIAN_POINT('',(-61.394953749505,0.316932243253257,38.9890000005754));
#180218=CARTESIAN_POINT('Origin',(5.49031038273072E-15,0.,38.989));
#180219=CARTESIAN_POINT('',(-61.3949537498373,0.31693224323956,38.989));
#180220=CARTESIAN_POINT('Origin',(62.2224557307631,0.,38.989));
#180221=CARTESIAN_POINT('',(-61.5639141665611,6.15137923967718,38.989));
#180222=CARTESIAN_POINT('',(61.5094129706996,-6.78414869068793,38.989));
#180223=CARTESIAN_POINT('',(-61.8696548221181,0.3175,38.989));
#180224=CARTESIAN_POINT('Origin',(5.49031038273072E-15,0.,38.989));
#180225=CARTESIAN_POINT('',(-61.3954762318973,0.3175,38.989));
#180226=CARTESIAN_POINT('Origin',(5.57972911860581E-15,0.,39.624));
#180227=CARTESIAN_POINT('Origin',(-59.7081714060829,5.95632779542356,39.6240070731883));
#180228=CARTESIAN_POINT('Origin',(-60.0036895869254,0.317504993060722,39.6240070731883));
#180229=CARTESIAN_POINT('Origin',(5.57972911860581E-15,0.,39.624));
#180230=CARTESIAN_POINT('Origin',(-61.6018382108737,6.15533149561012,39.5552135207994));
#180231=CARTESIAN_POINT('Origin',(-61.9077838296762,0.317533536648604,39.5552117598821));
#180232=CARTESIAN_POINT('Origin',(5.51210908043506E-15,0.,39.1438017080178));
#180233=CARTESIAN_POINT('Origin',(-60.7270021185293,6.06345353572164,39.17116253813));
#180234=CARTESIAN_POINT('Origin',(-61.0280426587373,0.317463144196525,39.1712173702556));
#180235=CARTESIAN_POINT('Origin',(5.51210908043507E-15,0.,39.1438017080178));
#180236=CARTESIAN_POINT('Origin',(-60.5451784741237,6.04426018543771,39.1712175859386));
#180237=CARTESIAN_POINT('Origin',(-60.8452088131251,0.317545622030734,39.1711627526739));
#180238=CARTESIAN_POINT('Origin',(60.4792282238308,0.,38.989));
#180239=CARTESIAN_POINT('',(-59.7081718144893,-5.95633285891171,38.989));
#180240=CARTESIAN_POINT('',(-60.003690522373,-0.3175,38.989));
#180241=CARTESIAN_POINT('Origin',(5.49031038273072E-15,0.,38.989));
#180242=CARTESIAN_POINT('',(-60.4783948217626,-0.317500000025261,38.989));
#180243=CARTESIAN_POINT('',(60.4792282238308,-0.3175,38.989));
#180244=CARTESIAN_POINT('',(-60.4783917836889,-0.318078445377852,38.9889999995772));
#180245=CARTESIAN_POINT('Origin',(5.49031038273072E-15,0.,38.989));
#180246=CARTESIAN_POINT('',(-60.1803330762807,-6.00537737563954,38.9889999997818));
#180247=CARTESIAN_POINT('Origin',(5.49031038273072E-15,0.,38.989));
#180248=CARTESIAN_POINT('',(-60.1802756340597,-6.00595296980823,38.989));
#180249=CARTESIAN_POINT('Origin',(5.49031038273072E-15,0.,38.989));
#180250=CARTESIAN_POINT('',(-59.7087064673299,-5.95638905318966,38.989));
#180251=CARTESIAN_POINT('Origin',(5.49031038273072E-15,0.,38.989));
#180252=CARTESIAN_POINT('',(-60.6410923272405,-0.318076890623366,39.2708017080178));
#180253=CARTESIAN_POINT('',(-60.4783917829566,-0.318078445374005,38.989));
#180254=CARTESIAN_POINT('',(-60.3421421673489,-6.02238575973044,39.2708017078546));
#180255=CARTESIAN_POINT('Origin',(5.52999282761009E-15,0.,39.2708017080178));
#180256=CARTESIAN_POINT('',(-60.3421421670675,-6.02238575970236,39.2708017080178));
#180257=CARTESIAN_POINT('Origin',(60.71525,0.,39.3978017080178));
#180258=CARTESIAN_POINT('',(-60.5608532912344,-6.04595329345021,39.3978017080178));
#180259=CARTESIAN_POINT('',(-60.8610688070707,-0.3175,39.3978017080178));
#180260=CARTESIAN_POINT('Origin',(5.5478765747851E-15,0.,39.3978017080178));
#180261=CARTESIAN_POINT('',(-61.0122769227456,-0.3175,39.3978017080178));
#180262=CARTESIAN_POINT('',(60.71525,-0.3175,39.3978017080178));
#180263=CARTESIAN_POINT('',(-60.7112330730304,-6.0617588454153,39.3978017080178));
#180264=CARTESIAN_POINT('Origin',(5.5478765747851E-15,0.,39.3978017080178));
#180265=CARTESIAN_POINT('',(-60.5613804122369,-6.04600869610007,39.3978017080178));
#180266=CARTESIAN_POINT('Origin',(5.5478765747851E-15,0.,39.3978017080178));
#180267=CARTESIAN_POINT('',(-60.9299448846691,-6.0853187813828,39.2708017080178));
#180268=CARTESIAN_POINT('',(-61.2322532923707,-0.31693073739733,39.2708017081757));
#180269=CARTESIAN_POINT('Origin',(5.52999282761008E-15,0.,39.2708017080178));
#180270=CARTESIAN_POINT('',(-61.3949537495049,-0.31693224325326,38.9890000005756));
#180271=CARTESIAN_POINT('',(-61.2322532920972,-0.316930737395914,39.2708017080178));
#180272=CARTESIAN_POINT('',(-61.3949508163453,-0.3175,38.989));
#180273=CARTESIAN_POINT('Origin',(5.49031038273072E-15,0.,38.989));
#180274=CARTESIAN_POINT('',(-61.0918106390012,-6.10175915944593,38.989));
#180275=CARTESIAN_POINT('Origin',(5.49031038273072E-15,0.,38.989));
#180276=CARTESIAN_POINT('',(-61.0917542093524,-6.10232411256048,38.9890000005754));
#180277=CARTESIAN_POINT('Origin',(5.49031038273072E-15,0.,38.989));
#180278=CARTESIAN_POINT('',(-61.0917542096815,-6.10232411260883,38.989));
#180279=CARTESIAN_POINT('Origin',(62.2224557307631,0.,38.989));
#180280=CARTESIAN_POINT('',(-61.8696548221181,-0.3175,38.989));
#180281=CARTESIAN_POINT('',(62.2224557307631,-0.3175,38.989));
#180282=CARTESIAN_POINT('',(-61.5639141665612,-6.15137923967635,38.989));
#180283=CARTESIAN_POINT('Origin',(5.49031038273072E-15,0.,38.989));
#180284=CARTESIAN_POINT('',(-61.0923331762718,-6.10181408032615,38.989));
#180285=CARTESIAN_POINT('Origin',(5.57972911860581E-15,0.,39.624));
#180286=CARTESIAN_POINT('Origin',(-60.0036895869254,-0.317504993060547,
39.6240070731883));
#180287=CARTESIAN_POINT('Origin',(-59.708171406083,-5.95632779542259,39.6240070731883));
#180288=CARTESIAN_POINT('Origin',(5.57972911860581E-15,0.,39.624));
#180289=CARTESIAN_POINT('Origin',(-61.9077842377874,-0.317533537011564,
39.5552135207981));
#180290=CARTESIAN_POINT('Origin',(-61.6018378049611,-6.15533145331103,39.5552117598819));
#180291=CARTESIAN_POINT('Origin',(5.51210908043506E-15,0.,39.1438017080178));
#180292=CARTESIAN_POINT('Origin',(-61.028136727137,-0.317462907478496,39.1711625381301));
#180293=CARTESIAN_POINT('Origin',(-60.726908590193,-6.0634434674746,39.1712173702598));
#180294=CARTESIAN_POINT('Origin',(5.51210908043507E-15,0.,39.1438017080178));
#180295=CARTESIAN_POINT('Origin',(-60.845302880271,-0.31754536844547,39.1712175859354));
#180296=CARTESIAN_POINT('Origin',(-60.5450849487951,-6.04425010054802,39.1711627526745));
#180297=CARTESIAN_POINT('Origin',(60.4792282238308,0.,38.989));
#180298=CARTESIAN_POINT('',(-58.7584778814677,-12.1649068885788,38.989));
#180299=CARTESIAN_POINT('',(-59.6417962403143,-6.58785426247057,38.989));
#180300=CARTESIAN_POINT('Origin',(5.49031038273072E-15,0.,38.989));
#180301=CARTESIAN_POINT('',(-60.1139000598801,-6.63747437341743,38.989));
#180302=CARTESIAN_POINT('',(59.8516078896891,5.9714085979051,38.989));
#180303=CARTESIAN_POINT('',(-60.1138365744455,-6.63804933242069,38.9889999995772));
#180304=CARTESIAN_POINT('Origin',(5.49031038273072E-15,0.,38.989));
#180305=CARTESIAN_POINT('',(-59.2229260464987,-12.2630370254219,38.9889999997818));
#180306=CARTESIAN_POINT('Origin',(5.49031038273072E-15,0.,38.989));
#180307=CARTESIAN_POINT('',(-59.2228087529783,-12.2636034620785,38.989));
#180308=CARTESIAN_POINT('Origin',(5.49031038273072E-15,0.,38.989));
#180309=CARTESIAN_POINT('',(-58.7590037315226,-12.1650186614584,38.989));
#180310=CARTESIAN_POINT('Origin',(5.49031038273072E-15,0.,38.989));
#180311=CARTESIAN_POINT('',(-60.2756459899119,-6.65505462397356,39.2708017080178));
#180312=CARTESIAN_POINT('',(-60.1138365737176,-6.6380493323403,38.989));
#180313=CARTESIAN_POINT('',(-59.382070870184,-12.2968658914373,39.2708017078546));
#180314=CARTESIAN_POINT('Origin',(5.52999282761009E-15,0.,39.2708017080178));
#180315=CARTESIAN_POINT('',(-59.3820708699071,-12.2968658913799,39.2708017080178));
#180316=CARTESIAN_POINT('Origin',(60.71525,0.,39.3978017080178));
#180317=CARTESIAN_POINT('',(-59.597120393566,-12.3431658574207,39.3978017080178));
#180318=CARTESIAN_POINT('',(-60.4944777170594,-6.67747469700906,39.3978017080178));
#180319=CARTESIAN_POINT('Origin',(5.5478765747851E-15,0.,39.3978017080178));
#180320=CARTESIAN_POINT('',(-60.6448574988555,-6.69328024897415,39.3978017080178));
#180321=CARTESIAN_POINT('',(60.0850508448142,5.99594444118168,39.3978017080178));
#180322=CARTESIAN_POINT('',(-59.7450242491248,-12.374603792416,39.3978017080178));
#180323=CARTESIAN_POINT('Origin',(5.5478765747851E-15,0.,39.3978017080178));
#180324=CARTESIAN_POINT('',(-59.5976388357907,-12.3432760557174,39.3978017080178));
#180325=CARTESIAN_POINT('Origin',(5.5478765747851E-15,0.,39.3978017080178));
#180326=CARTESIAN_POINT('',(-59.9600752506738,-12.4208962741583,39.2708017080178));
#180327=CARTESIAN_POINT('',(-60.8636883190563,-6.71570789672369,39.2708017081757));
#180328=CARTESIAN_POINT('Origin',(5.52999282761008E-15,0.,39.2708017080178));
#180329=CARTESIAN_POINT('',(-61.0254973286579,-6.73271622308757,38.9890000005756));
#180330=CARTESIAN_POINT('',(-60.8636883187845,-6.7157078966937,39.2708017080178));
#180331=CARTESIAN_POINT('',(-61.0254350648263,-6.73328056300478,38.989));
#180332=CARTESIAN_POINT('Origin',(5.49031038273072E-15,0.,38.989));
#180333=CARTESIAN_POINT('',(-60.1193358000129,-12.4541661686662,38.989));
#180334=CARTESIAN_POINT('Origin',(5.49031038273072E-15,0.,38.989));
#180335=CARTESIAN_POINT('',(-60.1192206258108,-12.454722128404,38.9890000005754));
#180336=CARTESIAN_POINT('Origin',(5.49031038273072E-15,0.,38.989));
#180337=CARTESIAN_POINT('',(-60.119220626133,-12.4547221284865,38.989));
#180338=CARTESIAN_POINT('Origin',(62.2224557307631,0.,38.989));
#180339=CARTESIAN_POINT('',(-61.4975385923863,-6.7829006432352,38.989));
#180340=CARTESIAN_POINT('',(61.5757885448748,6.15262728712825,38.989));
#180341=CARTESIAN_POINT('',(-60.5836663843182,-12.5528626811443,38.989));
#180342=CARTESIAN_POINT('Origin',(5.49031038273072E-15,0.,38.989));
#180343=CARTESIAN_POINT('',(-60.1198497339744,-12.454275408702,38.989));
#180344=CARTESIAN_POINT('Origin',(5.57972911860581E-15,0.,39.624));
#180345=CARTESIAN_POINT('Origin',(-59.6417947880742,-6.58785913039772,39.6240070731883));
#180346=CARTESIAN_POINT('Origin',(-58.7584780045775,-12.1649018101379,39.6240070731883));
#180347=CARTESIAN_POINT('Origin',(5.57972911860581E-15,0.,39.624));
#180348=CARTESIAN_POINT('Origin',(-61.5354556255515,-6.78691960575365,39.555213520804));
#180349=CARTESIAN_POINT('Origin',(-60.620969154242,-12.5607573437815,39.555211759881));
#180350=CARTESIAN_POINT('Origin',(5.51210908043506E-15,0.,39.1438017080178));
#180351=CARTESIAN_POINT('Origin',(-60.6606342988047,-6.69490116063027,39.1711625381324));
#180352=CARTESIAN_POINT('Origin',(-59.7604378032096,-12.3779177236595,39.171217370261));
#180353=CARTESIAN_POINT('Origin',(5.51210908043507E-15,0.,39.1438017080178));
#180354=CARTESIAN_POINT('Origin',(-60.478793415361,-6.67587182882111,39.1712175859386));
#180355=CARTESIAN_POINT('Origin',(-59.5816164638925,-12.3398237541832,39.1711627526759));
#180356=CARTESIAN_POINT('Origin',(60.4792282238308,0.,38.989));
#180357=CARTESIAN_POINT('',(-57.1650137687748,-18.2401996527042,38.989));
#180358=CARTESIAN_POINT('',(-58.6264539577984,-12.7860306150448,38.989));
#180359=CARTESIAN_POINT('Origin',(5.49031038273072E-15,0.,38.989));
#180360=CARTESIAN_POINT('',(-59.0907848292991,-12.884727188594,38.989));
#180361=CARTESIAN_POINT('',(57.9308881865556,11.9889972685547,38.989));
#180362=CARTESIAN_POINT('',(-59.0906615920626,-12.8852923618766,38.9889999995776));
#180363=CARTESIAN_POINT('Origin',(5.49031038273072E-15,0.,38.989));
#180364=CARTESIAN_POINT('',(-57.6166602457573,-18.3863402753484,38.9889999997818));
#180365=CARTESIAN_POINT('Origin',(5.49031038273072E-15,0.,38.989));
#180366=CARTESIAN_POINT('',(-57.6164843860298,-18.3868913484942,38.989));
#180367=CARTESIAN_POINT('Origin',(5.49031038273072E-15,0.,38.989));
#180368=CARTESIAN_POINT('',(-57.1655250547207,-18.2403657795784,38.989));
#180369=CARTESIAN_POINT('Origin',(5.49031038273072E-15,0.,38.989));
#180370=CARTESIAN_POINT('',(-59.249807061628,-12.9191181862042,39.2708017080178));
#180371=CARTESIAN_POINT('',(-59.0906615913478,-12.8852923617207,38.989));
#180372=CARTESIAN_POINT('',(-57.7713971780681,-18.4366189871529,39.2708017078546));
#180373=CARTESIAN_POINT('Origin',(5.52999282761009E-15,0.,39.2708017080178));
#180374=CARTESIAN_POINT('',(-57.7713971777988,-18.4366189870669,39.2708017080178));
#180375=CARTESIAN_POINT('Origin',(60.71525,0.,39.3978017080178));
#180376=CARTESIAN_POINT('',(-57.9804289733665,-18.5051441132838,39.3978017080178));
#180377=CARTESIAN_POINT('',(-59.4650964698967,-12.9642895838867,39.3978017080178));
#180378=CARTESIAN_POINT('Origin',(5.5478765747851E-15,0.,39.3978017080178));
#180379=CARTESIAN_POINT('',(-59.6130003254556,-12.995727518882,39.3978017080178));
#180380=CARTESIAN_POINT('',(58.1567073854023,12.0369966210207,39.3978017080178));
#180381=CARTESIAN_POINT('',(-58.1242364370958,-18.5518699907147,39.3978017080178));
#180382=CARTESIAN_POINT('Origin',(5.5478765747851E-15,0.,39.3978017080178));
#180383=CARTESIAN_POINT('',(-57.9809330566518,-18.5053078998717,39.3978017080178));
#180384=CARTESIAN_POINT('Origin',(5.5478765747851E-15,0.,39.3978017080178));
#180385=CARTESIAN_POINT('',(-58.3332704847797,-18.6203878281144,39.2708017080178));
#180386=CARTESIAN_POINT('',(-59.8282880399728,-13.0409063549817,39.2708017081757));
#180387=CARTESIAN_POINT('Origin',(5.52999282761008E-15,0.,39.2708017080178));
#180388=CARTESIAN_POINT('',(-59.9874327886718,-13.0747351550707,38.9890000005756));
#180389=CARTESIAN_POINT('',(-59.8282880397056,-13.0409063549235,39.2708017080178));
#180390=CARTESIAN_POINT('',(-59.9873118763436,-13.0752898951321,38.989));
#180391=CARTESIAN_POINT('Origin',(5.49031038273072E-15,0.,38.989));
#180392=CARTESIAN_POINT('',(-58.4881809372199,-18.6701227271407,38.989));
#180393=CARTESIAN_POINT('Origin',(5.49031038273072E-15,0.,38.989));
#180394=CARTESIAN_POINT('',(-58.488008280337,-18.6706636022905,38.9890000005754));
#180395=CARTESIAN_POINT('Origin',(5.49031038273072E-15,0.,38.989));
#180396=CARTESIAN_POINT('',(-58.4880082806488,-18.6706636024062,38.989));
#180397=CARTESIAN_POINT('Origin',(62.2224557307631,0.,38.989));
#180398=CARTESIAN_POINT('',(-60.451642460649,-13.1739864076103,38.989));
#180399=CARTESIAN_POINT('',(59.5987607253196,12.3435145206982,38.989));
#180400=CARTESIAN_POINT('',(-58.9396512752214,-18.8168143322223,38.989));
#180401=CARTESIAN_POINT('Origin',(5.49031038273072E-15,0.,38.989));
#180402=CARTESIAN_POINT('',(-58.4886806371043,-18.6702850894754,38.989));
#180403=CARTESIAN_POINT('Origin',(5.57972911860581E-15,0.,39.624));
#180404=CARTESIAN_POINT('Origin',(-58.6264520046769,-12.7860353045044,39.6240070731883));
#180405=CARTESIAN_POINT('Origin',(-57.1650144220518,-18.240194614952,39.6240070731883));
#180406=CARTESIAN_POINT('Origin',(5.57972911860581E-15,0.,39.624));
#180407=CARTESIAN_POINT('Origin',(-60.488931684366,-13.1819467630401,39.5552135207985));
#180408=CARTESIAN_POINT('Origin',(-58.9759244797144,-18.8285649482878,39.5552117598814));
#180409=CARTESIAN_POINT('Origin',(5.51210908043506E-15,0.,39.1438017080178));
#180410=CARTESIAN_POINT('Origin',(-59.6285212670397,-12.9989886756685,39.1711625381335));
#180411=CARTESIAN_POINT('Origin',(-58.139219153978,-18.556776923018,39.171217370261));
#180412=CARTESIAN_POINT('Origin',(5.51210908043507E-15,0.,39.1438017080178));
#180413=CARTESIAN_POINT('Origin',(-59.4496656337937,-12.9610560404249,39.1712175859361));
#180414=CARTESIAN_POINT('Origin',(-57.9653593207593,-18.5001997164937,39.1711627526731));
#180415=CARTESIAN_POINT('Origin',(60.4792282238308,0.,38.989));
#180416=CARTESIAN_POINT('',(-54.945237802683,-24.1156489724274,38.989));
#180417=CARTESIAN_POINT('',(-56.9687879773467,-18.8441205405516,38.989));
#180418=CARTESIAN_POINT('Origin',(5.49031038273072E-15,0.,38.989));
#180419=CARTESIAN_POINT('',(-57.4202585945867,-18.9908122363899,38.989));
#180420=CARTESIAN_POINT('',(54.8020887275097,17.4724387660752,38.989));
#180421=CARTESIAN_POINT('',(-57.4200769557628,-18.9913614317954,38.9889999995771));
#180422=CARTESIAN_POINT('Origin',(5.49031038273072E-15,0.,38.989));
#180423=CARTESIAN_POINT('',(-55.3791342583021,-24.308198933629,38.9889999997818));
#180424=CARTESIAN_POINT('Origin',(5.49031038273072E-15,0.,38.989));
#180425=CARTESIAN_POINT('',(-55.3789017591235,-24.3087286055914,38.989));
#180426=CARTESIAN_POINT('Origin',(5.49031038273072E-15,0.,38.989));
#180427=CARTESIAN_POINT('',(-54.9457289227642,-24.1158676331754,38.989));
#180428=CARTESIAN_POINT('Origin',(5.49031038273072E-15,0.,38.989));
#180429=CARTESIAN_POINT('',(-57.5748148483577,-19.0416371860875,39.2708017080178));
#180430=CARTESIAN_POINT('',(-57.4200769550674,-18.9913614315654,38.989));
#180431=CARTESIAN_POINT('',(-55.5277679690273,-24.3743766271347,39.2708017078546));
#180432=CARTESIAN_POINT('Origin',(5.52999282761009E-15,0.,39.2708017080178));
#180433=CARTESIAN_POINT('',(-55.5277679687684,-24.3743766270211,39.2708017080178));
#180434=CARTESIAN_POINT('Origin',(60.71525,0.,39.3978017080178));
#180435=CARTESIAN_POINT('',(-55.7284918401499,-24.4643761377914,39.3978017080178));
#180436=CARTESIAN_POINT('',(-57.7842031819384,-19.1090650011312,39.3978017080178));
#180437=CARTESIAN_POINT('Origin',(5.5478765747851E-15,0.,39.3978017080178));
#180438=CARTESIAN_POINT('',(-57.9280106456677,-19.1557908785622,39.3978017080178));
#180439=CARTESIAN_POINT('',(55.0155724295761,17.5418038257013,39.3978017080178));
#180440=CARTESIAN_POINT('',(-55.8666273273834,-24.5258780191668,39.3978017080178));
#180441=CARTESIAN_POINT('Origin',(5.5478765747851E-15,0.,39.3978017080178));
#180442=CARTESIAN_POINT('',(-55.728976041654,-24.4645917181904,39.3978017080178));
#180443=CARTESIAN_POINT('Origin',(5.5478765747851E-15,0.,39.3978017080178));
#180444=CARTESIAN_POINT('',(-56.0673542004327,-24.6158705164591,39.2708017080178));
#180445=CARTESIAN_POINT('',(-58.1373965172491,-19.2232259142295,39.2708017081757));
#180446=CARTESIAN_POINT('Origin',(5.52999282761008E-15,0.,39.2708017080178));
#180447=CARTESIAN_POINT('',(-58.2921333818757,-19.2735045526306,38.9890000005756));
#180448=CARTESIAN_POINT('',(-58.1373965169894,-19.2232259141436,39.2708017080178));
#180449=CARTESIAN_POINT('',(-58.2919551457918,-19.2740436149881,38.989));
#180450=CARTESIAN_POINT('Origin',(5.49031038273072E-15,0.,38.989));
#180451=CARTESIAN_POINT('',(-56.2162173246399,-24.6815255140423,38.989));
#180452=CARTESIAN_POINT('Origin',(5.49031038273072E-15,0.,38.989));
#180453=CARTESIAN_POINT('',(-56.2159890767413,-24.6820453786628,38.9890000005754));
#180454=CARTESIAN_POINT('Origin',(5.49031038273072E-15,0.,38.989));
#180455=CARTESIAN_POINT('',(-56.2159890770393,-24.6820453788105,38.989));
#180456=CARTESIAN_POINT('Origin',(62.2224557307631,0.,38.989));
#180457=CARTESIAN_POINT('',(-58.7434254837933,-19.4207352200698,38.989));
#180458=CARTESIAN_POINT('',(56.3788528200609,17.9847604760579,38.989));
#180459=CARTESIAN_POINT('',(-56.6498810128383,-24.8746050278049,38.989));
#180460=CARTESIAN_POINT('Origin',(5.49031038273072E-15,0.,38.989));
#180461=CARTESIAN_POINT('',(-56.2166973156307,-24.6817392198001,38.989));
#180462=CARTESIAN_POINT('Origin',(5.57972911860581E-15,0.,39.624));
#180463=CARTESIAN_POINT('Origin',(-56.9687855447425,-18.8441250001651,39.6240070731883));
#180464=CARTESIAN_POINT('Origin',(-54.9452389789698,-24.1156440305586,39.6240070731883));
#180465=CARTESIAN_POINT('Origin',(5.57972911860581E-15,0.,39.624));
#180466=CARTESIAN_POINT('Origin',(-58.7796783495205,-19.4325497530928,39.5552135207989));
#180467=CARTESIAN_POINT('Origin',(-56.6847272350812,-24.8900828550894,39.5552117598828));
#180468=CARTESIAN_POINT('Origin',(5.51210908043506E-15,0.,39.1438017080178));
#180469=CARTESIAN_POINT('Origin',(-57.9431056782044,-19.1606565505634,39.1711625381365));
#180470=CARTESIAN_POINT('Origin',(-55.8810150532827,-24.5323241911531,39.1712173702617));
#180471=CARTESIAN_POINT('Origin',(5.51210908043507E-15,0.,39.1438017080178));
#180472=CARTESIAN_POINT('Origin',(-57.7691948748979,-19.1042362097727,39.171217585939));
#180473=CARTESIAN_POINT('Origin',(-55.7140215708744,-24.4578836192969,39.1711627526724));
#180474=CARTESIAN_POINT('Origin',(60.4792282238308,0.,38.989));
#180475=CARTESIAN_POINT('',(-52.1234703131948,-29.7268821954847,38.989));
#180476=CARTESIAN_POINT('',(-54.6869600343299,-24.6957503380304,38.989));
#180477=CARTESIAN_POINT('Origin',(5.49031038273072E-15,0.,38.989));
#180478=CARTESIAN_POINT('',(-55.1206239907504,-24.8888299712409,38.989));
#180479=CARTESIAN_POINT('',(50.603004322856,22.1823620689013,38.989));
#180480=CARTESIAN_POINT('',(-55.1203859404106,-24.8893571716692,38.9889999995774));
#180481=CARTESIAN_POINT('Origin',(5.49031038273072E-15,0.,38.989));
#180482=CARTESIAN_POINT('',(-52.534862887084,-29.9637318775751,38.9889999997818));
#180483=CARTESIAN_POINT('Origin',(5.49031038273072E-15,0.,38.989));
#180484=CARTESIAN_POINT('',(-52.5345762957639,-29.9642343451572,38.989));
#180485=CARTESIAN_POINT('Origin',(5.49031038273072E-15,0.,38.989));
#180486=CARTESIAN_POINT('',(-52.1239358865968,-29.7271509944136,38.989));
#180487=CARTESIAN_POINT('Origin',(5.49031038273072E-15,0.,38.989));
#180488=CARTESIAN_POINT('',(-55.2690209153042,-24.9555320242412,39.2708017080178));
#180489=CARTESIAN_POINT('',(-55.1203859397436,-24.889357171368,38.989));
#180490=CARTESIAN_POINT('',(-52.6757649141853,-30.0450834961234,39.2708017078546));
#180491=CARTESIAN_POINT('Origin',(5.52999282761009E-15,0.,39.2708017080178));
#180492=CARTESIAN_POINT('',(-52.6757649139398,-30.0450834959834,39.2708017080178));
#180493=CARTESIAN_POINT('Origin',(60.71525,0.,39.3978017080178));
#180494=CARTESIAN_POINT('',(-52.8659816883961,-30.1555713378335,39.3978017080178));
#180495=CARTESIAN_POINT('',(-55.4702140717968,-25.0444775033944,39.3978017080178));
#180496=CARTESIAN_POINT('Origin',(5.5478765747851E-15,0.,39.3978017080178));
#180497=CARTESIAN_POINT('',(-55.6083495590303,-25.1059793847698,39.3978017080178));
#180498=CARTESIAN_POINT('',(50.7999799080417,22.2700612497314,39.3978017080178));
#180499=CARTESIAN_POINT('',(-52.9969317578289,-30.2311753956709,39.3978017080178));
#180500=CARTESIAN_POINT('Origin',(5.5478765747851E-15,0.,39.3978017080178));
#180501=CARTESIAN_POINT('',(-52.8664407031058,-30.1558363500997,39.3978017080178));
#180502=CARTESIAN_POINT('Origin',(5.5478765747851E-15,0.,39.3978017080178));
#180503=CARTESIAN_POINT('',(-53.1871522506177,-30.3416565762233,39.2708017080178));
#180504=CARTESIAN_POINT('',(-55.8095395122501,-25.1949317876423,39.2708017081757));
#180505=CARTESIAN_POINT('Origin',(5.52999282761008E-15,0.,39.2708017080178));
#180506=CARTESIAN_POINT('',(-55.9581731633346,-25.2611094010718,38.9890000005756));
#180507=CARTESIAN_POINT('',(-55.8095395120008,-25.1949317875298,39.2708017080178));
#180508=CARTESIAN_POINT('',(-55.9579395562868,-25.2616268796454,38.989));
#180509=CARTESIAN_POINT('Origin',(5.49031038273072E-15,0.,38.989));
#180510=CARTESIAN_POINT('',(-53.3283370710514,-30.4225123424708,38.989));
#180511=CARTESIAN_POINT('Origin',(5.49031038273072E-15,0.,38.989));
#180512=CARTESIAN_POINT('',(-53.3280557328688,-30.4230055008165,38.9890000005754));
#180513=CARTESIAN_POINT('Origin',(5.49031038273072E-15,0.,38.989));
#180514=CARTESIAN_POINT('',(-53.3280557331497,-30.4230055009945,38.989));
#180515=CARTESIAN_POINT('Origin',(62.2224557307631,0.,38.989));
#180516=CARTESIAN_POINT('',(-56.3916032444852,-25.454706393408,38.989));
#180517=CARTESIAN_POINT('',(52.0578415156897,22.8300973196046,38.989));
#180518=CARTESIAN_POINT('',(-53.7394427993288,-30.6598643453572,38.989));
#180519=CARTESIAN_POINT('Origin',(5.49031038273072E-15,0.,38.989));
#180520=CARTESIAN_POINT('',(-53.3287920942669,-30.4227750502468,38.989));
#180521=CARTESIAN_POINT('Origin',(5.57972911860581E-15,0.,39.624));
#180522=CARTESIAN_POINT('Origin',(-54.6869571488952,-24.6957545189373,39.6240070731883));
#180523=CARTESIAN_POINT('Origin',(-52.1234719996037,-29.7268774036434,39.6240070731883));
#180524=CARTESIAN_POINT('Origin',(5.57972911860581E-15,0.,39.624));
#180525=CARTESIAN_POINT('Origin',(-56.4264225582403,-25.4702456615252,39.5552135207993));
#180526=CARTESIAN_POINT('Origin',(-53.7724802568185,-30.6788998055495,39.5552117598812));
#180527=CARTESIAN_POINT('Origin',(5.51210908043506E-15,0.,39.1438017080178));
#180528=CARTESIAN_POINT('Origin',(-55.6228532981808,-25.1123962626642,39.1711625381337));
#180529=CARTESIAN_POINT('Origin',(-53.0105668578087,-30.2390901817308,39.1712173702625));
#180530=CARTESIAN_POINT('Origin',(5.51210908043507E-15,0.,39.1438017080178));
#180531=CARTESIAN_POINT('Origin',(-55.4557927279719,-25.0381063693876,39.1712175859413));
#180532=CARTESIAN_POINT('Origin',(-52.852269341752,-30.1476018310227,39.1711627526721));
#180533=CARTESIAN_POINT('Origin',(60.4792282238308,0.,38.989));
#180534=CARTESIAN_POINT('',(-48.7306271754178,-35.0124214764582,38.989));
#180535=CARTESIAN_POINT('',(-51.8059703131948,-30.2768083268878,38.989));
#180536=CARTESIAN_POINT('Origin',(5.49031038273072E-15,0.,38.989));
#180537=CARTESIAN_POINT('',(-52.2170762957392,-30.5141604766044,38.989));
#180538=CARTESIAN_POINT('',(45.5181711678734,25.9133109558554,38.989));
#180539=CARTESIAN_POINT('',(-52.2167844420139,-30.5146599059376,38.9889999995773));
#180540=CARTESIAN_POINT('Origin',(5.49031038273072E-15,0.,38.989));
#180541=CARTESIAN_POINT('',(-49.1150085644482,-35.2909759047566,38.9889999997818));
#180542=CARTESIAN_POINT('Origin',(5.49031038273072E-15,0.,38.989));
#180543=CARTESIAN_POINT('',(-49.1146710209412,-35.2914456628184,38.989));
#180544=CARTESIAN_POINT('Origin',(5.49031038273072E-15,0.,38.989));
#180545=CARTESIAN_POINT('',(-48.731062101221,-35.0127374685508,38.989));
#180546=CARTESIAN_POINT('Origin',(5.49031038273072E-15,0.,38.989));
#180547=CARTESIAN_POINT('',(-52.3576880233164,-30.5960088312566,39.2708017080178));
#180548=CARTESIAN_POINT('',(-52.2167844413817,-30.5146599055682,38.989));
#180549=CARTESIAN_POINT('',(-49.2466351558311,-35.3866101429907,39.2708017078546));
#180550=CARTESIAN_POINT('Origin',(5.52999282761009E-15,0.,39.2708017080178));
#180551=CARTESIAN_POINT('',(-49.2466351556015,-35.3866101428257,39.2708017080178));
#180552=CARTESIAN_POINT('Origin',(60.71525,0.,39.3978017080178));
#180553=CARTESIAN_POINT('',(-49.4242607783462,-35.5163757878393,39.3978017080178));
#180554=CARTESIAN_POINT('',(-52.5484816883961,-30.7054974692366,39.3978017080178));
#180555=CARTESIAN_POINT('Origin',(5.5478765747851E-15,0.,39.3978017080178));
#180556=CARTESIAN_POINT('',(-52.6794317578289,-30.781101527074,39.3978017080178));
#180557=CARTESIAN_POINT('',(45.6951875000003,26.0155113828598,39.3978017080178));
#180558=CARTESIAN_POINT('',(-49.5465907136146,-35.6052536882599,39.3978017080178));
#180559=CARTESIAN_POINT('Origin',(5.5478765747851E-15,0.,39.3978017080178));
#180560=CARTESIAN_POINT('',(-49.4246895772004,-35.5166873284428,39.3978017080178));
#180561=CARTESIAN_POINT('Origin',(5.5478765747851E-15,0.,39.3978017080178));
#180562=CARTESIAN_POINT('',(-49.7242207306177,-35.7350130971387,39.2708017080178));
#180563=CARTESIAN_POINT('',(-52.8702215134579,-30.8905967160113,39.2708017081757));
#180564=CARTESIAN_POINT('Origin',(5.52999282761008E-15,0.,39.2708017080178));
#180565=CARTESIAN_POINT('',(-53.0111234896155,-30.9719482486879,38.9890000005756));
#180566=CARTESIAN_POINT('',(-52.8702215132218,-30.8905967158733,39.2708017080178));
#180567=CARTESIAN_POINT('',(-53.0108370710514,-30.9724384738739,38.989));
#180568=CARTESIAN_POINT('Origin',(5.49031038273072E-15,0.,38.989));
#180569=CARTESIAN_POINT('',(-49.8561803968405,-35.8301837593552,38.989));
#180570=CARTESIAN_POINT('Origin',(5.49031038273072E-15,0.,38.989));
#180571=CARTESIAN_POINT('',(-49.8558490507739,-35.83064480828,38.9890000005754));
#180572=CARTESIAN_POINT('Origin',(5.49031038273072E-15,0.,38.989));
#180573=CARTESIAN_POINT('',(-49.8558490510346,-35.8306448084864,38.989));
#180574=CARTESIAN_POINT('Origin',(62.2224557307631,0.,38.989));
#180575=CARTESIAN_POINT('',(-53.4219427993288,-31.2097904767603,38.989));
#180576=CARTESIAN_POINT('',(46.8255917980726,26.668150608645,38.989));
#180577=CARTESIAN_POINT('',(-50.2402240048085,-36.1092077731526,38.989));
#180578=CARTESIAN_POINT('Origin',(5.49031038273072E-15,0.,38.989));
#180579=CARTESIAN_POINT('',(-49.8566054669511,-35.830492590868,38.989));
#180580=CARTESIAN_POINT('Origin',(5.57972911860581E-15,0.,39.624));
#180581=CARTESIAN_POINT('Origin',(-51.8059670065431,-30.2768121832812,39.6240070731883));
#180582=CARTESIAN_POINT('Origin',(-48.7306293534723,-35.0124168871448,39.6240070731883));
#180583=CARTESIAN_POINT('Origin',(5.57972911860581E-15,0.,39.624));
#180584=CARTESIAN_POINT('Origin',(-53.4549470734238,-31.2288842284974,39.5552135208002));
#180585=CARTESIAN_POINT('Origin',(-50.2710907322476,-36.1315923097635,39.5552117598819));
#180586=CARTESIAN_POINT('Origin',(5.51210908043506E-15,0.,39.1438017080178));
#180587=CARTESIAN_POINT('Origin',(-52.6931852975955,-30.788999306206,39.1711625381373));
#180588=CARTESIAN_POINT('Origin',(-49.559323798665,-35.6145503723402,39.1712173702594));
#180589=CARTESIAN_POINT('Origin',(5.51210908043507E-15,0.,39.1438017080178));
#180590=CARTESIAN_POINT('Origin',(-52.5348053110496,-30.6976537960616,39.1712175859388));
#180591=CARTESIAN_POINT('Origin',(-49.4114565896704,-35.5070166082983,39.1711627526735));
#180592=CARTESIAN_POINT('Origin',(60.4792282238308,0.,38.989));
#180593=CARTESIAN_POINT('',(-44.8038810887676,-39.9143573409155,38.989));
#180594=CARTESIAN_POINT('',(-48.3573835402121,-35.5261472678863,38.989));
#180595=CARTESIAN_POINT('Origin',(5.49031038273072E-15,0.,38.989));
#180596=CARTESIAN_POINT('',(-48.7414273857063,-35.8051714542878,38.989));
#180597=CARTESIAN_POINT('',(39.7707905934409,28.5027191556738,38.989));
#180598=CARTESIAN_POINT('',(-48.7410849262056,-35.8056376406735,38.9889999995771));
#180599=CARTESIAN_POINT('Origin',(5.49031038273072E-15,0.,38.989));
#180600=CARTESIAN_POINT('',(-45.157039930004,-40.231564614814,38.9889999997818));
#180601=CARTESIAN_POINT('Origin',(5.49031038273072E-15,0.,38.989));
#180602=CARTESIAN_POINT('',(-45.1566551325073,-40.231996516588,38.989));
#180603=CARTESIAN_POINT('Origin',(5.49031038273072E-15,0.,38.989));
#180604=CARTESIAN_POINT('',(-44.804280601834,-39.9147170640961,38.989));
#180605=CARTESIAN_POINT('Origin',(5.49031038273072E-15,0.,38.989));
#180606=CARTESIAN_POINT('',(-48.8727133447945,-35.9012693628902,39.2708017080178));
#180607=CARTESIAN_POINT('',(-48.7410849256153,-35.8056376402399,38.989));
#180608=CARTESIAN_POINT('',(-45.2779489571886,-40.3404336840071,39.2708017078546));
#180609=CARTESIAN_POINT('Origin',(5.52999282761009E-15,0.,39.2708017080178));
#180610=CARTESIAN_POINT('',(-45.2779489569775,-40.340433683819,39.2708017080178));
#180611=CARTESIAN_POINT('Origin',(60.71525,0.,39.3978017080178));
#180612=CARTESIAN_POINT('',(-45.4410373245174,-40.4880553924341,39.3978017080178));
#180613=CARTESIAN_POINT('',(-49.0510171431405,-36.0301015792674,39.3978017080178));
#180614=CARTESIAN_POINT('Origin',(5.5478765747851E-15,0.,39.3978017080178));
#180615=CARTESIAN_POINT('',(-49.1733470784089,-36.118979479688,39.3978017080178));
#180616=CARTESIAN_POINT('',(39.9252688514649,28.6149541797805,39.3978017080178));
#180617=CARTESIAN_POINT('',(-45.5534068532513,-40.589233370562,39.3978017080178));
#180618=CARTESIAN_POINT('Origin',(5.5478765747851E-15,0.,39.3978017080178));
#180619=CARTESIAN_POINT('',(-45.441431209506,-40.4884100480709,39.3978017080178));
#180620=CARTESIAN_POINT('Origin',(5.5478765747851E-15,0.,39.3978017080178));
#180621=CARTESIAN_POINT('',(-45.7165002428309,-40.7368493365295,39.2708017080178));
#180622=CARTESIAN_POINT('',(-49.3516463039591,-36.2478178024867,39.2708017081757));
#180623=CARTESIAN_POINT('Origin',(5.52999282761008E-15,0.,39.2708017080178));
#180624=CARTESIAN_POINT('',(-49.4832728536533,-36.3434519499945,38.9890000005756));
#180625=CARTESIAN_POINT('',(-49.3516463037387,-36.2478178023248,39.2708017080178));
#180626=CARTESIAN_POINT('',(-49.4829367616348,-36.3439095507833,38.989));
#180627=CARTESIAN_POINT('Origin',(5.49031038273072E-15,0.,38.989));
#180628=CARTESIAN_POINT('',(-45.8377889771253,-40.8452921850241,38.989));
#180629=CARTESIAN_POINT('Origin',(5.49031038273072E-15,0.,38.989));
#180630=CARTESIAN_POINT('',(-45.8374112534715,-40.8457160731795,38.9890000005754));
#180631=CARTESIAN_POINT('Origin',(5.49031038273072E-15,0.,38.989));
#180632=CARTESIAN_POINT('',(-45.8374112537093,-40.845716073412,38.989));
#180633=CARTESIAN_POINT('Origin',(62.2224557307631,0.,38.989));
#180634=CARTESIAN_POINT('',(-49.8669803696028,-36.6229335645807,38.989));
#180635=CARTESIAN_POINT('',(40.911747809259,29.3316730956003,38.989));
#180636=CARTESIAN_POINT('',(-46.1905628026487,-41.1629311642478,38.989));
#180637=CARTESIAN_POINT('Origin',(5.49031038273072E-15,0.,38.989));
#180638=CARTESIAN_POINT('',(-45.838179436974,-40.845643756651,38.989));
#180639=CARTESIAN_POINT('Origin',(5.57972911860581E-15,0.,39.624));
#180640=CARTESIAN_POINT('Origin',(-48.3573798485717,-35.5261507575148,39.6240070731883));
#180641=CARTESIAN_POINT('Origin',(-44.8038837346043,-39.9143530044115,39.6240070731883));
#180642=CARTESIAN_POINT('Origin',(5.57972911860581E-15,0.,39.624));
#180643=CARTESIAN_POINT('Origin',(-49.8978080023051,-36.6453726047975,39.5552135208017));
#180644=CARTESIAN_POINT('Origin',(-46.2189206177146,-41.188419527607,39.5552117598829));
#180645=CARTESIAN_POINT('Origin',(5.51210908043506E-15,0.,39.1438017080178));
#180646=CARTESIAN_POINT('Origin',(-49.1861997321292,-36.1282716303355,39.1711625381366));
#180647=CARTESIAN_POINT('Origin',(-45.5650984170296,-40.5998100962475,39.1712173702608));
#180648=CARTESIAN_POINT('Origin',(5.51210908043507E-15,0.,39.1438017080178));
#180649=CARTESIAN_POINT('Origin',(-49.0382355735267,-36.0208713038452,39.1712175859367));
#180650=CARTESIAN_POINT('Origin',(-45.4292815791796,-40.4774090812932,39.1711627526754));
#180651=CARTESIAN_POINT('Origin',(60.4792282238308,0.,38.989));
#180652=CARTESIAN_POINT('',(-40.386254305094,-44.3789831537294,38.989));
#180653=CARTESIAN_POINT('',(-44.3789831537298,-40.3862543050936,38.989));
#180654=CARTESIAN_POINT('Origin',(5.49031038273072E-15,0.,38.989));
#180655=CARTESIAN_POINT('',(-44.7317571974361,-40.7038934808041,38.989));
#180656=CARTESIAN_POINT('',(33.61296347236,29.8380098596982,38.989));
#180657=CARTESIAN_POINT('',(-44.7313678842178,-40.7043213166066,38.9889999995772));
#180658=CARTESIAN_POINT('Origin',(5.49031038273072E-15,0.,38.989));
#180659=CARTESIAN_POINT('',(-40.7043213163686,-44.7313678839554,38.9889999997818));
#180660=CARTESIAN_POINT('Origin',(5.49031038273072E-15,0.,38.989));
#180661=CARTESIAN_POINT('',(-40.7038934808041,-44.7317571974352,38.989));
#180662=CARTESIAN_POINT('Origin',(5.49031038273072E-15,0.,38.989));
#180663=CARTESIAN_POINT('',(-40.3866140282747,-44.3793826667957,38.989));
#180664=CARTESIAN_POINT('Origin',(5.49031038273072E-15,0.,38.989));
#180665=CARTESIAN_POINT('',(-44.8522789915944,-40.8131880745604,39.2708017080178));
#180666=CARTESIAN_POINT('',(-44.7313678836762,-40.7043213161137,38.989));
#180667=CARTESIAN_POINT('',(-40.8131880747511,-44.8522789918031,39.2708017078546));
#180668=CARTESIAN_POINT('Origin',(5.52999282761009E-15,0.,39.2708017080178));
#180669=CARTESIAN_POINT('',(-40.8131880745609,-44.8522789915939,39.2708017080178));
#180670=CARTESIAN_POINT('Origin',(60.71525,0.,39.3978017080178));
#180671=CARTESIAN_POINT('',(-40.9599523566127,-45.0161393894791,39.3978017080178));
#180672=CARTESIAN_POINT('',(-45.0161393894795,-40.9599523566123,39.3978017080178));
#180673=CARTESIAN_POINT('Origin',(5.5478765747851E-15,0.,39.3978017080178));
#180674=CARTESIAN_POINT('',(-45.1285089182135,-41.0611303347402,39.3978017080178));
#180675=CARTESIAN_POINT('',(33.743309857225,29.9553742717902,39.3978017080178));
#180676=CARTESIAN_POINT('',(-41.0611303347406,-45.1285089182131,39.3978017080178));
#180677=CARTESIAN_POINT('Origin',(5.5478765747851E-15,0.,39.3978017080178));
#180678=CARTESIAN_POINT('',(-40.9603070122495,-45.0165332744677,39.3978017080178));
#180679=CARTESIAN_POINT('Origin',(5.5478765747851E-15,0.,39.3978017080178));
#180680=CARTESIAN_POINT('',(-41.2079002115909,-45.2923641298555,39.2708017080178));
#180681=CARTESIAN_POINT('',(-45.2923641300582,-41.2079002117745,39.2708017081757));
#180682=CARTESIAN_POINT('Origin',(5.52999282761008E-15,0.,39.2708017080178));
#180683=CARTESIAN_POINT('',(-45.413273125266,-41.3167691863806,38.9890000005756));
#180684=CARTESIAN_POINT('',(-45.2923641298559,-41.2079002115905,39.2708017080178));
#180685=CARTESIAN_POINT('',(-45.4128910420874,-41.3171891492023,38.989));
#180686=CARTESIAN_POINT('Origin',(5.49031038273072E-15,0.,38.989));
#180687=CARTESIAN_POINT('',(-41.3171891492027,-45.412891042087,38.989));
#180688=CARTESIAN_POINT('Origin',(5.49031038273072E-15,0.,38.989));
#180689=CARTESIAN_POINT('',(-41.3167691863812,-45.4132731252656,38.9890000005754));
#180690=CARTESIAN_POINT('Origin',(5.49031038273072E-15,0.,38.989));
#180691=CARTESIAN_POINT('',(-41.3167691865933,-45.4132731255218,38.989));
#180692=CARTESIAN_POINT('Origin',(62.2224557307631,0.,38.989));
#180693=CARTESIAN_POINT('',(-45.7656648676108,-41.634828128426,38.989));
#180694=CARTESIAN_POINT('',(34.5756856720389,30.7048488218244,38.989));
#180695=CARTESIAN_POINT('',(-41.6348281284264,-45.7656648676104,38.989));
#180696=CARTESIAN_POINT('Origin',(5.49031038273072E-15,0.,38.989));
#180697=CARTESIAN_POINT('',(-41.3175407208296,-45.4132815019357,38.989));
#180698=CARTESIAN_POINT('Origin',(5.57972911860581E-15,0.,39.624));
#180699=CARTESIAN_POINT('Origin',(-44.378979117547,-40.386257389724,39.6240070731883));
#180700=CARTESIAN_POINT('Origin',(-40.3862573897246,-44.3789791175465,39.6240070731883));
#180701=CARTESIAN_POINT('Origin',(5.57972911860581E-15,0.,39.624));
#180702=CARTESIAN_POINT('Origin',(-45.7939781049219,-41.6603666103106,39.5552135207989));
#180703=CARTESIAN_POINT('Origin',(-41.6603663369578,-45.7939778018852,39.5552117598784));
#180704=CARTESIAN_POINT('Origin',(5.51210908043506E-15,0.,39.1438017080178));
#180705=CARTESIAN_POINT('Origin',(-45.1403198695221,-41.0717150501546,39.1711625381318));
#180706=CARTESIAN_POINT('Origin',(-41.0716522820273,-45.1402498046841,39.1712173702621));
#180707=CARTESIAN_POINT('Origin',(5.51210908043507E-15,0.,39.1438017080178));
#180708=CARTESIAN_POINT('Origin',(-45.0043926651424,-40.9494366077789,39.1712175859375));
#180709=CARTESIAN_POINT('Origin',(-40.9493738530243,-45.0043225899483,39.1711627526731));
#180710=CARTESIAN_POINT('Origin',(60.4792282238308,0.,38.989));
#180711=CARTESIAN_POINT('',(-35.5261472678868,-48.3573835402117,38.989));
#180712=CARTESIAN_POINT('',(-39.9143573409159,-44.8038810887672,38.989));
#180713=CARTESIAN_POINT('Origin',(5.49031038273072E-15,0.,38.989));
#180714=CARTESIAN_POINT('',(-40.2319965165888,-45.1566551325074,38.989));
#180715=CARTESIAN_POINT('',(27.3146622010794,29.8615093742684,38.989));
#180716=CARTESIAN_POINT('',(-40.2315646150499,-45.1570399302679,38.9889999995774));
#180717=CARTESIAN_POINT('Origin',(5.49031038273072E-15,0.,38.989));
#180718=CARTESIAN_POINT('',(-35.8056376404641,-48.7410849259196,38.9889999997818));
#180719=CARTESIAN_POINT('Origin',(5.49031038273072E-15,0.,38.989));
#180720=CARTESIAN_POINT('',(-35.8051714542879,-48.7414273857054,38.989));
#180721=CARTESIAN_POINT('Origin',(5.49031038273072E-15,0.,38.989));
#180722=CARTESIAN_POINT('',(-35.5264632599794,-48.357818466015,38.989));
#180723=CARTESIAN_POINT('Origin',(5.49031038273072E-15,0.,38.989));
#180724=CARTESIAN_POINT('',(-40.3404336838195,-45.2779489569771,39.2708017080178));
#180725=CARTESIAN_POINT('',(-40.231564614563,-45.1570399297214,38.989));
#180726=CARTESIAN_POINT('',(-35.9012693630581,-48.872713345022,39.2708017078546));
#180727=CARTESIAN_POINT('Origin',(5.52999282761009E-15,0.,39.2708017080178));
#180728=CARTESIAN_POINT('',(-35.9012693628907,-48.8727133447942,39.2708017080178));
#180729=CARTESIAN_POINT('Origin',(60.71525,0.,39.3978017080178));
#180730=CARTESIAN_POINT('',(-36.0301015792679,-49.0510171431402,39.3978017080178));
#180731=CARTESIAN_POINT('',(-40.4880553924345,-45.441037324517,39.3978017080178));
#180732=CARTESIAN_POINT('Origin',(5.5478765747851E-15,0.,39.3978017080178));
#180733=CARTESIAN_POINT('',(-40.5892333705625,-45.5534068532509,39.3978017080178));
#180734=CARTESIAN_POINT('',(27.4203375923837,29.9788737863604,39.3978017080178));
#180735=CARTESIAN_POINT('',(-36.1189794796885,-49.1733470784086,39.3978017080178));
#180736=CARTESIAN_POINT('Origin',(5.5478765747851E-15,0.,39.3978017080178));
#180737=CARTESIAN_POINT('',(-36.0304131198714,-49.0514459419943,39.3978017080178));
#180738=CARTESIAN_POINT('Origin',(5.5478765747851E-15,0.,39.3978017080178));
#180739=CARTESIAN_POINT('',(-36.2478178023253,-49.3516463037383,39.2708017080178));
#180740=CARTESIAN_POINT('',(-40.7368493367119,-45.7165002430347,39.2708017081757));
#180741=CARTESIAN_POINT('Origin',(5.52999282761008E-15,0.,39.2708017080178));
#180742=CARTESIAN_POINT('',(-40.8457160731799,-45.837411253471,38.9890000005756));
#180743=CARTESIAN_POINT('',(-40.7368493365299,-45.7165002428305,39.2708017080178));
#180744=CARTESIAN_POINT('',(-40.8452921850246,-45.8377889771249,38.989));
#180745=CARTESIAN_POINT('Origin',(5.49031038273072E-15,0.,38.989));
#180746=CARTESIAN_POINT('',(-36.3439095507838,-49.4829367616344,38.989));
#180747=CARTESIAN_POINT('Origin',(5.49031038273072E-15,0.,38.989));
#180748=CARTESIAN_POINT('',(-36.343451949995,-49.483272853653,38.9890000005754));
#180749=CARTESIAN_POINT('Origin',(5.49031038273072E-15,0.,38.989));
#180750=CARTESIAN_POINT('',(-36.3434519501792,-49.4832728539299,38.989));
#180751=CARTESIAN_POINT('Origin',(62.2224557307631,0.,38.989));
#180752=CARTESIAN_POINT('',(-41.1629311642483,-46.1905628026483,38.989));
#180753=CARTESIAN_POINT('',(28.0951675083328,30.7283483363946,38.989));
#180754=CARTESIAN_POINT('',(-36.6229335645812,-49.8669803696024,38.989));
#180755=CARTESIAN_POINT('Origin',(5.49031038273072E-15,0.,38.989));
#180756=CARTESIAN_POINT('',(-36.3442183822966,-49.483361831745,38.989));
#180757=CARTESIAN_POINT('Origin',(5.57972911860581E-15,0.,39.624));
#180758=CARTESIAN_POINT('Origin',(-39.9143530044121,-44.8038837346038,39.6240070731883));
#180759=CARTESIAN_POINT('Origin',(-35.5261507575154,-48.3573798485712,39.6240070731883));
#180760=CARTESIAN_POINT('Origin',(5.57972911860581E-15,0.,39.624));
#180761=CARTESIAN_POINT('Origin',(-41.1884198004145,-46.2189209212423,39.555213520803));
#180762=CARTESIAN_POINT('Origin',(-36.6453723646293,-49.8978076723474,39.5552117598808));
#180763=CARTESIAN_POINT('Origin',(5.51210908043506E-15,0.,39.1438017080178));
#180764=CARTESIAN_POINT('Origin',(-40.5998732162091,-45.5651681650783,39.1711625381351));
#180765=CARTESIAN_POINT('Origin',(-36.1282165298269,-49.1861234900555,39.1712173702626));
#180766=CARTESIAN_POINT('Origin',(5.51210908043507E-15,0.,39.1438017080178));
#180767=CARTESIAN_POINT('Origin',(-40.4774722129479,-45.4293513150148,39.1712175859345));
#180768=CARTESIAN_POINT('Origin',(-36.0208162177223,-49.03815932255,39.1711627526757));
#180769=CARTESIAN_POINT('Origin',(60.4792282238308,0.,38.989));
#180770=CARTESIAN_POINT('',(-30.2768083268883,-51.8059703131945,38.989));
#180771=CARTESIAN_POINT('',(-35.0124214764587,-48.7306271754175,38.989));
#180772=CARTESIAN_POINT('Origin',(5.49031038273072E-15,0.,38.989));
#180773=CARTESIAN_POINT('',(-35.2914456628193,-49.1146710209414,38.989));
#180774=CARTESIAN_POINT('',(21.1519223437074,28.5729602337852,38.989));
#180775=CARTESIAN_POINT('',(-35.2909759049637,-49.1150085647354,38.9889999995773));
#180776=CARTESIAN_POINT('Origin',(5.49031038273072E-15,0.,38.989));
#180777=CARTESIAN_POINT('',(-30.5146599057594,-52.2167844417077,38.9889999997818));
#180778=CARTESIAN_POINT('Origin',(5.49031038273072E-15,0.,38.989));
#180779=CARTESIAN_POINT('',(-30.5141604766047,-52.2170762957384,38.989));
#180780=CARTESIAN_POINT('Origin',(5.49031038273072E-15,0.,38.989));
#180781=CARTESIAN_POINT('',(-30.2770771258173,-51.8064358865965,38.989));
#180782=CARTESIAN_POINT('Origin',(5.49031038273072E-15,0.,38.989));
#180783=CARTESIAN_POINT('',(-35.3866101428262,-49.2466351556011,39.2708017080178));
#180784=CARTESIAN_POINT('',(-35.2909759045365,-49.1150085641409,38.989));
#180785=CARTESIAN_POINT('',(-30.5960088313997,-52.3576880235602,39.2708017078546));
#180786=CARTESIAN_POINT('Origin',(5.52999282761009E-15,0.,39.2708017080178));
#180787=CARTESIAN_POINT('',(-30.5960088312571,-52.3576880233161,39.2708017080178));
#180788=CARTESIAN_POINT('Origin',(60.71525,0.,39.3978017080178));
#180789=CARTESIAN_POINT('',(-30.7054974692372,-52.5484816883958,39.3978017080178));
#180790=CARTESIAN_POINT('',(-35.5163757878398,-49.4242607783459,39.3978017080178));
#180791=CARTESIAN_POINT('Origin',(5.5478765747851E-15,0.,39.3978017080178));
#180792=CARTESIAN_POINT('',(-35.6052536882604,-49.5465907136143,39.3978017080178));
#180793=CARTESIAN_POINT('',(21.2334658618526,28.6851952578919,39.3978017080178));
#180794=CARTESIAN_POINT('',(-30.7811015270746,-52.6794317578286,39.3978017080178));
#180795=CARTESIAN_POINT('Origin',(5.5478765747851E-15,0.,39.3978017080178));
#180796=CARTESIAN_POINT('',(-30.7057624815034,-52.5489407031055,39.3978017080178));
#180797=CARTESIAN_POINT('Origin',(5.5478765747851E-15,0.,39.3978017080178));
#180798=CARTESIAN_POINT('',(-30.8905967158739,-52.8702215132214,39.2708017080178));
#180799=CARTESIAN_POINT('',(-35.7350130972987,-49.7242207308394,39.2708017081757));
#180800=CARTESIAN_POINT('Origin',(5.52999282761008E-15,0.,39.2708017080178));
#180801=CARTESIAN_POINT('',(-35.8306448082804,-49.8558490507735,38.9890000005756));
#180802=CARTESIAN_POINT('',(-35.7350130971392,-49.7242207306173,39.2708017080178));
#180803=CARTESIAN_POINT('',(-35.8301837593557,-49.8561803968401,38.989));
#180804=CARTESIAN_POINT('Origin',(5.49031038273072E-15,0.,38.989));
#180805=CARTESIAN_POINT('',(-30.9724384738745,-53.0108370710511,38.989));
#180806=CARTESIAN_POINT('Origin',(5.49031038273072E-15,0.,38.989));
#180807=CARTESIAN_POINT('',(-30.9719482486884,-53.0111234896152,38.9890000005754));
#180808=CARTESIAN_POINT('Origin',(5.49031038273072E-15,0.,38.989));
#180809=CARTESIAN_POINT('',(-30.9719482488427,-53.0111234899098,38.989));
#180810=CARTESIAN_POINT('Origin',(62.2224557307631,0.,38.989));
#180811=CARTESIAN_POINT('',(-36.1092077731531,-50.2402240048081,38.989));
#180812=CARTESIAN_POINT('',(21.7541926348216,29.4019141737117,38.989));
#180813=CARTESIAN_POINT('',(-31.2097904767608,-53.4219427993285,38.989));
#180814=CARTESIAN_POINT('Origin',(5.49031038273072E-15,0.,38.989));
#180815=CARTESIAN_POINT('',(-30.9727011816504,-53.0112920942666,38.989));
#180816=CARTESIAN_POINT('Origin',(5.57972911860581E-15,0.,39.624));
#180817=CARTESIAN_POINT('Origin',(-35.0124168871455,-48.7306293534718,39.6240070731883));
#180818=CARTESIAN_POINT('Origin',(-30.276812183282,-51.8059670065426,39.6240070731883));
#180819=CARTESIAN_POINT('Origin',(5.57972911860581E-15,0.,39.624));
#180820=CARTESIAN_POINT('Origin',(-36.1315925493512,-50.2710910626307,39.5552135207972));
#180821=CARTESIAN_POINT('Origin',(-31.2288840241297,-53.4549467201703,39.5552117598825));
#180822=CARTESIAN_POINT('Origin',(5.51210908043506E-15,0.,39.1438017080178));
#180823=CARTESIAN_POINT('Origin',(-35.6146058558682,-49.55939976246,39.171162538136));
#180824=CARTESIAN_POINT('Origin',(-30.7889524770111,-52.6931037136134,39.1712173702653));
#180825=CARTESIAN_POINT('Origin',(5.51210908043507E-15,0.,39.1438017080178));
#180826=CARTESIAN_POINT('Origin',(-35.5070721047369,-49.4115325425342,39.171217585936));
#180827=CARTESIAN_POINT('Origin',(-30.6976069821036,-52.534723719719,39.1711627526727));
#180828=CARTESIAN_POINT('Origin',(60.4792282238308,0.,38.989));
#180829=CARTESIAN_POINT('',(-24.695750338031,-54.6869600343296,38.989));
#180830=CARTESIAN_POINT('',(-29.7268821954852,-52.1234703131945,38.989));
#180831=CARTESIAN_POINT('Origin',(5.49031038273072E-15,0.,38.989));
#180832=CARTESIAN_POINT('',(-29.9642343451581,-52.5345762957642,38.989));
#180833=CARTESIAN_POINT('',(15.3947701216595,26.0295240215573,38.989));
#180834=CARTESIAN_POINT('',(-29.9637318777512,-52.5348628873915,38.9889999995772));
#180835=CARTESIAN_POINT('Origin',(5.49031038273072E-15,0.,38.989));
#180836=CARTESIAN_POINT('',(-24.8893571715241,-55.1203859400878,38.9889999997818));
#180837=CARTESIAN_POINT('Origin',(5.49031038273072E-15,0.,38.989));
#180838=CARTESIAN_POINT('',(-24.8888299712412,-55.1206239907495,38.989));
#180839=CARTESIAN_POINT('Origin',(5.49031038273072E-15,0.,38.989));
#180840=CARTESIAN_POINT('',(-24.6959689987791,-54.6874511544108,38.989));
#180841=CARTESIAN_POINT('Origin',(5.49031038273072E-15,0.,38.989));
#180842=CARTESIAN_POINT('',(-30.0450834959839,-52.6757649139395,39.2708017080178));
#180843=CARTESIAN_POINT('',(-29.9637318773884,-52.5348628867553,38.989));
#180844=CARTESIAN_POINT('',(-24.9555320243581,-55.2690209155616,39.2708017078546));
#180845=CARTESIAN_POINT('Origin',(5.52999282761009E-15,0.,39.2708017080178));
#180846=CARTESIAN_POINT('',(-24.9555320242418,-55.2690209153039,39.2708017080178));
#180847=CARTESIAN_POINT('Origin',(60.71525,0.,39.3978017080178));
#180848=CARTESIAN_POINT('',(-25.044477503395,-55.4702140717966,39.3978017080178));
#180849=CARTESIAN_POINT('',(-30.155571337834,-52.8659816883958,39.3978017080178));
#180850=CARTESIAN_POINT('Origin',(5.5478765747851E-15,0.,39.3978017080178));
#180851=CARTESIAN_POINT('',(-30.2311753956715,-52.9969317578286,39.3978017080178));
#180852=CARTESIAN_POINT('',(15.4537755657018,26.1317244485617,39.3978017080178));
#180853=CARTESIAN_POINT('',(-25.1059793847704,-55.60834955903,39.3978017080178));
#180854=CARTESIAN_POINT('Origin',(5.5478765747851E-15,0.,39.3978017080178));
#180855=CARTESIAN_POINT('',(-25.0446930837941,-55.4706982733006,39.3978017080178));
#180856=CARTESIAN_POINT('Origin',(5.5478765747851E-15,0.,39.3978017080178));
#180857=CARTESIAN_POINT('',(-25.1949317875303,-55.8095395120006,39.2708017080178));
#180858=CARTESIAN_POINT('',(-30.3416565763594,-53.1871522508549,39.2708017081757));
#180859=CARTESIAN_POINT('Origin',(5.52999282761008E-15,0.,39.2708017080178));
#180860=CARTESIAN_POINT('',(-30.423005500817,-53.3280557328684,38.9890000005756));
#180861=CARTESIAN_POINT('',(-30.3416565762239,-53.1871522506173,39.2708017080178));
#180862=CARTESIAN_POINT('',(-30.4225123424714,-53.3283370710511,38.989));
#180863=CARTESIAN_POINT('Origin',(5.49031038273072E-15,0.,38.989));
#180864=CARTESIAN_POINT('',(-25.2616268796459,-55.9579395562865,38.989));
#180865=CARTESIAN_POINT('Origin',(5.49031038273072E-15,0.,38.989));
#180866=CARTESIAN_POINT('',(-25.2611094010724,-55.9581731633344,38.9890000005754));
#180867=CARTESIAN_POINT('Origin',(5.49031038273072E-15,0.,38.989));
#180868=CARTESIAN_POINT('',(-25.261109401195,-55.9581731636436,38.989));
#180869=CARTESIAN_POINT('Origin',(62.2224557307631,0.,38.989));
#180870=CARTESIAN_POINT('',(-30.6598643453577,-53.7394427993285,38.989));
#180871=CARTESIAN_POINT('',(15.8305769983926,26.7843636743469,38.989));
#180872=CARTESIAN_POINT('',(-25.4547063934086,-56.3916032444849,38.989));
#180873=CARTESIAN_POINT('Origin',(5.49031038273072E-15,0.,38.989));
#180874=CARTESIAN_POINT('',(-25.2618405854037,-55.9584195472774,38.989));
#180875=CARTESIAN_POINT('Origin',(5.57972911860581E-15,0.,39.624));
#180876=CARTESIAN_POINT('Origin',(-29.7268774036441,-52.1234719996033,39.6240070731883));
#180877=CARTESIAN_POINT('Origin',(-24.6957545189381,-54.6869571488949,39.6240070731883));
#180878=CARTESIAN_POINT('Origin',(5.57972911860581E-15,0.,39.624));
#180879=CARTESIAN_POINT('Origin',(-30.6789000092878,-53.7724806104346,39.5552135207999));
#180880=CARTESIAN_POINT('Origin',(-25.4702454952,-56.4264221855589,39.5552117598839));
#180881=CARTESIAN_POINT('Origin',(5.51210908043506E-15,0.,39.1438017080178));
#180882=CARTESIAN_POINT('Origin',(-30.2391374209327,-53.0106482050692,39.1711625381285));
#180883=CARTESIAN_POINT('Origin',(-25.1123582178529,-55.6227672661409,39.1712173702621));
#180884=CARTESIAN_POINT('Origin',(5.51210908043507E-15,0.,39.1438017080178));
#180885=CARTESIAN_POINT('Origin',(-30.1476490842061,-52.8523506794962,39.1712175859364));
#180886=CARTESIAN_POINT('Origin',(-25.0380683404975,-55.4557066902184,39.1711627526722));
#180887=CARTESIAN_POINT('Origin',(60.4792282238308,0.,38.989));
#180888=CARTESIAN_POINT('',(-18.8441205405522,-56.9687879773465,38.989));
#180889=CARTESIAN_POINT('',(-24.1156489724279,-54.9452378026827,38.989));
#180890=CARTESIAN_POINT('Origin',(5.49031038273072E-15,0.,38.989));
#180891=CARTESIAN_POINT('',(-24.3087286055922,-55.3789017591238,38.989));
#180892=CARTESIAN_POINT('',(10.2954134679533,22.3432738675267,38.989));
#180893=CARTESIAN_POINT('',(-24.3081989337718,-55.3791342586258,38.9889999995775));
#180894=CARTESIAN_POINT('Origin',(5.49031038273072E-15,0.,38.989));
#180895=CARTESIAN_POINT('',(-18.9913614316847,-57.420076955426,38.9889999997818));
#180896=CARTESIAN_POINT('Origin',(5.49031038273072E-15,0.,38.989));
#180897=CARTESIAN_POINT('',(-18.9908122363903,-57.4202585945859,38.989));
#180898=CARTESIAN_POINT('Origin',(5.49031038273072E-15,0.,38.989));
#180899=CARTESIAN_POINT('',(-18.8442866674264,-56.9692992632925,38.989));
#180900=CARTESIAN_POINT('Origin',(5.49031038273072E-15,0.,38.989));
#180901=CARTESIAN_POINT('',(-24.3743766270217,-55.5277679687682,39.2708017080178));
#180902=CARTESIAN_POINT('',(-24.3081989334776,-55.3791342579557,38.989));
#180903=CARTESIAN_POINT('',(-19.0416371861768,-57.5748148486259,39.2708017078546));
#180904=CARTESIAN_POINT('Origin',(5.52999282761009E-15,0.,39.2708017080178));
#180905=CARTESIAN_POINT('',(-19.041637186088,-57.5748148483575,39.2708017080178));
#180906=CARTESIAN_POINT('Origin',(60.71525,0.,39.3978017080178));
#180907=CARTESIAN_POINT('',(-19.1090650011318,-57.7842031819382,39.3978017080178));
#180908=CARTESIAN_POINT('',(-24.464376137792,-55.7284918401497,39.3978017080178));
#180909=CARTESIAN_POINT('Origin',(5.5478765747851E-15,0.,39.3978017080178));
#180910=CARTESIAN_POINT('',(-24.5258780191674,-55.8666273273832,39.3978017080178));
#180911=CARTESIAN_POINT('',(10.3344596589369,22.4309730483568,39.3978017080178));
#180912=CARTESIAN_POINT('',(-19.1557908785628,-57.9280106456675,39.3978017080178));
#180913=CARTESIAN_POINT('Origin',(5.5478765747851E-15,0.,39.3978017080178));
#180914=CARTESIAN_POINT('',(-19.1092287877198,-57.7847072652235,39.3978017080178));
#180915=CARTESIAN_POINT('Origin',(5.5478765747851E-15,0.,39.3978017080178));
#180916=CARTESIAN_POINT('',(-19.2232259141442,-58.1373965169892,39.2708017080178));
#180917=CARTESIAN_POINT('',(-24.6158705165696,-56.0673542006829,39.2708017081757));
#180918=CARTESIAN_POINT('Origin',(5.52999282761008E-15,0.,39.2708017080178));
#180919=CARTESIAN_POINT('',(-24.6820453786634,-56.215989076741,38.9890000005756));
#180920=CARTESIAN_POINT('',(-24.6158705164596,-56.0673542004325,39.2708017080178));
#180921=CARTESIAN_POINT('',(-24.6815255140429,-56.2162173246396,38.989));
#180922=CARTESIAN_POINT('Origin',(5.49031038273072E-15,0.,38.989));
#180923=CARTESIAN_POINT('',(-19.2740436149887,-58.2919551457916,38.989));
#180924=CARTESIAN_POINT('Origin',(5.49031038273072E-15,0.,38.989));
#180925=CARTESIAN_POINT('',(-19.2735045526312,-58.2921333818756,38.9890000005754));
#180926=CARTESIAN_POINT('Origin',(5.49031038273072E-15,0.,38.989));
#180927=CARTESIAN_POINT('',(-19.2735045527209,-58.2921333821958,38.989));
#180928=CARTESIAN_POINT('Origin',(62.2224557307631,0.,38.989));
#180929=CARTESIAN_POINT('',(-24.8746050278055,-56.6498810128381,38.989));
#180930=CARTESIAN_POINT('',(10.5838037820519,22.99100911823,38.989));
#180931=CARTESIAN_POINT('',(-19.4207352200703,-58.7434254837931,38.989));
#180932=CARTESIAN_POINT('Origin',(5.49031038273072E-15,0.,38.989));
#180933=CARTESIAN_POINT('',(-19.2742059773234,-58.292454845676,38.989));
#180934=CARTESIAN_POINT('Origin',(5.57972911860581E-15,0.,39.624));
#180935=CARTESIAN_POINT('Origin',(-24.1156440305593,-54.9452389789695,39.6240070731883));
#180936=CARTESIAN_POINT('Origin',(-18.844125000166,-56.9687855447423,39.6240070731883));
#180937=CARTESIAN_POINT('Origin',(5.57972911860581E-15,0.,39.624));
#180938=CARTESIAN_POINT('Origin',(-24.8900830207539,-56.6847276080563,39.5552135207985));
#180939=CARTESIAN_POINT('Origin',(-19.432549626632,-58.779677961498,39.5552117598806));
#180940=CARTESIAN_POINT('Origin',(5.51210908043506E-15,0.,39.1438017080178));
#180941=CARTESIAN_POINT('Origin',(-24.5323626684707,-55.8811008927581,39.171162538133));
#180942=CARTESIAN_POINT('Origin',(-19.1606277069624,-57.9430161406907,39.1712173702639));
#180943=CARTESIAN_POINT('Origin',(5.51210908043507E-15,0.,39.1438017080178));
#180944=CARTESIAN_POINT('Origin',(-24.4579221115101,-55.7141074023459,39.1712175859372));
#180945=CARTESIAN_POINT('Origin',(-19.1042073826023,-57.7691053333654,39.1711627526724));
#180946=CARTESIAN_POINT('Origin',(60.4792282238308,0.,38.989));
#180947=CARTESIAN_POINT('',(-12.7860306150453,-58.6264539577983,38.989));
#180948=CARTESIAN_POINT('',(-18.2401996527048,-57.1650137687746,38.989));
#180949=CARTESIAN_POINT('Origin',(5.49031038273072E-15,0.,38.989));
#180950=CARTESIAN_POINT('',(-18.386891348495,-57.6164843860302,38.989));
#180951=CARTESIAN_POINT('',(6.07721283595923,17.6762863142854,38.989));
#180952=CARTESIAN_POINT('',(-18.3863402754567,-57.6166602460949,38.988999999577));
#180953=CARTESIAN_POINT('Origin',(5.49031038273072E-15,0.,38.989));
#180954=CARTESIAN_POINT('',(-12.8852923618019,-59.090661591717,38.9889999997818));
#180955=CARTESIAN_POINT('Origin',(5.49031038273072E-15,0.,38.989));
#180956=CARTESIAN_POINT('',(-12.8847271885945,-59.0907848292984,38.989));
#180957=CARTESIAN_POINT('Origin',(5.49031038273072E-15,0.,38.989));
#180958=CARTESIAN_POINT('',(-12.786142387925,-58.6269798078532,38.989));
#180959=CARTESIAN_POINT('Origin',(5.49031038273072E-15,0.,38.989));
#180960=CARTESIAN_POINT('',(-18.4366189870675,-57.7713971777986,39.2708017080178));
#180961=CARTESIAN_POINT('',(-18.386340275234,-57.616660245397,38.989));
#180962=CARTESIAN_POINT('',(-12.919118186265,-59.2498070619041,39.2708017078546));
#180963=CARTESIAN_POINT('Origin',(5.52999282761009E-15,0.,39.2708017080178));
#180964=CARTESIAN_POINT('',(-12.9191181862048,-59.2498070616279,39.2708017080178));
#180965=CARTESIAN_POINT('Origin',(60.71525,0.,39.3978017080178));
#180966=CARTESIAN_POINT('',(-12.9642895838873,-59.4650964698966,39.3978017080178));
#180967=CARTESIAN_POINT('',(-18.5051441132844,-57.9804289733663,39.3978017080178));
#180968=CARTESIAN_POINT('Origin',(5.5478765747851E-15,0.,39.3978017080178));
#180969=CARTESIAN_POINT('',(-18.5518699907153,-58.1242364370956,39.3978017080178));
#180970=CARTESIAN_POINT('',(6.0997509100621,17.7456513739115,39.3978017080178));
#180971=CARTESIAN_POINT('',(-12.9957275188826,-59.6130003254554,39.3978017080178));
#180972=CARTESIAN_POINT('Origin',(5.5478765747851E-15,0.,39.3978017080178));
#180973=CARTESIAN_POINT('',(-12.964399782184,-59.4656149121213,39.3978017080178));
#180974=CARTESIAN_POINT('Origin',(5.5478765747851E-15,0.,39.3978017080178));
#180975=CARTESIAN_POINT('',(-13.0409063549241,-59.8282880397054,39.2708017080178));
#180976=CARTESIAN_POINT('',(-18.6203878281982,-58.33327048504,39.2708017081757));
#180977=CARTESIAN_POINT('Origin',(5.52999282761008E-15,0.,39.2708017080178));
#180978=CARTESIAN_POINT('',(-18.6706636022911,-58.4880082803368,38.9890000005756));
#180979=CARTESIAN_POINT('',(-18.620387828115,-58.3332704847795,39.2708017080178));
#180980=CARTESIAN_POINT('',(-18.6701227271413,-58.4881809372197,38.989));
#180981=CARTESIAN_POINT('Origin',(5.49031038273072E-15,0.,38.989));
#180982=CARTESIAN_POINT('',(-13.0752898951327,-59.9873118763435,38.989));
#180983=CARTESIAN_POINT('Origin',(5.49031038273072E-15,0.,38.989));
#180984=CARTESIAN_POINT('',(-13.0747351550713,-59.9874327886718,38.9890000005754));
#180985=CARTESIAN_POINT('Origin',(5.49031038273072E-15,0.,38.989));
#180986=CARTESIAN_POINT('',(-13.074735155127,-59.9874327889997,38.989));
#180987=CARTESIAN_POINT('Origin',(62.2224557307631,0.,38.989));
#180988=CARTESIAN_POINT('',(-18.8168143322229,-58.9396512752212,38.989));
#180989=CARTESIAN_POINT('',(6.24367625034032,18.1886080242681,38.989));
#180990=CARTESIAN_POINT('',(-13.1739864076109,-60.4516424606488,38.989));
#180991=CARTESIAN_POINT('Origin',(5.49031038273072E-15,0.,38.989));
#180992=CARTESIAN_POINT('',(-13.0753991351685,-59.987825810305,38.989));
#180993=CARTESIAN_POINT('Origin',(5.57972911860581E-15,0.,39.624));
#180994=CARTESIAN_POINT('Origin',(-18.2401946149528,-57.1650144220516,39.6240070731883));
#180995=CARTESIAN_POINT('Origin',(-12.7860353045052,-58.6264520046767,39.6240070731883));
#180996=CARTESIAN_POINT('Origin',(5.57972911860581E-15,0.,39.624));
#180997=CARTESIAN_POINT('Origin',(-18.8285650740579,-58.9759248679608,39.5552135208012));
#180998=CARTESIAN_POINT('Origin',(-13.1819466778331,-60.488931285249,39.5552117598823));
#180999=CARTESIAN_POINT('Origin',(5.51210908043506E-15,0.,39.1438017080178));
#181000=CARTESIAN_POINT('Origin',(-18.5568062168851,-58.139308545193,39.1711625381365));
#181001=CARTESIAN_POINT('Origin',(-12.9989693492948,-59.6284292050461,39.1712173702627));
#181002=CARTESIAN_POINT('Origin',(5.51210908043507E-15,0.,39.1438017080178));
#181003=CARTESIAN_POINT('Origin',(-18.5002290260138,-57.9654487055683,39.1712175859374));
#181004=CARTESIAN_POINT('Origin',(-12.961036730811,-59.4495735695164,39.1711627526749));
#181005=CARTESIAN_POINT('Origin',(60.4792282238308,0.,38.989));
#181006=CARTESIAN_POINT('',(-6.58785426247116,-59.6417962403142,38.989));
#181007=CARTESIAN_POINT('',(-12.1649068885794,-58.7584778814676,38.989));
#181008=CARTESIAN_POINT('Origin',(5.49031038273072E-15,0.,38.989));
#181009=CARTESIAN_POINT('',(-12.2636034620792,-59.2228087529788,38.989));
#181010=CARTESIAN_POINT('',(2.92491386234308,12.2335471699536,38.989));
#181011=CARTESIAN_POINT('',(-12.2630370254944,-59.2229260468456,38.9889999995772));
#181012=CARTESIAN_POINT('Origin',(5.49031038273072E-15,0.,38.989));
#181013=CARTESIAN_POINT('',(-6.63804933238239,-60.1138365740932,38.9889999997818));
#181014=CARTESIAN_POINT('Origin',(5.49031038273072E-15,0.,38.989));
#181015=CARTESIAN_POINT('',(-6.63747437341798,-60.1139000598793,38.989));
#181016=CARTESIAN_POINT('Origin',(5.49031038273072E-15,0.,38.989));
#181017=CARTESIAN_POINT('',(-6.58791045674911,-59.6423308931549,38.989));
#181018=CARTESIAN_POINT('Origin',(5.49031038273072E-15,0.,38.989));
#181019=CARTESIAN_POINT('',(-12.2968658913805,-59.382070869907,39.2708017080178));
#181020=CARTESIAN_POINT('',(-12.2630370253459,-59.2229260461285,38.989));
#181021=CARTESIAN_POINT('',(-6.65505462400518,-60.2756459901929,39.2708017078546));
#181022=CARTESIAN_POINT('Origin',(5.52999282761009E-15,0.,39.2708017080178));
#181023=CARTESIAN_POINT('',(-6.65505462397415,-60.2756459899119,39.2708017080178));
#181024=CARTESIAN_POINT('Origin',(60.71525,0.,39.3978017080178));
#181025=CARTESIAN_POINT('',(-6.67747469700966,-60.4944777170594,39.3978017080178));
#181026=CARTESIAN_POINT('',(-12.3431658574213,-59.5971203935659,39.3978017080178));
#181027=CARTESIAN_POINT('Origin',(5.5478765747851E-15,0.,39.3978017080178));
#181028=CARTESIAN_POINT('',(-12.3746037924166,-59.7450242491247,39.3978017080178));
#181029=CARTESIAN_POINT('',(2.93511643966565,12.2815465224196,39.3978017080178));
#181030=CARTESIAN_POINT('',(-6.69328024897475,-60.6448574988554,39.3978017080178));
#181031=CARTESIAN_POINT('Origin',(5.5478765747851E-15,0.,39.3978017080178));
#181032=CARTESIAN_POINT('',(-6.67753009965953,-60.4950048380619,39.3978017080178));
#181033=CARTESIAN_POINT('Origin',(5.5478765747851E-15,0.,39.3978017080178));
#181034=CARTESIAN_POINT('',(-6.7157078966943,-60.8636883187844,39.2708017080178));
#181035=CARTESIAN_POINT('',(-12.4208962742143,-59.9600752509414,39.2708017081757));
#181036=CARTESIAN_POINT('Origin',(5.52999282761008E-15,0.,39.2708017080178));
#181037=CARTESIAN_POINT('',(-12.4547221284046,-60.1192206258106,38.9890000005756));
#181038=CARTESIAN_POINT('',(-12.4208962741589,-59.9600752506736,39.2708017080178));
#181039=CARTESIAN_POINT('',(-12.4541661686668,-60.1193358000128,38.989));
#181040=CARTESIAN_POINT('Origin',(5.49031038273072E-15,0.,38.989));
#181041=CARTESIAN_POINT('',(-6.73328056300539,-61.0254350648262,38.989));
#181042=CARTESIAN_POINT('Origin',(5.49031038273072E-15,0.,38.989));
#181043=CARTESIAN_POINT('',(-6.73271622308818,-61.0254973286579,38.9890000005754));
#181044=CARTESIAN_POINT('Origin',(5.49031038273072E-15,0.,38.989));
#181045=CARTESIAN_POINT('',(-6.73271622310929,-61.0254973289898,38.989));
#181046=CARTESIAN_POINT('Origin',(62.2224557307631,0.,38.989));
#181047=CARTESIAN_POINT('',(-12.5528626811449,-60.5836663843181,38.989));
#181048=CARTESIAN_POINT('',(3.00026883051142,12.5880644220972,38.989));
#181049=CARTESIAN_POINT('',(-6.78290064323581,-61.4975385923862,38.989));
#181050=CARTESIAN_POINT('Origin',(5.49031038273072E-15,0.,38.989));
#181051=CARTESIAN_POINT('',(-6.73333548388561,-61.0259576020968,38.989));
#181052=CARTESIAN_POINT('Origin',(5.57972911860581E-15,0.,39.624));
#181053=CARTESIAN_POINT('Origin',(-12.1649018101387,-58.7584780045774,39.6240070731883));
#181054=CARTESIAN_POINT('Origin',(-6.58785913039844,-59.6417947880741,39.6240070731883));
#181055=CARTESIAN_POINT('Origin',(5.57972911860581E-15,0.,39.624));
#181056=CARTESIAN_POINT('Origin',(-12.560757428279,-60.6209695535074,39.5552135208015));
#181057=CARTESIAN_POINT('Origin',(-6.78691956273258,-61.5354552197177,39.5552117598811));
#181058=CARTESIAN_POINT('Origin',(5.51210908043506E-15,0.,39.1438017080178));
#181059=CARTESIAN_POINT('Origin',(-12.3779375131254,-59.7605297667732,39.1711625381368));
#181060=CARTESIAN_POINT('Origin',(-6.69489156322713,-60.6605407209803,39.1712173702631));
#181061=CARTESIAN_POINT('Origin',(5.51210908043507E-15,0.,39.1438017080178));
#181062=CARTESIAN_POINT('Origin',(-12.3398435598864,-59.581708422721,39.1712175859406));
#181063=CARTESIAN_POINT('Origin',(-6.67586224832375,-60.4786998370192,39.1711627526733));
#181064=CARTESIAN_POINT('Origin',(60.4792282238308,0.,38.989));
#181065=CARTESIAN_POINT('',(-0.317500000000204,-60.0036905223731,38.989));
#181066=CARTESIAN_POINT('',(-5.9563328589123,-59.7081718144892,38.989));
#181067=CARTESIAN_POINT('Origin',(5.49031038273072E-15,0.,38.989));
#181068=CARTESIAN_POINT('',(-6.00595296980892,-60.1802756340603,38.989));
#181069=CARTESIAN_POINT('',(0.9765688230087,6.25398151259764,38.989));
#181070=CARTESIAN_POINT('',(-6.00537737567531,-60.1803330766331,38.9889999995773));
#181071=CARTESIAN_POINT('Origin',(5.49031038273072E-15,0.,38.989));
#181072=CARTESIAN_POINT('',(-0.3180784453762,-60.4783917833346,38.9889999997818));
#181073=CARTESIAN_POINT('Origin',(5.49031038273072E-15,0.,38.989));
#181074=CARTESIAN_POINT('',(-0.31750000002549,-60.478394821762,38.989));
#181075=CARTESIAN_POINT('Origin',(5.49031038273072E-15,0.,38.989));
#181076=CARTESIAN_POINT('',(-0.317500000000204,-60.004228120231,38.989));
#181077=CARTESIAN_POINT('Origin',(5.49031038273072E-15,0.,38.989));
#181078=CARTESIAN_POINT('',(-6.02238575970296,-60.3421421670675,39.2708017080178));
#181079=CARTESIAN_POINT('',(-6.0053773756026,-60.1803330759045,38.989));
#181080=CARTESIAN_POINT('',(-0.318076890625054,-60.6410923275232,39.2708017078546));
#181081=CARTESIAN_POINT('Origin',(5.52999282761009E-15,0.,39.2708017080178));
#181082=CARTESIAN_POINT('',(-0.318076890623573,-60.6410923272405,39.2708017080178));
#181083=CARTESIAN_POINT('Origin',(60.71525,0.,39.3978017080178));
#181084=CARTESIAN_POINT('',(-0.317500000000207,-60.8610688070707,39.3978017080178));
#181085=CARTESIAN_POINT('',(-6.04595329345081,-60.5608532912343,39.3978017080178));
#181086=CARTESIAN_POINT('Origin',(5.5478765747851E-15,0.,39.3978017080178));
#181087=CARTESIAN_POINT('',(-6.0617588454159,-60.7112330730304,39.3978017080178));
#181088=CARTESIAN_POINT('',(0.97914764405288,6.27851735587422,39.3978017080178));
#181089=CARTESIAN_POINT('',(-0.317500000000208,-61.0122769227456,39.3978017080178));
#181090=CARTESIAN_POINT('Origin',(5.5478765747851E-15,0.,39.3978017080178));
#181091=CARTESIAN_POINT('',(-0.317500000000207,-60.8615988316031,39.3978017080178));
#181092=CARTESIAN_POINT('Origin',(5.5478765747851E-15,0.,39.3978017080178));
#181093=CARTESIAN_POINT('',(-0.316930737396123,-61.2322532920972,39.2708017080178));
#181094=CARTESIAN_POINT('',(-6.08531878141059,-60.9299448849411,39.2708017081757));
#181095=CARTESIAN_POINT('Origin',(5.52999282761008E-15,0.,39.2708017080178));
#181096=CARTESIAN_POINT('',(-6.10232411256107,-61.0917542093523,38.9890000005756));
#181097=CARTESIAN_POINT('',(-6.08531878138341,-60.929944884669,39.2708017080178));
#181098=CARTESIAN_POINT('',(-6.10175915944654,-61.0918106390012,38.989));
#181099=CARTESIAN_POINT('Origin',(5.49031038273072E-15,0.,38.989));
#181100=CARTESIAN_POINT('',(-0.317500000000209,-61.3949508163454,38.989));
#181101=CARTESIAN_POINT('Origin',(5.49031038273072E-15,0.,38.989));
#181102=CARTESIAN_POINT('',(-0.316932243253465,-61.394953749505,38.9890000005754));
#181103=CARTESIAN_POINT('Origin',(5.49031038273072E-15,0.,38.989));
#181104=CARTESIAN_POINT('',(-0.316932243239769,-61.3949537498373,38.989));
#181105=CARTESIAN_POINT('Origin',(62.2224557307631,0.,38.989));
#181106=CARTESIAN_POINT('',(-6.15137923967696,-61.5639141665612,38.989));
#181107=CARTESIAN_POINT('',(0.995615674755347,6.43520020182081,38.989));
#181108=CARTESIAN_POINT('',(-0.317500000000211,-61.8696548221181,38.989));
#181109=CARTESIAN_POINT('Origin',(5.49031038273072E-15,0.,38.989));
#181110=CARTESIAN_POINT('',(-0.317500000000209,-61.3954762318973,38.989));
#181111=CARTESIAN_POINT('Origin',(5.57972911860581E-15,0.,39.624));
#181112=CARTESIAN_POINT('Origin',(-5.95632779542335,-59.708171406083,39.6240070731883));
#181113=CARTESIAN_POINT('Origin',(-0.317504993060902,-60.0036895869254,
39.6240070731883));
#181114=CARTESIAN_POINT('Origin',(5.57972911860581E-15,0.,39.624));
#181115=CARTESIAN_POINT('Origin',(-6.15533149561007,-61.6018382108724,39.5552135208017));
#181116=CARTESIAN_POINT('Origin',(-0.317533536648827,-61.9077838296766,
39.5552117598813));
#181117=CARTESIAN_POINT('Origin',(5.51210908043506E-15,0.,39.1438017080178));
#181118=CARTESIAN_POINT('Origin',(-6.06345353572162,-60.7270021185312,39.1711625381328));
#181119=CARTESIAN_POINT('Origin',(-0.317463144196724,-61.0280426587412,
39.1712173702625));
#181120=CARTESIAN_POINT('Origin',(5.51210908043507E-15,0.,39.1438017080178));
#181121=CARTESIAN_POINT('Origin',(-6.04426018543789,-60.5451784741235,39.1712175859388));
#181122=CARTESIAN_POINT('Origin',(-0.317545622030958,-60.8452088131237,
39.171162752676));
#181123=CARTESIAN_POINT('Origin',(60.4792282238308,0.,38.989));
#181124=CARTESIAN_POINT('',(5.95633285891191,-59.7081718144893,38.989));
#181125=CARTESIAN_POINT('',(0.317499999999796,-60.0036905223731,38.989));
#181126=CARTESIAN_POINT('Origin',(5.49031038273072E-15,0.,38.989));
#181127=CARTESIAN_POINT('',(0.317500000025055,-60.4783948217626,38.989));
#181128=CARTESIAN_POINT('',(0.317500000000005,2.10053551406057E-13,38.989));
#181129=CARTESIAN_POINT('',(0.318078445377651,-60.4783917836887,38.9889999995774));
#181130=CARTESIAN_POINT('Origin',(5.49031038273072E-15,0.,38.989));
#181131=CARTESIAN_POINT('',(6.00537737563974,-60.1803330762807,38.9889999997818));
#181132=CARTESIAN_POINT('Origin',(5.49031038273072E-15,0.,38.989));
#181133=CARTESIAN_POINT('',(6.00595296980844,-60.1802756340597,38.989));
#181134=CARTESIAN_POINT('Origin',(5.49031038273072E-15,0.,38.989));
#181135=CARTESIAN_POINT('',(5.95638905318986,-59.7087064673299,38.989));
#181136=CARTESIAN_POINT('Origin',(5.49031038273072E-15,0.,38.989));
#181137=CARTESIAN_POINT('',(0.31807689062316,-60.6410923272405,39.2708017080178));
#181138=CARTESIAN_POINT('',(0.318078445373799,-60.4783917829566,38.989));
#181139=CARTESIAN_POINT('',(6.02238575973065,-60.3421421673489,39.2708017078546));
#181140=CARTESIAN_POINT('Origin',(5.52999282761009E-15,0.,39.2708017080178));
#181141=CARTESIAN_POINT('',(6.02238575970257,-60.3421421670675,39.2708017080178));
#181142=CARTESIAN_POINT('Origin',(60.71525,0.,39.3978017080178));
#181143=CARTESIAN_POINT('',(6.04595329345041,-60.5608532912344,39.3978017080178));
#181144=CARTESIAN_POINT('',(0.317499999999793,-60.8610688070707,39.3978017080178));
#181145=CARTESIAN_POINT('Origin',(5.5478765747851E-15,0.,39.3978017080178));
#181146=CARTESIAN_POINT('',(0.317499999999792,-61.0122769227456,39.3978017080178));
#181147=CARTESIAN_POINT('',(0.317500000000005,2.10877617033113E-13,39.3978017080178));
#181148=CARTESIAN_POINT('',(6.0617588454155,-60.7112330730304,39.3978017080178));
#181149=CARTESIAN_POINT('Origin',(5.5478765747851E-15,0.,39.3978017080178));
#181150=CARTESIAN_POINT('',(6.04600869610028,-60.5613804122369,39.3978017080178));
#181151=CARTESIAN_POINT('Origin',(5.5478765747851E-15,0.,39.3978017080178));
#181152=CARTESIAN_POINT('',(6.08531878138301,-60.929944884669,39.2708017080178));
#181153=CARTESIAN_POINT('',(0.316930737397122,-61.2322532923707,39.2708017081757));
#181154=CARTESIAN_POINT('Origin',(5.52999282761008E-15,0.,39.2708017080178));
#181155=CARTESIAN_POINT('',(0.316932243253051,-61.3949537495049,38.9890000005756));
#181156=CARTESIAN_POINT('',(0.316930737395706,-61.2322532920972,39.2708017080178));
#181157=CARTESIAN_POINT('',(0.317499999999791,-61.3949508163454,38.989));
#181158=CARTESIAN_POINT('Origin',(5.49031038273072E-15,0.,38.989));
#181159=CARTESIAN_POINT('',(6.10175915944613,-61.0918106390012,38.989));
#181160=CARTESIAN_POINT('Origin',(5.49031038273072E-15,0.,38.989));
#181161=CARTESIAN_POINT('',(6.10232411256069,-61.0917542093524,38.9890000005754));
#181162=CARTESIAN_POINT('Origin',(5.49031038273072E-15,0.,38.989));
#181163=CARTESIAN_POINT('',(6.10232411260904,-61.0917542096815,38.989));
#181164=CARTESIAN_POINT('Origin',(62.2224557307631,0.,38.989));
#181165=CARTESIAN_POINT('',(0.31749999999979,-61.8696548221181,38.989));
#181166=CARTESIAN_POINT('',(0.317500000000005,2.1613999771587E-13,38.989));
#181167=CARTESIAN_POINT('',(6.15137923967656,-61.5639141665612,38.989));
#181168=CARTESIAN_POINT('Origin',(5.49031038273072E-15,0.,38.989));
#181169=CARTESIAN_POINT('',(6.10181408032636,-61.0923331762718,38.989));
#181170=CARTESIAN_POINT('Origin',(5.57972911860581E-15,0.,39.624));
#181171=CARTESIAN_POINT('Origin',(0.317504993060349,-60.0036895869254,39.6240070731883));
#181172=CARTESIAN_POINT('Origin',(5.95632779542281,-59.708171406083,39.6240070731883));
#181173=CARTESIAN_POINT('Origin',(5.57972911860581E-15,0.,39.624));
#181174=CARTESIAN_POINT('Origin',(0.31753353701135,-61.9077842377855,39.5552135208018));
#181175=CARTESIAN_POINT('Origin',(6.15533145331131,-61.6018378049618,39.5552117598803));
#181176=CARTESIAN_POINT('Origin',(5.51210908043506E-15,0.,39.1438017080178));
#181177=CARTESIAN_POINT('Origin',(0.317462907478285,-61.0281367271401,39.1711625381349));
#181178=CARTESIAN_POINT('Origin',(6.06344346747477,-60.7269085901925,39.1712173702593));
#181179=CARTESIAN_POINT('Origin',(5.51210908043507E-15,0.,39.1438017080178));
#181180=CARTESIAN_POINT('Origin',(0.317545368445239,-60.8453028802699,39.1712175859377));
#181181=CARTESIAN_POINT('Origin',(6.04425010054675,-60.5450849487952,39.1711627526747));
#181182=CARTESIAN_POINT('Origin',(60.4792282238308,0.,38.989));
#181183=CARTESIAN_POINT('',(12.164906888579,-58.7584778814677,38.989));
#181184=CARTESIAN_POINT('',(6.58785426247077,-59.6417962403143,38.989));
#181185=CARTESIAN_POINT('Origin',(5.49031038273072E-15,0.,38.989));
#181186=CARTESIAN_POINT('',(6.63747437341763,-60.1139000598801,38.989));
#181187=CARTESIAN_POINT('',(0.976568823008617,-6.25398151259724,38.989));
#181188=CARTESIAN_POINT('',(6.63804933242089,-60.1138365744455,38.9889999995772));
#181189=CARTESIAN_POINT('Origin',(5.49031038273072E-15,0.,38.989));
#181190=CARTESIAN_POINT('',(12.2630370254221,-59.2229260464987,38.9889999997818));
#181191=CARTESIAN_POINT('Origin',(5.49031038273072E-15,0.,38.989));
#181192=CARTESIAN_POINT('',(12.2636034620787,-59.2228087529783,38.989));
#181193=CARTESIAN_POINT('Origin',(5.49031038273072E-15,0.,38.989));
#181194=CARTESIAN_POINT('',(12.1650186614586,-58.7590037315226,38.989));
#181195=CARTESIAN_POINT('Origin',(5.49031038273072E-15,0.,38.989));
#181196=CARTESIAN_POINT('',(6.65505462397376,-60.2756459899119,39.2708017080178));
#181197=CARTESIAN_POINT('',(6.6380493323405,-60.1138365737175,38.989));
#181198=CARTESIAN_POINT('',(12.2968658914375,-59.382070870184,39.2708017078546));
#181199=CARTESIAN_POINT('Origin',(5.52999282761009E-15,0.,39.2708017080178));
#181200=CARTESIAN_POINT('',(12.2968658913801,-59.3820708699071,39.2708017080178));
#181201=CARTESIAN_POINT('Origin',(60.71525,0.,39.3978017080178));
#181202=CARTESIAN_POINT('',(12.3431658574209,-59.5971203935659,39.3978017080178));
#181203=CARTESIAN_POINT('',(6.67747469700926,-60.4944777170594,39.3978017080178));
#181204=CARTESIAN_POINT('Origin',(5.5478765747851E-15,0.,39.3978017080178));
#181205=CARTESIAN_POINT('',(6.69328024897435,-60.6448574988554,39.3978017080178));
#181206=CARTESIAN_POINT('',(0.979147644052797,-6.27851735587382,39.3978017080178));
#181207=CARTESIAN_POINT('',(12.3746037924162,-59.7450242491248,39.3978017080178));
#181208=CARTESIAN_POINT('Origin',(5.5478765747851E-15,0.,39.3978017080178));
#181209=CARTESIAN_POINT('',(12.3432760557176,-59.5976388357907,39.3978017080178));
#181210=CARTESIAN_POINT('Origin',(5.5478765747851E-15,0.,39.3978017080178));
#181211=CARTESIAN_POINT('',(12.4208962741585,-59.9600752506737,39.2708017080178));
#181212=CARTESIAN_POINT('',(6.7157078967239,-60.8636883190563,39.2708017081757));
#181213=CARTESIAN_POINT('Origin',(5.52999282761008E-15,0.,39.2708017080178));
#181214=CARTESIAN_POINT('',(6.73271622308777,-61.0254973286579,38.9890000005756));
#181215=CARTESIAN_POINT('',(6.7157078966939,-60.8636883187845,39.2708017080178));
#181216=CARTESIAN_POINT('',(6.73328056300499,-61.0254350648262,38.989));
#181217=CARTESIAN_POINT('Origin',(5.49031038273072E-15,0.,38.989));
#181218=CARTESIAN_POINT('',(12.4541661686664,-60.1193358000129,38.989));
#181219=CARTESIAN_POINT('Origin',(5.49031038273072E-15,0.,38.989));
#181220=CARTESIAN_POINT('',(12.4547221284042,-60.1192206258107,38.9890000005754));
#181221=CARTESIAN_POINT('Origin',(5.49031038273072E-15,0.,38.989));
#181222=CARTESIAN_POINT('',(12.4547221284867,-60.1192206261329,38.989));
#181223=CARTESIAN_POINT('Origin',(62.2224557307631,0.,38.989));
#181224=CARTESIAN_POINT('',(6.78290064323541,-61.4975385923862,38.989));
#181225=CARTESIAN_POINT('',(0.995615674755264,-6.4352002018204,38.989));
#181226=CARTESIAN_POINT('',(12.5528626811445,-60.5836663843182,38.989));
#181227=CARTESIAN_POINT('Origin',(5.49031038273072E-15,0.,38.989));
#181228=CARTESIAN_POINT('',(12.4542754087022,-60.1198497339744,38.989));
#181229=CARTESIAN_POINT('Origin',(5.57972911860581E-15,0.,39.624));
#181230=CARTESIAN_POINT('Origin',(6.5878591303979,-59.6417947880742,39.6240070731883));
#181231=CARTESIAN_POINT('Origin',(12.1649018101382,-58.7584780045775,39.6240070731883));
#181232=CARTESIAN_POINT('Origin',(5.57972911860581E-15,0.,39.624));
#181233=CARTESIAN_POINT('Origin',(6.78691960575346,-61.5354556255537,39.5552135208006));
#181234=CARTESIAN_POINT('Origin',(12.5607573437828,-60.6209691542412,39.5552117598815));
#181235=CARTESIAN_POINT('Origin',(5.51210908043506E-15,0.,39.1438017080178));
#181236=CARTESIAN_POINT('Origin',(6.69490116063052,-60.6606342988051,39.1711625381332));
#181237=CARTESIAN_POINT('Origin',(12.3779177236596,-59.7604378032094,39.1712173702605));
#181238=CARTESIAN_POINT('Origin',(5.51210908043507E-15,0.,39.1438017080178));
#181239=CARTESIAN_POINT('Origin',(6.67587182882202,-60.4787934153613,39.1712175859376));
#181240=CARTESIAN_POINT('Origin',(12.3398237541815,-59.5816164638928,39.171162752676));
#181241=CARTESIAN_POINT('Origin',(60.4792282238308,0.,38.989));
#181242=CARTESIAN_POINT('',(18.2401996527044,-57.1650137687747,38.989));
#181243=CARTESIAN_POINT('',(12.786030615045,-58.6264539577984,38.989));
#181244=CARTESIAN_POINT('Origin',(5.49031038273072E-15,0.,38.989));
#181245=CARTESIAN_POINT('',(12.8847271885942,-59.0907848292991,38.989));
#181246=CARTESIAN_POINT('',(2.92491386234291,-12.2335471699533,38.989));
#181247=CARTESIAN_POINT('',(12.885292361877,-59.0906615920632,38.9889999995772));
#181248=CARTESIAN_POINT('Origin',(5.49031038273072E-15,0.,38.989));
#181249=CARTESIAN_POINT('',(18.3863402753486,-57.6166602457573,38.9889999997818));
#181250=CARTESIAN_POINT('Origin',(5.49031038273072E-15,0.,38.989));
#181251=CARTESIAN_POINT('',(18.3868913484944,-57.6164843860297,38.989));
#181252=CARTESIAN_POINT('Origin',(5.49031038273072E-15,0.,38.989));
#181253=CARTESIAN_POINT('',(18.2403657795786,-57.1655250547207,38.989));
#181254=CARTESIAN_POINT('Origin',(5.49031038273072E-15,0.,38.989));
#181255=CARTESIAN_POINT('',(12.9191181862044,-59.249807061628,39.2708017080178));
#181256=CARTESIAN_POINT('',(12.8852923617209,-59.0906615913478,38.989));
#181257=CARTESIAN_POINT('',(18.4366189871531,-57.7713971780681,39.2708017078546));
#181258=CARTESIAN_POINT('Origin',(5.52999282761009E-15,0.,39.2708017080178));
#181259=CARTESIAN_POINT('',(18.4366189870671,-57.7713971777987,39.2708017080178));
#181260=CARTESIAN_POINT('Origin',(60.71525,0.,39.3978017080178));
#181261=CARTESIAN_POINT('',(18.505144113284,-57.9804289733664,39.3978017080178));
#181262=CARTESIAN_POINT('',(12.9642895838869,-59.4650964698967,39.3978017080178));
#181263=CARTESIAN_POINT('Origin',(5.5478765747851E-15,0.,39.3978017080178));
#181264=CARTESIAN_POINT('',(12.9957275188822,-59.6130003254555,39.3978017080178));
#181265=CARTESIAN_POINT('',(2.93511643966547,-12.2815465224192,39.3978017080178));
#181266=CARTESIAN_POINT('',(18.5518699907149,-58.1242364370957,39.3978017080178));
#181267=CARTESIAN_POINT('Origin',(5.5478765747851E-15,0.,39.3978017080178));
#181268=CARTESIAN_POINT('',(18.505307899872,-57.9809330566518,39.3978017080178));
#181269=CARTESIAN_POINT('Origin',(5.5478765747851E-15,0.,39.3978017080178));
#181270=CARTESIAN_POINT('',(18.6203878281146,-58.3332704847796,39.2708017080178));
#181271=CARTESIAN_POINT('',(13.0409063549819,-59.8282880399727,39.2708017081757));
#181272=CARTESIAN_POINT('Origin',(5.52999282761008E-15,0.,39.2708017080178));
#181273=CARTESIAN_POINT('',(13.0747351550709,-59.9874327886718,38.9890000005756));
#181274=CARTESIAN_POINT('',(13.0409063549237,-59.8282880397055,39.2708017080178));
#181275=CARTESIAN_POINT('',(13.0752898951324,-59.9873118763436,38.989));
#181276=CARTESIAN_POINT('Origin',(5.49031038273072E-15,0.,38.989));
#181277=CARTESIAN_POINT('',(18.6701227271409,-58.4881809372198,38.989));
#181278=CARTESIAN_POINT('Origin',(5.49031038273072E-15,0.,38.989));
#181279=CARTESIAN_POINT('',(18.6706636022907,-58.488008280337,38.9890000005754));
#181280=CARTESIAN_POINT('Origin',(5.49031038273072E-15,0.,38.989));
#181281=CARTESIAN_POINT('',(18.6706636024065,-58.4880082806488,38.989));
#181282=CARTESIAN_POINT('Origin',(62.2224557307631,0.,38.989));
#181283=CARTESIAN_POINT('',(13.1739864076105,-60.4516424606489,38.989));
#181284=CARTESIAN_POINT('',(3.00026883051124,-12.5880644220968,38.989));
#181285=CARTESIAN_POINT('',(18.8168143322225,-58.9396512752214,38.989));
#181286=CARTESIAN_POINT('Origin',(5.49031038273072E-15,0.,38.989));
#181287=CARTESIAN_POINT('',(18.6702850894756,-58.4886806371042,38.989));
#181288=CARTESIAN_POINT('Origin',(5.57972911860581E-15,0.,39.624));
#181289=CARTESIAN_POINT('Origin',(12.7860353045047,-58.6264520046768,39.6240070731883));
#181290=CARTESIAN_POINT('Origin',(18.2401946149522,-57.1650144220518,39.6240070731883));
#181291=CARTESIAN_POINT('Origin',(5.57972911860581E-15,0.,39.624));
#181292=CARTESIAN_POINT('Origin',(13.18194676304,-60.4889316843658,39.5552135207995));
#181293=CARTESIAN_POINT('Origin',(18.8285649482889,-58.9759244797131,39.5552117598831));
#181294=CARTESIAN_POINT('Origin',(5.51210908043506E-15,0.,39.1438017080178));
#181295=CARTESIAN_POINT('Origin',(12.9989886756685,-59.6285212670386,39.1711625381305));
#181296=CARTESIAN_POINT('Origin',(18.5567769230188,-58.1392191539798,39.1712173702638));
#181297=CARTESIAN_POINT('Origin',(5.51210908043507E-15,0.,39.1438017080178));
#181298=CARTESIAN_POINT('Origin',(12.9610560404262,-59.4496656337931,39.171217585937));
#181299=CARTESIAN_POINT('Origin',(18.5001997164958,-57.9653593207584,39.1711627526739));
#181300=CARTESIAN_POINT('Origin',(60.4792282238308,0.,38.989));
#181301=CARTESIAN_POINT('',(24.1156489724276,-54.9452378026829,38.989));
#181302=CARTESIAN_POINT('',(18.8441205405518,-56.9687879773467,38.989));
#181303=CARTESIAN_POINT('Origin',(5.49031038273072E-15,0.,38.989));
#181304=CARTESIAN_POINT('',(18.9908122363901,-57.4202585945866,38.989));
#181305=CARTESIAN_POINT('',(6.07721283595898,-17.676286314285,38.989));
#181306=CARTESIAN_POINT('',(18.9913614317957,-57.4200769557629,38.988999999577));
#181307=CARTESIAN_POINT('Origin',(5.49031038273072E-15,0.,38.989));
#181308=CARTESIAN_POINT('',(24.3081989336292,-55.379134258302,38.9889999997818));
#181309=CARTESIAN_POINT('Origin',(5.49031038273072E-15,0.,38.989));
#181310=CARTESIAN_POINT('',(24.3087286055916,-55.3789017591234,38.989));
#181311=CARTESIAN_POINT('Origin',(5.49031038273072E-15,0.,38.989));
#181312=CARTESIAN_POINT('',(24.1158676331756,-54.9457289227641,38.989));
#181313=CARTESIAN_POINT('Origin',(5.49031038273072E-15,0.,38.989));
#181314=CARTESIAN_POINT('',(19.0416371860877,-57.5748148483576,39.2708017080178));
#181315=CARTESIAN_POINT('',(18.9913614315656,-57.4200769550673,38.989));
#181316=CARTESIAN_POINT('',(24.3743766271349,-55.5277679690272,39.2708017078546));
#181317=CARTESIAN_POINT('Origin',(5.52999282761009E-15,0.,39.2708017080178));
#181318=CARTESIAN_POINT('',(24.3743766270213,-55.5277679687684,39.2708017080178));
#181319=CARTESIAN_POINT('Origin',(60.71525,0.,39.3978017080178));
#181320=CARTESIAN_POINT('',(24.4643761377916,-55.7284918401499,39.3978017080178));
#181321=CARTESIAN_POINT('',(19.1090650011314,-57.7842031819383,39.3978017080178));
#181322=CARTESIAN_POINT('Origin',(5.5478765747851E-15,0.,39.3978017080178));
#181323=CARTESIAN_POINT('',(19.1557908785624,-57.9280106456676,39.3978017080178));
#181324=CARTESIAN_POINT('',(6.09975091006187,-17.7456513739111,39.3978017080178));
#181325=CARTESIAN_POINT('',(24.525878019167,-55.8666273273833,39.3978017080178));
#181326=CARTESIAN_POINT('Origin',(5.5478765747851E-15,0.,39.3978017080178));
#181327=CARTESIAN_POINT('',(24.4645917181906,-55.7289760416539,39.3978017080178));
#181328=CARTESIAN_POINT('Origin',(5.5478765747851E-15,0.,39.3978017080178));
#181329=CARTESIAN_POINT('',(24.6158705164593,-56.0673542004326,39.2708017080178));
#181330=CARTESIAN_POINT('',(19.2232259142297,-58.137396517249,39.2708017081757));
#181331=CARTESIAN_POINT('Origin',(5.52999282761008E-15,0.,39.2708017080178));
#181332=CARTESIAN_POINT('',(19.2735045526308,-58.2921333818756,38.9890000005756));
#181333=CARTESIAN_POINT('',(19.2232259141438,-58.1373965169894,39.2708017080178));
#181334=CARTESIAN_POINT('',(19.2740436149883,-58.2919551457917,38.989));
#181335=CARTESIAN_POINT('Origin',(5.49031038273072E-15,0.,38.989));
#181336=CARTESIAN_POINT('',(24.6815255140425,-56.2162173246398,38.989));
#181337=CARTESIAN_POINT('Origin',(5.49031038273072E-15,0.,38.989));
#181338=CARTESIAN_POINT('',(24.6820453786631,-56.2159890767412,38.9890000005754));
#181339=CARTESIAN_POINT('Origin',(5.49031038273072E-15,0.,38.989));
#181340=CARTESIAN_POINT('',(24.6820453788107,-56.2159890770392,38.989));
#181341=CARTESIAN_POINT('Origin',(62.2224557307631,0.,38.989));
#181342=CARTESIAN_POINT('',(19.42073522007,-58.7434254837933,38.989));
#181343=CARTESIAN_POINT('',(6.24367625034007,-18.1886080242677,38.989));
#181344=CARTESIAN_POINT('',(24.8746050278051,-56.6498810128382,38.989));
#181345=CARTESIAN_POINT('Origin',(5.49031038273072E-15,0.,38.989));
#181346=CARTESIAN_POINT('',(24.6817392198003,-56.2166973156307,38.989));
#181347=CARTESIAN_POINT('Origin',(5.57972911860581E-15,0.,39.624));
#181348=CARTESIAN_POINT('Origin',(18.8441250001654,-56.9687855447425,39.6240070731883));
#181349=CARTESIAN_POINT('Origin',(24.1156440305588,-54.9452389789697,39.6240070731883));
#181350=CARTESIAN_POINT('Origin',(5.57972911860581E-15,0.,39.624));
#181351=CARTESIAN_POINT('Origin',(19.4325497530937,-58.7796783495198,39.5552135207998));
#181352=CARTESIAN_POINT('Origin',(24.890082855091,-56.6847272350816,39.5552117598808));
#181353=CARTESIAN_POINT('Origin',(5.51210908043506E-15,0.,39.1438017080178));
#181354=CARTESIAN_POINT('Origin',(19.1606565505633,-57.9431056782032,39.1711625381345));
#181355=CARTESIAN_POINT('Origin',(24.5323241911535,-55.8810150532832,39.1712173702631));
#181356=CARTESIAN_POINT('Origin',(5.51210908043507E-15,0.,39.1438017080178));
#181357=CARTESIAN_POINT('Origin',(19.1042362097731,-57.7691948748978,39.1712175859387));
#181358=CARTESIAN_POINT('Origin',(24.457883619298,-55.7140215708725,39.1711627526749));
#181359=CARTESIAN_POINT('Origin',(60.4792282238308,0.,38.989));
#181360=CARTESIAN_POINT('',(29.7268821954849,-52.1234703131947,38.989));
#181361=CARTESIAN_POINT('',(24.6957503380306,-54.6869600343298,38.989));
#181362=CARTESIAN_POINT('Origin',(5.49031038273072E-15,0.,38.989));
#181363=CARTESIAN_POINT('',(24.8888299712411,-55.1206239907503,38.989));
#181364=CARTESIAN_POINT('',(10.295413467953,-22.3432738675264,38.989));
#181365=CARTESIAN_POINT('',(24.8893571716697,-55.1203859404113,38.988999999577));
#181366=CARTESIAN_POINT('Origin',(5.49031038273072E-15,0.,38.989));
#181367=CARTESIAN_POINT('',(29.9637318775753,-52.5348628870839,38.9889999997818));
#181368=CARTESIAN_POINT('Origin',(5.49031038273072E-15,0.,38.989));
#181369=CARTESIAN_POINT('',(29.9642343451574,-52.5345762957638,38.989));
#181370=CARTESIAN_POINT('Origin',(5.49031038273072E-15,0.,38.989));
#181371=CARTESIAN_POINT('',(29.7271509944138,-52.1239358865967,38.989));
#181372=CARTESIAN_POINT('Origin',(5.49031038273072E-15,0.,38.989));
#181373=CARTESIAN_POINT('',(24.9555320242414,-55.2690209153041,39.2708017080178));
#181374=CARTESIAN_POINT('',(24.8893571713682,-55.1203859397435,38.989));
#181375=CARTESIAN_POINT('',(30.0450834961236,-52.6757649141852,39.2708017078546));
#181376=CARTESIAN_POINT('Origin',(5.52999282761009E-15,0.,39.2708017080178));
#181377=CARTESIAN_POINT('',(30.0450834959836,-52.6757649139397,39.2708017080178));
#181378=CARTESIAN_POINT('Origin',(60.71525,0.,39.3978017080178));
#181379=CARTESIAN_POINT('',(30.1555713378337,-52.865981688396,39.3978017080178));
#181380=CARTESIAN_POINT('',(25.0444775033946,-55.4702140717967,39.3978017080178));
#181381=CARTESIAN_POINT('Origin',(5.5478765747851E-15,0.,39.3978017080178));
#181382=CARTESIAN_POINT('',(25.1059793847701,-55.6083495590302,39.3978017080178));
#181383=CARTESIAN_POINT('',(10.3344596589366,-22.4309730483565,39.3978017080178));
#181384=CARTESIAN_POINT('',(30.2311753956711,-52.9969317578288,39.3978017080178));
#181385=CARTESIAN_POINT('Origin',(5.5478765747851E-15,0.,39.3978017080178));
#181386=CARTESIAN_POINT('',(30.1558363500999,-52.8664407031057,39.3978017080178));
#181387=CARTESIAN_POINT('Origin',(5.5478765747851E-15,0.,39.3978017080178));
#181388=CARTESIAN_POINT('',(30.3416565762235,-53.1871522506176,39.2708017080178));
#181389=CARTESIAN_POINT('',(25.1949317876425,-55.80953951225,39.2708017081757));
#181390=CARTESIAN_POINT('Origin',(5.52999282761008E-15,0.,39.2708017080178));
#181391=CARTESIAN_POINT('',(25.261109401072,-55.9581731633345,38.9890000005756));
#181392=CARTESIAN_POINT('',(25.19493178753,-55.8095395120007,39.2708017080178));
#181393=CARTESIAN_POINT('',(25.2616268796456,-55.9579395562867,38.989));
#181394=CARTESIAN_POINT('Origin',(5.49031038273072E-15,0.,38.989));
#181395=CARTESIAN_POINT('',(30.422512342471,-53.3283370710513,38.989));
#181396=CARTESIAN_POINT('Origin',(5.49031038273072E-15,0.,38.989));
#181397=CARTESIAN_POINT('',(30.4230055008167,-53.3280557328687,38.9890000005754));
#181398=CARTESIAN_POINT('Origin',(5.49031038273072E-15,0.,38.989));
#181399=CARTESIAN_POINT('',(30.4230055009947,-53.3280557331496,38.989));
#181400=CARTESIAN_POINT('Origin',(62.2224557307631,0.,38.989));
#181401=CARTESIAN_POINT('',(25.4547063934082,-56.3916032444851,38.989));
#181402=CARTESIAN_POINT('',(10.5838037820516,-22.9910091182297,38.989));
#181403=CARTESIAN_POINT('',(30.6598643453574,-53.7394427993287,38.989));
#181404=CARTESIAN_POINT('Origin',(5.49031038273072E-15,0.,38.989));
#181405=CARTESIAN_POINT('',(30.422775050247,-53.3287920942668,38.989));
#181406=CARTESIAN_POINT('Origin',(5.57972911860581E-15,0.,39.624));
#181407=CARTESIAN_POINT('Origin',(24.6957545189376,-54.6869571488951,39.6240070731884));
#181408=CARTESIAN_POINT('Origin',(29.7268774036436,-52.1234719996036,39.6240070731883));
#181409=CARTESIAN_POINT('Origin',(5.57972911860581E-15,0.,39.624));
#181410=CARTESIAN_POINT('Origin',(25.470245661519,-56.4264225582401,39.5552135208038));
#181411=CARTESIAN_POINT('Origin',(30.6788998055465,-53.7724802568205,39.5552117598807));
#181412=CARTESIAN_POINT('Origin',(5.51210908043506E-15,0.,39.1438017080178));
#181413=CARTESIAN_POINT('Origin',(25.1123962626642,-55.6228532981804,39.1711625381332));
#181414=CARTESIAN_POINT('Origin',(30.2390901817301,-53.0105668578071,39.1712173702593));
#181415=CARTESIAN_POINT('Origin',(5.51210908043507E-15,0.,39.1438017080178));
#181416=CARTESIAN_POINT('Origin',(25.0381063693916,-55.4557927279735,39.1712175859357));
#181417=CARTESIAN_POINT('Origin',(30.1476018310217,-52.8522693417523,39.1711627526723));
#181418=CARTESIAN_POINT('Origin',(60.4792282238308,0.,38.989));
#181419=CARTESIAN_POINT('',(35.0124214764584,-48.7306271754177,38.989));
#181420=CARTESIAN_POINT('',(30.276808326888,-51.8059703131947,38.989));
#181421=CARTESIAN_POINT('Origin',(5.49031038273072E-15,0.,38.989));
#181422=CARTESIAN_POINT('',(30.5141604766046,-52.2170762957391,38.989));
#181423=CARTESIAN_POINT('',(15.3947701216591,-26.0295240215571,38.989));
#181424=CARTESIAN_POINT('',(30.5146599059377,-52.2167844420135,38.9889999995774));
#181425=CARTESIAN_POINT('Origin',(5.49031038273072E-15,0.,38.989));
#181426=CARTESIAN_POINT('',(35.2909759047567,-49.1150085644481,38.9889999997818));
#181427=CARTESIAN_POINT('Origin',(5.49031038273072E-15,0.,38.989));
#181428=CARTESIAN_POINT('',(35.2914456628186,-49.1146710209411,38.989));
#181429=CARTESIAN_POINT('Origin',(5.49031038273072E-15,0.,38.989));
#181430=CARTESIAN_POINT('',(35.012737468551,-48.7310621012209,38.989));
#181431=CARTESIAN_POINT('Origin',(5.49031038273072E-15,0.,38.989));
#181432=CARTESIAN_POINT('',(30.5960088312567,-52.3576880233163,39.2708017080178));
#181433=CARTESIAN_POINT('',(30.5146599055683,-52.2167844413816,38.989));
#181434=CARTESIAN_POINT('',(35.3866101429909,-49.246635155831,39.2708017078546));
#181435=CARTESIAN_POINT('Origin',(5.52999282761009E-15,0.,39.2708017080178));
#181436=CARTESIAN_POINT('',(35.3866101428259,-49.2466351556014,39.2708017080178));
#181437=CARTESIAN_POINT('Origin',(60.71525,0.,39.3978017080178));
#181438=CARTESIAN_POINT('',(35.5163757878395,-49.4242607783461,39.3978017080178));
#181439=CARTESIAN_POINT('',(30.7054974692368,-52.548481688396,39.3978017080178));
#181440=CARTESIAN_POINT('Origin',(5.5478765747851E-15,0.,39.3978017080178));
#181441=CARTESIAN_POINT('',(30.7811015270742,-52.6794317578288,39.3978017080178));
#181442=CARTESIAN_POINT('',(15.4537755657014,-26.1317244485615,39.3978017080178));
#181443=CARTESIAN_POINT('',(35.6052536882601,-49.5465907136145,39.3978017080178));
#181444=CARTESIAN_POINT('Origin',(5.5478765747851E-15,0.,39.3978017080178));
#181445=CARTESIAN_POINT('',(35.516687328443,-49.4246895772003,39.3978017080178));
#181446=CARTESIAN_POINT('Origin',(5.5478765747851E-15,0.,39.3978017080178));
#181447=CARTESIAN_POINT('',(35.7350130971388,-49.7242207306176,39.2708017080178));
#181448=CARTESIAN_POINT('',(30.8905967160115,-52.8702215134578,39.2708017081757));
#181449=CARTESIAN_POINT('Origin',(5.52999282761008E-15,0.,39.2708017080178));
#181450=CARTESIAN_POINT('',(30.971948248688,-53.0111234896154,38.9890000005756));
#181451=CARTESIAN_POINT('',(30.8905967158735,-52.8702215132217,39.2708017080178));
#181452=CARTESIAN_POINT('',(30.9724384738741,-53.0108370710513,38.989));
#181453=CARTESIAN_POINT('Origin',(5.49031038273072E-15,0.,38.989));
#181454=CARTESIAN_POINT('',(35.8301837593554,-49.8561803968404,38.989));
#181455=CARTESIAN_POINT('Origin',(5.49031038273072E-15,0.,38.989));
#181456=CARTESIAN_POINT('',(35.8306448082802,-49.8558490507737,38.9890000005754));
#181457=CARTESIAN_POINT('Origin',(5.49031038273072E-15,0.,38.989));
#181458=CARTESIAN_POINT('',(35.8306448084866,-49.8558490510345,38.989));
#181459=CARTESIAN_POINT('Origin',(62.2224557307631,0.,38.989));
#181460=CARTESIAN_POINT('',(31.2097904767605,-53.4219427993287,38.989));
#181461=CARTESIAN_POINT('',(15.8305769983922,-26.7843636743467,38.989));
#181462=CARTESIAN_POINT('',(36.1092077731528,-50.2402240048084,38.989));
#181463=CARTESIAN_POINT('Origin',(5.49031038273072E-15,0.,38.989));
#181464=CARTESIAN_POINT('',(35.8304925908681,-49.856605466951,38.989));
#181465=CARTESIAN_POINT('Origin',(5.57972911860581E-15,0.,39.624));
#181466=CARTESIAN_POINT('Origin',(30.2768121832815,-51.8059670065429,39.6240070731883));
#181467=CARTESIAN_POINT('Origin',(35.012416887145,-48.7306293534722,39.6240070731883));
#181468=CARTESIAN_POINT('Origin',(5.57972911860581E-15,0.,39.624));
#181469=CARTESIAN_POINT('Origin',(31.2288842284956,-53.4549470734246,39.5552135208005));
#181470=CARTESIAN_POINT('Origin',(36.1315923097622,-50.2710907322489,39.5552117598816));
#181471=CARTESIAN_POINT('Origin',(5.51210908043506E-15,0.,39.1438017080178));
#181472=CARTESIAN_POINT('Origin',(30.7889993062059,-52.6931852975948,39.1711625381365));
#181473=CARTESIAN_POINT('Origin',(35.6145503723398,-49.5593237986641,39.1712173702577));
#181474=CARTESIAN_POINT('Origin',(5.51210908043507E-15,0.,39.1438017080178));
#181475=CARTESIAN_POINT('Origin',(30.6976537960619,-52.5348053110497,39.171217585938));
#181476=CARTESIAN_POINT('Origin',(35.5070166083004,-49.4114565896691,39.1711627526733));
#181477=CARTESIAN_POINT('Origin',(60.4792282238308,0.,38.989));
#181478=CARTESIAN_POINT('',(39.9143573409156,-44.8038810887675,38.989));
#181479=CARTESIAN_POINT('',(35.5261472678865,-48.357383540212,38.989));
#181480=CARTESIAN_POINT('Origin',(5.49031038273072E-15,0.,38.989));
#181481=CARTESIAN_POINT('',(35.8051714542879,-48.7414273857062,38.989));
#181482=CARTESIAN_POINT('',(21.151922343707,-28.5729602337851,38.989));
#181483=CARTESIAN_POINT('',(35.8056376406738,-48.7410849262057,38.988999999577));
#181484=CARTESIAN_POINT('Origin',(5.49031038273072E-15,0.,38.989));
#181485=CARTESIAN_POINT('',(40.2315646148142,-45.1570399300039,38.9889999997818));
#181486=CARTESIAN_POINT('Origin',(5.49031038273072E-15,0.,38.989));
#181487=CARTESIAN_POINT('',(40.2319965165881,-45.1566551325072,38.989));
#181488=CARTESIAN_POINT('Origin',(5.49031038273072E-15,0.,38.989));
#181489=CARTESIAN_POINT('',(39.9147170640963,-44.8042806018338,38.989));
#181490=CARTESIAN_POINT('Origin',(5.49031038273072E-15,0.,38.989));
#181491=CARTESIAN_POINT('',(35.9012693628904,-48.8727133447944,39.2708017080178));
#181492=CARTESIAN_POINT('',(35.80563764024,-48.7410849256152,38.989));
#181493=CARTESIAN_POINT('',(40.3404336840073,-45.2779489571884,39.2708017078546));
#181494=CARTESIAN_POINT('Origin',(5.52999282761009E-15,0.,39.2708017080178));
#181495=CARTESIAN_POINT('',(40.3404336838192,-45.2779489569773,39.2708017080178));
#181496=CARTESIAN_POINT('Origin',(60.71525,0.,39.3978017080178));
#181497=CARTESIAN_POINT('',(40.4880553924343,-45.4410373245173,39.3978017080178));
#181498=CARTESIAN_POINT('',(36.0301015792676,-49.0510171431404,39.3978017080178));
#181499=CARTESIAN_POINT('Origin',(5.5478765747851E-15,0.,39.3978017080178));
#181500=CARTESIAN_POINT('',(36.1189794796882,-49.1733470784088,39.3978017080178));
#181501=CARTESIAN_POINT('',(21.2334658618522,-28.6851952578918,39.3978017080178));
#181502=CARTESIAN_POINT('',(40.5892333705622,-45.5534068532512,39.3978017080178));
#181503=CARTESIAN_POINT('Origin',(5.5478765747851E-15,0.,39.3978017080178));
#181504=CARTESIAN_POINT('',(40.488410048071,-45.4414312095059,39.3978017080178));
#181505=CARTESIAN_POINT('Origin',(5.5478765747851E-15,0.,39.3978017080178));
#181506=CARTESIAN_POINT('',(40.7368493365296,-45.7165002428308,39.2708017080178));
#181507=CARTESIAN_POINT('',(36.2478178024869,-49.351646303959,39.2708017081757));
#181508=CARTESIAN_POINT('Origin',(5.52999282761008E-15,0.,39.2708017080178));
#181509=CARTESIAN_POINT('',(36.3434519499946,-49.4832728536532,38.9890000005756));
#181510=CARTESIAN_POINT('',(36.247817802325,-49.3516463037386,39.2708017080178));
#181511=CARTESIAN_POINT('',(36.3439095507835,-49.4829367616347,38.989));
#181512=CARTESIAN_POINT('Origin',(5.49031038273072E-15,0.,38.989));
#181513=CARTESIAN_POINT('',(40.8452921850243,-45.8377889771252,38.989));
#181514=CARTESIAN_POINT('Origin',(5.49031038273072E-15,0.,38.989));
#181515=CARTESIAN_POINT('',(40.8457160731797,-45.8374112534714,38.9890000005754));
#181516=CARTESIAN_POINT('Origin',(5.49031038273072E-15,0.,38.989));
#181517=CARTESIAN_POINT('',(40.8457160734122,-45.8374112537091,38.989));
#181518=CARTESIAN_POINT('Origin',(62.2224557307631,0.,38.989));
#181519=CARTESIAN_POINT('',(36.6229335645808,-49.8669803696027,38.989));
#181520=CARTESIAN_POINT('',(21.7541926348211,-29.4019141737116,38.989));
#181521=CARTESIAN_POINT('',(41.162931164248,-46.1905628026486,38.989));
#181522=CARTESIAN_POINT('Origin',(5.49031038273072E-15,0.,38.989));
#181523=CARTESIAN_POINT('',(40.8456437566512,-45.8381794369738,38.989));
#181524=CARTESIAN_POINT('Origin',(5.57972911860581E-15,0.,39.624));
#181525=CARTESIAN_POINT('Origin',(35.5261507575148,-48.3573798485716,39.6240070731883));
#181526=CARTESIAN_POINT('Origin',(39.9143530044118,-44.8038837346041,39.6240070731883));
#181527=CARTESIAN_POINT('Origin',(5.57972911860581E-15,0.,39.624));
#181528=CARTESIAN_POINT('Origin',(36.6453726047983,-49.8978080023045,39.5552135208014));
#181529=CARTESIAN_POINT('Origin',(41.188419527604,-46.2189206177181,39.5552117598817));
#181530=CARTESIAN_POINT('Origin',(5.51210908043506E-15,0.,39.1438017080178));
#181531=CARTESIAN_POINT('Origin',(36.128271630334,-49.1861997321268,39.1711625381318));
#181532=CARTESIAN_POINT('Origin',(40.5998100962481,-45.5650984170299,39.171217370262));
#181533=CARTESIAN_POINT('Origin',(5.51210908043507E-15,0.,39.1438017080178));
#181534=CARTESIAN_POINT('Origin',(36.0208713038458,-49.0382355735244,39.1712175859395));
#181535=CARTESIAN_POINT('Origin',(40.4774090812916,-45.4292815791814,39.171162752675));
#181536=CARTESIAN_POINT('Origin',(60.4792282238308,0.,38.989));
#181537=CARTESIAN_POINT('',(44.3789831537295,-40.3862543050939,38.989));
#181538=CARTESIAN_POINT('',(40.3862543050938,-44.3789831537296,38.989));
#181539=CARTESIAN_POINT('Origin',(5.49031038273072E-15,0.,38.989));
#181540=CARTESIAN_POINT('',(40.7038934808042,-44.731757197436,38.989));
#181541=CARTESIAN_POINT('',(27.314662201079,-29.8615093742683,38.989));
#181542=CARTESIAN_POINT('',(40.7043213166065,-44.7313678842174,38.9889999995774));
#181543=CARTESIAN_POINT('Origin',(5.49031038273072E-15,0.,38.989));
#181544=CARTESIAN_POINT('',(44.7313678839555,-40.7043213163684,38.9889999997818));
#181545=CARTESIAN_POINT('Origin',(5.49031038273072E-15,0.,38.989));
#181546=CARTESIAN_POINT('',(44.7317571974354,-40.703893480804,38.989));
#181547=CARTESIAN_POINT('Origin',(5.49031038273072E-15,0.,38.989));
#181548=CARTESIAN_POINT('',(44.3793826667958,-40.3866140282746,38.989));
#181549=CARTESIAN_POINT('Origin',(5.49031038273072E-15,0.,38.989));
#181550=CARTESIAN_POINT('',(40.8131880745606,-44.8522789915942,39.2708017080178));
#181551=CARTESIAN_POINT('',(40.7043213161139,-44.7313678836761,38.989));
#181552=CARTESIAN_POINT('',(44.8522789918032,-40.813188074751,39.2708017078546));
#181553=CARTESIAN_POINT('Origin',(5.52999282761009E-15,0.,39.2708017080178));
#181554=CARTESIAN_POINT('',(44.8522789915941,-40.8131880745607,39.2708017080178));
#181555=CARTESIAN_POINT('Origin',(60.71525,0.,39.3978017080178));
#181556=CARTESIAN_POINT('',(45.0161393894793,-40.9599523566126,39.3978017080178));
#181557=CARTESIAN_POINT('',(40.9599523566124,-45.0161393894794,39.3978017080178));
#181558=CARTESIAN_POINT('Origin',(5.5478765747851E-15,0.,39.3978017080178));
#181559=CARTESIAN_POINT('',(41.0611303347403,-45.1285089182133,39.3978017080178));
#181560=CARTESIAN_POINT('',(27.4203375923833,-29.9788737863603,39.3978017080178));
#181561=CARTESIAN_POINT('',(45.1285089182132,-41.0611303347405,39.3978017080178));
#181562=CARTESIAN_POINT('Origin',(5.5478765747851E-15,0.,39.3978017080178));
#181563=CARTESIAN_POINT('',(45.0165332744679,-40.9603070122493,39.3978017080178));
#181564=CARTESIAN_POINT('Origin',(5.5478765747851E-15,0.,39.3978017080178));
#181565=CARTESIAN_POINT('',(45.2923641298556,-41.2079002115908,39.2708017080178));
#181566=CARTESIAN_POINT('',(41.2079002117747,-45.2923641300581,39.2708017081757));
#181567=CARTESIAN_POINT('Origin',(5.52999282761008E-15,0.,39.2708017080178));
#181568=CARTESIAN_POINT('',(41.3167691863808,-45.4132731252659,38.9890000005756));
#181569=CARTESIAN_POINT('',(41.2079002115907,-45.2923641298558,39.2708017080178));
#181570=CARTESIAN_POINT('',(41.3171891492024,-45.4128910420873,38.989));
#181571=CARTESIAN_POINT('Origin',(5.49031038273072E-15,0.,38.989));
#181572=CARTESIAN_POINT('',(45.4128910420872,-41.3171891492026,38.989));
#181573=CARTESIAN_POINT('Origin',(5.49031038273072E-15,0.,38.989));
#181574=CARTESIAN_POINT('',(45.4132731252658,-41.316769186381,38.9890000005754));
#181575=CARTESIAN_POINT('Origin',(5.49031038273072E-15,0.,38.989));
#181576=CARTESIAN_POINT('',(45.4132731255219,-41.3167691865932,38.989));
#181577=CARTESIAN_POINT('Origin',(62.2224557307631,0.,38.989));
#181578=CARTESIAN_POINT('',(41.6348281284261,-45.7656648676107,38.989));
#181579=CARTESIAN_POINT('',(28.0951675083324,-30.7283483363945,38.989));
#181580=CARTESIAN_POINT('',(45.7656648676106,-41.6348281284263,38.989));
#181581=CARTESIAN_POINT('Origin',(5.49031038273072E-15,0.,38.989));
#181582=CARTESIAN_POINT('',(45.4132815019358,-41.3175407208294,38.989));
#181583=CARTESIAN_POINT('Origin',(5.57972911860581E-15,0.,39.624));
#181584=CARTESIAN_POINT('Origin',(40.3862573897243,-44.3789791175468,39.6240070731883));
#181585=CARTESIAN_POINT('Origin',(44.3789791175466,-40.3862573897245,39.6240070731883));
#181586=CARTESIAN_POINT('Origin',(5.57972911860581E-15,0.,39.624));
#181587=CARTESIAN_POINT('Origin',(41.6603666103054,-45.7939781049239,39.5552135208022));
#181588=CARTESIAN_POINT('Origin',(45.793977801882,-41.6603663369584,39.5552117598818));
#181589=CARTESIAN_POINT('Origin',(5.51210908043506E-15,0.,39.1438017080178));
#181590=CARTESIAN_POINT('Origin',(41.0717150501549,-45.1403198695223,39.1711625381316));
#181591=CARTESIAN_POINT('Origin',(45.1402498046834,-41.0716522820265,39.1712173702609));
#181592=CARTESIAN_POINT('Origin',(5.51210908043507E-15,0.,39.1438017080178));
#181593=CARTESIAN_POINT('Origin',(40.9494366077774,-45.0043926651421,39.1712175859395));
#181594=CARTESIAN_POINT('Origin',(45.0043225899499,-40.9493738530219,39.171162752674));
#181595=CARTESIAN_POINT('Origin',(60.4792282238308,0.,38.989));
#181596=CARTESIAN_POINT('',(48.3573835402119,-35.5261472678866,38.989));
#181597=CARTESIAN_POINT('',(44.8038810887674,-39.9143573409157,38.989));
#181598=CARTESIAN_POINT('Origin',(5.49031038273072E-15,0.,38.989));
#181599=CARTESIAN_POINT('',(45.1566551325075,-40.2319965165887,38.989));
#181600=CARTESIAN_POINT('',(33.6129634723596,-29.8380098596982,38.989));
#181601=CARTESIAN_POINT('',(45.1570399302684,-40.2315646150501,38.9889999995771));
#181602=CARTESIAN_POINT('Origin',(5.49031038273072E-15,0.,38.989));
#181603=CARTESIAN_POINT('',(48.7410849259197,-35.805637640464,38.9889999997818));
#181604=CARTESIAN_POINT('Origin',(5.49031038273072E-15,0.,38.989));
#181605=CARTESIAN_POINT('',(48.7414273857055,-35.8051714542877,38.989));
#181606=CARTESIAN_POINT('Origin',(5.49031038273072E-15,0.,38.989));
#181607=CARTESIAN_POINT('',(48.3578184660151,-35.5264632599792,38.989));
#181608=CARTESIAN_POINT('Origin',(5.49031038273072E-15,0.,38.989));
#181609=CARTESIAN_POINT('',(45.2779489569772,-40.3404336838193,39.2708017080178));
#181610=CARTESIAN_POINT('',(45.1570399297215,-40.2315646145628,38.989));
#181611=CARTESIAN_POINT('',(48.8727133450222,-35.9012693630579,39.2708017078546));
#181612=CARTESIAN_POINT('Origin',(5.52999282761009E-15,0.,39.2708017080178));
#181613=CARTESIAN_POINT('',(48.8727133447943,-35.9012693628905,39.2708017080178));
#181614=CARTESIAN_POINT('Origin',(60.71525,0.,39.3978017080178));
#181615=CARTESIAN_POINT('',(49.0510171431403,-36.0301015792677,39.3978017080178));
#181616=CARTESIAN_POINT('',(45.4410373245171,-40.4880553924344,39.3978017080178));
#181617=CARTESIAN_POINT('Origin',(5.5478765747851E-15,0.,39.3978017080178));
#181618=CARTESIAN_POINT('',(45.5534068532511,-40.5892333705623,39.3978017080178));
#181619=CARTESIAN_POINT('',(33.7433098572246,-29.9553742717902,39.3978017080178));
#181620=CARTESIAN_POINT('',(49.1733470784087,-36.1189794796884,39.3978017080178));
#181621=CARTESIAN_POINT('Origin',(5.5478765747851E-15,0.,39.3978017080178));
#181622=CARTESIAN_POINT('',(49.0514459419945,-36.0304131198712,39.3978017080178));
#181623=CARTESIAN_POINT('Origin',(5.5478765747851E-15,0.,39.3978017080178));
#181624=CARTESIAN_POINT('',(49.3516463037384,-36.2478178023251,39.2708017080178));
#181625=CARTESIAN_POINT('',(45.7165002430348,-40.7368493367117,39.2708017081757));
#181626=CARTESIAN_POINT('Origin',(5.52999282761008E-15,0.,39.2708017080178));
#181627=CARTESIAN_POINT('',(45.8374112534712,-40.8457160731798,38.9890000005756));
#181628=CARTESIAN_POINT('',(45.7165002428306,-40.7368493365298,39.2708017080178));
#181629=CARTESIAN_POINT('',(45.8377889771251,-40.8452921850244,38.989));
#181630=CARTESIAN_POINT('Origin',(5.49031038273072E-15,0.,38.989));
#181631=CARTESIAN_POINT('',(49.4829367616345,-36.3439095507836,38.989));
#181632=CARTESIAN_POINT('Origin',(5.49031038273072E-15,0.,38.989));
#181633=CARTESIAN_POINT('',(49.4832728536532,-36.3434519499948,38.9890000005754));
#181634=CARTESIAN_POINT('Origin',(5.49031038273072E-15,0.,38.989));
#181635=CARTESIAN_POINT('',(49.48327285393,-36.3434519501791,38.989));
#181636=CARTESIAN_POINT('Origin',(62.2224557307631,0.,38.989));
#181637=CARTESIAN_POINT('',(46.1905628026484,-41.1629311642481,38.989));
#181638=CARTESIAN_POINT('',(34.5756856720385,-30.7048488218244,38.989));
#181639=CARTESIAN_POINT('',(49.8669803696025,-36.622933564581,38.989));
#181640=CARTESIAN_POINT('Origin',(5.49031038273072E-15,0.,38.989));
#181641=CARTESIAN_POINT('',(49.4833618317452,-36.3442183822964,38.989));
#181642=CARTESIAN_POINT('Origin',(5.57972911860581E-15,0.,39.624));
#181643=CARTESIAN_POINT('Origin',(44.803883734604,-39.9143530044119,39.6240070731883));
#181644=CARTESIAN_POINT('Origin',(48.3573798485713,-35.5261507575154,39.6240070731883));
#181645=CARTESIAN_POINT('Origin',(5.57972911860581E-15,0.,39.624));
#181646=CARTESIAN_POINT('Origin',(46.2189209212412,-41.1884198004176,39.5552135208008));
#181647=CARTESIAN_POINT('Origin',(49.8978076723516,-36.6453723646222,39.5552117598824));
#181648=CARTESIAN_POINT('Origin',(5.51210908043506E-15,0.,39.1438017080178));
#181649=CARTESIAN_POINT('Origin',(45.5651681650756,-40.5998732162064,39.1711625381287));
#181650=CARTESIAN_POINT('Origin',(49.1861234900558,-36.1282165298268,39.1712173702623));
#181651=CARTESIAN_POINT('Origin',(5.51210908043507E-15,0.,39.1438017080178));
#181652=CARTESIAN_POINT('Origin',(45.4293513150133,-40.4774722129475,39.1712175859372));
#181653=CARTESIAN_POINT('Origin',(49.0381593225499,-36.0208162177252,39.1711627526725));
#181654=CARTESIAN_POINT('Origin',(60.4792282238308,0.,38.989));
#181655=CARTESIAN_POINT('',(51.8059703131946,-30.2768083268882,38.989));
#181656=CARTESIAN_POINT('',(48.7306271754176,-35.0124214764585,38.989));
#181657=CARTESIAN_POINT('Origin',(5.49031038273072E-15,0.,38.989));
#181658=CARTESIAN_POINT('',(49.1146710209415,-35.2914456628191,38.989));
#181659=CARTESIAN_POINT('',(39.7707905934405,-28.502719155674,38.989));
#181660=CARTESIAN_POINT('',(49.1150085647358,-35.2909759049637,38.9889999995772));
#181661=CARTESIAN_POINT('Origin',(5.49031038273072E-15,0.,38.989));
#181662=CARTESIAN_POINT('',(52.2167844417078,-30.5146599057592,38.9889999997818));
#181663=CARTESIAN_POINT('Origin',(5.49031038273072E-15,0.,38.989));
#181664=CARTESIAN_POINT('',(52.2170762957385,-30.5141604766045,38.989));
#181665=CARTESIAN_POINT('Origin',(5.49031038273072E-15,0.,38.989));
#181666=CARTESIAN_POINT('',(51.8064358865966,-30.2770771258171,38.989));
#181667=CARTESIAN_POINT('Origin',(5.49031038273072E-15,0.,38.989));
#181668=CARTESIAN_POINT('',(49.2466351556012,-35.386610142826,39.2708017080178));
#181669=CARTESIAN_POINT('',(49.115008564141,-35.2909759045363,38.989));
#181670=CARTESIAN_POINT('',(52.3576880235603,-30.5960088313996,39.2708017078546));
#181671=CARTESIAN_POINT('Origin',(5.52999282761009E-15,0.,39.2708017080178));
#181672=CARTESIAN_POINT('',(52.3576880233162,-30.5960088312569,39.2708017080178));
#181673=CARTESIAN_POINT('Origin',(60.71525,0.,39.3978017080178));
#181674=CARTESIAN_POINT('',(52.5484816883959,-30.705497469237,39.3978017080178));
#181675=CARTESIAN_POINT('',(49.424260778346,-35.5163757878396,39.3978017080178));
#181676=CARTESIAN_POINT('Origin',(5.5478765747851E-15,0.,39.3978017080178));
#181677=CARTESIAN_POINT('',(49.5465907136144,-35.6052536882603,39.3978017080178));
#181678=CARTESIAN_POINT('',(39.9252688514646,-28.6149541797807,39.3978017080178));
#181679=CARTESIAN_POINT('',(52.6794317578287,-30.7811015270744,39.3978017080178));
#181680=CARTESIAN_POINT('Origin',(5.5478765747851E-15,0.,39.3978017080178));
#181681=CARTESIAN_POINT('',(52.5489407031056,-30.7057624815032,39.3978017080178));
#181682=CARTESIAN_POINT('Origin',(5.5478765747851E-15,0.,39.3978017080178));
#181683=CARTESIAN_POINT('',(52.8702215132216,-30.8905967158737,39.2708017080178));
#181684=CARTESIAN_POINT('',(49.7242207308395,-35.7350130972986,39.2708017081757));
#181685=CARTESIAN_POINT('Origin',(5.52999282761008E-15,0.,39.2708017080178));
#181686=CARTESIAN_POINT('',(49.8558490507736,-35.8306448082803,38.9890000005756));
#181687=CARTESIAN_POINT('',(49.7242207306174,-35.735013097139,39.2708017080178));
#181688=CARTESIAN_POINT('',(49.8561803968403,-35.8301837593555,38.989));
#181689=CARTESIAN_POINT('Origin',(5.49031038273072E-15,0.,38.989));
#181690=CARTESIAN_POINT('',(53.0108370710512,-30.9724384738743,38.989));
#181691=CARTESIAN_POINT('Origin',(5.49031038273072E-15,0.,38.989));
#181692=CARTESIAN_POINT('',(53.0111234896153,-30.9719482486883,38.9890000005754));
#181693=CARTESIAN_POINT('Origin',(5.49031038273072E-15,0.,38.989));
#181694=CARTESIAN_POINT('',(53.01112348991,-30.9719482488426,38.989));
#181695=CARTESIAN_POINT('Origin',(62.2224557307631,0.,38.989));
#181696=CARTESIAN_POINT('',(50.2402240048083,-36.1092077731529,38.989));
#181697=CARTESIAN_POINT('',(40.9117478092586,-29.3316730956005,38.989));
#181698=CARTESIAN_POINT('',(53.4219427993286,-31.2097904767607,38.989));
#181699=CARTESIAN_POINT('Origin',(5.49031038273072E-15,0.,38.989));
#181700=CARTESIAN_POINT('',(53.0112920942667,-30.9727011816503,38.989));
#181701=CARTESIAN_POINT('Origin',(5.57972911860581E-15,0.,39.624));
#181702=CARTESIAN_POINT('Origin',(48.7306293534718,-35.0124168871455,39.6240070731883));
#181703=CARTESIAN_POINT('Origin',(51.8059670065428,-30.2768121832818,39.6240070731883));
#181704=CARTESIAN_POINT('Origin',(5.57972911860581E-15,0.,39.624));
#181705=CARTESIAN_POINT('Origin',(50.2710910626291,-36.1315925493507,39.5552135208));
#181706=CARTESIAN_POINT('Origin',(53.4549467201732,-31.2288840241294,39.5552117598782));
#181707=CARTESIAN_POINT('Origin',(5.51210908043506E-15,0.,39.1438017080178));
#181708=CARTESIAN_POINT('Origin',(49.5593997624581,-35.6146058558666,39.1711625381308));
#181709=CARTESIAN_POINT('Origin',(52.6931037136124,-30.7889524770104,39.1712173702627));
#181710=CARTESIAN_POINT('Origin',(5.51210908043507E-15,0.,39.1438017080178));
#181711=CARTESIAN_POINT('Origin',(49.4115325425387,-35.507072104731,39.171217585936));
#181712=CARTESIAN_POINT('Origin',(52.5347237197204,-30.6976069821028,39.1711627526715));
#181713=CARTESIAN_POINT('Origin',(60.4792282238308,0.,38.989));
#181714=CARTESIAN_POINT('',(54.6869600343297,-24.6957503380308,38.989));
#181715=CARTESIAN_POINT('',(52.1234703131946,-29.726882195485,38.989));
#181716=CARTESIAN_POINT('Origin',(5.49031038273072E-15,0.,38.989));
#181717=CARTESIAN_POINT('',(52.5345762957643,-29.9642343451579,38.989));
#181718=CARTESIAN_POINT('',(45.518171167873,-25.9133109558556,38.989));
#181719=CARTESIAN_POINT('',(52.5348628873914,-29.9637318777509,38.9889999995773));
#181720=CARTESIAN_POINT('Origin',(5.49031038273072E-15,0.,38.989));
#181721=CARTESIAN_POINT('',(55.1203859400879,-24.8893571715239,38.9889999997818));
#181722=CARTESIAN_POINT('Origin',(5.49031038273072E-15,0.,38.989));
#181723=CARTESIAN_POINT('',(55.1206239907496,-24.888829971241,38.989));
#181724=CARTESIAN_POINT('Origin',(5.49031038273072E-15,0.,38.989));
#181725=CARTESIAN_POINT('',(54.6874511544109,-24.6959689987789,38.989));
#181726=CARTESIAN_POINT('Origin',(5.49031038273072E-15,0.,38.989));
#181727=CARTESIAN_POINT('',(52.6757649139395,-30.0450834959837,39.2708017080178));
#181728=CARTESIAN_POINT('',(52.5348628867555,-29.9637318773882,38.989));
#181729=CARTESIAN_POINT('',(55.2690209155617,-24.9555320243579,39.2708017078546));
#181730=CARTESIAN_POINT('Origin',(5.52999282761009E-15,0.,39.2708017080178));
#181731=CARTESIAN_POINT('',(55.269020915304,-24.9555320242416,39.2708017080178));
#181732=CARTESIAN_POINT('Origin',(60.71525,0.,39.3978017080178));
#181733=CARTESIAN_POINT('',(55.4702140717966,-25.0444775033948,39.3978017080178));
#181734=CARTESIAN_POINT('',(52.8659816883959,-30.1555713378339,39.3978017080178));
#181735=CARTESIAN_POINT('Origin',(5.5478765747851E-15,0.,39.3978017080178));
#181736=CARTESIAN_POINT('',(52.9969317578287,-30.2311753956713,39.3978017080178));
#181737=CARTESIAN_POINT('',(45.6951875,-26.0155113828601,39.3978017080178));
#181738=CARTESIAN_POINT('',(55.6083495590301,-25.1059793847702,39.3978017080178));
#181739=CARTESIAN_POINT('Origin',(5.5478765747851E-15,0.,39.3978017080178));
#181740=CARTESIAN_POINT('',(55.4706982733007,-25.0446930837939,39.3978017080178));
#181741=CARTESIAN_POINT('Origin',(5.5478765747851E-15,0.,39.3978017080178));
#181742=CARTESIAN_POINT('',(55.8095395120007,-25.1949317875302,39.2708017080178));
#181743=CARTESIAN_POINT('',(53.187152250855,-30.3416565763592,39.2708017081757));
#181744=CARTESIAN_POINT('Origin',(5.52999282761008E-15,0.,39.2708017080178));
#181745=CARTESIAN_POINT('',(53.3280557328685,-30.4230055008168,38.9890000005756));
#181746=CARTESIAN_POINT('',(53.1871522506175,-30.3416565762237,39.2708017080178));
#181747=CARTESIAN_POINT('',(53.3283370710512,-30.4225123424712,38.989));
#181748=CARTESIAN_POINT('Origin',(5.49031038273072E-15,0.,38.989));
#181749=CARTESIAN_POINT('',(55.9579395562866,-25.2616268796457,38.989));
#181750=CARTESIAN_POINT('Origin',(5.49031038273072E-15,0.,38.989));
#181751=CARTESIAN_POINT('',(55.9581731633345,-25.2611094010722,38.9890000005754));
#181752=CARTESIAN_POINT('Origin',(5.49031038273072E-15,0.,38.989));
#181753=CARTESIAN_POINT('',(55.9581731636437,-25.2611094011949,38.989));
#181754=CARTESIAN_POINT('Origin',(62.2224557307631,0.,38.989));
#181755=CARTESIAN_POINT('',(53.7394427993286,-30.6598643453575,38.989));
#181756=CARTESIAN_POINT('',(46.8255917980722,-26.6681506086452,38.989));
#181757=CARTESIAN_POINT('',(56.391603244485,-25.4547063934084,38.989));
#181758=CARTESIAN_POINT('Origin',(5.49031038273072E-15,0.,38.989));
#181759=CARTESIAN_POINT('',(55.9584195472775,-25.2618405854036,38.989));
#181760=CARTESIAN_POINT('Origin',(5.57972911860581E-15,0.,39.624));
#181761=CARTESIAN_POINT('Origin',(52.1234719996035,-29.7268774036438,39.6240070731883));
#181762=CARTESIAN_POINT('Origin',(54.6869571488949,-24.695754518938,39.6240070731883));
#181763=CARTESIAN_POINT('Origin',(5.57972911860581E-15,0.,39.624));
#181764=CARTESIAN_POINT('Origin',(53.7724806104346,-30.6789000092877,39.5552135208009));
#181765=CARTESIAN_POINT('Origin',(56.4264221855611,-25.4702454951992,39.5552117598807));
#181766=CARTESIAN_POINT('Origin',(5.51210908043506E-15,0.,39.1438017080178));
#181767=CARTESIAN_POINT('Origin',(53.0106482050716,-30.2391374209339,39.1711625381337));
#181768=CARTESIAN_POINT('Origin',(55.6227672661409,-25.1123582178528,39.1712173702621));
#181769=CARTESIAN_POINT('Origin',(5.51210908043507E-15,0.,39.1438017080178));
#181770=CARTESIAN_POINT('Origin',(52.852350679497,-30.1476490842092,39.1712175859328));
#181771=CARTESIAN_POINT('Origin',(55.4557066902172,-25.038068340499,39.1711627526733));
#181772=CARTESIAN_POINT('Origin',(60.4792282238308,0.,38.989));
#181773=CARTESIAN_POINT('',(56.9687879773466,-18.844120540552,38.989));
#181774=CARTESIAN_POINT('',(54.9452378026828,-24.1156489724277,38.989));
#181775=CARTESIAN_POINT('Origin',(5.49031038273072E-15,0.,38.989));
#181776=CARTESIAN_POINT('',(55.3789017591239,-24.308728605592,38.989));
#181777=CARTESIAN_POINT('',(50.6030043228557,-22.1823620689016,38.989));
#181778=CARTESIAN_POINT('',(55.3791342586264,-24.3081989337718,38.9889999995772));
#181779=CARTESIAN_POINT('Origin',(5.49031038273072E-15,0.,38.989));
#181780=CARTESIAN_POINT('',(57.4200769554261,-18.9913614316845,38.9889999997818));
#181781=CARTESIAN_POINT('Origin',(5.49031038273072E-15,0.,38.989));
#181782=CARTESIAN_POINT('',(57.420258594586,-18.9908122363901,38.989));
#181783=CARTESIAN_POINT('Origin',(5.49031038273072E-15,0.,38.989));
#181784=CARTESIAN_POINT('',(56.9692992632926,-18.8442866674262,38.989));
#181785=CARTESIAN_POINT('Origin',(5.49031038273072E-15,0.,38.989));
#181786=CARTESIAN_POINT('',(55.5277679687683,-24.3743766270215,39.2708017080178));
#181787=CARTESIAN_POINT('',(55.3791342579558,-24.3081989334774,38.989));
#181788=CARTESIAN_POINT('',(57.574814848626,-19.0416371861766,39.2708017078546));
#181789=CARTESIAN_POINT('Origin',(5.52999282761009E-15,0.,39.2708017080178));
#181790=CARTESIAN_POINT('',(57.5748148483576,-19.0416371860878,39.2708017080178));
#181791=CARTESIAN_POINT('Origin',(60.71525,0.,39.3978017080178));
#181792=CARTESIAN_POINT('',(57.7842031819382,-19.1090650011316,39.3978017080178));
#181793=CARTESIAN_POINT('',(55.7284918401498,-24.4643761377918,39.3978017080178));
#181794=CARTESIAN_POINT('Origin',(5.5478765747851E-15,0.,39.3978017080178));
#181795=CARTESIAN_POINT('',(55.8666273273833,-24.5258780191672,39.3978017080178));
#181796=CARTESIAN_POINT('',(50.7999799080414,-22.2700612497317,39.3978017080178));
#181797=CARTESIAN_POINT('',(57.9280106456676,-19.1557908785626,39.3978017080178));
#181798=CARTESIAN_POINT('Origin',(5.5478765747851E-15,0.,39.3978017080178));
#181799=CARTESIAN_POINT('',(57.7847072652236,-19.1092287877196,39.3978017080178));
#181800=CARTESIAN_POINT('Origin',(5.5478765747851E-15,0.,39.3978017080178));
#181801=CARTESIAN_POINT('',(58.1373965169893,-19.223225914144,39.2708017080178));
#181802=CARTESIAN_POINT('',(56.067354200683,-24.6158705165694,39.2708017081757));
#181803=CARTESIAN_POINT('Origin',(5.52999282761008E-15,0.,39.2708017080178));
#181804=CARTESIAN_POINT('',(56.2159890767411,-24.6820453786632,38.9890000005756));
#181805=CARTESIAN_POINT('',(56.0673542004326,-24.6158705164594,39.2708017080178));
#181806=CARTESIAN_POINT('',(56.2162173246397,-24.6815255140427,38.989));
#181807=CARTESIAN_POINT('Origin',(5.49031038273072E-15,0.,38.989));
#181808=CARTESIAN_POINT('',(58.2919551457916,-19.2740436149885,38.989));
#181809=CARTESIAN_POINT('Origin',(5.49031038273072E-15,0.,38.989));
#181810=CARTESIAN_POINT('',(58.2921333818757,-19.273504552631,38.9890000005754));
#181811=CARTESIAN_POINT('Origin',(5.49031038273072E-15,0.,38.989));
#181812=CARTESIAN_POINT('',(58.2921333821959,-19.2735045527207,38.989));
#181813=CARTESIAN_POINT('Origin',(62.2224557307631,0.,38.989));
#181814=CARTESIAN_POINT('',(56.6498810128382,-24.8746050278053,38.989));
#181815=CARTESIAN_POINT('',(52.0578415156894,-22.8300973196049,38.989));
#181816=CARTESIAN_POINT('',(58.7434254837932,-19.4207352200701,38.989));
#181817=CARTESIAN_POINT('Origin',(5.49031038273072E-15,0.,38.989));
#181818=CARTESIAN_POINT('',(58.2924548456761,-19.2742059773232,38.989));
#181819=CARTESIAN_POINT('Origin',(5.57972911860581E-15,0.,39.624));
#181820=CARTESIAN_POINT('Origin',(54.9452389789695,-24.1156440305593,39.6240070731883));
#181821=CARTESIAN_POINT('Origin',(56.9687855447424,-18.8441250001657,39.6240070731883));
#181822=CARTESIAN_POINT('Origin',(5.57972911860581E-15,0.,39.624));
#181823=CARTESIAN_POINT('Origin',(56.6847276080575,-24.8900830207517,39.5552135207979));
#181824=CARTESIAN_POINT('Origin',(58.7796779614986,-19.4325496266341,39.5552117598785));
#181825=CARTESIAN_POINT('Origin',(5.51210908043506E-15,0.,39.1438017080178));
#181826=CARTESIAN_POINT('Origin',(55.881100892759,-24.5323626684708,39.1711625381347));
#181827=CARTESIAN_POINT('Origin',(57.9430161406909,-19.1606277069622,39.1712173702642));
#181828=CARTESIAN_POINT('Origin',(5.51210908043507E-15,0.,39.1438017080178));
#181829=CARTESIAN_POINT('Origin',(55.7141074023426,-24.4579221115153,39.1712175859392));
#181830=CARTESIAN_POINT('Origin',(57.7691053333641,-19.1042073825995,39.1711627526757));
#181831=CARTESIAN_POINT('Origin',(60.4792282238308,0.,38.989));
#181832=CARTESIAN_POINT('',(58.6264539577984,-12.7860306150452,38.989));
#181833=CARTESIAN_POINT('',(57.1650137687747,-18.2401996527046,38.989));
#181834=CARTESIAN_POINT('Origin',(5.49031038273072E-15,0.,38.989));
#181835=CARTESIAN_POINT('',(57.6164843860303,-18.3868913484948,38.989));
#181836=CARTESIAN_POINT('',(54.8020887275094,-17.4724387660755,38.989));
#181837=CARTESIAN_POINT('',(57.6166602460947,-18.3863402754565,38.9889999995772));
#181838=CARTESIAN_POINT('Origin',(5.49031038273072E-15,0.,38.989));
#181839=CARTESIAN_POINT('',(59.0906615917171,-12.8852923618017,38.9889999997818));
#181840=CARTESIAN_POINT('Origin',(5.49031038273072E-15,0.,38.989));
#181841=CARTESIAN_POINT('',(59.0907848292984,-12.8847271885943,38.989));
#181842=CARTESIAN_POINT('Origin',(5.49031038273072E-15,0.,38.989));
#181843=CARTESIAN_POINT('',(58.6269798078533,-12.7861423879248,38.989));
#181844=CARTESIAN_POINT('Origin',(5.49031038273072E-15,0.,38.989));
#181845=CARTESIAN_POINT('',(57.7713971777987,-18.4366189870673,39.2708017080178));
#181846=CARTESIAN_POINT('',(57.6166602453971,-18.3863402752338,38.989));
#181847=CARTESIAN_POINT('',(59.2498070619042,-12.9191181862648,39.2708017078546));
#181848=CARTESIAN_POINT('Origin',(5.52999282761009E-15,0.,39.2708017080178));
#181849=CARTESIAN_POINT('',(59.249807061628,-12.9191181862046,39.2708017080178));
#181850=CARTESIAN_POINT('Origin',(60.71525,0.,39.3978017080178));
#181851=CARTESIAN_POINT('',(59.4650964698966,-12.9642895838871,39.3978017080178));
#181852=CARTESIAN_POINT('',(57.9804289733663,-18.5051441132842,39.3978017080178));
#181853=CARTESIAN_POINT('Origin',(5.5478765747851E-15,0.,39.3978017080178));
#181854=CARTESIAN_POINT('',(58.1242364370956,-18.5518699907151,39.3978017080178));
#181855=CARTESIAN_POINT('',(55.0155724295758,-17.5418038257016,39.3978017080178));
#181856=CARTESIAN_POINT('',(59.6130003254555,-12.9957275188824,39.3978017080178));
#181857=CARTESIAN_POINT('Origin',(5.5478765747851E-15,0.,39.3978017080178));
#181858=CARTESIAN_POINT('',(59.4656149121214,-12.9643997821838,39.3978017080178));
#181859=CARTESIAN_POINT('Origin',(5.5478765747851E-15,0.,39.3978017080178));
#181860=CARTESIAN_POINT('',(59.8282880397055,-13.0409063549239,39.2708017080178));
#181861=CARTESIAN_POINT('',(58.3332704850401,-18.620387828198,39.2708017081757));
#181862=CARTESIAN_POINT('Origin',(5.52999282761008E-15,0.,39.2708017080178));
#181863=CARTESIAN_POINT('',(58.4880082803368,-18.6706636022909,38.9890000005756));
#181864=CARTESIAN_POINT('',(58.3332704847796,-18.6203878281148,39.2708017080178));
#181865=CARTESIAN_POINT('',(58.4881809372197,-18.6701227271411,38.989));
#181866=CARTESIAN_POINT('Origin',(5.49031038273072E-15,0.,38.989));
#181867=CARTESIAN_POINT('',(59.9873118763436,-13.0752898951325,38.989));
#181868=CARTESIAN_POINT('Origin',(5.49031038273072E-15,0.,38.989));
#181869=CARTESIAN_POINT('',(59.9874327886718,-13.0747351550711,38.9890000005754));
#181870=CARTESIAN_POINT('Origin',(5.49031038273072E-15,0.,38.989));
#181871=CARTESIAN_POINT('',(59.9874327889997,-13.0747351551268,38.989));
#181872=CARTESIAN_POINT('Origin',(62.2224557307631,0.,38.989));
#181873=CARTESIAN_POINT('',(58.9396512752213,-18.8168143322227,38.989));
#181874=CARTESIAN_POINT('',(56.3788528200606,-17.9847604760582,38.989));
#181875=CARTESIAN_POINT('',(60.4516424606489,-13.1739864076107,38.989));
#181876=CARTESIAN_POINT('Origin',(5.49031038273072E-15,0.,38.989));
#181877=CARTESIAN_POINT('',(59.9878258103051,-13.0753991351683,38.989));
#181878=CARTESIAN_POINT('Origin',(5.57972911860581E-15,0.,39.624));
#181879=CARTESIAN_POINT('Origin',(57.1650144220517,-18.2401946149524,39.6240070731883));
#181880=CARTESIAN_POINT('Origin',(58.6264520046768,-12.786035304505,39.6240070731883));
#181881=CARTESIAN_POINT('Origin',(5.57972911860581E-15,0.,39.624));
#181882=CARTESIAN_POINT('Origin',(58.9759248679598,-18.828565074058,39.5552135208021));
#181883=CARTESIAN_POINT('Origin',(60.4889312852489,-13.1819466778325,39.5552117598828));
#181884=CARTESIAN_POINT('Origin',(5.51210908043506E-15,0.,39.1438017080178));
#181885=CARTESIAN_POINT('Origin',(58.1393085451921,-18.5568062168846,39.171162538134));
#181886=CARTESIAN_POINT('Origin',(59.6284292050448,-12.9989693492943,39.1712173702605));
#181887=CARTESIAN_POINT('Origin',(5.51210908043507E-15,0.,39.1438017080178));
#181888=CARTESIAN_POINT('Origin',(57.9654487055673,-18.5002290260163,39.1712175859376));
#181889=CARTESIAN_POINT('Origin',(59.4495735695174,-12.9610367308101,39.1711627526733));
#181890=CARTESIAN_POINT('Origin',(60.4792282238308,0.,38.989));
#181891=CARTESIAN_POINT('',(59.6417962403143,-6.58785426247096,38.989));
#181892=CARTESIAN_POINT('',(58.7584778814676,-12.1649068885792,38.989));
#181893=CARTESIAN_POINT('Origin',(5.49031038273072E-15,0.,38.989));
#181894=CARTESIAN_POINT('',(59.2228087529788,-12.263603462079,38.989));
#181895=CARTESIAN_POINT('',(57.9308881865554,-11.9889972685551,38.989));
#181896=CARTESIAN_POINT('',(59.2229260468457,-12.2630370254942,38.9889999995772));
#181897=CARTESIAN_POINT('Origin',(5.49031038273072E-15,0.,38.989));
#181898=CARTESIAN_POINT('',(60.1138365740932,-6.63804933238219,38.9889999997818));
#181899=CARTESIAN_POINT('Origin',(5.49031038273072E-15,0.,38.989));
#181900=CARTESIAN_POINT('',(60.1139000598794,-6.63747437341778,38.989));
#181901=CARTESIAN_POINT('Origin',(5.49031038273072E-15,0.,38.989));
#181902=CARTESIAN_POINT('',(59.6423308931549,-6.58791045674891,38.989));
#181903=CARTESIAN_POINT('Origin',(5.49031038273072E-15,0.,38.989));
#181904=CARTESIAN_POINT('',(59.3820708699071,-12.2968658913803,39.2708017080178));
#181905=CARTESIAN_POINT('',(59.2229260461285,-12.2630370253457,38.989));
#181906=CARTESIAN_POINT('',(60.2756459901929,-6.65505462400498,39.2708017078546));
#181907=CARTESIAN_POINT('Origin',(5.52999282761009E-15,0.,39.2708017080178));
#181908=CARTESIAN_POINT('',(60.2756459899119,-6.65505462397395,39.2708017080178));
#181909=CARTESIAN_POINT('Origin',(60.71525,0.,39.3978017080178));
#181910=CARTESIAN_POINT('',(60.4944777170594,-6.67747469700946,39.3978017080178));
#181911=CARTESIAN_POINT('',(59.5971203935659,-12.3431658574211,39.3978017080178));
#181912=CARTESIAN_POINT('Origin',(5.5478765747851E-15,0.,39.3978017080178));
#181913=CARTESIAN_POINT('',(59.7450242491248,-12.3746037924164,39.3978017080178));
#181914=CARTESIAN_POINT('',(58.1567073854021,-12.036996621021,39.3978017080178));
#181915=CARTESIAN_POINT('',(60.6448574988554,-6.69328024897455,39.3978017080178));
#181916=CARTESIAN_POINT('Origin',(5.5478765747851E-15,0.,39.3978017080178));
#181917=CARTESIAN_POINT('',(60.495004838062,-6.67753009965933,39.3978017080178));
#181918=CARTESIAN_POINT('Origin',(5.5478765747851E-15,0.,39.3978017080178));
#181919=CARTESIAN_POINT('',(60.8636883187845,-6.7157078966941,39.2708017080178));
#181920=CARTESIAN_POINT('',(59.9600752509415,-12.4208962742141,39.2708017081757));
#181921=CARTESIAN_POINT('Origin',(5.52999282761008E-15,0.,39.2708017080178));
#181922=CARTESIAN_POINT('',(60.1192206258106,-12.4547221284044,38.9890000005756));
#181923=CARTESIAN_POINT('',(59.9600752506737,-12.4208962741587,39.2708017080178));
#181924=CARTESIAN_POINT('',(60.1193358000128,-12.4541661686666,38.989));
#181925=CARTESIAN_POINT('Origin',(5.49031038273072E-15,0.,38.989));
#181926=CARTESIAN_POINT('',(61.0254350648262,-6.73328056300519,38.989));
#181927=CARTESIAN_POINT('Origin',(5.49031038273072E-15,0.,38.989));
#181928=CARTESIAN_POINT('',(61.025497328658,-6.73271622308798,38.9890000005754));
#181929=CARTESIAN_POINT('Origin',(5.49031038273072E-15,0.,38.989));
#181930=CARTESIAN_POINT('',(61.0254973289899,-6.73271622310909,38.989));
#181931=CARTESIAN_POINT('Origin',(62.2224557307631,0.,38.989));
#181932=CARTESIAN_POINT('',(60.5836663843182,-12.5528626811448,38.989));
#181933=CARTESIAN_POINT('',(59.5987607253194,-12.3435145206986,38.989));
#181934=CARTESIAN_POINT('',(61.4975385923862,-6.78290064323561,38.989));
#181935=CARTESIAN_POINT('Origin',(5.49031038273072E-15,0.,38.989));
#181936=CARTESIAN_POINT('',(61.0259576020968,-6.73333548388541,38.989));
#181937=CARTESIAN_POINT('Origin',(5.57972911860581E-15,0.,39.624));
#181938=CARTESIAN_POINT('Origin',(58.7584780045774,-12.1649018101385,39.6240070731883));
#181939=CARTESIAN_POINT('Origin',(59.6417947880741,-6.58785913039828,39.6240070731883));
#181940=CARTESIAN_POINT('Origin',(5.57972911860581E-15,0.,39.624));
#181941=CARTESIAN_POINT('Origin',(60.6209695535084,-12.5607574282778,39.5552135208006));
#181942=CARTESIAN_POINT('Origin',(61.5354552197178,-6.78691956273256,39.5552117598807));
#181943=CARTESIAN_POINT('Origin',(5.51210908043506E-15,0.,39.1438017080178));
#181944=CARTESIAN_POINT('Origin',(59.760529766771,-12.3779375131248,39.1711625381325));
#181945=CARTESIAN_POINT('Origin',(60.6605407209802,-6.69489156322693,39.1712173702618));
#181946=CARTESIAN_POINT('Origin',(5.51210908043507E-15,0.,39.1438017080178));
#181947=CARTESIAN_POINT('Origin',(59.5817084227223,-12.3398435598876,39.1712175859377));
#181948=CARTESIAN_POINT('Origin',(60.4786998370193,-6.67586224832376,39.1711627526732));
#181949=CARTESIAN_POINT('Origin',(57.8669800961561,0.,40.5765));
#181950=CARTESIAN_POINT('Origin',(60.4792282238308,0.,38.989));
#181951=CARTESIAN_POINT('',(60.0036905223731,-0.3175,38.989));
#181952=CARTESIAN_POINT('',(59.7081718144892,-5.95633285891211,38.989));
#181953=CARTESIAN_POINT('Origin',(5.49031038273072E-15,0.,38.989));
#181954=CARTESIAN_POINT('',(60.1802756340603,-6.00595296980872,38.989));
#181955=CARTESIAN_POINT('',(59.851607889689,-5.97140859790549,38.989));
#181956=CARTESIAN_POINT('',(60.1803330766335,-6.00537737567514,38.988999999577));
#181957=CARTESIAN_POINT('Origin',(5.49031038273072E-15,0.,38.989));
#181958=CARTESIAN_POINT('',(60.4783917833346,-0.318078445375993,38.9889999997818));
#181959=CARTESIAN_POINT('Origin',(5.49031038273072E-15,0.,38.989));
#181960=CARTESIAN_POINT('',(60.478394821762,-0.317500000025285,38.989));
#181961=CARTESIAN_POINT('Origin',(5.49031038273072E-15,0.,38.989));
#181962=CARTESIAN_POINT('',(60.004228120231,-0.3175,38.989));
#181963=CARTESIAN_POINT('Origin',(5.49031038273072E-15,0.,38.989));
#181964=CARTESIAN_POINT('',(60.3421421670675,-6.02238575970276,39.2708017080178));
#181965=CARTESIAN_POINT('',(60.1803330759045,-6.0053773756024,38.989));
#181966=CARTESIAN_POINT('',(60.6410923275233,-0.318076890624849,39.2708017078546));
#181967=CARTESIAN_POINT('Origin',(5.52999282761009E-15,0.,39.2708017080178));
#181968=CARTESIAN_POINT('',(60.6410923272405,-0.318076890623366,39.2708017080178));
#181969=CARTESIAN_POINT('Origin',(60.71525,0.,39.3978017080178));
#181970=CARTESIAN_POINT('',(60.8610688070707,-0.3175,39.3978017080178));
#181971=CARTESIAN_POINT('',(60.5608532912343,-6.04595329345061,39.3978017080178));
#181972=CARTESIAN_POINT('Origin',(5.5478765747851E-15,0.,39.3978017080178));
#181973=CARTESIAN_POINT('',(60.7112330730304,-6.0617588454157,39.3978017080178));
#181974=CARTESIAN_POINT('',(60.0850508448141,-5.99594444118207,39.3978017080178));
#181975=CARTESIAN_POINT('',(61.0122769227456,-0.3175,39.3978017080178));
#181976=CARTESIAN_POINT('Origin',(5.5478765747851E-15,0.,39.3978017080178));
#181977=CARTESIAN_POINT('',(60.8615988316031,-0.3175,39.3978017080178));
#181978=CARTESIAN_POINT('Origin',(5.5478765747851E-15,0.,39.3978017080178));
#181979=CARTESIAN_POINT('',(61.2322532920972,-0.316930737395914,39.2708017080178));
#181980=CARTESIAN_POINT('',(60.9299448849412,-6.08531878141038,39.2708017081757));
#181981=CARTESIAN_POINT('Origin',(5.52999282761008E-15,0.,39.2708017080178));
#181982=CARTESIAN_POINT('',(61.0917542093523,-6.10232411256087,38.9890000005756));
#181983=CARTESIAN_POINT('',(60.929944884669,-6.0853187813832,39.2708017080178));
#181984=CARTESIAN_POINT('',(61.0918106390012,-6.10175915944633,38.989));
#181985=CARTESIAN_POINT('Origin',(5.49031038273072E-15,0.,38.989));
#181986=CARTESIAN_POINT('',(61.3949508163454,-0.3175,38.989));
#181987=CARTESIAN_POINT('Origin',(5.49031038273072E-15,0.,38.989));
#181988=CARTESIAN_POINT('',(61.394953749505,-0.316932243253256,38.9890000005754));
#181989=CARTESIAN_POINT('Origin',(5.49031038273072E-15,0.,38.989));
#181990=CARTESIAN_POINT('',(61.3949537498373,-0.31693224323956,38.989));
#181991=CARTESIAN_POINT('Origin',(62.2224557307631,0.,38.989));
#181992=CARTESIAN_POINT('',(61.5639141665612,-6.15137923967676,38.989));
#181993=CARTESIAN_POINT('',(61.5757885448747,-6.15262728712865,38.989));
#181994=CARTESIAN_POINT('',(61.8696548221181,-0.3175,38.989));
#181995=CARTESIAN_POINT('Origin',(5.49031038273072E-15,0.,38.989));
#181996=CARTESIAN_POINT('',(61.3954762318973,-0.3175,38.989));
#181997=CARTESIAN_POINT('Origin',(63.2144358269191,0.,40.5765));
#181998=CARTESIAN_POINT('Origin',(65.,0.,38.6715));
#181999=CARTESIAN_POINT('Origin',(5.57972911860581E-15,0.,39.624));
#182000=CARTESIAN_POINT('Origin',(59.708171406083,-5.95632779542302,39.6240070731883));
#182001=CARTESIAN_POINT('Origin',(60.0036895869254,-0.317504993060752,39.6240070731883));
#182002=CARTESIAN_POINT('Origin',(5.57972911860581E-15,0.,39.624));
#182003=CARTESIAN_POINT('Origin',(61.6018382108738,-6.15533149560949,39.5552135207993));
#182004=CARTESIAN_POINT('Origin',(61.9077838296774,-0.317533536648587,39.55521175988));
#182005=CARTESIAN_POINT('Origin',(5.51210908043506E-15,0.,39.1438017080178));
#182006=CARTESIAN_POINT('Origin',(60.7270021185297,-6.06345353572125,39.1711625381299));
#182007=CARTESIAN_POINT('Origin',(61.0280426587402,-0.317463144196517,39.1712173702601));
#182008=CARTESIAN_POINT('Origin',(5.51210908043507E-15,0.,39.1438017080178));
#182009=CARTESIAN_POINT('Origin',(60.5451784741259,-6.04426018543854,39.1712175859343));
#182010=CARTESIAN_POINT('Origin',(60.8452088131256,-0.317545622030759,39.1711627526726));
#182011=CARTESIAN_POINT('Origin',(58.2637721346185,0.1905,40.10025));
#182012=CARTESIAN_POINT('',(59.0285534841296,-0.01524,40.10025));
#182013=CARTESIAN_POINT('',(62.8464427007196,-0.01524,40.10025));
#182014=CARTESIAN_POINT('',(58.2637721346185,-0.01524,40.10025));
#182015=CARTESIAN_POINT('',(62.8464427007196,0.01524,40.10025));
#182016=CARTESIAN_POINT('Origin',(-1.95097259456047E-16,0.,40.10025));
#182017=CARTESIAN_POINT('',(59.0285534841296,0.01524,40.10025));
#182018=CARTESIAN_POINT('',(58.9578504383728,0.01524,40.10025));
#182019=CARTESIAN_POINT('Origin',(4.7062627014205E-16,0.,40.10025));
#182020=CARTESIAN_POINT('Origin',(0.,0.1905,0.));
#182021=CARTESIAN_POINT('',(60.0036905223731,0.1905,39.116));
#182022=CARTESIAN_POINT('',(59.5728760150042,0.1905,39.3548010137695));
#182023=CARTESIAN_POINT('Origin',(59.9654595002501,0.1905,39.5550297832849));
#182024=CARTESIAN_POINT('',(59.2165773020941,0.190499999468626,39.92499));
#182025=CARTESIAN_POINT('',(59.5728760150042,0.1905,39.3548010137695));
#182026=CARTESIAN_POINT('',(62.6567671111299,0.190499999999999,39.92499));
#182027=CARTESIAN_POINT('',(62.9165533988763,0.1905,39.92499));
#182028=CARTESIAN_POINT('',(62.3004688883555,0.190500000605232,39.3548010137695));
#182029=CARTESIAN_POINT('',(62.6567671111299,0.1905,39.92499));
#182030=CARTESIAN_POINT('',(61.8696548221181,0.1905,39.116));
#182031=CARTESIAN_POINT('Origin',(61.907885967377,0.1905,39.5550293907185));
#182032=CARTESIAN_POINT('',(61.4682752798284,0.190500000711878,39.116));
#182033=CARTESIAN_POINT('',(5.50819412990574E-15,0.1905,39.116));
#182034=CARTESIAN_POINT('',(61.3422370451705,0.1905,39.3343017080178));
#182035=CARTESIAN_POINT('',(61.4682752798284,0.1905,39.116));
#182036=CARTESIAN_POINT('',(61.0122769227456,0.1905,39.5248017080178));
#182037=CARTESIAN_POINT('Origin',(61.0417043405058,0.190499486622398,39.1947747614266));
#182038=CARTESIAN_POINT('',(60.8610688070707,0.1905,39.5248017080178));
#182039=CARTESIAN_POINT('',(5.56576032196012E-15,0.1905,39.5248017080178));
#182040=CARTESIAN_POINT('',(60.5311086139135,0.1905,39.3343017080178));
#182041=CARTESIAN_POINT('Origin',(60.831638480741,0.190499486573503,39.19477289119));
#182042=CARTESIAN_POINT('',(60.4050703266283,0.1905,39.116));
#182043=CARTESIAN_POINT('',(60.5311086139135,0.1905,39.3343017080178));
#182044=CARTESIAN_POINT('',(5.50819412990574E-15,0.1905,39.116));
#182045=CARTESIAN_POINT('Origin',(0.,-0.1905,0.));
#182046=CARTESIAN_POINT('',(61.8696548221181,-0.1905,39.116));
#182047=CARTESIAN_POINT('',(62.3004688883555,-0.190500000000001,39.3548010137695));
#182048=CARTESIAN_POINT('Origin',(61.9078859670888,-0.1905,39.5550293912443));
#182049=CARTESIAN_POINT('',(62.6567671111299,-0.19050000045281,39.92499));
#182050=CARTESIAN_POINT('',(62.3004688883555,-0.1905,39.3548010137695));
#182051=CARTESIAN_POINT('',(59.2165773020941,-0.1905,39.92499));
#182052=CARTESIAN_POINT('',(0.,-0.1905,39.92499));
#182053=CARTESIAN_POINT('',(59.5728760150042,-0.190499999293268,39.3548010137695));
#182054=CARTESIAN_POINT('',(59.2165773020941,-0.1905,39.92499));
#182055=CARTESIAN_POINT('',(60.0036905223731,-0.1905,39.116));
#182056=CARTESIAN_POINT('Origin',(59.9654594999459,-0.1905,39.5550297827296));
#182057=CARTESIAN_POINT('',(60.4050703266283,-0.190499999258369,39.116));
#182058=CARTESIAN_POINT('',(60.4789282006569,-0.1905,39.116));
#182059=CARTESIAN_POINT('',(60.5311086139135,-0.1905,39.3343017080178));
#182060=CARTESIAN_POINT('',(60.4050703266283,-0.1905,39.116));
#182061=CARTESIAN_POINT('',(60.8610688070707,-0.1905,39.5248017080178));
#182062=CARTESIAN_POINT('Origin',(60.8316414495909,-0.190499486502558,39.1947745585603));
#182063=CARTESIAN_POINT('',(61.0122769227456,-0.1905,39.5248017080178));
#182064=CARTESIAN_POINT('',(61.0128056337175,-0.1905,39.5248017080178));
#182065=CARTESIAN_POINT('',(61.3422370451705,-0.1905,39.3343017080178));
#182066=CARTESIAN_POINT('Origin',(61.0417071743798,-0.190499486688097,39.1947728594227));
#182067=CARTESIAN_POINT('',(61.4682752798284,-0.1905,39.116));
#182068=CARTESIAN_POINT('',(61.3422370451705,-0.1905,39.3343017080178));
#182069=CARTESIAN_POINT('',(61.8701762063762,-0.1905,39.116));
#182070=CARTESIAN_POINT('Origin',(58.2637721346185,-0.01524,39.92499));
#182071=CARTESIAN_POINT('Ctrl Pts',(62.6567671111299,-0.1905,39.92499));
#182072=CARTESIAN_POINT('Ctrl Pts',(62.6673774406538,-0.1905,39.9348354642021));
#182073=CARTESIAN_POINT('Ctrl Pts',(62.6779562874465,-0.189662809673067,
39.9446440828463));
#182074=CARTESIAN_POINT('Ctrl Pts',(62.6884465439476,-0.1880036041151,39.9543641760338));
#182075=CARTESIAN_POINT('Ctrl Pts',(62.6985959295776,-0.186398312857848,
39.963768424072));
#182076=CARTESIAN_POINT('Ctrl Pts',(62.7086636500152,-0.184023290311169,
39.9730909636405));
#182077=CARTESIAN_POINT('Ctrl Pts',(62.718593962217,-0.180846261210442,
39.982280897715));
#182078=CARTESIAN_POINT('Ctrl Pts',(62.7279874260866,-0.177840987311337,
39.990974009466));
#182079=CARTESIAN_POINT('Ctrl Pts',(62.7372588214087,-0.174117798730811,
39.9995492765012));
#182080=CARTESIAN_POINT('Ctrl Pts',(62.7463424082318,-0.169611579426027,
40.0079462328706));
#182081=CARTESIAN_POINT('Ctrl Pts',(62.7547090486376,-0.165461025548246,
40.0156804369701));
#182082=CARTESIAN_POINT('Ctrl Pts',(62.7629168328863,-0.16064587058751,
40.0232638017434));
#182083=CARTESIAN_POINT('Ctrl Pts',(62.7708892610819,-0.155086395961918,
40.0306257269979));
#182084=CARTESIAN_POINT('Ctrl Pts',(62.7732017594462,-0.153473803704847,
40.032761141666));
#182085=CARTESIAN_POINT('Ctrl Pts',(62.7754942590279,-0.151798403770304,
40.0348777427275));
#182086=CARTESIAN_POINT('Ctrl Pts',(62.7777643638145,-0.150057792857652,
40.0369733168701));
#182087=CARTESIAN_POINT('Ctrl Pts',(62.780225303358,-0.148170858717032,
40.039245053974));
#182088=CARTESIAN_POINT('Ctrl Pts',(62.7826571567198,-0.14621076955376,
40.041487875195));
#182089=CARTESIAN_POINT('Ctrl Pts',(62.7850565204094,-0.144175421826142,
40.0436985701601));
#182090=CARTESIAN_POINT('Ctrl Pts',(62.791641592883,-0.138589394016614,
40.0497658398386));
#182091=CARTESIAN_POINT('Ctrl Pts',(62.7979456687653,-0.132410786669041,
40.0555581699984));
#182092=CARTESIAN_POINT('Ctrl Pts',(62.8038680995981,-0.125664597436735,
40.0609828468885));
#182093=CARTESIAN_POINT('Ctrl Pts',(62.8092868022738,-0.119492200548398,
40.0659461317304));
#182094=CARTESIAN_POINT('Ctrl Pts',(62.8143744518938,-0.112844347460372,
40.0706039980705));
#182095=CARTESIAN_POINT('Ctrl Pts',(62.8190433630432,-0.10570804383351,
40.0748843180602));
#182096=CARTESIAN_POINT('Ctrl Pts',(62.8213367169482,-0.102202714803632,
40.0769867972569));
#182097=CARTESIAN_POINT('Ctrl Pts',(62.8235285419787,-0.0985794274533726,
40.0789976708174));
#182098=CARTESIAN_POINT('Ctrl Pts',(62.8256051102647,-0.0948363533472265,
40.08090504915));
#182099=CARTESIAN_POINT('Ctrl Pts',(62.825999118871,-0.0941261414936272,
40.0812669556105));
#182100=CARTESIAN_POINT('Ctrl Pts',(62.8263888407139,-0.0934111032312788,
40.0816253922032));
#182101=CARTESIAN_POINT('Ctrl Pts',(62.826774159152,-0.0926913160160826,
40.0819801989139));
#182102=CARTESIAN_POINT('Ctrl Pts',(62.8271474363889,-0.0919940221513613,
40.0823239179149));
#182103=CARTESIAN_POINT('Ctrl Pts',(62.8275165811343,-0.0912922715310412,
40.0826642303498));
#182104=CARTESIAN_POINT('Ctrl Pts',(62.8278814873655,-0.0905861384169516,
40.0830009916099));
#182105=CARTESIAN_POINT('Ctrl Pts',(62.8318581602824,-0.0828908452418622,
40.0866709464312));
#182106=CARTESIAN_POINT('Ctrl Pts',(62.8353337180912,-0.0746698316630608,
40.0899175831877));
#182107=CARTESIAN_POINT('Ctrl Pts',(62.8381654210186,-0.0660491922297058,
40.0925642067062));
#182108=CARTESIAN_POINT('Ctrl Pts',(62.8393612667489,-0.0624086426654192,
40.0936818922527));
#182109=CARTESIAN_POINT('Ctrl Pts',(62.8404425512865,-0.0586971697057385,
40.094693009479));
#182110=CARTESIAN_POINT('Ctrl Pts',(62.8414000604479,-0.0549254519864779,
40.0955863397546));
#182111=CARTESIAN_POINT('Ctrl Pts',(62.8430124819501,-0.0485739735922166,
40.0970906856166));
#182112=CARTESIAN_POINT('Ctrl Pts',(62.8442717146911,-0.0420529246952733,
40.0982599215483));
#182113=CARTESIAN_POINT('Ctrl Pts',(62.8451307298764,-0.0354197192407095,
40.0990497370453));
#182114=CARTESIAN_POINT('Ctrl Pts',(62.8453454836727,-0.0337614178770686,
40.0992471909196));
#182115=CARTESIAN_POINT('Ctrl Pts',(62.8455349903695,-0.0320960919385888,
40.0994209989363));
#182116=CARTESIAN_POINT('Ctrl Pts',(62.8456982067485,-0.0304246312365872,
40.0995705982975));
#182117=CARTESIAN_POINT('Ctrl Pts',(62.845943031317,-0.0279174401835849,
40.0997949973393));
#182118=CARTESIAN_POINT('Ctrl Pts',(62.8461286892223,-0.0253964615339684,
40.0999649129781));
#182119=CARTESIAN_POINT('Ctrl Pts',(62.846253337618,-0.0228647168031114,
40.1000786629733));
#182120=CARTESIAN_POINT('Ctrl Pts',(62.8463779860137,-0.0203329720722545,
40.1001924129685));
#182121=CARTESIAN_POINT('Ctrl Pts',(62.8464416340693,-0.0177904683741538,
40.10025));
#182122=CARTESIAN_POINT('Ctrl Pts',(62.8464427007196,-0.01524,40.10025));
#182123=CARTESIAN_POINT('Ctrl Pts',(59.0285534841296,-0.0152400000000003,
40.10025));
#182124=CARTESIAN_POINT('Ctrl Pts',(59.0285496414744,-0.0238699985092282,
40.10025));
#182125=CARTESIAN_POINT('Ctrl Pts',(59.0292582026622,-0.0324255116353481,
40.0995786334241));
#182126=CARTESIAN_POINT('Ctrl Pts',(59.0305954788489,-0.0407807192225228,
40.0983063763366));
#182127=CARTESIAN_POINT('Ctrl Pts',(59.0314592220531,-0.0461773260301675,
40.0974846287993));
#182128=CARTESIAN_POINT('Ctrl Pts',(59.0325843328198,-0.051490526840898,
40.0964130309338));
#182129=CARTESIAN_POINT('Ctrl Pts',(59.0339399880044,-0.0566895722962414,
40.0951176960923));
#182130=CARTESIAN_POINT('Ctrl Pts',(59.0357368312949,-0.0635806092274516,
40.0934008039614));
#182131=CARTESIAN_POINT('Ctrl Pts',(59.0379438906768,-0.0702685278901257,
40.0912909372156));
#182132=CARTESIAN_POINT('Ctrl Pts',(59.0405007795597,-0.0766865040604523,
40.0888630467851));
#182133=CARTESIAN_POINT('Ctrl Pts',(59.0417792240012,-0.0798954921456156,
40.0876491015699));
#182134=CARTESIAN_POINT('Ctrl Pts',(59.0431451240706,-0.0830371938949207,
40.0863558569271));
#182135=CARTESIAN_POINT('Ctrl Pts',(59.0445909239228,-0.0861046703637865,
40.0849936342771));
#182136=CARTESIAN_POINT('Ctrl Pts',(59.0453138238489,-0.0876384085982195,
40.0843125229521));
#182137=CARTESIAN_POINT('Ctrl Pts',(59.0460566986719,-0.0891536069436217,
40.0836141747074));
#182138=CARTESIAN_POINT('Ctrl Pts',(59.0468186034776,-0.0906495011920565,
40.0828999161609));
#182139=CARTESIAN_POINT('Ctrl Pts',(59.047009079679,-0.0910234747541652,
40.0827213515243));
#182140=CARTESIAN_POINT('Ctrl Pts',(59.0472007452523,-0.0913962421596992,
40.0825417925842));
#182141=CARTESIAN_POINT('Ctrl Pts',(59.0473935854286,-0.0917677921727011,
40.082361260236));
#182142=CARTESIAN_POINT('Ctrl Pts',(59.0479721059574,-0.0928824422117066,
40.0818196631917));
#182143=CARTESIAN_POINT('Ctrl Pts',(59.0485611979309,-0.0939861339737851,
40.0812693052021));
#182144=CARTESIAN_POINT('Ctrl Pts',(59.0491604624443,-0.0950785796749054,
40.0807107531874));
#182145=CARTESIAN_POINT('Ctrl Pts',(59.0533816042977,-0.102773626133362,
40.0767763849181));
#182146=CARTESIAN_POINT('Ctrl Pts',(59.0580834293368,-0.109958823466688,
40.0724140586135));
#182147=CARTESIAN_POINT('Ctrl Pts',(59.0631465696374,-0.116642428647161,
40.0677221223765));
#182148=CARTESIAN_POINT('Ctrl Pts',(59.0656021872118,-0.119883969937114,
40.0654465383718));
#182149=CARTESIAN_POINT('Ctrl Pts',(59.068143371512,-0.123007567718246,
40.0630928000678));
#182150=CARTESIAN_POINT('Ctrl Pts',(59.0707593633743,-0.126014035556417,
40.0606689262479));
#182151=CARTESIAN_POINT('Ctrl Pts',(59.0747642641416,-0.130616727761041,
40.0569581447805));
#182152=CARTESIAN_POINT('Ctrl Pts',(59.0789414743143,-0.134943070277262,
40.0530843804605));
#182153=CARTESIAN_POINT('Ctrl Pts',(59.0832455674828,-0.138985142830725,
40.0490800251457));
#182154=CARTESIAN_POINT('Ctrl Pts',(59.0852444106167,-0.140862302235466,
40.0472203818218));
#182155=CARTESIAN_POINT('Ctrl Pts',(59.0872703932642,-0.142678271527114,
40.0453323608818));
#182156=CARTESIAN_POINT('Ctrl Pts',(59.0893195943183,-0.144431197308738,
40.0434201572162));
#182157=CARTESIAN_POINT('Ctrl Pts',(59.0894766575049,-0.144565552163021,
40.0432735943397));
#182158=CARTESIAN_POINT('Ctrl Pts',(59.0896338466134,-0.144699568925786,
40.0431268995707));
#182159=CARTESIAN_POINT('Ctrl Pts',(59.0897911602042,-0.144833247843074,
40.0429800745037));
#182160=CARTESIAN_POINT('Ctrl Pts',(59.0920009418701,-0.146711033602081,
40.0409176249753));
#182161=CARTESIAN_POINT('Ctrl Pts',(59.0942367399983,-0.148520654544882,
40.0388310783332));
#182162=CARTESIAN_POINT('Ctrl Pts',(59.0964928714566,-0.150262619641264,
40.036725739981));
#182163=CARTESIAN_POINT('Ctrl Pts',(59.1045829576263,-0.156508996678761,
40.0291763710718));
#182164=CARTESIAN_POINT('Ctrl Pts',(59.1129958342949,-0.161935290145609,
40.0213310894596));
#182165=CARTESIAN_POINT('Ctrl Pts',(59.1216309196484,-0.166622470787464,
40.0132837551322));
#182166=CARTESIAN_POINT('Ctrl Pts',(59.1311200109807,-0.171773211443903,
40.0044405431327));
#182167=CARTESIAN_POINT('Ctrl Pts',(59.1408779306737,-0.176031864362409,
39.9953528710602));
#182168=CARTESIAN_POINT('Ctrl Pts',(59.15080876581,-0.179468536017301,39.9861103629556));
#182169=CARTESIAN_POINT('Ctrl Pts',(59.1615315754581,-0.183179278917837,
39.9761307737552));
#182170=CARTESIAN_POINT('Ctrl Pts',(59.1724570142855,-0.185932239424911,
39.9659696936003));
#182171=CARTESIAN_POINT('Ctrl Pts',(59.1834936683149,-0.187766286100047,
39.9557128217493));
#182172=CARTESIAN_POINT('Ctrl Pts',(59.1944377361562,-0.189584947007891,
39.9455419945152));
#182173=CARTESIAN_POINT('Ctrl Pts',(59.205492595812,-0.1905,39.9352756289336));
#182174=CARTESIAN_POINT('Ctrl Pts',(59.2165773020941,-0.1905,39.92499));
#182175=CARTESIAN_POINT('Origin',(0.,0.01524,39.92499));
#182176=CARTESIAN_POINT('Ctrl Pts',(62.8464427007196,0.01524,40.10025));
#182177=CARTESIAN_POINT('Ctrl Pts',(62.8464391086779,0.0238289333903777,
40.10025));
#182178=CARTESIAN_POINT('Ctrl Pts',(62.8457180711405,0.0323412407623314,
40.0995859581842));
#182179=CARTESIAN_POINT('Ctrl Pts',(62.8443658068291,0.0406531130499672,
40.0983275959622));
#182180=CARTESIAN_POINT('Ctrl Pts',(62.843501774309,0.0459640037532213,
40.0975235624069));
#182181=CARTESIAN_POINT('Ctrl Pts',(62.8423809556999,0.0511932363888995,
40.0964777059491));
#182182=CARTESIAN_POINT('Ctrl Pts',(62.841033859251,0.0563116129573394,
40.0952149915961));
#182183=CARTESIAN_POINT('Ctrl Pts',(62.8391953428955,0.0632971699621427,
40.0934916398701));
#182184=CARTESIAN_POINT('Ctrl Pts',(62.8369299537504,0.0700734120983113,
40.0913643921631));
#182185=CARTESIAN_POINT('Ctrl Pts',(62.8343031482014,0.0765705776094334,
40.0889118607713));
#182186=CARTESIAN_POINT('Ctrl Pts',(62.8329897454269,0.0798191603649944,
40.0876855950754));
#182187=CARTESIAN_POINT('Ctrl Pts',(62.8315859904681,0.0829981827952882,
40.0863782327527));
#182188=CARTESIAN_POINT('Ctrl Pts',(62.8301000734874,0.0861004173278454,
40.0850006373334));
#182189=CARTESIAN_POINT('Ctrl Pts',(62.8293571149971,0.0876515345941241,
40.0843118396238));
#182190=CARTESIAN_POINT('Ctrl Pts',(62.8285936160519,0.0891834722996921,
40.0836054919165));
#182191=CARTESIAN_POINT('Ctrl Pts',(62.82781060087,0.090695436427861,40.0828829920418));
#182192=CARTESIAN_POINT('Ctrl Pts',(62.8276148470746,0.0910734274599033,
40.0827023670731));
#182193=CARTESIAN_POINT('Ctrl Pts',(62.8274178735164,0.0914501705143267,
40.0825207326933));
#182194=CARTESIAN_POINT('Ctrl Pts',(62.8272196962038,0.0918256539328356,
40.0823381109275));
#182195=CARTESIAN_POINT('Ctrl Pts',(62.8266251642659,0.0929521041883625,
40.0817902456303));
#182196=CARTESIAN_POINT('Ctrl Pts',(62.826019798519,0.0940672158686514,
40.0812334935553));
#182197=CARTESIAN_POINT('Ctrl Pts',(62.8254040313373,0.0951706907488451,
40.0806684524227));
#182198=CARTESIAN_POINT('Ctrl Pts',(62.8211486980557,0.102796386827344,
40.0767636676138));
#182199=CARTESIAN_POINT('Ctrl Pts',(62.8164204928787,0.109916699411088,
40.0724404510891));
#182200=CARTESIAN_POINT('Ctrl Pts',(62.81133770774,0.116542502759262,40.0677949937414));
#182201=CARTESIAN_POINT('Ctrl Pts',(62.8088115774778,0.119835508836132,
40.0654862141909));
#182202=CARTESIAN_POINT('Ctrl Pts',(62.8061972539434,0.123006400629168,
40.0630972003218));
#182203=CARTESIAN_POINT('Ctrl Pts',(62.8035061084565,0.126056303769965,
40.0606363359906));
#182204=CARTESIAN_POINT('Ctrl Pts',(62.7975690395531,0.132784845643283,
40.0552073017123));
#182205=CARTESIAN_POINT('Ctrl Pts',(62.7912680187377,0.138932019324687,
40.0494204304519));
#182206=CARTESIAN_POINT('Ctrl Pts',(62.7847385034067,0.14444511341317,40.0434049749851));
#182207=CARTESIAN_POINT('Ctrl Pts',(62.7823531891148,0.146459116207466,
40.0412074532442));
#182208=CARTESIAN_POINT('Ctrl Pts',(62.7799396422115,0.148396130390979,
40.0389814735788));
#182209=CARTESIAN_POINT('Ctrl Pts',(62.7775029828616,0.150257579786486,
40.0367321210016));
#182210=CARTESIAN_POINT('Ctrl Pts',(62.769318501945,0.156509991333365,40.0291767837143));
#182211=CARTESIAN_POINT('Ctrl Pts',(62.7608162581029,0.161942805717658,
40.0213235332581));
#182212=CARTESIAN_POINT('Ctrl Pts',(62.7520965944507,0.166635979460955,
40.0132649215866));
#182213=CARTESIAN_POINT('Ctrl Pts',(62.7425126511848,0.171794333347845,
40.0044075527543));
#182214=CARTESIAN_POINT('Ctrl Pts',(62.7326655363519,0.176059615357,39.9953016253733));
#182215=CARTESIAN_POINT('Ctrl Pts',(62.7226511116323,0.179500292056221,
39.9860353422374));
#182216=CARTESIAN_POINT('Ctrl Pts',(62.7118651471253,0.183206048282561,
39.9760551582714));
#182217=CARTESIAN_POINT('Ctrl Pts',(62.7008840239684,0.185955767118701,
39.9658879738179));
#182218=CARTESIAN_POINT('Ctrl Pts',(62.6897991274298,0.187785458034746,
39.9556174643281));
#182219=CARTESIAN_POINT('Ctrl Pts',(62.6788639144199,0.189590441945929,
39.9454856413922));
#182220=CARTESIAN_POINT('Ctrl Pts',(62.6678262782743,0.1905,39.9352519465122));
#182221=CARTESIAN_POINT('Ctrl Pts',(62.6567671111299,0.1905,39.92499));
#182222=CARTESIAN_POINT('Ctrl Pts',(59.2165773020941,0.1905,39.92499));
#182223=CARTESIAN_POINT('Ctrl Pts',(59.2059936184293,0.1905,39.9348107241722));
#182224=CARTESIAN_POINT('Ctrl Pts',(59.1954479901463,0.18966522548866,39.9446038383169));
#182225=CARTESIAN_POINT('Ctrl Pts',(59.1849969778462,0.188008762314096,
39.9543158069384));
#182226=CARTESIAN_POINT('Ctrl Pts',(59.17490560595,0.186409301377007,39.9636935671391));
#182227=CARTESIAN_POINT('Ctrl Pts',(59.1649012152151,0.184043455438166,
39.9729968320987));
#182228=CARTESIAN_POINT('Ctrl Pts',(59.1550396955537,0.18087742372664,39.9821731151334));
#182229=CARTESIAN_POINT('Ctrl Pts',(59.1457174710368,0.177884532219491,
39.9908475764351));
#182230=CARTESIAN_POINT('Ctrl Pts',(59.1365220583453,0.174176304386962,
39.9994093733845));
#182231=CARTESIAN_POINT('Ctrl Pts',(59.1275197082956,0.169686797572386,
40.0077966115841));
#182232=CARTESIAN_POINT('Ctrl Pts',(59.1192286949255,0.165552037113266,
40.0155211172595));
#182233=CARTESIAN_POINT('Ctrl Pts',(59.1111009786088,0.160754293903562,
40.0230979941021));
#182234=CARTESIAN_POINT('Ctrl Pts',(59.1032135992724,0.155213515013196,
40.0304554104748));
#182235=CARTESIAN_POINT('Ctrl Pts',(59.1008617419714,0.153561366595946,
40.0326492435181));
#182236=CARTESIAN_POINT('Ctrl Pts',(59.098531460358,0.151842962927709,40.0348233715061));
#182237=CARTESIAN_POINT('Ctrl Pts',(59.096225375957,0.150055686180142,40.0369753512356));
#182238=CARTESIAN_POINT('Ctrl Pts',(59.093942854056,0.148286670996707,40.0391053430352));
#182239=CARTESIAN_POINT('Ctrl Pts',(59.0916862380348,0.146452235168901,
40.041211089324));
#182240=CARTESIAN_POINT('Ctrl Pts',(59.0894604907299,0.144552116609965,
40.0432881154904));
#182241=CARTESIAN_POINT('Ctrl Pts',(59.0893057166152,0.144419986081416,
40.043432547828));
#182242=CARTESIAN_POINT('Ctrl Pts',(59.0891510807051,0.144287542502095,
40.0435768364421));
#182243=CARTESIAN_POINT('Ctrl Pts',(59.0889965840074,0.144154785043939,
40.0437209807855));
#182244=CARTESIAN_POINT('Ctrl Pts',(59.0822228828154,0.138334211749542,
40.050040796842));
#182245=CARTESIAN_POINT('Ctrl Pts',(59.0757535782846,0.131883990154185,
40.0560490279344));
#182246=CARTESIAN_POINT('Ctrl Pts',(59.0697047694308,0.124808417215433,
40.0616647108614));
#182247=CARTESIAN_POINT('Ctrl Pts',(59.0640662283033,0.118212753510261,
40.0668995033484));
#182248=CARTESIAN_POINT('Ctrl Pts',(59.0587927761314,0.111072931137642,
40.071793326748));
#182249=CARTESIAN_POINT('Ctrl Pts',(59.05400766547,0.103389544768602,40.076246030307));
#182250=CARTESIAN_POINT('Ctrl Pts',(59.0522572100838,0.100578862632908,
40.0778748868746));
#182251=CARTESIAN_POINT('Ctrl Pts',(59.0505724231958,0.0976954648439348,
40.0794443522247));
#182252=CARTESIAN_POINT('Ctrl Pts',(59.048960544286,0.094739558525343,40.0809482021492));
#182253=CARTESIAN_POINT('Ctrl Pts',(59.0485729412563,0.0940287618038469,
40.0813098278168));
#182254=CARTESIAN_POINT('Ctrl Pts',(59.0481896206934,0.0933131922167491,
40.0816679525672));
#182255=CARTESIAN_POINT('Ctrl Pts',(59.0478106940136,0.092592927197163,
40.082022419258));
#182256=CARTESIAN_POINT('Ctrl Pts',(59.0474436087926,0.0918951704594389,
40.0823658088648));
#182257=CARTESIAN_POINT('Ctrl Pts',(59.0470806471271,0.0911930071934228,
40.0827057654616));
#182258=CARTESIAN_POINT('Ctrl Pts',(59.0467219102889,0.0904865115878245,
40.0830421470151));
#182259=CARTESIAN_POINT('Ctrl Pts',(59.0427915336441,0.0827460357498801,
40.0867275956806));
#182260=CARTESIAN_POINT('Ctrl Pts',(59.039366072413,0.0744802459943286,
40.0899823432031));
#182261=CARTESIAN_POINT('Ctrl Pts',(59.036584160269,0.0658168714608708,
40.0926299529356));
#182262=CARTESIAN_POINT('Ctrl Pts',(59.0354304183829,0.0622239118143531,
40.0937279956084));
#182263=CARTESIAN_POINT('Ctrl Pts',(59.0343871039217,0.0585629032864951,
40.0947220371802));
#182264=CARTESIAN_POINT('Ctrl Pts',(59.0334626554262,0.0548440714999742,
40.0956014538692));
#182265=CARTESIAN_POINT('Ctrl Pts',(59.0318859121828,0.048501216358407,
40.097101390674));
#182266=CARTESIAN_POINT('Ctrl Pts',(59.0306571138137,0.0419914004944189,
40.0982667904316));
#182267=CARTESIAN_POINT('Ctrl Pts',(59.0298212958157,0.0353717968088257,
40.0990539325582));
#182268=CARTESIAN_POINT('Ctrl Pts',(59.0294033868167,0.032061994966029,
40.0994475036216));
#182269=CARTESIAN_POINT('Ctrl Pts',(59.0290851681639,0.0287246785546796,
40.0997467259952));
#182270=CARTESIAN_POINT('Ctrl Pts',(59.0288723192866,0.0253670368748701,
40.0999473488896));
#182271=CARTESIAN_POINT('Ctrl Pts',(59.0286594704093,0.0220093951950606,
40.100147971784));
#182272=CARTESIAN_POINT('Ctrl Pts',(59.0285519740191,0.0186314705080073,
40.10025));
#182273=CARTESIAN_POINT('Ctrl Pts',(59.0285534841296,0.01524,40.10025));
#182274=CARTESIAN_POINT('Origin',(61.4240753804089,-0.317499999706107,39.1925554495083));
#182275=CARTESIAN_POINT('Origin',(61.4683012396072,-0.317551690012947,39.116037328526));
#182276=CARTESIAN_POINT('Origin',(61.3422370451705,-0.3175,39.3343017080178));
#182277=CARTESIAN_POINT('Ctrl Pts',(61.2322532920972,-0.316930737395914,
39.2708017080178));
#182278=CARTESIAN_POINT('Ctrl Pts',(61.2327440814646,-0.190499999999994,
39.2710850691866));
#182279=CARTESIAN_POINT('Ctrl Pts',(61.3422370451705,-0.1905,39.3343017080178));
#182280=CARTESIAN_POINT('Ctrl Pts',(61.1872475084174,-0.317046579199636,
39.3487519293518));
#182281=CARTESIAN_POINT('Ctrl Pts',(61.1875064541762,-0.190500000001215,
39.3492068662928));
#182282=CARTESIAN_POINT('Ctrl Pts',(61.2747290395312,-0.1905,39.451227124874));
#182283=CARTESIAN_POINT('Ctrl Pts',(61.1019842137032,-0.31726659691349,
39.3978017080178));
#182284=CARTESIAN_POINT('Ctrl Pts',(61.1018997758106,-0.190499999999995,
39.3980347781183));
#182285=CARTESIAN_POINT('Ctrl Pts',(61.146836207171,-0.1905,39.5248015355195));
#182286=CARTESIAN_POINT('Ctrl Pts',(61.0122769227456,-0.3175,39.3978017080178));
#182287=CARTESIAN_POINT('Ctrl Pts',(61.0122769227456,-0.1905,39.3978017080178));
#182288=CARTESIAN_POINT('Ctrl Pts',(61.0122769227456,-0.1905,39.5248017080178));
#182289=CARTESIAN_POINT('Origin',(61.0122769227456,-0.3175,39.5248017080178));
#182290=CARTESIAN_POINT('Origin',(5.50819412990574E-15,-0.3175,39.116));
#182291=CARTESIAN_POINT('Origin',(61.8696548221181,-0.3175,39.116));
#182292=CARTESIAN_POINT('Origin',(5.56576032196012E-15,-0.3175,39.5248017080178));
#182293=CARTESIAN_POINT('Origin',(60.8610688070707,-0.3175,39.5248017080178));
#182294=CARTESIAN_POINT('Ctrl Pts',(62.4081695979768,-0.318048871877129,
39.2875012672119));
#182295=CARTESIAN_POINT('Ctrl Pts',(62.4086377819835,-0.190309034175017,
39.287208709576));
#182296=CARTESIAN_POINT('Ctrl Pts',(62.3003077603769,-0.190500142125054,
39.3549016990126));
#182297=CARTESIAN_POINT('Ctrl Pts',(62.2931881445371,-0.31793248988995,
39.103493917393));
#182298=CARTESIAN_POINT('Ctrl Pts',(62.2934975005738,-0.190309294367355,
39.1031692336349));
#182299=CARTESIAN_POINT('Ctrl Pts',(62.208356400327,-0.190500141995468,
39.2077507202312));
#182300=CARTESIAN_POINT('Ctrl Pts',(62.0866281564672,-0.317722686167412,
38.989));
#182301=CARTESIAN_POINT('Ctrl Pts',(62.0868143053088,-0.190309769569384,
38.9887769311152));
#182302=CARTESIAN_POINT('Ctrl Pts',(62.0431695205371,-0.190500141761867,
39.1161898712897));
#182303=CARTESIAN_POINT('Ctrl Pts',(61.8696548221181,-0.3175,38.989));
#182304=CARTESIAN_POINT('Ctrl Pts',(61.8696548221181,-0.190310267888658,
38.989));
#182305=CARTESIAN_POINT('Ctrl Pts',(61.8696548221181,-0.190500141513915,
39.116189590386));
#182306=CARTESIAN_POINT('Origin',(62.3004688883555,-0.3175,39.3548010137695));
#182307=CARTESIAN_POINT('Ctrl Pts',(60.8610688070707,-0.3175,39.3978017080178));
#182308=CARTESIAN_POINT('Ctrl Pts',(60.8610688070707,-0.1905,39.3978017080178));
#182309=CARTESIAN_POINT('Ctrl Pts',(60.8610688070707,-0.1905,39.5248017080178));
#182310=CARTESIAN_POINT('Ctrl Pts',(60.7710583184321,-0.317734773760269,
39.3978017080178));
#182311=CARTESIAN_POINT('Ctrl Pts',(60.7709717342408,-0.190499999999991,
39.3975666025021));
#182312=CARTESIAN_POINT('Ctrl Pts',(60.7260547307352,-0.1905,39.5248015517177));
#182313=CARTESIAN_POINT('Ctrl Pts',(60.6859465754578,-0.31795861791903,
39.3484894016716));
#182314=CARTESIAN_POINT('Ctrl Pts',(60.6862105562579,-0.190500000001618,
39.3480259000038));
#182315=CARTESIAN_POINT('Ctrl Pts',(60.5983892955417,-0.1905,39.4508333188945));
#182316=CARTESIAN_POINT('Ctrl Pts',(60.6410923272405,-0.318076890623366,
39.2708017080178));
#182317=CARTESIAN_POINT('Ctrl Pts',(60.6415942020421,-0.1905,39.27051194648));
#182318=CARTESIAN_POINT('Ctrl Pts',(60.5311086139135,-0.1905,39.3343017080178));
#182319=CARTESIAN_POINT('Origin',(60.5311086139135,-0.3175,39.3343017080178));
#182320=CARTESIAN_POINT('Origin',(62.4786179998489,-0.31749999997796,39.6398955068184));
#182321=CARTESIAN_POINT('Origin',(62.6567671111299,-0.3175,39.92499));
#182322=CARTESIAN_POINT('Origin',(60.4497583458782,-0.317499999994971,39.1934008539952));
#182323=CARTESIAN_POINT('Origin',(60.4050521322801,-0.317550804320654,39.1160402713849));
#182324=CARTESIAN_POINT('Ctrl Pts',(62.9541448057648,-0.0152661173108668,
40.1599502534424));
#182325=CARTESIAN_POINT('Ctrl Pts',(62.9168399481843,-0.0152570710386341,
40.10025));
#182326=CARTESIAN_POINT('Ctrl Pts',(62.8464427007196,-0.01524,40.10025));
#182327=CARTESIAN_POINT('Ctrl Pts',(62.9541233134297,-0.103381504925241,
40.1599500538463));
#182328=CARTESIAN_POINT('Ctrl Pts',(62.9168211560341,-0.0794415635236045,
40.100244835349));
#182329=CARTESIAN_POINT('Ctrl Pts',(62.8464212442881,-0.0662446030559618,
40.10025));
#182330=CARTESIAN_POINT('Ctrl Pts',(62.9290872705826,-0.184683583687744,
40.1202442001037));
#182331=CARTESIAN_POINT('Ctrl Pts',(62.8936771137448,-0.138547994784254,
40.0633873868017));
#182332=CARTESIAN_POINT('Ctrl Pts',(62.8213855864655,-0.113305567451532,
40.0772271723538));
#182333=CARTESIAN_POINT('Ctrl Pts',(62.8564203507742,-0.291340992631754,
40.0045995998164));
#182334=CARTESIAN_POINT('Ctrl Pts',(62.8329175802742,-0.201910351191398,
39.9663485808314));
#182335=CARTESIAN_POINT('Ctrl Pts',(62.7487193609389,-0.175042741957872,
40.0101727202466));
#182336=CARTESIAN_POINT('Ctrl Pts',(62.8099434033761,-0.318045276842621,
39.9304654349858));
#182337=CARTESIAN_POINT('Ctrl Pts',(62.7947175425014,-0.205831635642736,
39.905190016294));
#182338=CARTESIAN_POINT('Ctrl Pts',(62.7022409210439,-0.190500000000001,
39.9671857458183));
#182339=CARTESIAN_POINT('Ctrl Pts',(62.7644678366119,-0.318045750793045,
39.8576902534424));
#182340=CARTESIAN_POINT('Ctrl Pts',(62.7649326510148,-0.1905,39.8573998014387));
#182341=CARTESIAN_POINT('Ctrl Pts',(62.6567671111299,-0.1905,39.92499));
#182342=CARTESIAN_POINT('Origin',(62.8464427007196,-0.01524,40.22725));
#182343=CARTESIAN_POINT('Origin',(5.50819412990574E-15,-0.3175,39.116));
#182344=CARTESIAN_POINT('Origin',(60.0036905223731,-0.3175,39.116));
#182345=CARTESIAN_POINT('Origin',(-1.95097259456047E-16,0.,40.22725));
#182346=CARTESIAN_POINT('Origin',(62.8464427007196,0.01524,40.22725));
#182347=CARTESIAN_POINT('Ctrl Pts',(60.0036905223731,-0.3175,38.989));
#182348=CARTESIAN_POINT('Ctrl Pts',(60.0036905223731,-0.19030974826532,
38.989));
#182349=CARTESIAN_POINT('Ctrl Pts',(60.003690522373,-0.190500142289529,
39.116190109232));
#182350=CARTESIAN_POINT('Ctrl Pts',(59.7867137603524,-0.317270385524412,
38.989));
#182351=CARTESIAN_POINT('Ctrl Pts',(59.7869045527967,-0.190310262476384,
38.9892298989766));
#182352=CARTESIAN_POINT('Ctrl Pts',(59.8301727552493,-0.190500142032462,
39.1161900493206));
#182353=CARTESIAN_POINT('Ctrl Pts',(59.5801552670728,-0.317049440713614,
39.1034966344368));
#182354=CARTESIAN_POINT('Ctrl Pts',(59.5804765271874,-0.190310761082376,
39.1038314102564));
#182355=CARTESIAN_POINT('Ctrl Pts',(59.6649871046552,-0.190500141785105,
39.2077528789596));
#182356=CARTESIAN_POINT('Ctrl Pts',(59.4651754363832,-0.316925998273047,
39.2875012672119));
#182357=CARTESIAN_POINT('Ctrl Pts',(59.4656607446594,-0.190311035335061,
39.2878045257868));
#182358=CARTESIAN_POINT('Ctrl Pts',(59.5730368716576,-0.190500141646902,
39.3549015295898));
#182359=CARTESIAN_POINT('Origin',(59.5728760150042,-0.3175,39.3548010137695));
#182360=CARTESIAN_POINT('Ctrl Pts',(62.7644678366119,0.318045750793045,
39.8576902534424));
#182361=CARTESIAN_POINT('Ctrl Pts',(62.7649326510148,0.1905,39.8573998014387));
#182362=CARTESIAN_POINT('Ctrl Pts',(62.6567671111299,0.1905,39.92499));
#182363=CARTESIAN_POINT('Ctrl Pts',(62.8099640589334,0.318045262795179,
39.9304984902489));
#182364=CARTESIAN_POINT('Ctrl Pts',(62.7947344577637,0.205840330723205,
39.9052171569779));
#182365=CARTESIAN_POINT('Ctrl Pts',(62.7022616416345,0.1905,39.9672049726594));
#182366=CARTESIAN_POINT('Ctrl Pts',(62.8562601188215,0.29133411785554,40.0043437678664));
#182367=CARTESIAN_POINT('Ctrl Pts',(62.8328016940825,0.201836550627893,
39.9661628577643));
#182368=CARTESIAN_POINT('Ctrl Pts',(62.7485591297232,0.175038734052128,
40.0100243556235));
#182369=CARTESIAN_POINT('Ctrl Pts',(62.928611257107,0.18562218956026,40.1194874821985));
#182370=CARTESIAN_POINT('Ctrl Pts',(62.8932808767899,0.139140155999965,
40.062755148314));
#182371=CARTESIAN_POINT('Ctrl Pts',(62.8209095783125,0.113848895265745,
40.0767884282377));
#182372=CARTESIAN_POINT('Ctrl Pts',(62.9541233349674,0.103673266462929,
40.1599502015391));
#182373=CARTESIAN_POINT('Ctrl Pts',(62.9168211653022,0.0796882264537865,
40.1002449453869));
#182374=CARTESIAN_POINT('Ctrl Pts',(62.8464212664863,0.0664134143651042,
40.10025));
#182375=CARTESIAN_POINT('Ctrl Pts',(62.9541448057648,0.0152661173108668,
40.1599502534424));
#182376=CARTESIAN_POINT('Ctrl Pts',(62.9168399481843,0.0152570710386341,
40.10025));
#182377=CARTESIAN_POINT('Ctrl Pts',(62.8464427007196,0.01524,40.10025));
#182378=CARTESIAN_POINT('Origin',(62.6567671111299,0.3175,39.92499));
#182379=CARTESIAN_POINT('Origin',(59.3947266586252,-0.317499999970944,39.6398955069323));
#182380=CARTESIAN_POINT('Origin',(59.2165773020941,-0.3175,39.92499));
#182381=CARTESIAN_POINT('Origin',(62.478617999835,0.317499999978368,39.6398955068271));
#182382=CARTESIAN_POINT('Origin',(62.3004688883555,0.3175,39.3548010137695));
#182383=CARTESIAN_POINT('Ctrl Pts',(59.1088767419348,-0.316922544675689,
39.8576902534424));
#182384=CARTESIAN_POINT('Ctrl Pts',(59.1093642282367,-0.1905,39.8579948730703));
#182385=CARTESIAN_POINT('Ctrl Pts',(59.2165773020941,-0.1905,39.92499));
#182386=CARTESIAN_POINT('Ctrl Pts',(59.0634407053229,-0.316922012809157,
39.9304020711231));
#182387=CARTESIAN_POINT('Ctrl Pts',(59.0793536643045,-0.2056949737408,39.9058915297385));
#182388=CARTESIAN_POINT('Ctrl Pts',(59.1711393827295,-0.1905,39.9671523786035));
#182389=CARTESIAN_POINT('Ctrl Pts',(59.0174076205276,-0.290332993455009,
40.0043257306693));
#182390=CARTESIAN_POINT('Ctrl Pts',(59.0412846811395,-0.201480151665877,
39.9667894847835));
#182391=CARTESIAN_POINT('Ctrl Pts',(59.1251084688121,-0.175054909459681,
40.01001389752));
#182392=CARTESIAN_POINT('Ctrl Pts',(58.9458296250062,-0.184894967401558,
40.1195533054857));
#182393=CARTESIAN_POINT('Ctrl Pts',(58.9812445774292,-0.138672156931214,
40.0630813209236));
#182394=CARTESIAN_POINT('Ctrl Pts',(59.0535312451933,-0.113807322597802,
40.076826594242));
#182395=CARTESIAN_POINT('Ctrl Pts',(58.9208287018091,-0.103171606455737,
40.1599502027518));
#182396=CARTESIAN_POINT('Ctrl Pts',(58.9581363848263,-0.0793367652458399,
40.1002552791541));
#182397=CARTESIAN_POINT('Ctrl Pts',(59.0285307646513,-0.0663350652343413,
40.10025));
#182398=CARTESIAN_POINT('Ctrl Pts',(58.9208513795073,-0.0152121934559204,
40.1599502534424));
#182399=CARTESIAN_POINT('Ctrl Pts',(58.9581562369413,-0.0152218248291072,
40.10025));
#182400=CARTESIAN_POINT('Ctrl Pts',(59.0285534841296,-0.0152400000000003,
40.10025));
#182401=CARTESIAN_POINT('Origin',(59.0285534841296,-0.01524,40.22725));
#182402=CARTESIAN_POINT('Ctrl Pts',(61.8696548221181,0.3175,38.989));
#182403=CARTESIAN_POINT('Ctrl Pts',(61.8696548221181,0.190310256931022,
38.989));
#182404=CARTESIAN_POINT('Ctrl Pts',(61.8696548221181,0.190500141530249,
39.1161896013273));
#182405=CARTESIAN_POINT('Ctrl Pts',(62.0866315324121,0.31772268963223,38.989));
#182406=CARTESIAN_POINT('Ctrl Pts',(62.0868176889525,0.19030975857524,38.9887769275436));
#182407=CARTESIAN_POINT('Ctrl Pts',(62.0431722165642,0.190500141778233,
39.116189882183));
#182408=CARTESIAN_POINT('Ctrl Pts',(62.2931898887681,0.317932491655691,
39.1034967087243));
#182409=CARTESIAN_POINT('Ctrl Pts',(62.2934992458059,0.190309283351463,
39.1031720232722));
#182410=CARTESIAN_POINT('Ctrl Pts',(62.2083577878531,0.190500142011856,
39.2077529615015));
#182411=CARTESIAN_POINT('Ctrl Pts',(62.4081695979768,0.318048871877129,
39.2875012672119));
#182412=CARTESIAN_POINT('Ctrl Pts',(62.4086377820239,0.190309023146095,
39.2872087095507));
#182413=CARTESIAN_POINT('Ctrl Pts',(62.3003077510782,0.190500142141459,
39.3549017048231));
#182414=CARTESIAN_POINT('Origin',(61.8696548221181,0.3175,39.116));
#182415=CARTESIAN_POINT('Origin',(4.7062627014205E-16,0.,40.22725));
#182416=CARTESIAN_POINT('Origin',(59.0285534841296,0.01524,40.22725));
#182417=CARTESIAN_POINT('Origin',(62.2224557307631,0.3175,39.116));
#182418=CARTESIAN_POINT('Origin',(61.4683012396074,0.317551690013413,39.1160373285266));
#182419=CARTESIAN_POINT('Ctrl Pts',(58.9208513795073,0.0152121934559198,
40.1599502534424));
#182420=CARTESIAN_POINT('Ctrl Pts',(58.9581562369414,0.0152218248291069,
40.10025));
#182421=CARTESIAN_POINT('Ctrl Pts',(59.0285534841296,0.01524,40.10025));
#182422=CARTESIAN_POINT('Ctrl Pts',(58.9208288705618,0.102871702177323,
40.1599500566037));
#182423=CARTESIAN_POINT('Ctrl Pts',(58.9581365422943,0.0790852439333523,
40.1002551305372));
#182424=CARTESIAN_POINT('Ctrl Pts',(59.0285309330218,0.0661608181924836,
40.10025));
#182425=CARTESIAN_POINT('Ctrl Pts',(58.9453619764183,0.183955833237606,
40.1203070619046));
#182426=CARTESIAN_POINT('Ctrl Pts',(58.9808530699761,0.138075936736041,
40.0637098684499));
#182427=CARTESIAN_POINT('Ctrl Pts',(59.0530636028226,0.113261762368195,
40.0772636213362));
#182428=CARTESIAN_POINT('Ctrl Pts',(59.0172303255294,0.290319860890557,
40.0046102245801));
#182429=CARTESIAN_POINT('Ctrl Pts',(59.0411528690721,0.201541405841854,
39.9670001894012));
#182430=CARTESIAN_POINT('Ctrl Pts',(59.1249311745757,0.17504730955115,40.0101788811209));
#182431=CARTESIAN_POINT('Ctrl Pts',(59.0634600627912,0.316922027357347,
39.9303710930186));
#182432=CARTESIAN_POINT('Ctrl Pts',(59.0793694364691,0.20568700036727,39.9058663574113));
#182433=CARTESIAN_POINT('Ctrl Pts',(59.1711586818658,0.1905,39.9671344706364));
#182434=CARTESIAN_POINT('Ctrl Pts',(59.1088767419348,0.316922544675689,
39.8576902534424));
#182435=CARTESIAN_POINT('Ctrl Pts',(59.1093642282367,0.1905,39.8579948730703));
#182436=CARTESIAN_POINT('Ctrl Pts',(59.2165773020941,0.1905,39.92499));
#182437=CARTESIAN_POINT('Origin',(59.2165773020941,0.3175,39.92499));
#182438=CARTESIAN_POINT('Origin',(61.4240753793296,0.317499999995729,39.1925554488852));
#182439=CARTESIAN_POINT('Origin',(61.3422370451705,0.3175,39.3343017080178));
#182440=CARTESIAN_POINT('Origin',(59.3947266586076,0.317499999969843,39.6398955069213));
#182441=CARTESIAN_POINT('Origin',(59.5728760150042,0.3175,39.3548010137695));
#182442=CARTESIAN_POINT('Ctrl Pts',(61.0122769227456,0.3175,39.3978017080178));
#182443=CARTESIAN_POINT('Ctrl Pts',(61.0122769227456,0.1905,39.3978017080178));
#182444=CARTESIAN_POINT('Ctrl Pts',(61.0122769227456,0.1905,39.5248017080178));
#182445=CARTESIAN_POINT('Ctrl Pts',(61.1022873990971,0.317265808076389,
39.3978017080178));
#182446=CARTESIAN_POINT('Ctrl Pts',(61.1022028716714,0.190499999999991,
39.3980355775177));
#182447=CARTESIAN_POINT('Ctrl Pts',(61.1472909869841,0.1905,39.5248015517192));
#182448=CARTESIAN_POINT('Ctrl Pts',(61.1873990841185,0.317046189129096,
39.3484893995498));
#182449=CARTESIAN_POINT('Ctrl Pts',(61.1876587562312,0.190500000001213,
39.3489438303423));
#182450=CARTESIAN_POINT('Ctrl Pts',(61.2749563897832,0.1905,39.4508333155592));
#182451=CARTESIAN_POINT('Ctrl Pts',(61.2322532920972,0.316930737395914,
39.2708017080178));
#182452=CARTESIAN_POINT('Ctrl Pts',(61.2327440814646,0.190499999999994,
39.2710850691866));
#182453=CARTESIAN_POINT('Ctrl Pts',(61.3422370451705,0.1905,39.3343017080178));
#182454=CARTESIAN_POINT('Origin',(61.0122769227456,0.3175,39.5248017080178));
#182455=CARTESIAN_POINT('Ctrl Pts',(59.4651754363832,0.316925998273047,
39.2875012672119));
#182456=CARTESIAN_POINT('Ctrl Pts',(59.4656607446034,0.190311049925411,
39.2878045257518));
#182457=CARTESIAN_POINT('Ctrl Pts',(59.5730368592467,0.190500141625045,
39.3549015218345));
#182458=CARTESIAN_POINT('Ctrl Pts',(59.5801570044831,0.317049442579172,
39.1034938540228));
#182459=CARTESIAN_POINT('Ctrl Pts',(59.5804782634901,0.190310775688126,
39.1038286278819));
#182460=CARTESIAN_POINT('Ctrl Pts',(59.6649884842725,0.190500141763232,
39.2077506434032));
#182461=CARTESIAN_POINT('Ctrl Pts',(59.7867171285936,0.317270389088827,
38.989));
#182462=CARTESIAN_POINT('Ctrl Pts',(59.7869079131798,0.190310277118492,
38.9892298954611));
#182463=CARTESIAN_POINT('Ctrl Pts',(59.8301754438916,0.19050014201055,39.1161900347286));
#182464=CARTESIAN_POINT('Ctrl Pts',(60.0036905223731,0.3175,38.989));
#182465=CARTESIAN_POINT('Ctrl Pts',(60.0036905223731,0.190309762955091,
38.989));
#182466=CARTESIAN_POINT('Ctrl Pts',(60.0036905223731,0.190500142267573,
39.1161900945642));
#182467=CARTESIAN_POINT('Origin',(60.0036905223731,0.3175,39.116));
#182468=CARTESIAN_POINT('Origin',(60.71525,0.3175,39.5248017080178));
#182469=CARTESIAN_POINT('Origin',(60.8610688070707,0.3175,39.5248017080178));
#182470=CARTESIAN_POINT('Origin',(60.4792282238308,0.3175,39.116));
#182471=CARTESIAN_POINT('Origin',(60.4050521322803,0.317550804320378,39.1160402713846));
#182472=CARTESIAN_POINT('Ctrl Pts',(60.6410923272405,0.318076890623366,
39.2708017080178));
#182473=CARTESIAN_POINT('Ctrl Pts',(60.6415942020421,0.1905,39.27051194648));
#182474=CARTESIAN_POINT('Ctrl Pts',(60.5311086139135,0.1905,39.3343017080178));
#182475=CARTESIAN_POINT('Ctrl Pts',(60.6860981505083,0.317958218318763,
39.3487519301186));
#182476=CARTESIAN_POINT('Ctrl Pts',(60.6863613750282,0.190499999999993,
39.3482879463987));
#182477=CARTESIAN_POINT('Ctrl Pts',(60.5986166446955,0.1905,39.451227126164));
#182478=CARTESIAN_POINT('Ctrl Pts',(60.771361502534,0.317733982967541,39.3978017080178));
#182479=CARTESIAN_POINT('Ctrl Pts',(60.7712750141994,0.190499999999998,
39.3975673827397));
#182480=CARTESIAN_POINT('Ctrl Pts',(60.7265095085051,0.1905,39.524801535518));
#182481=CARTESIAN_POINT('Ctrl Pts',(60.8610688070707,0.3175,39.3978017080178));
#182482=CARTESIAN_POINT('Ctrl Pts',(60.8610688070707,0.1905,39.3978017080178));
#182483=CARTESIAN_POINT('Ctrl Pts',(60.8610688070707,0.1905,39.5248017080178));
#182484=CARTESIAN_POINT('Origin',(60.5311086139135,0.3175,39.3343017080178));
#182485=CARTESIAN_POINT('Origin',(60.449758346987,0.317500000300332,39.193400853355));
#182486=CARTESIAN_POINT('Origin',(57.9645097668785,-5.90076614434076,40.10025));
#182487=CARTESIAN_POINT('',(58.7035958781039,-6.18532049829399,40.10025));
#182488=CARTESIAN_POINT('',(62.5005702980931,-6.58439859103029,40.10025));
#182489=CARTESIAN_POINT('',(57.9430040808458,-6.10537907909383,40.10025));
#182490=CARTESIAN_POINT('',(62.5037563256535,-6.55408556365946,40.10025));
#182491=CARTESIAN_POINT('Origin',(5.50059263827931E-15,5.71025087946725E-15,
40.10025));
#182492=CARTESIAN_POINT('',(58.7067819056643,-6.15500747092316,40.10025));
#182493=CARTESIAN_POINT('',(58.63646617859,-6.14761699020186,40.10025));
#182494=CARTESIAN_POINT('Origin',(5.72291486498914E-15,5.24470718193599E-15,
40.10025));
#182495=CARTESIAN_POINT('Origin',(0.019912672252488,0.189456421067656,-2.80404091450791E-18));
#182496=CARTESIAN_POINT('',(59.6948966996543,-6.08263713962388,39.116));
#182497=CARTESIAN_POINT('',(59.2664422392336,-6.0376047612152,39.3548010137695));
#182498=CARTESIAN_POINT('Origin',(59.6568751110691,-6.07864090963206,39.555029783282));
#182499=CARTESIAN_POINT('',(58.9120953678975,-6.00036140481896,39.92499));
#182500=CARTESIAN_POINT('',(59.2664422392336,-6.0376047612152,39.3548010137695));
#182501=CARTESIAN_POINT('',(62.3334394572619,-6.35995915837802,39.92499));
#182502=CARTESIAN_POINT('',(62.5918026085422,-6.38711421981416,39.92499));
#182503=CARTESIAN_POINT('',(61.9790930734951,-6.32271585208485,39.3548010137695));
#182504=CARTESIAN_POINT('',(62.3334394572619,-6.35995915837802,39.92499));
#182505=CARTESIAN_POINT('',(61.5506390517262,-6.27768352038853,39.116));
#182506=CARTESIAN_POINT('Origin',(61.5886607627709,-6.28167976325137,39.5550293907194));
#182507=CARTESIAN_POINT('',(61.1514583086406,-6.23572793293807,39.116));
#182508=CARTESIAN_POINT('',(0.0199126722524935,0.189456421067656,39.116));
#182509=CARTESIAN_POINT('',(61.0261105245454,-6.22255335066416,39.3343017080178));
#182510=CARTESIAN_POINT('',(61.1514583085662,-6.23572793364592,39.116));
#182511=CARTESIAN_POINT('',(60.6979579581954,-6.18806312612747,39.5248017080178));
#182512=CARTESIAN_POINT('Origin',(60.7272241158256,-6.19113963944979,39.1947747614368));
#182513=CARTESIAN_POINT('',(60.5475781763993,-6.17225757416238,39.5248017080178));
#182514=CARTESIAN_POINT('',(0.0199126722524936,0.189456421067656,39.5248017080178));
#182515=CARTESIAN_POINT('',(60.2194255397045,-6.13776734223215,39.3343017080178));
#182516=CARTESIAN_POINT('Origin',(60.5183090188078,-6.16918177799145,39.1947728911918));
#182517=CARTESIAN_POINT('',(60.0940777033447,-6.12459275374935,39.116));
#182518=CARTESIAN_POINT('',(60.2194255397045,-6.13776734223215,39.3343017080178));
#182519=CARTESIAN_POINT('',(0.0199126722524935,0.189456421067656,39.116));
#182520=CARTESIAN_POINT('Origin',(-0.019912672252488,-0.189456421067656,
2.80404091450791E-18));
#182521=CARTESIAN_POINT('',(61.5108137072212,-6.65659636252384,39.116));
#182522=CARTESIAN_POINT('',(61.9392677289269,-6.70162869482172,39.3548010137695));
#182523=CARTESIAN_POINT('Origin',(61.5488354179797,-6.66059260535659,39.5550293912439));
#182524=CARTESIAN_POINT('',(62.2936141127097,-6.73887200096311,39.92499));
#182525=CARTESIAN_POINT('',(61.9392677289269,-6.70162869482172,39.3548010137695));
#182526=CARTESIAN_POINT('',(58.872270023448,-6.37927424642578,39.92499));
#182527=CARTESIAN_POINT('',(-0.019912672252488,-0.189456421067656,39.92499));
#182528=CARTESIAN_POINT('',(59.2266168948024,-6.41651760264851,39.3548010137695));
#182529=CARTESIAN_POINT('',(58.872270023448,-6.37927424642578,39.92499));
#182530=CARTESIAN_POINT('',(59.6550713551493,-6.46154998175919,39.116));
#182531=CARTESIAN_POINT('Origin',(59.6170497662622,-6.45755375173563,39.5550297827282));
#182532=CARTESIAN_POINT('',(60.0542523589173,-6.50350559514667,39.116));
#182533=CARTESIAN_POINT('',(60.1277056317065,-6.51122584595708,39.116));
#182534=CARTESIAN_POINT('',(60.1796001951995,-6.51668018436746,39.3343017080178));
#182535=CARTESIAN_POINT('',(60.0542523588397,-6.50350559588466,39.116));
#182536=CARTESIAN_POINT('',(60.5077528318944,-6.55117041629769,39.5248017080178));
#182537=CARTESIAN_POINT('Origin',(60.4784867342332,-6.54809390915787,39.1947745585596));
#182538=CARTESIAN_POINT('',(60.6581326136904,-6.56697596826278,39.5248017080178));
#182539=CARTESIAN_POINT('',(60.6586584283283,-6.56703123360819,39.5248017080178));
#182540=CARTESIAN_POINT('',(60.9862851800404,-6.60146619279947,39.3343017080178));
#182541=CARTESIAN_POINT('Origin',(60.6874016969799,-6.57005175673948,39.194772859418));
#182542=CARTESIAN_POINT('',(61.1116329640613,-6.61464077578123,39.116));
#182543=CARTESIAN_POINT('',(60.9862851800404,-6.60146619279947,39.3343017080178));
#182544=CARTESIAN_POINT('',(61.5113322352818,-6.65665086201911,39.116));
#182545=CARTESIAN_POINT('Origin',(57.030176100279,-11.9273822599894,40.10025));
#182546=CARTESIAN_POINT('',(57.7354693911204,-12.2876333308471,40.10025));
#182547=CARTESIAN_POINT('',(61.4699285681954,-13.0814171332233,40.10025));
#182548=CARTESIAN_POINT('',(56.9874003490102,-12.1286263473644,40.10025));
#182549=CARTESIAN_POINT('',(61.4762657165316,-13.0516031943529,40.10025));
#182550=CARTESIAN_POINT('Origin',(5.50299975530876E-15,5.72544881825791E-15,
40.10025));
#182551=CARTESIAN_POINT('',(57.7418065394566,-12.2578193919768,40.10025));
#182552=CARTESIAN_POINT('',(57.672648524885,-12.2431194021875,40.10025));
#182553=CARTESIAN_POINT('Origin',(5.72166156020094E-15,5.2367941269311E-15,
40.10025));
#182554=CARTESIAN_POINT('Origin',(0.0396071771007832,0.18633711793979,-5.57736016997319E-18));
#182555=CARTESIAN_POINT('',(58.7320730967338,-12.2891316338724,39.116));
#182556=CARTESIAN_POINT('',(58.3106729199896,-12.1995602612165,39.3548010137695));
#182557=CARTESIAN_POINT('Origin',(58.6946775141703,-12.281182957421,39.5550297832841));
#182558=CARTESIAN_POINT('',(57.9621601887016,-12.1254815938991,39.92499));
#182559=CARTESIAN_POINT('',(58.3106729199896,-12.1995602612165,39.3548010137695));
#182560=CARTESIAN_POINT('',(61.3271735965893,-12.8407372733098,39.92499));
#182561=CARTESIAN_POINT('',(61.581282930652,-12.8947498796465,39.92499));
#182562=CARTESIAN_POINT('',(60.9786613449626,-12.7666587067855,39.3548010137695));
#182563=CARTESIAN_POINT('',(61.3271735965893,-12.8407372733098,39.92499));
#182564=CARTESIAN_POINT('',(60.5572615995843,-12.6770874264379,39.116));
#182565=CARTESIAN_POINT('Origin',(60.5946573025927,-12.6850361284907,39.5550293907183));
#182566=CARTESIAN_POINT('',(60.164653163458,-12.5936359264446,39.116));
#182567=CARTESIAN_POINT('',(0.0396071771007887,0.18633711793979,39.116));
#182568=CARTESIAN_POINT('',(60.0413691664787,-12.5674311046654,39.3343017080178));
#182569=CARTESIAN_POINT('',(60.16465316331,-12.5936359271408,39.116));
#182570=CARTESIAN_POINT('',(59.7186194643909,-12.4988285377096,39.5248017080178));
#182571=CARTESIAN_POINT('Origin',(59.7474037157358,-12.5049473440525,39.1947747614341));
#182572=CARTESIAN_POINT('',(59.5707156088321,-12.4673906027143,39.5248017080178));
#182573=CARTESIAN_POINT('',(0.0396071771007888,0.18633711793979,39.5248017080178));
#182574=CARTESIAN_POINT('',(59.2479658375576,-12.3987880210524,39.3343017080178));
#182575=CARTESIAN_POINT('Origin',(59.5419282989939,-12.4612721960121,39.1947728911945));
#182576=CARTESIAN_POINT('',(59.124681789249,-12.3725831876352,39.116));
#182577=CARTESIAN_POINT('',(59.2479658375576,-12.3987880210524,39.3343017080178));
#182578=CARTESIAN_POINT('',(0.0396071771007887,0.18633711793979,39.116));
#182579=CARTESIAN_POINT('Origin',(-0.0396071771007832,-0.18633711793979,
5.57736016997319E-18));
#182580=CARTESIAN_POINT('',(60.4780472453827,-13.0497616623175,39.116));
#182581=CARTESIAN_POINT('',(60.8994469906352,-13.139332943257,39.3548010137695));
#182582=CARTESIAN_POINT('Origin',(60.5154429481078,-13.05771036431,39.5550293912467));
#182583=CARTESIAN_POINT('',(61.2479592422937,-13.213411509632,39.92499));
#182584=CARTESIAN_POINT('',(60.8994469906352,-13.139332943257,39.3548010137695));
#182585=CARTESIAN_POINT('',(57.8829458346105,-12.4981558292588,39.92499));
#182586=CARTESIAN_POINT('',(-0.0396071771007831,-0.186337117939789,39.92499));
#182587=CARTESIAN_POINT('',(58.2314585659349,-12.5722344964053,39.3548010137695));
#182588=CARTESIAN_POINT('',(57.8829458346105,-12.4981558292588,39.92499));
#182589=CARTESIAN_POINT('',(58.6528587425322,-12.661805869752,39.116));
#182590=CARTESIAN_POINT('Origin',(58.6154631596733,-12.6538571932378,39.5550297827333));
#182591=CARTESIAN_POINT('',(59.0454674352017,-12.7452574227892,39.116));
#182592=CARTESIAN_POINT('',(59.1177113373238,-12.7606133389842,39.116));
#182593=CARTESIAN_POINT('',(59.1687514833561,-12.771462256932,39.3343017080178));
#182594=CARTESIAN_POINT('',(59.0454674350475,-12.7452574235148,39.116));
#182595=CARTESIAN_POINT('',(59.4915012546305,-12.8400648385939,39.5248017080178));
#182596=CARTESIAN_POINT('Origin',(59.4627170622795,-12.833946044668,39.1947745585571));
#182597=CARTESIAN_POINT('',(59.6394051101893,-12.8715027735892,39.5248017080178));
#182598=CARTESIAN_POINT('',(59.639922267558,-12.8716126987813,39.5248017080178));
#182599=CARTESIAN_POINT('',(59.9621548122771,-12.940105340545,39.3343017080178));
#182600=CARTESIAN_POINT('Origin',(59.6681923469408,-12.8776211648735,39.1947728594281));
#182601=CARTESIAN_POINT('',(60.0854388091085,-12.9663101630204,39.116));
#182602=CARTESIAN_POINT('',(59.9621548122771,-12.940105340545,39.3343017080178));
#182603=CARTESIAN_POINT('',(60.4785572361439,-13.0498700642002,39.116));
#182604=CARTESIAN_POINT('Origin',(55.4710078899933,-17.8233194796324,40.10025));
#182605=CARTESIAN_POINT('',(56.1347810195642,-18.2553202812749,40.10025));
#182606=CARTESIAN_POINT('',(59.7658094374951,-19.4351129318421,40.10025));
#182607=CARTESIAN_POINT('',(55.4074307335706,-18.018989847295,40.10025));
#182608=CARTESIAN_POINT('',(59.7752282754837,-19.4061247292254,40.10025));
#182609=CARTESIAN_POINT('Origin',(5.50698230308588E-15,5.74031188890569E-15,
40.10025));
#182610=CARTESIAN_POINT('',(56.1441998575527,-18.2263320786583,40.10025));
#182611=CARTESIAN_POINT('',(56.0769572651639,-18.2044836359653,40.10025));
#182612=CARTESIAN_POINT('Origin',(5.71958798166808E-15,5.229055426493E-15,
40.10025));
#182613=CARTESIAN_POINT('Origin',(0.0588677374284276,0.181176266354227,
-8.28957270027859E-18));
#182614=CARTESIAN_POINT('',(57.1257686104891,-18.3609838302741,39.116));
#182615=CARTESIAN_POINT('',(56.7160396659414,-18.2278548260738,39.3548010137695));
#182616=CARTESIAN_POINT('Origin',(57.0894087477753,-18.349169794726,39.5550297832868));
#182617=CARTESIAN_POINT('',(56.3771794531165,-18.1177524692162,39.92499));
#182618=CARTESIAN_POINT('',(56.7160396659414,-18.2278548260738,39.3548010137695));
#182619=CARTESIAN_POINT('',(59.6489943884564,-19.1808295835782,39.92499));
#182620=CARTESIAN_POINT('',(59.8960658302617,-19.2611079613975,39.92499));
#182621=CARTESIAN_POINT('',(59.3101346421293,-19.0707273771,39.3548010137695));
#182622=CARTESIAN_POINT('',(59.6489943884564,-19.1808295835782,39.92499));
#182623=CARTESIAN_POINT('',(58.9004061169357,-18.9375985097922,39.116));
#182624=CARTESIAN_POINT('Origin',(58.9367660967592,-18.9494125833915,39.5550293907195));
#182625=CARTESIAN_POINT('',(58.5186714879536,-18.8135654093531,39.116));
#182626=CARTESIAN_POINT('',(0.0588677374284331,0.181176266354227,39.116));
#182627=CARTESIAN_POINT('',(58.3988020033598,-18.77461745358,39.3343017080178));
#182628=CARTESIAN_POINT('',(58.5186714877335,-18.8135654100303,39.116));
#182629=CARTESIAN_POINT('',(58.08499127881,-18.6726541682846,39.5248017080178));
#182630=CARTESIAN_POINT('Origin',(58.1129782575897,-18.6817482287253,39.1947747614326));
#182631=CARTESIAN_POINT('',(57.9411838150807,-18.6259282908537,39.5248017080178));
#182632=CARTESIAN_POINT('',(0.0588677374284332,0.181176266354227,39.5248017080178));
#182633=CARTESIAN_POINT('',(57.6273730232605,-18.5239649837008,39.3343017080178));
#182634=CARTESIAN_POINT('Origin',(57.9131937527906,-18.6168343081654,39.1947728911901));
#182635=CARTESIAN_POINT('',(57.5075034888353,-18.4850170109878,39.116));
#182636=CARTESIAN_POINT('',(57.6273730232605,-18.5239649837008,39.3343017080178));
#182637=CARTESIAN_POINT('',(0.0588677374284331,0.181176266354227,39.116));
#182638=CARTESIAN_POINT('Origin',(-0.0588677374284276,-0.181176266354227,
8.28957270027859E-18));
#182639=CARTESIAN_POINT('',(58.7826706420788,-19.2999510425007,39.116));
#182640=CARTESIAN_POINT('',(59.1923991670855,-19.4330799103838,39.3548010137695));
#182641=CARTESIAN_POINT('Origin',(58.8190306216277,-19.3117651160107,39.5550293912458));
#182642=CARTESIAN_POINT('',(59.5312589134599,-19.5431821167165,39.92499));
#182643=CARTESIAN_POINT('',(59.1923991670855,-19.4330799103838,39.3548010137695));
#182644=CARTESIAN_POINT('',(56.2594439784239,-18.4801050014191,39.92499));
#182645=CARTESIAN_POINT('',(-0.0588677374284273,-0.181176266354225,39.92499));
#182646=CARTESIAN_POINT('',(56.5983041913028,-18.5902073581106,39.3548010137695));
#182647=CARTESIAN_POINT('',(56.2594439784239,-18.4801050014191,39.92499));
#182648=CARTESIAN_POINT('',(57.0080331356322,-18.7233363629825,39.116));
#182649=CARTESIAN_POINT('Origin',(56.9716732726282,-18.7115223273402,39.5550297827295));
#182650=CARTESIAN_POINT('',(57.3897680142076,-18.8473695429909,39.116));
#182651=CARTESIAN_POINT('',(57.460011026353,-18.8701928819395,39.116));
#182652=CARTESIAN_POINT('',(57.5096375484037,-18.8863175164093,39.3343017080178));
#182653=CARTESIAN_POINT('',(57.3897680139784,-18.8473695436963,39.116));
#182654=CARTESIAN_POINT('',(57.8234483402239,-18.9882808235621,39.5248017080178));
#182655=CARTESIAN_POINT('Origin',(57.7954614188153,-18.9791867816364,39.194774558559));
#182656=CARTESIAN_POINT('',(57.9672558039532,-19.0350067009931,39.5248017080178));
#182657=CARTESIAN_POINT('',(57.9677586379683,-19.0351700816685,39.5248017080178));
#182658=CARTESIAN_POINT('',(58.281066528503,-19.1369699862884,39.3343017080178));
#182659=CARTESIAN_POINT('Origin',(57.995245795169,-19.0441006607084,39.1947728594241));
#182660=CARTESIAN_POINT('',(58.4009360128767,-19.1759179427387,39.116));
#182661=CARTESIAN_POINT('',(58.281066528503,-19.1369699862884,39.3343017080178));
#182662=CARTESIAN_POINT('',(58.783166507975,-19.300112159097,39.116));
#182663=CARTESIAN_POINT('Origin',(53.3040877092102,-23.5239806812872,40.10025));
#182664=CARTESIAN_POINT('',(53.9190682401995,-24.0229981225297,40.10025));
#182665=CARTESIAN_POINT('',(57.4068835917979,-25.5758735661209,40.10025));
#182666=CARTESIAN_POINT('',(53.2204057122638,-23.7119335237426,40.10025));
#182667=CARTESIAN_POINT('',(57.4192809246789,-25.5480287005719,40.10025));
#182668=CARTESIAN_POINT('Origin',(5.51249664798382E-15,5.75467724849828E-15,
40.10025));
#182669=CARTESIAN_POINT('',(53.9314655730804,-23.9951532569808,40.10025));
#182670=CARTESIAN_POINT('',(53.8668751267878,-23.9663957374944,40.10025));
#182671=CARTESIAN_POINT('Origin',(5.71671684795091E-15,5.22157586744312E-15,
40.10025));
#182672=CARTESIAN_POINT('Origin',(0.0774833305059401,0.174030409680915,
-1.09109629373751E-17));
#182673=CARTESIAN_POINT('',(54.8935822490122,-24.2316692455484,39.116));
#182674=CARTESIAN_POINT('',(54.5000136127188,-24.0564411990328,39.3548010137695));
#182675=CARTESIAN_POINT('Origin',(54.8586564724101,-24.2161192879484,39.5550297832837));
#182676=CARTESIAN_POINT('',(54.1745185417599,-23.9115214570969,39.92499));
#182677=CARTESIAN_POINT('',(54.5000136127188,-24.0564411990328,39.3548010137695));
#182678=CARTESIAN_POINT('',(57.317288315449,-25.3107727110823,39.92499));
#182679=CARTESIAN_POINT('',(57.5546148985775,-25.4164373136774,39.92499));
#182680=CARTESIAN_POINT('',(56.9917936927132,-25.1658531674647,39.3548010137695));
#182681=CARTESIAN_POINT('',(57.317288315449,-25.3107727110823,39.92499));
#182682=CARTESIAN_POINT('',(56.5982254591675,-24.9906253009259,39.116));
#182683=CARTESIAN_POINT('Origin',(56.6331513482598,-25.0061753086097,39.5550293907183));
#182684=CARTESIAN_POINT('',(56.2315470018076,-24.8273695326456,39.116));
#182685=CARTESIAN_POINT('',(0.0774833305059456,0.174030409680915,39.116));
#182686=CARTESIAN_POINT('',(56.1164053447571,-24.7761051648318,39.3343017080178));
#182687=CARTESIAN_POINT('',(56.2315470015181,-24.8273695332957,39.116));
#182688=CARTESIAN_POINT('',(55.8149717737126,-24.6418982922878,39.5248017080178));
#182689=CARTESIAN_POINT('Origin',(55.8418548487303,-24.6538679703967,39.1947747614298));
#182690=CARTESIAN_POINT('',(55.6768362864792,-24.5803964109124,39.5248017080178));
#182691=CARTESIAN_POINT('',(0.0774833305059457,0.174030409680915,39.5248017080178));
#182692=CARTESIAN_POINT('',(55.3754026508175,-24.4461895095989,39.3343017080178));
#182693=CARTESIAN_POINT('Origin',(55.6499501367123,-24.568426487814,39.1947728911939));
#182694=CARTESIAN_POINT('',(55.260260945979,-24.3949251197295,39.116));
#182695=CARTESIAN_POINT('',(55.3754026508175,-24.4461895095989,39.3343017080178));
#182696=CARTESIAN_POINT('',(0.0774833305059456,0.174030409680915,39.116));
#182697=CARTESIAN_POINT('Origin',(-0.0774833305059401,-0.174030409680915,
1.09109629373751E-17));
#182698=CARTESIAN_POINT('',(56.4432587981556,-25.3386861202878,39.116));
#182699=CARTESIAN_POINT('',(56.8368270314553,-25.513913987379,39.3548010137695));
#182700=CARTESIAN_POINT('Origin',(56.4781846869833,-25.3542361278537,39.5550293912457));
#182701=CARTESIAN_POINT('',(57.1623216542531,-25.6588335308574,39.92499));
#182702=CARTESIAN_POINT('',(56.8368270314553,-25.513913987379,39.3548010137695));
#182703=CARTESIAN_POINT('',(54.0195518809641,-24.2595822759734,39.92499));
#182704=CARTESIAN_POINT('',(-0.0774833305059396,-0.174030409680913,39.92499));
#182705=CARTESIAN_POINT('',(54.3450469519941,-24.4045020177498,39.3548010137695));
#182706=CARTESIAN_POINT('',(54.0195518809641,-24.2595822759734,39.92499));
#182707=CARTESIAN_POINT('',(54.7386155880003,-24.5797300649102,39.116));
#182708=CARTESIAN_POINT('Origin',(54.703689811123,-24.5641801071878,39.5550297827337));
#182709=CARTESIAN_POINT('',(55.1052942852688,-24.7429859384138,39.116));
#182710=CARTESIAN_POINT('',(55.1727668102971,-24.7730266428385,39.116));
#182711=CARTESIAN_POINT('',(55.2204359898056,-24.7942503289608,39.3343017080178));
#182712=CARTESIAN_POINT('',(55.1052942849672,-24.7429859390914,39.116));
#182713=CARTESIAN_POINT('',(55.5218696254673,-24.9284572302742,39.5248017080178));
#182714=CARTESIAN_POINT('Origin',(55.49498660557,-24.9164875765753,39.194774558559));
#182715=CARTESIAN_POINT('',(55.6600051127008,-24.9899591116496,39.5248017080178));
#182716=CARTESIAN_POINT('',(55.6604881142076,-24.9901741577755,39.5248017080178));
#182717=CARTESIAN_POINT('',(55.9614386837453,-25.1241659841936,39.3343017080178));
#182718=CARTESIAN_POINT('Origin',(55.6868911941832,-25.0019290044714,39.1947728594271));
#182719=CARTESIAN_POINT('',(56.0765803405063,-25.1754303526576,39.116));
#182720=CARTESIAN_POINT('',(55.9614386837453,-25.1241659841936,39.3343017080178));
#182721=CARTESIAN_POINT('',(56.4437351063763,-25.3388981863707,39.116));
#182722=CARTESIAN_POINT('Origin',(50.5531567888875,-28.9669082278884,40.10025));
#182723=CARTESIAN_POINT('',(51.1126068659047,-29.5274749692186,40.10025));
#182724=CARTESIAN_POINT('',(54.4189959163063,-31.4364195775136,40.10025));
#182725=CARTESIAN_POINT('',(50.4502867888875,-29.145084294463,40.10025));
#182726=CARTESIAN_POINT('',(54.4342359163063,-31.4100231232062,40.10025));
#182727=CARTESIAN_POINT('Origin',(5.51948237368594E-15,5.76838750714983E-15,
40.10025));
#182728=CARTESIAN_POINT('',(51.1278468659047,-29.5010785149112,40.10025));
#182729=CARTESIAN_POINT('',(51.0666162321543,-29.4657269920328,40.10025));
#182730=CARTESIAN_POINT('Origin',(5.71307961579125E-15,5.2144373973956E-15,
40.10025));
#182731=CARTESIAN_POINT('Origin',(0.0952500000000002,0.164977839420935,
-1.3412810381264E-17));
#182732=CARTESIAN_POINT('',(52.0599703131946,-29.8368674217657,39.116));
#182733=CARTESIAN_POINT('',(51.6868740054943,-29.6214601680812,39.3548010137695));
#182734=CARTESIAN_POINT('Origin',(52.0268612768236,-29.8177519107043,39.5550297832855));
#182735=CARTESIAN_POINT('',(51.3783102685129,-29.4433108120862,39.92499));
#182736=CARTESIAN_POINT('',(51.6868740054943,-29.6214601680812,39.3548010137695));
#182737=CARTESIAN_POINT('',(54.3576020372438,-31.1634057161441,39.92499));
#182738=CARTESIAN_POINT('',(54.582583561987,-31.2932988600173,39.92499));
#182739=CARTESIAN_POINT('',(54.0490387253005,-30.9852566042327,39.3548010137695));
#182740=CARTESIAN_POINT('',(54.3576020372438,-31.1634057161441,39.92499));
#182741=CARTESIAN_POINT('',(53.6759427993286,-30.7698495716382,39.116));
#182742=CARTESIAN_POINT('Origin',(53.7090519423387,-30.7889651442676,39.5550293907189));
#182743=CARTESIAN_POINT('',(53.3283379195023,-30.5691597998769,39.116));
#182744=CARTESIAN_POINT('',(0.0952500000000057,0.164977839420935,39.116));
#182745=CARTESIAN_POINT('',(53.2191856060845,-30.5061406831644,39.3343017080178));
#182746=CARTESIAN_POINT('',(53.3283379191464,-30.5691598004933,39.116));
#182747=CARTESIAN_POINT('',(52.9334317578287,-30.3411606219519,39.5248017080178));
#182748=CARTESIAN_POINT('Origin',(52.958916392489,-30.3558747754306,39.1947747614273));
#182749=CARTESIAN_POINT('',(52.8024816883959,-30.2655565641145,39.5248017080178));
#182750=CARTESIAN_POINT('',(0.0952500000000058,0.164977839420935,39.5248017080178));
#182751=CARTESIAN_POINT('',(52.5167277788841,-30.1005764675359,39.3343017080178));
#182752=CARTESIAN_POINT('Origin',(52.7769940214392,-30.2508418455899,39.1947728911908));
#182753=CARTESIAN_POINT('',(52.4075754202456,-30.0375573238933,39.116));
#182754=CARTESIAN_POINT('',(52.5167277788841,-30.1005764675359,39.3343017080178));
#182755=CARTESIAN_POINT('',(0.0952500000000057,0.164977839420935,39.116));
#182756=CARTESIAN_POINT('Origin',(-0.0952500000000002,-0.164977839420935,
1.3412810381264E-17));
#182757=CARTESIAN_POINT('',(53.4854427993286,-31.09980525048,39.116));
#182758=CARTESIAN_POINT('',(53.8585387249979,-31.3152122835987,39.3548010137695));
#182759=CARTESIAN_POINT('Origin',(53.518551942088,-31.1189208229648,39.5550293912464));
#182760=CARTESIAN_POINT('',(54.1671020370176,-31.4933613953777,39.92499));
#182761=CARTESIAN_POINT('',(53.8585387249979,-31.3152122835987,39.3548010137695));
#182762=CARTESIAN_POINT('',(51.1878102687785,-29.7732664904681,39.92499));
#182763=CARTESIAN_POINT('',(-0.0952499999999994,-0.164977839420933,39.92499));
#182764=CARTESIAN_POINT('',(51.4963740058478,-29.9514158463108,39.3548010137695));
#182765=CARTESIAN_POINT('',(51.1878102687785,-29.7732664904681,39.92499));
#182766=CARTESIAN_POINT('',(51.8694703131946,-30.1668231006075,39.116));
#182767=CARTESIAN_POINT('Origin',(51.8363612765606,-30.1477075893943,39.5550297827308));
#182768=CARTESIAN_POINT('',(52.2170754206164,-30.3675130020929,39.116));
#182769=CARTESIAN_POINT('',(52.2810382154239,-30.4044419397494,39.116));
#182770=CARTESIAN_POINT('',(52.3262277788841,-30.4305321463777,39.3343017080178));
#182771=CARTESIAN_POINT('',(52.2170754202456,-30.3675130027351,39.116));
#182772=CARTESIAN_POINT('',(52.6119816883959,-30.5955122429563,39.5248017080178));
#182773=CARTESIAN_POINT('Origin',(52.5864971060027,-30.5807981195157,39.1947745585563));
#182774=CARTESIAN_POINT('',(52.7429317578287,-30.6711163007938,39.5248017080178));
#182775=CARTESIAN_POINT('',(52.7433896349617,-30.6713806562798,39.5248017080178));
#182776=CARTESIAN_POINT('',(53.0286856060845,-30.8360963620063,39.3343017080178));
#182777=CARTESIAN_POINT('Origin',(52.7684193600401,-30.68583098207,39.1947728594247));
#182778=CARTESIAN_POINT('',(53.1378379191464,-30.8991154793352,39.116));
#182779=CARTESIAN_POINT('',(53.0286856060845,-30.8360963620063,39.3343017080178));
#182780=CARTESIAN_POINT('',(53.4858943313413,-31.1000659426091,39.116));
#182781=CARTESIAN_POINT('Origin',(47.2483549038575,-34.0924682662295,40.10025));
#182782=CARTESIAN_POINT('',(47.7461450747864,-34.7084426211232,40.10025));
#182783=CARTESIAN_POINT('',(50.8348823336486,-36.9525415975213,40.10025));
#182784=CARTESIAN_POINT('',(47.1274239660509,-34.2589154226522,40.10025));
#182785=CARTESIAN_POINT('',(50.8527980281384,-36.9278827595327,40.10025));
#182786=CARTESIAN_POINT('Origin',(5.52786294311959E-15,5.78129245239752E-15,
40.10025));
#182787=CARTESIAN_POINT('',(47.7640607692763,-34.6837837831347,40.10025));
#182788=CARTESIAN_POINT('',(47.706860803705,-34.6422255755467,40.10025));
#182789=CARTESIAN_POINT('Origin',(5.70871613546578E-15,5.20771822692212E-15,
40.10025));
#182790=CARTESIAN_POINT('Origin',(0.111973090561716,0.154117737428427,-1.57677042678047E-17));
#182791=CARTESIAN_POINT('',(48.6559784483765,-35.1151666347442,39.116));
#182792=CARTESIAN_POINT('',(48.3074421904918,-34.8619402208391,39.3548010137695));
#182793=CARTESIAN_POINT('Origin',(48.6250489017663,-35.09269500376,39.5550297832842));
#182794=CARTESIAN_POINT('',(48.019190476361,-34.6525130924099,39.92499));
#182795=CARTESIAN_POINT('',(48.3074421904918,-34.8619402208391,39.3548010137695));
#182796=CARTESIAN_POINT('',(50.8023624960591,-36.6746059268179,39.92499));
#182797=CARTESIAN_POINT('',(51.0125340177515,-36.827304475503,39.92499));
#182798=CARTESIAN_POINT('',(50.5141111791244,-36.4651790855637,39.3548010137695));
#182799=CARTESIAN_POINT('',(50.8023624960591,-36.6746059268179,39.92499));
#182800=CARTESIAN_POINT('',(50.1655752777671,-36.2119529314385,39.116));
#182801=CARTESIAN_POINT('Origin',(50.196504923995,-36.2344246347993,39.5550293907212));
#182802=CARTESIAN_POINT('',(49.8408524072787,-35.976027955333,39.116));
#182803=CARTESIAN_POINT('',(0.111973090561722,0.154117737428427,39.116));
#182804=CARTESIAN_POINT('',(49.7388853330811,-35.9019445403519,39.3343017080178));
#182805=CARTESIAN_POINT('',(49.8408524068603,-35.9760279559088,39.116));
#182806=CARTESIAN_POINT('',(49.4719419865733,-35.7079988465459,39.5248017080178));
#182807=CARTESIAN_POINT('Origin',(49.4957489658851,-35.7252962640489,39.1947747614236));
#182808=CARTESIAN_POINT('',(49.3496120513049,-35.6191209461253,39.5248017080178));
#182809=CARTESIAN_POINT('',(0.111973090561722,0.154117737428427,39.5248017080178));
#182810=CARTESIAN_POINT('',(49.0826686475734,-35.4251752107439,39.3343017080178));
#182811=CARTESIAN_POINT('Origin',(49.3258021153687,-35.6018226497085,39.1947728911923));
#182812=CARTESIAN_POINT('',(48.9807015312178,-35.3510917642534,39.116));
#182813=CARTESIAN_POINT('',(49.0826686475734,-35.4251752107439,39.3343017080178));
#182814=CARTESIAN_POINT('',(0.111973090561722,0.154117737428427,39.116));
#182815=CARTESIAN_POINT('Origin',(-0.111973090561716,-0.154117737428427,
1.57677042678047E-17));
#182816=CARTESIAN_POINT('',(49.9416290966437,-36.5201884062954,39.116));
#182817=CARTESIAN_POINT('',(50.2901649976455,-36.7734145609099,39.3548010137695));
#182818=CARTESIAN_POINT('Origin',(49.9725587426391,-36.5426601094872,39.5550293912449));
#182819=CARTESIAN_POINT('',(50.5784163146695,-36.9828414020411,39.92499));
#182820=CARTESIAN_POINT('',(50.2901649976455,-36.7734145609099,39.3548010137695));
#182821=CARTESIAN_POINT('',(47.7952442955502,-34.9607485668366,39.92499));
#182822=CARTESIAN_POINT('',(-0.111973090561715,-0.154117737428424,39.92499));
#182823=CARTESIAN_POINT('',(48.0834960097836,-35.1701756951243,39.3548010137695));
#182824=CARTESIAN_POINT('',(47.7952442955502,-34.9607485668366,39.92499));
#182825=CARTESIAN_POINT('',(48.432032267253,-35.423402109601,39.116));
#182826=CARTESIAN_POINT('Origin',(48.4011027203971,-35.4009304784382,39.5550297827298));
#182827=CARTESIAN_POINT('',(48.7567553505303,-35.6593272385103,39.116));
#182828=CARTESIAN_POINT('',(48.8165076253519,-35.7027398082299,39.116));
#182829=CARTESIAN_POINT('',(48.85872246645,-35.7334106856007,39.3343017080178));
#182830=CARTESIAN_POINT('',(48.7567553500944,-35.6593272391103,39.116));
#182831=CARTESIAN_POINT('',(49.1256658701815,-35.9273564209821,39.5248017080178));
#182832=CARTESIAN_POINT('Origin',(49.1018589397078,-35.910059038814,39.1947745585581));
#182833=CARTESIAN_POINT('',(49.2479958054498,-36.0162343214027,39.5248017080178));
#182834=CARTESIAN_POINT('',(49.2484235416113,-36.0165450899148,39.5248017080178));
#182835=CARTESIAN_POINT('',(49.5149391519577,-36.2101800152087,39.3343017080178));
#182836=CARTESIAN_POINT('Origin',(49.2718056808862,-36.0335325740054,39.1947728594183));
#182837=CARTESIAN_POINT('',(49.6169062257369,-36.2842634307656,39.116));
#182838=CARTESIAN_POINT('',(49.5149391519577,-36.2101800152087,39.3343017080178));
#182839=CARTESIAN_POINT('',(49.9420509053691,-36.5204948682731,39.116));
#182840=CARTESIAN_POINT('Origin',(43.425890155147,-38.8445040879382,40.10025));
#182841=CARTESIAN_POINT('',(43.8565665267056,-39.5091373124623,40.10025));
#182842=CARTESIAN_POINT('',(46.6938111422604,-42.0638038389701,40.10025));
#182843=CARTESIAN_POINT('',(43.2882232241948,-38.997398704332,40.10025));
#182844=CARTESIAN_POINT('',(46.7142062431422,-42.0411527846896,40.10025));
#182845=CARTESIAN_POINT('Origin',(5.5375465370123E-15,5.79325069496066E-15,
40.10025));
#182846=CARTESIAN_POINT('',(43.8769616275874,-39.4864862581817,40.10025));
#182847=CARTESIAN_POINT('',(43.8244190249878,-39.4391766863031,40.10025));
#182848=CARTESIAN_POINT('Origin',(5.70367421417806E-15,5.20149197266044E-15,
40.10025));
#182849=CARTESIAN_POINT('Origin',(0.127469380511363,0.141569089253443,-1.79498438867831E-17));
#182850=CARTESIAN_POINT('',(44.7189015017598,-40.0087367337514,39.116));
#182851=CARTESIAN_POINT('',(44.398743929868,-39.7204655612074,39.3548010137695));
#182852=CARTESIAN_POINT('Origin',(44.6904903154964,-39.9831551867365,39.5550297832852));
#182853=CARTESIAN_POINT('',(44.1339623846891,-39.482055187788,39.92499));
#182854=CARTESIAN_POINT('',(44.398743929868,-39.7204655612074,39.3548010137695));
#182855=CARTESIAN_POINT('',(46.6905216402897,-41.7839914803027,39.92499));
#182856=CARTESIAN_POINT('',(46.8835804757584,-41.9578224365462,39.92499));
#182857=CARTESIAN_POINT('',(46.425740460113,-41.5455814340034,39.3548010137695));
#182858=CARTESIAN_POINT('',(46.6905216402897,-41.7839914803027,39.92499));
#182859=CARTESIAN_POINT('',(46.1055832156409,-41.2573105570837,39.116));
#182860=CARTESIAN_POINT('Origin',(46.1339944934108,-41.2828921864915,39.5550293907218));
#182861=CARTESIAN_POINT('',(45.8073000862121,-40.9887352200425,39.116));
#182862=CARTESIAN_POINT('',(0.127469380511368,0.141569089253443,39.116));
#182863=CARTESIAN_POINT('',(45.7136354238375,-40.9043991801904,39.3343017080178));
#182864=CARTESIAN_POINT('',(45.8073000857358,-40.9887352205714,39.116));
#182865=CARTESIAN_POINT('',(45.4684272662435,-40.6836127633979,39.5248017080178));
#182866=CARTESIAN_POINT('Origin',(45.4902957559679,-40.7033039308062,39.1947747614394));
#182867=CARTESIAN_POINT('',(45.3560577375095,-40.58243478527,39.5248017080178));
#182868=CARTESIAN_POINT('',(0.127469380511368,0.141569089253443,39.5248017080178));
#182869=CARTESIAN_POINT('',(45.1108495273512,-40.3616483211485,39.3343017080178));
#182870=CARTESIAN_POINT('Origin',(45.3341863992353,-40.5627424347171,39.1947728911915));
#182871=CARTESIAN_POINT('',(45.0171848263432,-40.2773122455529,39.116));
#182872=CARTESIAN_POINT('',(45.1108495273512,-40.3616483211485,39.3343017080178));
#182873=CARTESIAN_POINT('',(0.127469380511368,0.141569089253443,39.116));
#182874=CARTESIAN_POINT('Origin',(-0.127469380511363,-0.141569089253443,
1.79498438867831E-17));
#182875=CARTESIAN_POINT('',(45.8506444546181,-41.5404487355906,39.116));
#182876=CARTESIAN_POINT('',(46.1708016986853,-41.82871961296,39.3548010137695));
#182877=CARTESIAN_POINT('Origin',(45.8790557321746,-41.5660303648061,39.5550293912458));
#182878=CARTESIAN_POINT('',(46.4355828789645,-42.0671296591456,39.92499));
#182879=CARTESIAN_POINT('',(46.1708016986853,-41.82871961296,39.3548010137695));
#182880=CARTESIAN_POINT('',(43.8790236240219,-39.7651933658999,39.92499));
#182881=CARTESIAN_POINT('',(-0.127469380511361,-0.14156908925344,39.92499));
#182882=CARTESIAN_POINT('',(44.1438051693183,-40.003603739189,39.3548010137695));
#182883=CARTESIAN_POINT('',(43.8790236240219,-39.7651933658999,39.92499));
#182884=CARTESIAN_POINT('',(44.4639627407371,-40.2918749122583,39.116));
#182885=CARTESIAN_POINT('Origin',(44.4355515542499,-40.2662933650419,39.5550297827353));
#182886=CARTESIAN_POINT('',(44.7622460658165,-40.5604504235089,39.116));
#182887=CARTESIAN_POINT('',(44.8171331622256,-40.6098709880929,39.116));
#182888=CARTESIAN_POINT('',(44.8559107663285,-40.6447864996553,39.3343017080178));
#182889=CARTESIAN_POINT('',(44.7622460653205,-40.5604504240598,39.116));
#182890=CARTESIAN_POINT('',(45.1011189764868,-40.8655729637769,39.5248017080178));
#182891=CARTESIAN_POINT('Origin',(45.0792505316454,-40.8458818366201,39.1947745585599));
#182892=CARTESIAN_POINT('',(45.2134885052208,-40.9667509419048,39.5248017080178));
#182893=CARTESIAN_POINT('',(45.2138814140438,-40.9671047185981,39.5248017080178));
#182894=CARTESIAN_POINT('',(45.4586966628148,-41.1875373586973,39.3343017080178));
#182895=CARTESIAN_POINT('Origin',(45.2353597879066,-40.9864432425598,39.1947728594184));
#182896=CARTESIAN_POINT('',(45.5523613247131,-41.2718733990783,39.116));
#182897=CARTESIAN_POINT('',(45.4586966628148,-41.1875373586973,39.3343017080178));
#182898=CARTESIAN_POINT('',(45.8510319186316,-41.5407976097554,39.116));
#182899=CARTESIAN_POINT('Origin',(39.127642266445,-43.1709513941244,40.10025));
#182900=CARTESIAN_POINT('',(39.4864862581816,-43.8769616275875,40.10025));
#182901=CARTESIAN_POINT('',(42.0411527846894,-46.7142062431423,40.10025));
#182902=CARTESIAN_POINT('',(38.9747476500513,-43.3086183250767,40.10025));
#182903=CARTESIAN_POINT('',(42.06380383897,-46.6938111422605,40.10025));
#182904=CARTESIAN_POINT('Origin',(5.54842705988296E-15,5.80413121783132E-15,
40.10025));
#182905=CARTESIAN_POINT('',(39.5091373124621,-43.8565665267057,40.10025));
#182906=CARTESIAN_POINT('',(39.4618277405835,-43.804023924106,40.10025));
#182907=CARTESIAN_POINT('Origin',(5.69800909227282E-15,5.1958268507552E-15,
40.10025));
#182908=CARTESIAN_POINT('Origin',(0.141569089253444,0.127469380511362,-1.99353212598916E-17));
#182909=CARTESIAN_POINT('',(40.2918749122581,-44.4639627407372,39.116));
#182910=CARTESIAN_POINT('',(40.0036037397142,-44.1438051688454,39.3548010137695));
#182911=CARTESIAN_POINT('Origin',(40.2662933652425,-44.4355515544729,39.5550297832825));
#182912=CARTESIAN_POINT('',(39.7651933655048,-43.8790236243778,39.92499));
#182913=CARTESIAN_POINT('',(40.0036037397142,-44.1438051688454,39.3548010137695));
#182914=CARTESIAN_POINT('',(42.0671296588095,-46.4355828792671,39.92499));
#182915=CARTESIAN_POINT('',(42.240960615053,-46.6286417147358,39.92499));
#182916=CARTESIAN_POINT('',(41.8287196134096,-46.1708016982805,39.3548010137695));
#182917=CARTESIAN_POINT('',(42.0671296588095,-46.4355828792671,39.92499));
#182918=CARTESIAN_POINT('',(41.5404487355905,-45.8506444546183,39.116));
#182919=CARTESIAN_POINT('Origin',(41.5660303649986,-45.8790557323886,39.5550293907208));
#182920=CARTESIAN_POINT('',(41.2718733996072,-45.5523613242369,39.116));
#182921=CARTESIAN_POINT('',(0.141569089253449,0.127469380511362,39.116));
#182922=CARTESIAN_POINT('',(41.1875373586971,-45.4586966628149,39.3343017080178));
#182923=CARTESIAN_POINT('',(41.2718733990782,-45.5523613247132,39.116));
#182924=CARTESIAN_POINT('',(40.9667509419047,-45.2134885052209,39.5248017080178));
#182925=CARTESIAN_POINT('Origin',(40.9864413462789,-45.2353576819716,39.1947747614227));
#182926=CARTESIAN_POINT('',(40.8655729637768,-45.101118976487,39.5248017080178));
#182927=CARTESIAN_POINT('',(0.141569089253449,0.127469380511362,39.5248017080178));
#182928=CARTESIAN_POINT('',(40.6447864996552,-44.8559107663286,39.3343017080178));
#182929=CARTESIAN_POINT('Origin',(40.8458798501228,-45.0792483253108,39.1947728911931));
#182930=CARTESIAN_POINT('',(40.5604504240596,-44.7622460653206,39.116));
#182931=CARTESIAN_POINT('',(40.6447864996552,-44.8559107663286,39.3343017080178));
#182932=CARTESIAN_POINT('',(0.141569089253449,0.127469380511362,39.116));
#182933=CARTESIAN_POINT('Origin',(-0.141569089253444,-0.127469380511362,
1.99353212598916E-17));
#182934=CARTESIAN_POINT('',(41.2573105570836,-46.105583215641,39.116));
#182935=CARTESIAN_POINT('',(41.5455814344529,-46.4257404597082,39.3548010137695));
#182936=CARTESIAN_POINT('Origin',(41.2828921862997,-46.1339944931981,39.555029391244));
#182937=CARTESIAN_POINT('',(41.7839914799665,-46.6905216405924,39.92499));
#182938=CARTESIAN_POINT('',(41.5455814344529,-46.4257404597082,39.3548010137695));
#182939=CARTESIAN_POINT('',(39.4820551873929,-44.1339623850448,39.92499));
#182940=CARTESIAN_POINT('',(-0.141569089253442,-0.127469380511358,39.92499));
#182941=CARTESIAN_POINT('',(39.7204655617324,-44.3987439293954,39.3548010137695));
#182942=CARTESIAN_POINT('',(39.4820551873929,-44.1339623850448,39.92499));
#182943=CARTESIAN_POINT('',(40.0087367337512,-44.7189015017599,39.116));
#182944=CARTESIAN_POINT('Origin',(39.9831551865335,-44.6904903152712,39.5550297827315));
#182945=CARTESIAN_POINT('',(40.2773122461036,-45.0171848258473,39.116));
#182946=CARTESIAN_POINT('',(40.3267328095859,-45.0720719232484,39.116));
#182947=CARTESIAN_POINT('',(40.3616483211483,-45.1108495273513,39.3343017080178));
#182948=CARTESIAN_POINT('',(40.2773122455527,-45.0171848263433,39.116));
#182949=CARTESIAN_POINT('',(40.5824347852699,-45.3560577375097,39.5248017080178));
#182950=CARTESIAN_POINT('Origin',(40.5627444213182,-45.3341886054734,39.1947745585617));
#182951=CARTESIAN_POINT('',(40.6836127633978,-45.4684272662437,39.5248017080178));
#182952=CARTESIAN_POINT('',(40.6839665400911,-45.4688201750666,39.5248017080178));
#182953=CARTESIAN_POINT('',(40.9043991801903,-45.7136354238376,39.3343017080178));
#182954=CARTESIAN_POINT('Origin',(40.7033058269822,-45.4902978619832,39.1947728594174));
#182955=CARTESIAN_POINT('',(40.9887352205713,-45.807300085736,39.116));
#182956=CARTESIAN_POINT('',(40.9043991801903,-45.7136354238376,39.3343017080178));
#182957=CARTESIAN_POINT('',(41.2576594312484,-46.1059706796545,39.116));
#182958=CARTESIAN_POINT('Origin',(34.4007037410862,-47.0244087227342,40.10025));
#182959=CARTESIAN_POINT('',(34.6837837831345,-47.7640607692764,40.10025));
#182960=CARTESIAN_POINT('',(36.9278827595326,-50.8527980281386,40.10025));
#182961=CARTESIAN_POINT('',(34.2342565846635,-47.1453396605409,40.10025));
#182962=CARTESIAN_POINT('',(36.9525415975211,-50.8348823336487,40.10025));
#182963=CARTESIAN_POINT('Origin',(5.5603853024461E-15,5.81381481172403E-15,
40.10025));
#182964=CARTESIAN_POINT('',(34.7084426211231,-47.7461450747865,40.10025));
#182965=CARTESIAN_POINT('',(34.6668844135351,-47.6889451092152,40.10025));
#182966=CARTESIAN_POINT('Origin',(5.69178283801114E-15,5.19078492946748E-15,
40.10025));
#182967=CARTESIAN_POINT('Origin',(0.154117737428428,0.111973090561716,-2.17023830815426E-17));
#182968=CARTESIAN_POINT('',(35.4234021096009,-48.4320322672531,39.116));
#182969=CARTESIAN_POINT('',(35.1701756956958,-48.0834960093684,39.3548010137695));
#182970=CARTESIAN_POINT('Origin',(35.4009304786184,-48.4011027206453,39.5550297832894));
#182971=CARTESIAN_POINT('',(34.9607485664066,-47.7952442958626,39.92499));
#182972=CARTESIAN_POINT('',(35.1701756956958,-48.0834960093684,39.3548010137695));
#182973=CARTESIAN_POINT('',(36.9828414016746,-50.5784163149358,39.92499));
#182974=CARTESIAN_POINT('',(37.1355399503597,-50.7885878366282,39.92499));
#182975=CARTESIAN_POINT('',(36.7734145613992,-50.29016499729,39.3548010137695));
#182976=CARTESIAN_POINT('',(36.9828414016746,-50.5784163149357,39.92499));
#182977=CARTESIAN_POINT('',(36.5201884062952,-49.9416290966438,39.116));
#182978=CARTESIAN_POINT('Origin',(36.5426601096567,-49.9725587428728,39.5550293907182));
#182979=CARTESIAN_POINT('',(36.284263431341,-49.6169062253189,39.116));
#182980=CARTESIAN_POINT('',(0.154117737428433,0.111973090561716,39.116));
#182981=CARTESIAN_POINT('',(36.2101800152086,-49.5149391519578,39.3343017080178));
#182982=CARTESIAN_POINT('',(36.2842634307655,-49.616906225737,39.116));
#182983=CARTESIAN_POINT('',(36.0162343214026,-49.24799580545,39.5248017080178));
#182984=CARTESIAN_POINT('Origin',(36.0335309082456,-49.2718033882767,39.1947747614309));
#182985=CARTESIAN_POINT('',(35.927356420982,-49.1256658701816,39.5248017080178));
#182986=CARTESIAN_POINT('',(0.154117737428433,0.111973090561716,39.5248017080178));
#182987=CARTESIAN_POINT('',(35.7334106856005,-48.8587224664501,39.3343017080178));
#182988=CARTESIAN_POINT('Origin',(35.9100572938238,-49.1018565378146,39.1947728911917));
#182989=CARTESIAN_POINT('',(35.6593272391101,-48.7567553500945,39.116));
#182990=CARTESIAN_POINT('',(35.7334106856005,-48.8587224664501,39.3343017080178));
#182991=CARTESIAN_POINT('',(0.154117737428433,0.111973090561716,39.116));
#182992=CARTESIAN_POINT('Origin',(-0.154117737428428,-0.111973090561716,
2.17023830815426E-17));
#182993=CARTESIAN_POINT('',(36.2119529314384,-50.1655752777672,39.116));
#182994=CARTESIAN_POINT('',(36.4651790860528,-50.514111178769,39.3548010137695));
#182995=CARTESIAN_POINT('Origin',(36.2344246346305,-50.196504923763,39.5550293912442));
#182996=CARTESIAN_POINT('',(36.6746059264518,-50.802362496325,39.92499));
#182997=CARTESIAN_POINT('',(36.4651790860528,-50.514111178769,39.3548010137695));
#182998=CARTESIAN_POINT('',(34.6525130919796,-48.0191904766737,39.92499));
#182999=CARTESIAN_POINT('',(-0.154117737428425,-0.111973090561711,39.92499));
#183000=CARTESIAN_POINT('',(34.8619402214101,-48.3074421900769,39.3548010137695));
#183001=CARTESIAN_POINT('',(34.6525130919796,-48.0191904766737,39.92499));
#183002=CARTESIAN_POINT('',(35.115166634744,-48.6559784483766,39.116));
#183003=CARTESIAN_POINT('Origin',(35.0926950035817,-48.6250489015213,39.5550297827311));
#183004=CARTESIAN_POINT('',(35.3510917648534,-48.9807015307819,39.116));
#183005=CARTESIAN_POINT('',(35.3945043333729,-49.0404538064755,39.116));
#183006=CARTESIAN_POINT('',(35.4251752107437,-49.0826686475735,39.3343017080178));
#183007=CARTESIAN_POINT('',(35.3510917642532,-48.9807015312179,39.116));
#183008=CARTESIAN_POINT('',(35.6191209461251,-49.349612051305,39.5248017080178));
#183009=CARTESIAN_POINT('Origin',(35.6018243948131,-49.3258045171787,39.1947745585585));
#183010=CARTESIAN_POINT('',(35.7079988465457,-49.4719419865734,39.5248017080178));
#183011=CARTESIAN_POINT('',(35.7083096150578,-49.4723697227348,39.5248017080178));
#183012=CARTESIAN_POINT('',(35.9019445403517,-49.7388853330812,39.3343017080178));
#183013=CARTESIAN_POINT('Origin',(35.7252979297061,-49.4957512585778,39.1947728594245));
#183014=CARTESIAN_POINT('',(35.9760279559086,-49.8408524068605,39.116));
#183015=CARTESIAN_POINT('',(35.9019445403517,-49.7388853330812,39.3343017080178));
#183016=CARTESIAN_POINT('',(36.2122593934161,-50.1659970864927,39.116));
#183017=CARTESIAN_POINT('Origin',(29.2968639067301,-50.3626567888876,40.10025));
#183018=CARTESIAN_POINT('',(29.501078514911,-51.1278468659048,40.10025));
#183019=CARTESIAN_POINT('',(31.410023123206,-54.4342359163064,40.10025));
#183020=CARTESIAN_POINT('',(29.1186878401555,-50.4655267888876,40.10025));
#183021=CARTESIAN_POINT('',(31.4364195775134,-54.4189959163064,40.10025));
#183022=CARTESIAN_POINT('Origin',(5.57329024769379E-15,5.82219538115768E-15,
40.10025));
#183023=CARTESIAN_POINT('',(29.5274749692184,-51.1126068659048,40.10025));
#183024=CARTESIAN_POINT('',(29.49212344634,-51.0513762321545,40.10025));
#183025=CARTESIAN_POINT('Origin',(5.68506366753766E-15,5.18642144914201E-15,
40.10025));
#183026=CARTESIAN_POINT('Origin',(0.164977839420936,0.0952499999999996,
-2.32316690526365E-17));
#183027=CARTESIAN_POINT('',(30.1668231006074,-51.8694703131947,39.116));
#183028=CARTESIAN_POINT('',(29.9514158469229,-51.4963740054944,39.3548010137695));
#183029=CARTESIAN_POINT('Origin',(30.1477075895458,-51.8363612768235,39.5550297832851));
#183030=CARTESIAN_POINT('',(29.7732664900074,-51.1878102690444,39.92499));
#183031=CARTESIAN_POINT('',(29.9514158469229,-51.4963740054944,39.3548010137695));
#183032=CARTESIAN_POINT('',(31.4933613949858,-54.1671020372439,39.92499));
#183033=CARTESIAN_POINT('',(31.623254538859,-54.3920835619871,39.92499));
#183034=CARTESIAN_POINT('',(31.3152122841232,-53.8585387246951,39.3548010137695));
#183035=CARTESIAN_POINT('',(31.4933613949858,-54.1671020372439,39.92499));
#183036=CARTESIAN_POINT('',(31.0998052504799,-53.4854427993287,39.116));
#183037=CARTESIAN_POINT('Origin',(31.1189208231087,-53.5185519423377,39.5550293907207));
#183038=CARTESIAN_POINT('',(30.8991154799516,-53.1378379187905,39.116));
#183039=CARTESIAN_POINT('',(0.164977839420941,0.0952499999999996,39.116));
#183040=CARTESIAN_POINT('',(30.8360963620061,-53.0286856060847,39.3343017080178));
#183041=CARTESIAN_POINT('',(30.899115479335,-53.1378379191465,39.116));
#183042=CARTESIAN_POINT('',(30.6711163007936,-52.7429317578288,39.5248017080178));
#183043=CARTESIAN_POINT('Origin',(30.6858295650754,-52.7684169058653,39.1947747614259));
#183044=CARTESIAN_POINT('',(30.5955122429562,-52.611981688396,39.5248017080178));
#183045=CARTESIAN_POINT('',(0.164977839420941,0.0952499999999996,39.5248017080178));
#183046=CARTESIAN_POINT('',(30.4305321463776,-52.3262277788842,39.3343017080178));
#183047=CARTESIAN_POINT('Origin',(30.5807966351526,-52.5864945348689,39.1947728911841));
#183048=CARTESIAN_POINT('',(30.367513002735,-52.2170754202457,39.116));
#183049=CARTESIAN_POINT('',(30.4305321463776,-52.3262277788842,39.3343017080178));
#183050=CARTESIAN_POINT('',(0.164977839420941,0.0952499999999996,39.116));
#183051=CARTESIAN_POINT('Origin',(-0.164977839420936,-0.0952499999999996,
2.32316690526365E-17));
#183052=CARTESIAN_POINT('',(30.769849571638,-53.6759427993287,39.116));
#183053=CARTESIAN_POINT('',(30.9852566047567,-54.0490387249979,39.3548010137695));
#183054=CARTESIAN_POINT('Origin',(30.788965144123,-53.7090519420886,39.555029391245));
#183055=CARTESIAN_POINT('',(31.163405715752,-54.3576020374702,39.92499));
#183056=CARTESIAN_POINT('',(30.9852566047567,-54.0490387249979,39.3548010137695));
#183057=CARTESIAN_POINT('',(29.443310811626,-51.3783102687785,39.92499));
#183058=CARTESIAN_POINT('',(-0.164977839420933,-0.0952499999999948,39.92499));
#183059=CARTESIAN_POINT('',(29.6214601686927,-51.6868740051412,39.3548010137695));
#183060=CARTESIAN_POINT('',(29.443310811626,-51.3783102687785,39.92499));
#183061=CARTESIAN_POINT('',(29.8368674217655,-52.0599703131947,39.116));
#183062=CARTESIAN_POINT('Origin',(29.8177519105517,-52.0268612765597,39.5550297827289));
#183063=CARTESIAN_POINT('',(30.0375573245355,-52.4075754198748,39.116));
#183064=CARTESIAN_POINT('',(30.0744862609074,-52.471538215424,39.116));
#183065=CARTESIAN_POINT('',(30.1005764675357,-52.5167277788842,39.3343017080178));
#183066=CARTESIAN_POINT('',(30.0375573238931,-52.4075754202457,39.116));
#183067=CARTESIAN_POINT('',(30.2655565641143,-52.802481688396,39.5248017080178));
#183068=CARTESIAN_POINT('Origin',(30.2508433300769,-52.7769965925048,39.1947745585576));
#183069=CARTESIAN_POINT('',(30.3411606219517,-52.9334317578288,39.5248017080178));
#183070=CARTESIAN_POINT('',(30.3414249774377,-52.9338896349618,39.5248017080178));
#183071=CARTESIAN_POINT('',(30.5061406831642,-53.2191856060846,39.3343017080178));
#183072=CARTESIAN_POINT('Origin',(30.3558761923092,-52.9589188467264,39.1947728594198));
#183073=CARTESIAN_POINT('',(30.5691598004931,-53.3283379191465,39.116));
#183074=CARTESIAN_POINT('',(30.5061406831642,-53.2191856060846,39.3343017080178));
#183075=CARTESIAN_POINT('',(30.770110263767,-53.6763943313414,39.116));
#183076=CARTESIAN_POINT('Origin',(23.8720415006489,-53.1491210481984,40.10025));
#183077=CARTESIAN_POINT('',(23.9951532569806,-53.9314655730805,40.10025));
#183078=CARTESIAN_POINT('',(25.5480287005717,-57.4192809246789,40.10025));
#183079=CARTESIAN_POINT('',(23.6840886581935,-53.2328030451448,40.10025));
#183080=CARTESIAN_POINT('',(25.5758735661207,-57.406883591798,40.10025));
#183081=CARTESIAN_POINT('Origin',(5.58700050634535E-15,5.8291811068598E-15,
40.10025));
#183082=CARTESIAN_POINT('',(24.0229981225296,-53.9190682401995,40.10025));
#183083=CARTESIAN_POINT('',(23.9942406030432,-53.8544777939069,40.10025));
#183084=CARTESIAN_POINT('Origin',(5.67792519749014E-15,5.18278421698235E-15,
40.10025));
#183085=CARTESIAN_POINT('Origin',(0.174030409680916,0.0774833305059395,
-2.45064239960505E-17));
#183086=CARTESIAN_POINT('',(24.57973006491,-54.7386155880004,39.116));
#183087=CARTESIAN_POINT('',(24.4045020183944,-54.345046951707,39.3548010137695));
#183088=CARTESIAN_POINT('Origin',(24.5641801073104,-54.7036898113989,39.5550297832849));
#183089=CARTESIAN_POINT('',(24.2595822754874,-54.0195518811805,39.92499));
#183090=CARTESIAN_POINT('',(24.4045020183944,-54.345046951707,39.3548010137695));
#183091=CARTESIAN_POINT('',(25.658833530444,-57.1623216544372,39.92499));
#183092=CARTESIAN_POINT('',(25.764498133039,-57.3996482375657,39.92499));
#183093=CARTESIAN_POINT('',(25.5139139879314,-56.8368270312094,39.3548010137695));
#183094=CARTESIAN_POINT('',(25.658833530444,-57.1623216544372,39.92499));
#183095=CARTESIAN_POINT('',(25.3386861202876,-56.4432587981557,39.116));
#183096=CARTESIAN_POINT('Origin',(25.3542361279706,-56.4781846872463,39.5550293907214));
#183097=CARTESIAN_POINT('',(25.1754303533075,-56.0765803402169,39.116));
#183098=CARTESIAN_POINT('',(0.174030409680921,0.0774833305059395,39.116));
#183099=CARTESIAN_POINT('',(25.1241659841934,-55.9614386837454,39.3343017080178));
#183100=CARTESIAN_POINT('',(25.1754303526574,-56.0765803405064,39.116));
#183101=CARTESIAN_POINT('',(24.9899591116494,-55.6600051127008,39.5248017080178));
#183102=CARTESIAN_POINT('Origin',(25.0019278517687,-55.6868886053327,39.1947747614216));
#183103=CARTESIAN_POINT('',(24.928457230274,-55.5218696254673,39.5248017080178));
#183104=CARTESIAN_POINT('',(0.174030409680921,0.0774833305059395,39.5248017080178));
#183105=CARTESIAN_POINT('',(24.7942503289606,-55.2204359898057,39.3343017080178));
#183106=CARTESIAN_POINT('Origin',(24.9164863690992,-55.4949838933603,39.1947728911913));
#183107=CARTESIAN_POINT('',(24.7429859390912,-55.1052942849672,39.116));
#183108=CARTESIAN_POINT('',(24.7942503289606,-55.2204359898057,39.3343017080178));
#183109=CARTESIAN_POINT('',(0.174030409680921,0.0774833305059395,39.116));
#183110=CARTESIAN_POINT('Origin',(-0.174030409680916,-0.0774833305059395,
2.45064239960505E-17));
#183111=CARTESIAN_POINT('',(24.9906253009257,-56.5982254591676,39.116));
#183112=CARTESIAN_POINT('',(25.165853168017,-56.9917936924673,39.3548010137695));
#183113=CARTESIAN_POINT('Origin',(25.006175308492,-56.6331513479958,39.5550293912451));
#183114=CARTESIAN_POINT('',(25.3107727106685,-57.3172883156332,39.92499));
#183115=CARTESIAN_POINT('',(25.165853168017,-56.9917936924673,39.3548010137695));
#183116=CARTESIAN_POINT('',(23.9115214566113,-54.174518541976,39.92499));
#183117=CARTESIAN_POINT('',(-0.174030409680912,-0.0774833305059344,39.92499));
#183118=CARTESIAN_POINT('',(24.0564411996773,-54.5000136124319,39.3548010137695));
#183119=CARTESIAN_POINT('',(23.9115214566113,-54.174518541976,39.92499));
#183120=CARTESIAN_POINT('',(24.2316692455482,-54.8935822490123,39.116));
#183121=CARTESIAN_POINT('Origin',(24.2161192878248,-54.8586564721328,39.5550297827294));
#183122=CARTESIAN_POINT('',(24.3949251204072,-55.2602609456773,39.116));
#183123=CARTESIAN_POINT('',(24.4249658234765,-55.3277334713091,39.116));
#183124=CARTESIAN_POINT('',(24.4461895095988,-55.3754026508175,39.3343017080178));
#183125=CARTESIAN_POINT('',(24.3949251197294,-55.2602609459791,39.116));
#183126=CARTESIAN_POINT('',(24.5803964109122,-55.6768362864792,39.5248017080178));
#183127=CARTESIAN_POINT('Origin',(24.5684276954197,-55.6499528488653,39.1947745585593));
#183128=CARTESIAN_POINT('',(24.6418982922876,-55.8149717737127,39.5248017080178));
#183129=CARTESIAN_POINT('',(24.6421133384135,-55.8154547752195,39.5248017080178));
#183130=CARTESIAN_POINT('',(24.7761051648316,-56.1164053447572,39.3343017080178));
#183131=CARTESIAN_POINT('Origin',(24.6538691229762,-55.8418574376282,39.194772859424));
#183132=CARTESIAN_POINT('',(24.8273695332956,-56.2315470015182,39.116));
#183133=CARTESIAN_POINT('',(24.7761051648316,-56.1164053447572,39.3343017080178));
#183134=CARTESIAN_POINT('',(24.9908373670086,-56.5987017673883,39.116));
#183135=CARTESIAN_POINT('Origin',(18.1856720123407,-55.3532724151365,40.10025));
#183136=CARTESIAN_POINT('',(18.2263320786581,-56.1441998575528,40.10025));
#183137=CARTESIAN_POINT('',(19.4061247292252,-59.7752282754837,40.10025));
#183138=CARTESIAN_POINT('',(17.9900016446781,-55.4168495715592,40.10025));
#183139=CARTESIAN_POINT('',(19.4351129318419,-59.7658094374952,40.10025));
#183140=CARTESIAN_POINT('Origin',(5.60136586593794E-15,5.83469545175774E-15,
40.10025));
#183141=CARTESIAN_POINT('',(18.2553202812748,-56.1347810195642,40.10025));
#183142=CARTESIAN_POINT('',(18.2334718385819,-56.0675384271753,40.10025));
#183143=CARTESIAN_POINT('Origin',(5.67044563844026E-15,5.17991308326517E-15,
40.10025));
#183144=CARTESIAN_POINT('Origin',(0.181176266354227,0.058867737428427,-2.55126814298648E-17));
#183145=CARTESIAN_POINT('',(18.7233363629823,-57.0080331356323,39.116));
#183146=CARTESIAN_POINT('',(18.5902073587821,-56.5983041910846,39.3548010137695));
#183147=CARTESIAN_POINT('Origin',(18.7115223274341,-56.9716732729178,39.5550297832854));
#183148=CARTESIAN_POINT('',(18.4801050009135,-56.2594439785882,39.92499));
#183149=CARTESIAN_POINT('',(18.5902073587821,-56.5983041910846,39.3548010137695));
#183150=CARTESIAN_POINT('',(19.5431821162865,-59.5312589135996,39.92499));
#183151=CARTESIAN_POINT('',(19.6234604941057,-59.778330355405,39.92499));
#183152=CARTESIAN_POINT('',(19.4330799109586,-59.1923991668987,39.3548010137695));
#183153=CARTESIAN_POINT('',(19.5431821162865,-59.5312589135996,39.92499));
#183154=CARTESIAN_POINT('',(19.2999510425005,-58.7826706420789,39.116));
#183155=CARTESIAN_POINT('Origin',(19.3117651160996,-58.8190306219019,39.5550293907203));
#183156=CARTESIAN_POINT('',(19.1759179434156,-58.4009360126567,39.116));
#183157=CARTESIAN_POINT('',(0.181176266354232,0.058867737428427,39.116));
#183158=CARTESIAN_POINT('',(19.1369699862882,-58.281066528503,39.3343017080178));
#183159=CARTESIAN_POINT('',(19.1759179427385,-58.4009360128767,39.116));
#183160=CARTESIAN_POINT('',(19.0350067009929,-57.9672558039532,39.5248017080178));
#183161=CARTESIAN_POINT('Origin',(19.0440997849305,-57.9952431000151,39.1947747614281));
#183162=CARTESIAN_POINT('',(18.9882808235619,-57.8234483402239,39.5248017080178));
#183163=CARTESIAN_POINT('',(0.181176266354233,0.058867737428427,39.5248017080178));
#183164=CARTESIAN_POINT('',(18.8863175164091,-57.5096375484037,39.3343017080178));
#183165=CARTESIAN_POINT('Origin',(18.9791858642777,-57.7954585952468,39.1947728911937));
#183166=CARTESIAN_POINT('',(18.8473695436961,-57.3897680139785,39.116));
#183167=CARTESIAN_POINT('',(18.8863175164091,-57.5096375484037,39.3343017080178));
#183168=CARTESIAN_POINT('',(0.181176266354232,0.058867737428427,39.116));
#183169=CARTESIAN_POINT('Origin',(-0.181176266354227,-0.058867737428427,
2.55126814298648E-17));
#183170=CARTESIAN_POINT('',(18.937598509792,-58.9004061169357,39.116));
#183171=CARTESIAN_POINT('',(19.0707273776751,-59.3101346419424,39.3548010137695));
#183172=CARTESIAN_POINT('Origin',(18.9494125833023,-58.9367660964853,39.5550293912449));
#183173=CARTESIAN_POINT('',(19.1808295831476,-59.6489943885963,39.92499));
#183174=CARTESIAN_POINT('',(19.0707273776751,-59.3101346419424,39.3548010137695));
#183175=CARTESIAN_POINT('',(18.1177524687105,-56.3771794532808,39.92499));
#183176=CARTESIAN_POINT('',(-0.181176266354223,-0.0588677374284217,39.92499));
#183177=CARTESIAN_POINT('',(18.2278548267459,-56.716039665723,39.3548010137695));
#183178=CARTESIAN_POINT('',(18.1177524687105,-56.3771794532808,39.92499));
#183179=CARTESIAN_POINT('',(18.3609838302739,-57.1257686104891,39.116));
#183180=CARTESIAN_POINT('Origin',(18.3491697946315,-57.0894087474849,39.5550297827295));
#183181=CARTESIAN_POINT('',(18.4850170116927,-57.5075034886062,39.116));
#183182=CARTESIAN_POINT('',(18.5078403492309,-57.5777465012099,39.116));
#183183=CARTESIAN_POINT('',(18.5239649837007,-57.6273730232606,39.3343017080178));
#183184=CARTESIAN_POINT('',(18.4850170109876,-57.5075034888353,39.116));
#183185=CARTESIAN_POINT('',(18.6259282908535,-57.9411838150808,39.5248017080178));
#183186=CARTESIAN_POINT('Origin',(18.6168352256581,-57.9131965763138,39.1947745585583));
#183187=CARTESIAN_POINT('',(18.6726541682844,-58.0849912788101,39.5248017080178));
#183188=CARTESIAN_POINT('',(18.6728175489599,-58.0854941128252,39.5248017080178));
#183189=CARTESIAN_POINT('',(18.7746174535798,-58.3988020033599,39.3343017080178));
#183190=CARTESIAN_POINT('Origin',(18.6817491043777,-58.1129809527839,39.1947728594284));
#183191=CARTESIAN_POINT('',(18.8135654100301,-58.5186714877336,39.116));
#183192=CARTESIAN_POINT('',(18.7746174535798,-58.3988020033599,39.3343017080178));
#183193=CARTESIAN_POINT('',(18.9377596263884,-58.9009019828319,39.116));
#183194=CARTESIAN_POINT('Origin',(12.3000564958688,-56.9509617460775,40.10025));
#183195=CARTESIAN_POINT('',(12.2578193919766,-57.7418065394566,40.10025));
#183196=CARTESIAN_POINT('',(13.0516031943527,-61.4762657165316,40.10025));
#183197=CARTESIAN_POINT('',(12.0988124084938,-56.9937374973463,40.10025));
#183198=CARTESIAN_POINT('',(13.0814171332231,-61.4699285681955,40.10025));
#183199=CARTESIAN_POINT('Origin',(5.61622893658571E-15,5.83867799953487E-15,
40.10025));
#183200=CARTESIAN_POINT('',(12.2876333308469,-57.7354693911205,40.10025));
#183201=CARTESIAN_POINT('',(12.2729333410577,-57.6663113765489,40.10025));
#183202=CARTESIAN_POINT('Origin',(5.66270693800216E-15,5.17783950473232E-15,
40.10025));
#183203=CARTESIAN_POINT('Origin',(0.18633711793979,0.0396071771007826,-2.62394165870617E-17));
#183204=CARTESIAN_POINT('',(12.6618058697518,-58.6528587425323,39.116));
#183205=CARTESIAN_POINT('',(12.5722344970959,-58.2314585657881,39.3548010137695));
#183206=CARTESIAN_POINT('Origin',(12.6538571933006,-58.6154631599697,39.5550297832864));
#183207=CARTESIAN_POINT('',(12.4981558287384,-57.8829458347211,39.92499));
#183208=CARTESIAN_POINT('',(12.5722344970959,-58.2314585657881,39.3548010137695));
#183209=CARTESIAN_POINT('',(13.2134115091892,-61.2479592423878,39.92499));
#183210=CARTESIAN_POINT('',(13.2674241155258,-61.5020685764505,39.92499));
#183211=CARTESIAN_POINT('',(13.1393329438488,-60.8994469905094,39.3548010137695));
#183212=CARTESIAN_POINT('',(13.2134115091892,-61.2479592423878,39.92499));
#183213=CARTESIAN_POINT('',(13.0497616623173,-60.4780472453828,39.116));
#183214=CARTESIAN_POINT('Origin',(13.0577103643698,-60.5154429483902,39.5550293907202));
#183215=CARTESIAN_POINT('',(12.9663101637164,-60.0854388089605,39.116));
#183216=CARTESIAN_POINT('',(0.186337117939796,0.0396071771007826,39.116));
#183217=CARTESIAN_POINT('',(12.9401053405448,-59.9621548122772,39.3343017080178));
#183218=CARTESIAN_POINT('',(12.9663101630202,-60.0854388091085,39.116));
#183219=CARTESIAN_POINT('',(12.871502773589,-59.6394051101894,39.5248017080178));
#183220=CARTESIAN_POINT('Origin',(12.8776205756134,-59.6681895750072,39.1947747614316));
#183221=CARTESIAN_POINT('',(12.8400648385937,-59.4915012546305,39.5248017080178));
#183222=CARTESIAN_POINT('',(0.186337117939796,0.0396071771007826,39.5248017080178));
#183223=CARTESIAN_POINT('',(12.7714622569318,-59.1687514833561,39.3343017080178));
#183224=CARTESIAN_POINT('Origin',(12.833945427478,-59.4627141582885,39.1947728911924));
#183225=CARTESIAN_POINT('',(12.7452574235146,-59.0454674350475,39.116));
#183226=CARTESIAN_POINT('',(12.7714622569318,-59.1687514833561,39.3343017080178));
#183227=CARTESIAN_POINT('',(0.186337117939796,0.0396071771007826,39.116));
#183228=CARTESIAN_POINT('Origin',(-0.18633711793979,-0.0396071771007826,
2.62394165870617E-17));
#183229=CARTESIAN_POINT('',(12.6770874264377,-60.5572615995844,39.116));
#183230=CARTESIAN_POINT('',(12.7666587073772,-60.9786613448368,39.3548010137695));
#183231=CARTESIAN_POINT('Origin',(12.6850361284303,-60.5946573023097,39.5550293912463));
#183232=CARTESIAN_POINT('',(12.840737272867,-61.3271735966835,39.92499));
#183233=CARTESIAN_POINT('',(12.7666587073772,-60.9786613448368,39.3548010137695));
#183234=CARTESIAN_POINT('',(12.125481593379,-57.9621601888121,39.92499));
#183235=CARTESIAN_POINT('',(-0.186337117939786,-0.0396071771007771,39.92499));
#183236=CARTESIAN_POINT('',(12.1995602619083,-58.3106729198425,39.3548010137695));
#183237=CARTESIAN_POINT('',(12.125481593379,-57.9621601888121,39.92499));
#183238=CARTESIAN_POINT('',(12.2891316338722,-58.7320730967338,39.116));
#183239=CARTESIAN_POINT('Origin',(12.281182957358,-58.6946775138747,39.5550297827326));
#183240=CARTESIAN_POINT('',(12.3725831883602,-59.1246817890949,39.116));
#183241=CARTESIAN_POINT('',(12.3879391031045,-59.1969256915254,39.116));
#183242=CARTESIAN_POINT('',(12.3987880210522,-59.2479658375577,39.3343017080178));
#183243=CARTESIAN_POINT('',(12.372583187635,-59.1246817892491,39.116));
#183244=CARTESIAN_POINT('',(12.4673906027141,-59.5707156088321,39.5248017080178));
#183245=CARTESIAN_POINT('Origin',(12.4612728133404,-59.5419312029551,39.1947745585607));
#183246=CARTESIAN_POINT('',(12.4988285377094,-59.7186194643909,39.5248017080178));
#183247=CARTESIAN_POINT('',(12.4989384629016,-59.7191366217596,39.5248017080178));
#183248=CARTESIAN_POINT('',(12.5674311046652,-60.0413691664788,39.3343017080178));
#183249=CARTESIAN_POINT('Origin',(12.5049479331829,-59.7474064876936,39.1947728594244));
#183250=CARTESIAN_POINT('',(12.5936359271406,-60.1646531633101,39.116));
#183251=CARTESIAN_POINT('',(12.5674311046652,-60.0413691664788,39.3343017080178));
#183252=CARTESIAN_POINT('',(12.6771958283204,-60.5577715903455,39.116));
#183253=CARTESIAN_POINT('Origin',(6.27967898647588,-57.9246844223735,40.10025));
#183254=CARTESIAN_POINT('',(6.15500747092297,-58.7067819056643,40.10025));
#183255=CARTESIAN_POINT('',(6.55408556365926,-62.5037563256535,40.10025));
#183256=CARTESIAN_POINT('',(6.07506605172282,-57.9461901084062,40.10025));
#183257=CARTESIAN_POINT('',(6.58439859103008,-62.5005702980931,40.10025));
#183258=CARTESIAN_POINT('Origin',(5.63142687537637E-15,5.84108511656431E-15,
40.10025));
#183259=CARTESIAN_POINT('',(6.1853204982938,-58.7035958781039,40.10025));
#183260=CARTESIAN_POINT('',(6.1779300175725,-58.6332801510296,40.10025));
#183261=CARTESIAN_POINT('Origin',(5.65479388299727E-15,5.17658619994411E-15,
40.10025));
#183262=CARTESIAN_POINT('Origin',(0.189456421067656,0.0199126722524874,
-2.66786672051798E-17));
#183263=CARTESIAN_POINT('',(6.46154998175899,-59.6550713551493,39.116));
#183264=CARTESIAN_POINT('',(6.41651760335031,-59.2266168947286,39.3548010137695));
#183265=CARTESIAN_POINT('Origin',(6.45755375176722,-59.6170497665647,39.5550297832833));
#183266=CARTESIAN_POINT('',(6.37927424589724,-58.8722700235036,39.92499));
#183267=CARTESIAN_POINT('',(6.41651760335031,-59.2266168947286,39.3548010137695));
#183268=CARTESIAN_POINT('',(6.73887200051313,-62.2936141127569,39.92499));
#183269=CARTESIAN_POINT('',(6.76602706194927,-62.5519772640372,39.92499));
#183270=CARTESIAN_POINT('',(6.70162869542395,-61.9392677288636,39.3548010137695));
#183271=CARTESIAN_POINT('',(6.73887200051313,-62.2936141127569,39.92499));
#183272=CARTESIAN_POINT('',(6.65659636252364,-61.5108137072212,39.116));
#183273=CARTESIAN_POINT('Origin',(6.66059260538629,-61.5488354182641,39.5550293907226));
#183274=CARTESIAN_POINT('',(6.61464077648889,-61.1116329639869,39.116));
#183275=CARTESIAN_POINT('',(0.189456421067662,0.0199126722524874,39.116));
#183276=CARTESIAN_POINT('',(6.60146619279927,-60.9862851800404,39.3343017080178));
#183277=CARTESIAN_POINT('',(6.61464077578103,-61.1116329640613,39.116));
#183278=CARTESIAN_POINT('',(6.56697596826259,-60.6581326136904,39.5248017080178));
#183279=CARTESIAN_POINT('Origin',(6.57005146045377,-60.68739887864,39.1947747614269));
#183280=CARTESIAN_POINT('',(6.55117041629749,-60.5077528318944,39.5248017080178));
#183281=CARTESIAN_POINT('',(0.189456421067662,0.0199126722524874,39.5248017080178));
#183282=CARTESIAN_POINT('',(6.51668018436727,-60.1796001951995,39.3343017080178));
#183283=CARTESIAN_POINT('Origin',(6.54809359889865,-60.478483781637,39.1947728911937));
#183284=CARTESIAN_POINT('',(6.50350559588446,-60.0542523588397,39.116));
#183285=CARTESIAN_POINT('',(6.51668018436727,-60.1796001951995,39.3343017080178));
#183286=CARTESIAN_POINT('',(0.189456421067662,0.0199126722524874,39.116));
#183287=CARTESIAN_POINT('Origin',(-0.189456421067656,-0.0199126722524874,
2.66786672051798E-17));
#183288=CARTESIAN_POINT('',(6.27768352038833,-61.5506390517262,39.116));
#183289=CARTESIAN_POINT('',(6.32271585268621,-61.9790930734319,39.3548010137695));
#183290=CARTESIAN_POINT('Origin',(6.2816797632211,-61.5886607624848,39.555029391244));
#183291=CARTESIAN_POINT('',(6.35995915792839,-62.3334394573092,39.92499));
#183292=CARTESIAN_POINT('',(6.32271585268621,-61.9790930734319,39.3548010137695));
#183293=CARTESIAN_POINT('',(6.00036140429027,-58.912095367953,39.92499));
#183294=CARTESIAN_POINT('',(-0.189456421067651,-0.0199126722524818,39.92499));
#183295=CARTESIAN_POINT('',(6.03760476191764,-59.2664422391598,39.3548010137695));
#183296=CARTESIAN_POINT('',(6.00036140429027,-58.912095367953,39.92499));
#183297=CARTESIAN_POINT('',(6.08263713962368,-59.6948966996543,39.116));
#183298=CARTESIAN_POINT('Origin',(6.07864090960028,-59.6568751107687,39.5550297827311));
#183299=CARTESIAN_POINT('',(6.12459275448592,-60.0940777032673,39.116));
#183300=CARTESIAN_POINT('',(6.13231300382157,-60.1675309762115,39.116));
#183301=CARTESIAN_POINT('',(6.13776734223196,-60.2194255397045,39.3343017080178));
#183302=CARTESIAN_POINT('',(6.12459275374915,-60.0940777033447,39.116));
#183303=CARTESIAN_POINT('',(6.17225757416218,-60.5475781763994,39.5248017080178));
#183304=CARTESIAN_POINT('Origin',(6.16918208839128,-60.5183119713882,39.194774558559));
#183305=CARTESIAN_POINT('',(6.18806312612727,-60.6979579581954,39.5248017080178));
#183306=CARTESIAN_POINT('',(6.18811839147268,-60.6984837728333,39.5248017080178));
#183307=CARTESIAN_POINT('',(6.22255335066396,-61.0261105245454,39.3343017080178));
#183308=CARTESIAN_POINT('Origin',(6.19113993560417,-60.7272269341768,39.1947728594245));
#183309=CARTESIAN_POINT('',(6.23572793364572,-61.1514583085662,39.116));
#183310=CARTESIAN_POINT('',(6.22255335066396,-61.0261105245454,39.3343017080178));
#183311=CARTESIAN_POINT('',(6.2777380198836,-61.5511575797868,39.116));
#183312=CARTESIAN_POINT('Origin',(0.190499999999802,-58.2637721346185,40.10025));
#183313=CARTESIAN_POINT('',(-0.0152400000002005,-59.0285534841296,40.10025));
#183314=CARTESIAN_POINT('',(-0.0152400000002138,-62.8464427007196,40.10025));
#183315=CARTESIAN_POINT('',(-0.0152400000001978,-58.2637721346185,40.10025));
#183316=CARTESIAN_POINT('',(0.0152399999997862,-62.8464427007196,40.10025));
#183317=CARTESIAN_POINT('Origin',(-4.80914138193527E-17,1.47005845636695E-16,
40.10025));
#183318=CARTESIAN_POINT('',(0.0152399999997995,-59.0285534841296,40.10025));
#183319=CARTESIAN_POINT('',(0.0152399999997998,-58.9578504383728,40.10025));
#183320=CARTESIAN_POINT('Origin',(3.94085276091011E-16,-7.6540994051039E-17,
40.10025));
#183321=CARTESIAN_POINT('Origin',(0.1905,-6.65127195049617E-16,-2.68256207625279E-17));
#183322=CARTESIAN_POINT('',(0.190499999999796,-60.0036905223731,39.116));
#183323=CARTESIAN_POINT('',(0.190499999999797,-59.5728760150042,39.3548010137695));
#183324=CARTESIAN_POINT('Origin',(0.190499999999796,-59.9654595002498,39.5550297832847));
#183325=CARTESIAN_POINT('',(0.190499999468434,-59.2165773020941,39.92499));
#183326=CARTESIAN_POINT('',(0.190499999999798,-59.5728760150042,39.3548010137695));
#183327=CARTESIAN_POINT('',(0.190499999999788,-62.6567671111299,39.92499));
#183328=CARTESIAN_POINT('',(0.190499999999786,-62.9165533988763,39.92499));
#183329=CARTESIAN_POINT('',(0.19050000060545,-62.3004688883555,39.3548010137695));
#183330=CARTESIAN_POINT('',(0.190499999999787,-62.6567671111299,39.92499));
#183331=CARTESIAN_POINT('',(0.19049999999979,-61.8696548221181,39.116));
#183332=CARTESIAN_POINT('Origin',(0.190499999999789,-61.9078859673761,39.5550293907201));
#183333=CARTESIAN_POINT('',(0.190500000711669,-61.4682752798284,39.116));
#183334=CARTESIAN_POINT('',(0.190500000000006,-6.65127195049617E-16,39.116));
#183335=CARTESIAN_POINT('',(0.190499999999791,-61.3422370451705,39.3343017080178));
#183336=CARTESIAN_POINT('',(0.190499999999791,-61.4682752798284,39.116));
#183337=CARTESIAN_POINT('',(0.190499999999793,-61.0122769227456,39.5248017080178));
#183338=CARTESIAN_POINT('Origin',(0.19049948662219,-61.0417043405089,39.1947747614312));
#183339=CARTESIAN_POINT('',(0.190499999999793,-60.8610688070707,39.5248017080178));
#183340=CARTESIAN_POINT('',(0.190500000000006,-6.65127195049617E-16,39.5248017080178));
#183341=CARTESIAN_POINT('',(0.190499999999794,-60.5311086139135,39.3343017080178));
#183342=CARTESIAN_POINT('Origin',(0.190499486573297,-60.8316384807416,39.1947728911891));
#183343=CARTESIAN_POINT('',(0.190499999999795,-60.4050703266283,39.116));
#183344=CARTESIAN_POINT('',(0.190499999999794,-60.5311086139135,39.3343017080178));
#183345=CARTESIAN_POINT('',(0.190500000000006,-6.65127195049617E-16,39.116));
#183346=CARTESIAN_POINT('Origin',(-0.1905,6.65127195049617E-16,2.68256207625279E-17));
#183347=CARTESIAN_POINT('',(-0.190500000000211,-61.8696548221181,39.116));
#183348=CARTESIAN_POINT('',(-0.190500000000213,-62.3004688883554,39.3548010137695));
#183349=CARTESIAN_POINT('Origin',(-0.190500000000211,-61.9078859670887,
39.5550293912444));
#183350=CARTESIAN_POINT('',(-0.190500000452744,-62.6567671111299,39.92499));
#183351=CARTESIAN_POINT('',(-0.190500000000212,-62.3004688883554,39.3548010137695));
#183352=CARTESIAN_POINT('',(-0.190500000000201,-59.2165773020941,39.92499));
#183353=CARTESIAN_POINT('',(-0.190499999999994,6.28724079446023E-15,39.92499));
#183354=CARTESIAN_POINT('',(-0.190499999294014,-59.5728760150042,39.3548010137695));
#183355=CARTESIAN_POINT('',(-0.190500000000201,-59.2165773020941,39.92499));
#183356=CARTESIAN_POINT('',(-0.190500000000204,-60.0036905223731,39.116));
#183357=CARTESIAN_POINT('Origin',(-0.190500000000204,-59.9654594999465,
39.5550297827309));
#183358=CARTESIAN_POINT('',(-0.190499999258436,-60.4050703266283,39.116));
#183359=CARTESIAN_POINT('',(-0.190500000000206,-60.4789282006569,39.116));
#183360=CARTESIAN_POINT('',(-0.190500000000206,-60.5311086139135,39.3343017080178));
#183361=CARTESIAN_POINT('',(-0.190500000000205,-60.4050703266283,39.116));
#183362=CARTESIAN_POINT('',(-0.190500000000207,-60.8610688070707,39.5248017080178));
#183363=CARTESIAN_POINT('Origin',(-0.190499486502767,-60.8316414495905,
39.1947745585607));
#183364=CARTESIAN_POINT('',(-0.190500000000207,-61.0122769227456,39.5248017080178));
#183365=CARTESIAN_POINT('',(-0.190500000000207,-61.0128056337175,39.5248017080178));
#183366=CARTESIAN_POINT('',(-0.190500000000209,-61.3422370451705,39.3343017080178));
#183367=CARTESIAN_POINT('Origin',(-0.190499486688308,-61.0417071743813,
39.1947728594259));
#183368=CARTESIAN_POINT('',(-0.190500000000209,-61.4682752798284,39.116));
#183369=CARTESIAN_POINT('',(-0.190500000000209,-61.3422370451705,39.3343017080178));
#183370=CARTESIAN_POINT('',(-0.190500000000211,-61.8701762063762,39.116));
#183371=CARTESIAN_POINT('Origin',(-5.90076614434095,-57.9645097668785,40.10025));
#183372=CARTESIAN_POINT('',(-6.18532049829418,-58.7035958781039,40.10025));
#183373=CARTESIAN_POINT('',(-6.58439859103049,-62.5005702980931,40.10025));
#183374=CARTESIAN_POINT('',(-6.10537907909402,-57.9430040808458,40.10025));
#183375=CARTESIAN_POINT('',(-6.55408556365967,-62.5037563256534,40.10025));
#183376=CARTESIAN_POINT('Origin',(-3.27251186835855E-17,1.46200532232821E-16,
40.10025));
#183377=CARTESIAN_POINT('',(-6.15500747092336,-58.7067819056643,40.10025));
#183378=CARTESIAN_POINT('',(-6.14761699020206,-58.6364661785899,40.10025));
#183379=CARTESIAN_POINT('Origin',(3.86084563605877E-16,-7.61216944770112E-17,
40.10025));
#183380=CARTESIAN_POINT('Origin',(0.189456421067656,-0.0199126722524887,
-2.66786672051798E-17));
#183381=CARTESIAN_POINT('',(-6.08263713962407,-59.6948966996542,39.116));
#183382=CARTESIAN_POINT('',(-6.03760476121539,-59.2664422392336,39.3548010137695));
#183383=CARTESIAN_POINT('Origin',(-6.07864090963236,-59.6568751110701,39.5550297832838));
#183384=CARTESIAN_POINT('',(-6.0003614048196,-58.9120953678974,39.92499));
#183385=CARTESIAN_POINT('',(-6.03760476121539,-59.2664422392336,39.3548010137695));
#183386=CARTESIAN_POINT('',(-6.35995915837823,-62.3334394572619,39.92499));
#183387=CARTESIAN_POINT('',(-6.38711421981437,-62.5918026085421,39.92499));
#183388=CARTESIAN_POINT('',(-6.32271585208497,-61.9790930734951,39.3548010137695));
#183389=CARTESIAN_POINT('',(-6.35995915837823,-62.3334394572619,39.92499));
#183390=CARTESIAN_POINT('',(-6.27768352038873,-61.5506390517262,39.116));
#183391=CARTESIAN_POINT('Origin',(-6.28167976325141,-61.5886607627694,39.5550293907224));
#183392=CARTESIAN_POINT('',(-6.23572793293811,-61.1514583086406,39.116));
#183393=CARTESIAN_POINT('',(0.189456421067662,-0.0199126722524887,39.116));
#183394=CARTESIAN_POINT('',(-6.22255335066436,-61.0261105245454,39.3343017080178));
#183395=CARTESIAN_POINT('',(-6.23572793364612,-61.1514583085662,39.116));
#183396=CARTESIAN_POINT('',(-6.18806312612767,-60.6979579581954,39.5248017080178));
#183397=CARTESIAN_POINT('Origin',(-6.19113963945004,-60.7272241158261,39.1947747614376));
#183398=CARTESIAN_POINT('',(-6.17225757416258,-60.5475781763993,39.5248017080178));
#183399=CARTESIAN_POINT('',(0.189456421067662,-0.0199126722524887,39.5248017080178));
#183400=CARTESIAN_POINT('',(-6.13776734223235,-60.2194255397045,39.3343017080178));
#183401=CARTESIAN_POINT('Origin',(-6.16918177799152,-60.5183090188066,39.1947728911941));
#183402=CARTESIAN_POINT('',(-6.12459275374954,-60.0940777033447,39.116));
#183403=CARTESIAN_POINT('',(-6.13776734223235,-60.2194255397045,39.3343017080178));
#183404=CARTESIAN_POINT('',(0.189456421067662,-0.0199126722524887,39.116));
#183405=CARTESIAN_POINT('Origin',(-0.189456421067656,0.0199126722524887,
2.66786672051798E-17));
#183406=CARTESIAN_POINT('',(-6.65659636252404,-61.5108137072212,39.116));
#183407=CARTESIAN_POINT('',(-6.70162869482193,-61.9392677289269,39.3548010137695));
#183408=CARTESIAN_POINT('Origin',(-6.6605926053566,-61.5488354179777,39.5550293912481));
#183409=CARTESIAN_POINT('',(-6.73887200096381,-62.2936141127096,39.92499));
#183410=CARTESIAN_POINT('',(-6.70162869482193,-61.9392677289269,39.3548010137695));
#183411=CARTESIAN_POINT('',(-6.37927424642597,-58.872270023448,39.92499));
#183412=CARTESIAN_POINT('',(-0.18945642106765,0.0199126722524943,39.92499));
#183413=CARTESIAN_POINT('',(-6.41651760264748,-59.2266168948025,39.3548010137695));
#183414=CARTESIAN_POINT('',(-6.37927424642597,-58.872270023448,39.92499));
#183415=CARTESIAN_POINT('',(-6.46154998175939,-59.6550713551492,39.116));
#183416=CARTESIAN_POINT('Origin',(-6.45755375173582,-59.6170497662621,39.5550297827283));
#183417=CARTESIAN_POINT('',(-6.5035055951475,-60.0542523589172,39.116));
#183418=CARTESIAN_POINT('',(-6.51122584595728,-60.1277056317065,39.116));
#183419=CARTESIAN_POINT('',(-6.51668018436767,-60.1796001951995,39.3343017080178));
#183420=CARTESIAN_POINT('',(-6.50350559588486,-60.0542523588397,39.116));
#183421=CARTESIAN_POINT('',(-6.55117041629789,-60.5077528318944,39.5248017080178));
#183422=CARTESIAN_POINT('Origin',(-6.54809390915818,-60.4784867342341,39.1947745585578));
#183423=CARTESIAN_POINT('',(-6.56697596826298,-60.6581326136904,39.5248017080178));
#183424=CARTESIAN_POINT('',(-6.5670312336084,-60.6586584283283,39.5248017080178));
#183425=CARTESIAN_POINT('',(-6.60146619279967,-60.9862851800404,39.3343017080178));
#183426=CARTESIAN_POINT('Origin',(-6.57005175673992,-60.687401696982,39.1947728594215));
#183427=CARTESIAN_POINT('',(-6.61464077578143,-61.1116329640612,39.116));
#183428=CARTESIAN_POINT('',(-6.60146619279967,-60.9862851800404,39.3343017080178));
#183429=CARTESIAN_POINT('',(-6.65665086201932,-61.5113322352818,39.116));
#183430=CARTESIAN_POINT('Origin',(-11.9273822599896,-57.030176100279,40.10025));
#183431=CARTESIAN_POINT('',(-12.2876333308473,-57.7354693911204,40.10025));
#183432=CARTESIAN_POINT('',(-13.0814171332235,-61.4699285681954,40.10025));
#183433=CARTESIAN_POINT('',(-12.1286263473646,-56.9874003490101,40.10025));
#183434=CARTESIAN_POINT('',(-13.0516031943531,-61.4762657165315,40.10025));
#183435=CARTESIAN_POINT('Origin',(-1.75271798929331E-17,1.43793415203377E-16,
40.10025));
#183436=CARTESIAN_POINT('',(-12.257819391977,-57.7418065394565,40.10025));
#183437=CARTESIAN_POINT('',(-12.2431194021877,-57.672648524885,40.10025));
#183438=CARTESIAN_POINT('Origin',(3.78171508600985E-16,-7.48683896888047E-17,
40.10025));
#183439=CARTESIAN_POINT('Origin',(0.18633711793979,-0.0396071771007839,
-2.62394165870617E-17));
#183440=CARTESIAN_POINT('',(-12.2891316338726,-58.7320730967337,39.116));
#183441=CARTESIAN_POINT('',(-12.1995602612167,-58.3106729199896,39.3548010137695));
#183442=CARTESIAN_POINT('Origin',(-12.281182957421,-58.6946775141692,39.5550297832827));
#183443=CARTESIAN_POINT('',(-12.1254815938996,-57.9621601887015,39.92499));
#183444=CARTESIAN_POINT('',(-12.1995602612167,-58.3106729199896,39.3548010137695));
#183445=CARTESIAN_POINT('',(-12.84073727331,-61.3271735965893,39.92499));
#183446=CARTESIAN_POINT('',(-12.8947498796467,-61.581282930652,39.92499));
#183447=CARTESIAN_POINT('',(-12.7666587067853,-60.9786613449626,39.3548010137695));
#183448=CARTESIAN_POINT('',(-12.84073727331,-61.3271735965893,39.92499));
#183449=CARTESIAN_POINT('',(-12.6770874264381,-60.5572615995843,39.116));
#183450=CARTESIAN_POINT('Origin',(-12.6850361284907,-60.5946573025919,39.5550293907204));
#183451=CARTESIAN_POINT('',(-12.5936359264447,-60.164653163458,39.116));
#183452=CARTESIAN_POINT('',(0.186337117939795,-0.0396071771007839,39.116));
#183453=CARTESIAN_POINT('',(-12.5674311046656,-60.0413691664787,39.3343017080178));
#183454=CARTESIAN_POINT('',(-12.593635927141,-60.16465316331,39.116));
#183455=CARTESIAN_POINT('',(-12.4988285377098,-59.7186194643909,39.5248017080178));
#183456=CARTESIAN_POINT('Origin',(-12.5049473440529,-59.7474037157365,39.1947747614353));
#183457=CARTESIAN_POINT('',(-12.4673906027145,-59.570715608832,39.5248017080178));
#183458=CARTESIAN_POINT('',(0.186337117939795,-0.0396071771007839,39.5248017080178));
#183459=CARTESIAN_POINT('',(-12.3987880210526,-59.2479658375576,39.3343017080178));
#183460=CARTESIAN_POINT('Origin',(-12.4612721960127,-59.5419282989955,39.1947728911913));
#183461=CARTESIAN_POINT('',(-12.3725831876354,-59.124681789249,39.116));
#183462=CARTESIAN_POINT('',(-12.3987880210526,-59.2479658375576,39.3343017080178));
#183463=CARTESIAN_POINT('',(0.186337117939795,-0.0396071771007839,39.116));
#183464=CARTESIAN_POINT('Origin',(-0.18633711793979,0.0396071771007839,
2.62394165870617E-17));
#183465=CARTESIAN_POINT('',(-13.0497616623177,-60.4780472453827,39.116));
#183466=CARTESIAN_POINT('',(-13.1393329432572,-60.8994469906352,39.3548010137695));
#183467=CARTESIAN_POINT('Origin',(-13.0577103643103,-60.5154429481083,39.5550293912458));
#183468=CARTESIAN_POINT('',(-13.2134115096323,-61.2479592422936,39.92499));
#183469=CARTESIAN_POINT('',(-13.1393329432572,-60.8994469906352,39.3548010137695));
#183470=CARTESIAN_POINT('',(-12.4981558292589,-57.8829458346105,39.92499));
#183471=CARTESIAN_POINT('',(-0.186337117939783,0.0396071771007894,39.92499));
#183472=CARTESIAN_POINT('',(-12.5722344964058,-58.2314585659347,39.3548010137695));
#183473=CARTESIAN_POINT('',(-12.4981558292589,-57.8829458346105,39.92499));
#183474=CARTESIAN_POINT('',(-12.6618058697522,-58.6528587425322,39.116));
#183475=CARTESIAN_POINT('Origin',(-12.6538571932377,-58.6154631596715,39.5550297827294));
#183476=CARTESIAN_POINT('',(-12.7452574227898,-59.0454674352015,39.116));
#183477=CARTESIAN_POINT('',(-12.7606133389844,-59.1177113373238,39.116));
#183478=CARTESIAN_POINT('',(-12.7714622569322,-59.168751483356,39.3343017080178));
#183479=CARTESIAN_POINT('',(-12.745257423515,-59.0454674350474,39.116));
#183480=CARTESIAN_POINT('',(-12.8400648385941,-59.4915012546304,39.5248017080178));
#183481=CARTESIAN_POINT('Origin',(-12.8339460446676,-59.4627170622764,39.1947745585626));
#183482=CARTESIAN_POINT('',(-12.8715027735894,-59.6394051101893,39.5248017080178));
#183483=CARTESIAN_POINT('',(-12.8716126987815,-59.639922267558,39.5248017080178));
#183484=CARTESIAN_POINT('',(-12.9401053405452,-59.9621548122771,39.3343017080178));
#183485=CARTESIAN_POINT('Origin',(-12.8776211648735,-59.6681923469399,39.1947728594259));
#183486=CARTESIAN_POINT('',(-12.9663101630206,-60.0854388091084,39.116));
#183487=CARTESIAN_POINT('',(-12.9401053405452,-59.9621548122771,39.3343017080178));
#183488=CARTESIAN_POINT('',(-13.0498700642004,-60.4785572361438,39.116));
#183489=CARTESIAN_POINT('Origin',(-17.8233194796326,-55.4710078899933,40.10025));
#183490=CARTESIAN_POINT('',(-18.2553202812751,-56.1347810195641,40.10025));
#183491=CARTESIAN_POINT('',(-19.4351129318423,-59.765809437495,40.10025));
#183492=CARTESIAN_POINT('',(-18.0189898472952,-55.4074307335706,40.10025));
#183493=CARTESIAN_POINT('',(-19.4061247292256,-59.7752282754836,40.10025));
#183494=CARTESIAN_POINT('Origin',(-2.66410924515271E-18,1.39810867426259E-16,
40.10025));
#183495=CARTESIAN_POINT('',(-18.2263320786585,-56.1441998575527,40.10025));
#183496=CARTESIAN_POINT('',(-18.2044836359655,-56.0769572651638,40.10025));
#183497=CARTESIAN_POINT('Origin',(3.70432808162889E-16,-7.27948111559479E-17,
40.10025));
#183498=CARTESIAN_POINT('Origin',(0.181176266354227,-0.0588677374284282,
-2.55126814298647E-17));
#183499=CARTESIAN_POINT('',(-18.3609838302743,-57.125768610489,39.116));
#183500=CARTESIAN_POINT('',(-18.227854826074,-56.7160396659413,39.3548010137695));
#183501=CARTESIAN_POINT('Origin',(-18.3491697947259,-57.0894087477742,39.5550297832844));
#183502=CARTESIAN_POINT('',(-18.1177524692165,-56.3771794531163,39.92499));
#183503=CARTESIAN_POINT('',(-18.227854826074,-56.7160396659413,39.3548010137695));
#183504=CARTESIAN_POINT('',(-19.1808295835784,-59.6489943884563,39.92499));
#183505=CARTESIAN_POINT('',(-19.2611079613977,-59.8960658302617,39.92499));
#183506=CARTESIAN_POINT('',(-19.0707273770997,-59.3101346421294,39.3548010137695));
#183507=CARTESIAN_POINT('',(-19.1808295835784,-59.6489943884563,39.92499));
#183508=CARTESIAN_POINT('',(-18.9375985097924,-58.9004061169356,39.116));
#183509=CARTESIAN_POINT('Origin',(-18.9494125833914,-58.936766096758,39.5550293907216));
#183510=CARTESIAN_POINT('',(-18.8135654093534,-58.5186714879534,39.116));
#183511=CARTESIAN_POINT('',(0.181176266354232,-0.0588677374284282,39.116));
#183512=CARTESIAN_POINT('',(-18.7746174535802,-58.3988020033598,39.3343017080178));
#183513=CARTESIAN_POINT('',(-18.8135654100305,-58.5186714877335,39.116));
#183514=CARTESIAN_POINT('',(-18.6726541682848,-58.08499127881,39.5248017080178));
#183515=CARTESIAN_POINT('Origin',(-18.6817482287253,-58.1129782575888,39.1947747614318));
#183516=CARTESIAN_POINT('',(-18.6259282908539,-57.9411838150807,39.5248017080178));
#183517=CARTESIAN_POINT('',(0.181176266354232,-0.0588677374284282,39.5248017080178));
#183518=CARTESIAN_POINT('',(-18.523964983701,-57.6273730232604,39.3343017080178));
#183519=CARTESIAN_POINT('Origin',(-18.6168343081655,-57.9131937527902,39.1947728911903));
#183520=CARTESIAN_POINT('',(-18.485017010988,-57.5075034888352,39.116));
#183521=CARTESIAN_POINT('',(-18.523964983701,-57.6273730232604,39.3343017080178));
#183522=CARTESIAN_POINT('',(0.181176266354232,-0.0588677374284282,39.116));
#183523=CARTESIAN_POINT('Origin',(-0.181176266354227,0.0588677374284282,
2.55126814298647E-17));
#183524=CARTESIAN_POINT('',(-19.2999510425009,-58.7826706420788,39.116));
#183525=CARTESIAN_POINT('',(-19.433079910384,-59.1923991670854,39.3548010137695));
#183526=CARTESIAN_POINT('Origin',(-19.311765116011,-58.8190306216278,39.555029391246));
#183527=CARTESIAN_POINT('',(-19.5431821167168,-59.5312589134598,39.92499));
#183528=CARTESIAN_POINT('',(-19.433079910384,-59.1923991670854,39.3548010137695));
#183529=CARTESIAN_POINT('',(-18.4801050014193,-56.2594439784238,39.92499));
#183530=CARTESIAN_POINT('',(-0.181176266354219,0.0588677374284336,39.92499));
#183531=CARTESIAN_POINT('',(-18.5902073581106,-56.5983041913028,39.3548010137695));
#183532=CARTESIAN_POINT('',(-18.4801050014193,-56.2594439784238,39.92499));
#183533=CARTESIAN_POINT('',(-18.7233363629827,-57.0080331356321,39.116));
#183534=CARTESIAN_POINT('Origin',(-18.7115223273411,-56.9716732726305,39.555029782734));
#183535=CARTESIAN_POINT('',(-18.8473695429908,-57.3897680142076,39.116));
#183536=CARTESIAN_POINT('',(-18.8701928819397,-57.4600110263529,39.116));
#183537=CARTESIAN_POINT('',(-18.8863175164095,-57.5096375484036,39.3343017080178));
#183538=CARTESIAN_POINT('',(-18.8473695436964,-57.3897680139783,39.116));
#183539=CARTESIAN_POINT('',(-18.9882808235623,-57.8234483402238,39.5248017080178));
#183540=CARTESIAN_POINT('Origin',(-18.9791867816365,-57.7954614188148,39.19477455856));
#183541=CARTESIAN_POINT('',(-19.0350067009933,-57.9672558039531,39.5248017080178));
#183542=CARTESIAN_POINT('',(-19.0351700816687,-57.9677586379682,39.5248017080178));
#183543=CARTESIAN_POINT('',(-19.1369699862886,-58.2810665285029,39.3343017080178));
#183544=CARTESIAN_POINT('Origin',(-19.0441006607084,-57.9952457951681,39.1947728594225));
#183545=CARTESIAN_POINT('',(-19.1759179427389,-58.4009360128766,39.116));
#183546=CARTESIAN_POINT('',(-19.1369699862886,-58.2810665285029,39.3343017080178));
#183547=CARTESIAN_POINT('',(-19.3001121590972,-58.7831665079749,39.116));
#183548=CARTESIAN_POINT('Origin',(-23.5239806812874,-53.3040877092101,40.10025));
#183549=CARTESIAN_POINT('',(-24.0229981225299,-53.9190682401994,40.10025));
#183550=CARTESIAN_POINT('',(-25.5758735661211,-57.4068835917978,40.10025));
#183551=CARTESIAN_POINT('',(-23.7119335237428,-53.2204057122637,40.10025));
#183552=CARTESIAN_POINT('',(-25.5480287005721,-57.4192809246788,40.10025));
#183553=CARTESIAN_POINT('Origin',(1.17012503474363E-17,1.34296522528312E-16,
40.10025));
#183554=CARTESIAN_POINT('',(-23.995153256981,-53.9314655730803,40.10025));
#183555=CARTESIAN_POINT('',(-23.9663957374946,-53.8668751267877,40.10025));
#183556=CARTESIAN_POINT('Origin',(3.62953249113008E-16,-6.99236774387749E-17,
40.10025));
#183557=CARTESIAN_POINT('Origin',(0.174030409680915,-0.0774833305059407,
-2.45064239960504E-17));
#183558=CARTESIAN_POINT('',(-24.2316692455485,-54.8935822490121,39.116));
#183559=CARTESIAN_POINT('',(-24.056441199033,-54.5000136127188,39.3548010137695));
#183560=CARTESIAN_POINT('Origin',(-24.2161192879494,-54.8586564724117,39.5550297832871));
#183561=CARTESIAN_POINT('',(-23.9115214570974,-54.1745185417596,39.92499));
#183562=CARTESIAN_POINT('',(-24.056441199033,-54.5000136127187,39.3548010137695));
#183563=CARTESIAN_POINT('',(-25.3107727110825,-57.3172883154489,39.92499));
#183564=CARTESIAN_POINT('',(-25.4164373136776,-57.5546148985774,39.92499));
#183565=CARTESIAN_POINT('',(-25.1658531674643,-56.9917936927134,39.3548010137695));
#183566=CARTESIAN_POINT('',(-25.3107727110825,-57.3172883154489,39.92499));
#183567=CARTESIAN_POINT('',(-24.9906253009261,-56.5982254591674,39.116));
#183568=CARTESIAN_POINT('Origin',(-25.0061753086093,-56.6331513482585,39.5550293907201));
#183569=CARTESIAN_POINT('',(-24.8273695326456,-56.2315470018076,39.116));
#183570=CARTESIAN_POINT('',(0.174030409680921,-0.0774833305059407,39.116));
#183571=CARTESIAN_POINT('',(-24.776105164832,-56.1164053447571,39.3343017080178));
#183572=CARTESIAN_POINT('',(-24.8273695332959,-56.2315470015181,39.116));
#183573=CARTESIAN_POINT('',(-24.641898292288,-55.8149717737125,39.5248017080178));
#183574=CARTESIAN_POINT('Origin',(-24.6538679703959,-55.841854848728,39.1947747614267));
#183575=CARTESIAN_POINT('',(-24.5803964109126,-55.6768362864791,39.5248017080178));
#183576=CARTESIAN_POINT('',(0.174030409680921,-0.0774833305059407,39.5248017080178));
#183577=CARTESIAN_POINT('',(-24.4461895095991,-55.3754026508174,39.3343017080178));
#183578=CARTESIAN_POINT('Origin',(-24.568426487815,-55.6499501367141,39.1947728911901));
#183579=CARTESIAN_POINT('',(-24.3949251197297,-55.2602609459789,39.116));
#183580=CARTESIAN_POINT('',(-24.4461895095991,-55.3754026508174,39.3343017080178));
#183581=CARTESIAN_POINT('',(0.174030409680921,-0.0774833305059407,39.116));
#183582=CARTESIAN_POINT('Origin',(-0.174030409680915,0.0774833305059407,
2.45064239960504E-17));
#183583=CARTESIAN_POINT('',(-25.338686120288,-56.4432587981556,39.116));
#183584=CARTESIAN_POINT('',(-25.5139139873792,-56.8368270314553,39.3548010137695));
#183585=CARTESIAN_POINT('Origin',(-25.3542361278543,-56.4781846869842,39.5550293912438));
#183586=CARTESIAN_POINT('',(-25.6588335308579,-57.1623216542529,39.92499));
#183587=CARTESIAN_POINT('',(-25.5139139873792,-56.8368270314553,39.3548010137695));
#183588=CARTESIAN_POINT('',(-24.2595822759735,-54.019551880964,39.92499));
#183589=CARTESIAN_POINT('',(-0.174030409680907,0.0774833305059458,39.92499));
#183590=CARTESIAN_POINT('',(-24.4045020177493,-54.3450469519942,39.3548010137695));
#183591=CARTESIAN_POINT('',(-24.2595822759735,-54.019551880964,39.92499));
#183592=CARTESIAN_POINT('',(-24.5797300649104,-54.7386155880002,39.116));
#183593=CARTESIAN_POINT('Origin',(-24.5641801071868,-54.7036898111204,39.5550297827287));
#183594=CARTESIAN_POINT('',(-24.742985938414,-55.1052942852688,39.116));
#183595=CARTESIAN_POINT('',(-24.7730266428387,-55.172766810297,39.116));
#183596=CARTESIAN_POINT('',(-24.794250328961,-55.2204359898055,39.3343017080178));
#183597=CARTESIAN_POINT('',(-24.7429859390916,-55.1052942849671,39.116));
#183598=CARTESIAN_POINT('',(-24.9284572302744,-55.5218696254672,39.5248017080178));
#183599=CARTESIAN_POINT('Origin',(-24.9164875765753,-55.4949866055695,39.1947745585593));
#183600=CARTESIAN_POINT('',(-24.9899591116498,-55.6600051127007,39.5248017080178));
#183601=CARTESIAN_POINT('',(-24.9901741577757,-55.6604881142075,39.5248017080178));
#183602=CARTESIAN_POINT('',(-25.1241659841938,-55.9614386837452,39.3343017080178));
#183603=CARTESIAN_POINT('Origin',(-25.001929004471,-55.686891194182,39.1947728594246));
#183604=CARTESIAN_POINT('',(-25.1754303526578,-56.0765803405062,39.116));
#183605=CARTESIAN_POINT('',(-25.1241659841938,-55.9614386837452,39.3343017080178));
#183606=CARTESIAN_POINT('',(-25.3388981863709,-56.4437351063763,39.116));
#183607=CARTESIAN_POINT('Origin',(-28.9669082278886,-50.5531567888874,40.10025));
#183608=CARTESIAN_POINT('',(-29.5274749692187,-51.1126068659046,40.10025));
#183609=CARTESIAN_POINT('',(-31.4364195775137,-54.4189959163062,40.10025));
#183610=CARTESIAN_POINT('',(-29.1450842944632,-50.4502867888874,40.10025));
#183611=CARTESIAN_POINT('',(-31.4100231232064,-54.4342359163062,40.10025));
#183612=CARTESIAN_POINT('Origin',(2.54115089989956E-17,1.27310796826192E-16,
40.10025));
#183613=CARTESIAN_POINT('',(-29.5010785149114,-51.1278468659046,40.10025));
#183614=CARTESIAN_POINT('',(-29.465726992033,-51.0666162321542,40.10025));
#183615=CARTESIAN_POINT('Origin',(3.55814779065492E-16,-6.62864452791125E-17,
40.10025));
#183616=CARTESIAN_POINT('Origin',(0.164977839420935,-0.0952500000000008,
-2.32316690526364E-17));
#183617=CARTESIAN_POINT('',(-29.8368674217658,-52.0599703131945,39.116));
#183618=CARTESIAN_POINT('',(-29.6214601680814,-51.6868740054942,39.3548010137695));
#183619=CARTESIAN_POINT('Origin',(-29.8177519107039,-52.0268612768225,39.5550297832829));
#183620=CARTESIAN_POINT('',(-29.4433108120869,-51.3783102685125,39.92499));
#183621=CARTESIAN_POINT('',(-29.6214601680814,-51.6868740054942,39.3548010137695));
#183622=CARTESIAN_POINT('',(-31.1634057161443,-54.3576020372437,39.92499));
#183623=CARTESIAN_POINT('',(-31.2932988600175,-54.5825835619869,39.92499));
#183624=CARTESIAN_POINT('',(-30.9852566042328,-54.0490387253004,39.3548010137695));
#183625=CARTESIAN_POINT('',(-31.1634057161443,-54.3576020372437,39.92499));
#183626=CARTESIAN_POINT('',(-30.7698495716383,-53.6759427993285,39.116));
#183627=CARTESIAN_POINT('Origin',(-30.7889651442679,-53.7090519423387,39.555029390718));
#183628=CARTESIAN_POINT('',(-30.5691597998771,-53.3283379195022,39.116));
#183629=CARTESIAN_POINT('',(0.164977839420941,-0.0952500000000008,39.116));
#183630=CARTESIAN_POINT('',(-30.5061406831646,-53.2191856060844,39.3343017080178));
#183631=CARTESIAN_POINT('',(-30.5691598004935,-53.3283379191463,39.116));
#183632=CARTESIAN_POINT('',(-30.3411606219521,-52.9334317578286,39.5248017080178));
#183633=CARTESIAN_POINT('Origin',(-30.3558747754319,-52.9589163924907,39.1947747614318));
#183634=CARTESIAN_POINT('',(-30.2655565641147,-52.8024816883958,39.5248017080178));
#183635=CARTESIAN_POINT('',(0.164977839420941,-0.0952500000000008,39.5248017080178));
#183636=CARTESIAN_POINT('',(-30.100576467536,-52.516727778884,39.3343017080178));
#183637=CARTESIAN_POINT('Origin',(-30.250841845589,-52.7769940214372,39.1947728911941));
#183638=CARTESIAN_POINT('',(-30.0375573238934,-52.4075754202455,39.116));
#183639=CARTESIAN_POINT('',(-30.100576467536,-52.516727778884,39.3343017080178));
#183640=CARTESIAN_POINT('',(0.164977839420941,-0.0952500000000008,39.116));
#183641=CARTESIAN_POINT('Origin',(-0.164977839420935,0.0952500000000008,
2.32316690526364E-17));
#183642=CARTESIAN_POINT('',(-31.0998052504802,-53.4854427993285,39.116));
#183643=CARTESIAN_POINT('',(-31.3152122835989,-53.8585387249978,39.3548010137695));
#183644=CARTESIAN_POINT('Origin',(-31.1189208229653,-53.5185519420886,39.5550293912447));
#183645=CARTESIAN_POINT('',(-31.493361395377,-54.167102037018,39.92499));
#183646=CARTESIAN_POINT('',(-31.3152122835989,-53.8585387249977,39.3548010137695));
#183647=CARTESIAN_POINT('',(-29.7732664904682,-51.1878102687783,39.92499));
#183648=CARTESIAN_POINT('',(-0.164977839420927,0.0952500000000056,39.92499));
#183649=CARTESIAN_POINT('',(-29.951415846311,-51.4963740058477,39.3548010137695));
#183650=CARTESIAN_POINT('',(-29.7732664904682,-51.1878102687783,39.92499));
#183651=CARTESIAN_POINT('',(-30.1668231006077,-51.8694703131945,39.116));
#183652=CARTESIAN_POINT('Origin',(-30.1477075893945,-51.8363612765607,39.5550297827313));
#183653=CARTESIAN_POINT('',(-30.3675130020931,-52.2170754206163,39.116));
#183654=CARTESIAN_POINT('',(-30.4044419397496,-52.2810382154238,39.116));
#183655=CARTESIAN_POINT('',(-30.4305321463779,-52.326227778884,39.3343017080178));
#183656=CARTESIAN_POINT('',(-30.3675130027353,-52.2170754202455,39.116));
#183657=CARTESIAN_POINT('',(-30.5955122429565,-52.6119816883958,39.5248017080178));
#183658=CARTESIAN_POINT('Origin',(-30.5807981195149,-52.5864971060008,39.1947745585599));
#183659=CARTESIAN_POINT('',(-30.671116300794,-52.7429317578286,39.5248017080178));
#183660=CARTESIAN_POINT('',(-30.6713806562799,-52.7433896349616,39.5248017080178));
#183661=CARTESIAN_POINT('',(-30.8360963620065,-53.0286856060844,39.3343017080178));
#183662=CARTESIAN_POINT('Origin',(-30.6858309820702,-52.7684193600399,39.1947728594235));
#183663=CARTESIAN_POINT('',(-30.8991154793354,-53.1378379191463,39.116));
#183664=CARTESIAN_POINT('',(-30.8360963620065,-53.0286856060844,39.3343017080178));
#183665=CARTESIAN_POINT('',(-31.1000659426093,-53.4858943313412,39.116));
#183666=CARTESIAN_POINT('Origin',(-34.0924682662297,-47.2483549038574,40.10025));
#183667=CARTESIAN_POINT('',(-34.7084426211234,-47.7461450747863,40.10025));
#183668=CARTESIAN_POINT('',(-36.9525415975215,-50.8348823336484,40.10025));
#183669=CARTESIAN_POINT('',(-34.2589154226524,-47.1274239660508,40.10025));
#183670=CARTESIAN_POINT('',(-36.9278827595329,-50.8527980281383,40.10025));
#183671=CARTESIAN_POINT('Origin',(3.83164542466812E-17,1.18930227392546E-16,
40.10025));
#183672=CARTESIAN_POINT('',(-34.6837837831348,-47.7640607692762,40.10025));
#183673=CARTESIAN_POINT('',(-34.6422255755468,-47.7068608037048,40.10025));
#183674=CARTESIAN_POINT('Origin',(3.49095608592005E-16,-6.19229649536416E-17,
40.10025));
#183675=CARTESIAN_POINT('Origin',(0.154117737428427,-0.111973090561717,
-2.17023830815425E-17));
#183676=CARTESIAN_POINT('',(-35.1151666347443,-48.6559784483763,39.116));
#183677=CARTESIAN_POINT('',(-34.8619402208392,-48.3074421904916,39.3548010137695));
#183678=CARTESIAN_POINT('Origin',(-35.0926950037607,-48.6250489017669,39.5550297832855));
#183679=CARTESIAN_POINT('',(-34.65251309241,-48.019190476361,39.92499));
#183680=CARTESIAN_POINT('',(-34.8619402208392,-48.3074421904916,39.3548010137695));
#183681=CARTESIAN_POINT('',(-36.674605926818,-50.8023624960589,39.92499));
#183682=CARTESIAN_POINT('',(-36.8273044755032,-51.0125340177513,39.92499));
#183683=CARTESIAN_POINT('',(-36.4651790855633,-50.5141111791247,39.3548010137695));
#183684=CARTESIAN_POINT('',(-36.674605926818,-50.8023624960589,39.92499));
#183685=CARTESIAN_POINT('',(-36.2119529314387,-50.165575277767,39.116));
#183686=CARTESIAN_POINT('Origin',(-36.2344246347989,-50.1965049239941,39.5550293907223));
#183687=CARTESIAN_POINT('',(-35.9760279553332,-49.8408524072785,39.116));
#183688=CARTESIAN_POINT('',(0.154117737428432,-0.111973090561717,39.116));
#183689=CARTESIAN_POINT('',(-35.9019445403521,-49.738885333081,39.3343017080178));
#183690=CARTESIAN_POINT('',(-35.9760279559089,-49.8408524068602,39.116));
#183691=CARTESIAN_POINT('',(-35.7079988465461,-49.4719419865731,39.5248017080178));
#183692=CARTESIAN_POINT('Origin',(-35.7252962640503,-49.4957489658867,39.1947747614277));
#183693=CARTESIAN_POINT('',(-35.6191209461254,-49.3496120513048,39.5248017080178));
#183694=CARTESIAN_POINT('',(0.154117737428432,-0.111973090561717,39.5248017080178));
#183695=CARTESIAN_POINT('',(-35.425175210744,-49.0826686475733,39.3343017080178));
#183696=CARTESIAN_POINT('Origin',(-35.6018226497073,-49.3258021153664,39.1947728911967));
#183697=CARTESIAN_POINT('',(-35.3510917642536,-48.9807015312177,39.116));
#183698=CARTESIAN_POINT('',(-35.425175210744,-49.0826686475733,39.3343017080178));
#183699=CARTESIAN_POINT('',(0.154117737428432,-0.111973090561717,39.116));
#183700=CARTESIAN_POINT('Origin',(-0.154117737428427,0.111973090561717,
2.17023830815425E-17));
#183701=CARTESIAN_POINT('',(-36.5201884062956,-49.9416290966435,39.116));
#183702=CARTESIAN_POINT('',(-36.7734145609101,-50.2901649976454,39.3548010137695));
#183703=CARTESIAN_POINT('Origin',(-36.5426601094875,-49.9725587426392,39.5550293912446));
#183704=CARTESIAN_POINT('',(-36.9828414020407,-50.5784163146697,39.92499));
#183705=CARTESIAN_POINT('',(-36.7734145609101,-50.2901649976454,39.3548010137695));
#183706=CARTESIAN_POINT('',(-34.9607485668368,-47.79524429555,39.92499));
#183707=CARTESIAN_POINT('',(-0.154117737428418,0.111973090561721,39.92499));
#183708=CARTESIAN_POINT('',(-35.1701756951245,-48.0834960097835,39.3548010137695));
#183709=CARTESIAN_POINT('',(-34.9607485668368,-47.79524429555,39.92499));
#183710=CARTESIAN_POINT('',(-35.4234021096012,-48.4320322672529,39.116));
#183711=CARTESIAN_POINT('Origin',(-35.4009304784381,-48.4011027203966,39.555029782729));
#183712=CARTESIAN_POINT('',(-35.6593272385104,-48.7567553505302,39.116));
#183713=CARTESIAN_POINT('',(-35.7027398082301,-48.8165076253518,39.116));
#183714=CARTESIAN_POINT('',(-35.7334106856009,-48.8587224664499,39.3343017080178));
#183715=CARTESIAN_POINT('',(-35.6593272391104,-48.7567553500942,39.116));
#183716=CARTESIAN_POINT('',(-35.9273564209823,-49.1256658701813,39.5248017080178));
#183717=CARTESIAN_POINT('Origin',(-35.910059038814,-49.1018589397074,39.1947745585586));
#183718=CARTESIAN_POINT('',(-36.0162343214029,-49.2479958054497,39.5248017080178));
#183719=CARTESIAN_POINT('',(-36.0165450899149,-49.2484235416111,39.5248017080178));
#183720=CARTESIAN_POINT('',(-36.2101800152089,-49.5149391519575,39.3343017080178));
#183721=CARTESIAN_POINT('Origin',(-36.0335325740062,-49.2718056808869,39.1947728594212));
#183722=CARTESIAN_POINT('',(-36.2842634307658,-49.6169062257368,39.116));
#183723=CARTESIAN_POINT('',(-36.2101800152089,-49.5149391519575,39.3343017080178));
#183724=CARTESIAN_POINT('',(-36.5204948682733,-49.942050905369,39.116));
#183725=CARTESIAN_POINT('Origin',(-38.8445040879384,-43.4258901551469,40.10025));
#183726=CARTESIAN_POINT('',(-39.5091373124624,-43.8565665267054,40.10025));
#183727=CARTESIAN_POINT('',(-42.0638038389703,-46.6938111422602,40.10025));
#183728=CARTESIAN_POINT('',(-38.9973987043321,-43.2882232241946,40.10025));
#183729=CARTESIAN_POINT('',(-42.0411527846897,-46.7142062431421,40.10025));
#183730=CARTESIAN_POINT('Origin',(5.02746968098277E-17,1.09246633499838E-16,
40.10025));
#183731=CARTESIAN_POINT('',(-39.4864862581819,-43.8769616275872,40.10025));
#183732=CARTESIAN_POINT('',(-39.4391766863032,-43.8244190249876,40.10025));
#183733=CARTESIAN_POINT('Origin',(3.42869354330331E-16,-5.68810436659251E-17,
40.10025));
#183734=CARTESIAN_POINT('Origin',(0.141569089253443,-0.127469380511363,
-1.99353212598915E-17));
#183735=CARTESIAN_POINT('',(-40.0087367337515,-44.7189015017597,39.116));
#183736=CARTESIAN_POINT('',(-39.7204655612076,-44.3987439298679,39.3548010137695));
#183737=CARTESIAN_POINT('Origin',(-39.9831551867361,-44.6904903154957,39.5550297832831));
#183738=CARTESIAN_POINT('',(-39.4820551877882,-44.1339623846889,39.92499));
#183739=CARTESIAN_POINT('',(-39.7204655612076,-44.3987439298679,39.3548010137695));
#183740=CARTESIAN_POINT('',(-41.7839914803029,-46.6905216402895,39.92499));
#183741=CARTESIAN_POINT('',(-41.9578224365464,-46.8835804757583,39.92499));
#183742=CARTESIAN_POINT('',(-41.5455814340034,-46.4257404601129,39.3548010137695));
#183743=CARTESIAN_POINT('',(-41.7839914803029,-46.6905216402895,39.92499));
#183744=CARTESIAN_POINT('',(-41.2573105570839,-46.1055832156407,39.116));
#183745=CARTESIAN_POINT('Origin',(-41.2828921864909,-46.1339944934099,39.5550293907235));
#183746=CARTESIAN_POINT('',(-40.9887352200426,-45.807300086212,39.116));
#183747=CARTESIAN_POINT('',(0.141569089253448,-0.127469380511363,39.116));
#183748=CARTESIAN_POINT('',(-40.9043991801906,-45.7136354238374,39.3343017080178));
#183749=CARTESIAN_POINT('',(-40.9887352205716,-45.8073000857357,39.116));
#183750=CARTESIAN_POINT('',(-40.6836127633981,-45.4684272662434,39.5248017080178));
#183751=CARTESIAN_POINT('Origin',(-40.7033039308042,-45.4902957559654,39.1947747614341));
#183752=CARTESIAN_POINT('',(-40.5824347852702,-45.3560577375094,39.5248017080178));
#183753=CARTESIAN_POINT('',(0.141569089253449,-0.127469380511363,39.5248017080178));
#183754=CARTESIAN_POINT('',(-40.3616483211486,-45.1108495273511,39.3343017080178));
#183755=CARTESIAN_POINT('Origin',(-40.5627424347164,-45.334186399234,39.1947728911947));
#183756=CARTESIAN_POINT('',(-40.277312245553,-45.0171848263431,39.116));
#183757=CARTESIAN_POINT('',(-40.3616483211486,-45.1108495273511,39.3343017080178));
#183758=CARTESIAN_POINT('',(0.141569089253448,-0.127469380511363,39.116));
#183759=CARTESIAN_POINT('Origin',(-0.141569089253443,0.127469380511363,
1.99353212598915E-17));
#183760=CARTESIAN_POINT('',(-41.5404487355908,-45.850644454618,39.116));
#183761=CARTESIAN_POINT('',(-41.8287196129601,-46.1708016986852,39.3548010137695));
#183762=CARTESIAN_POINT('Origin',(-41.5660303648068,-45.8790557321751,39.5550293912439));
#183763=CARTESIAN_POINT('',(-42.0671296591461,-46.435582878964,39.92499));
#183764=CARTESIAN_POINT('',(-41.8287196129601,-46.1708016986852,39.3548010137695));
#183765=CARTESIAN_POINT('',(-39.7651933659001,-43.8790236240218,39.92499));
#183766=CARTESIAN_POINT('',(-0.141569089253434,0.127469380511367,39.92499));
#183767=CARTESIAN_POINT('',(-40.0036037391898,-44.1438051693176,39.3548010137695));
#183768=CARTESIAN_POINT('',(-39.7651933659001,-43.8790236240218,39.92499));
#183769=CARTESIAN_POINT('',(-40.2918749122584,-44.4639627407369,39.116));
#183770=CARTESIAN_POINT('Origin',(-40.2662933650397,-44.4355515542471,39.555029782729));
#183771=CARTESIAN_POINT('',(-40.560450423509,-44.7622460658163,39.116));
#183772=CARTESIAN_POINT('',(-40.609870988093,-44.8171331622254,39.116));
#183773=CARTESIAN_POINT('',(-40.6447864996555,-44.8559107663283,39.3343017080178));
#183774=CARTESIAN_POINT('',(-40.5604504240599,-44.7622460653203,39.116));
#183775=CARTESIAN_POINT('',(-40.8655729637771,-45.1011189764867,39.5248017080178));
#183776=CARTESIAN_POINT('Origin',(-40.8458818366203,-45.0792505316452,39.1947745585594));
#183777=CARTESIAN_POINT('',(-40.966750941905,-45.2134885052207,39.5248017080178));
#183778=CARTESIAN_POINT('',(-40.9671047185982,-45.2138814140436,39.5248017080178));
#183779=CARTESIAN_POINT('',(-41.1875373586974,-45.4586966628146,39.3343017080178));
#183780=CARTESIAN_POINT('Origin',(-40.9864432425609,-45.2353597879075,39.1947728594213));
#183781=CARTESIAN_POINT('',(-41.2718733990785,-45.5523613247129,39.116));
#183782=CARTESIAN_POINT('',(-41.1875373586974,-45.4586966628146,39.3343017080178));
#183783=CARTESIAN_POINT('',(-41.5407976097556,-45.8510319186315,39.116));
#183784=CARTESIAN_POINT('Origin',(-43.1709513941246,-39.1276422664448,40.10025));
#183785=CARTESIAN_POINT('',(-43.8769616275876,-39.4864862581814,40.10025));
#183786=CARTESIAN_POINT('',(-46.7142062431425,-42.0411527846893,40.10025));
#183787=CARTESIAN_POINT('',(-43.3086183250768,-38.9747476500511,40.10025));
#183788=CARTESIAN_POINT('',(-46.6938111422606,-42.0638038389698,40.10025));
#183789=CARTESIAN_POINT('Origin',(6.11552196804858E-17,9.83661106291779E-17,
40.10025));
#183790=CARTESIAN_POINT('',(-43.8565665267058,-39.509137312462,40.10025));
#183791=CARTESIAN_POINT('',(-43.8040239241062,-39.4618277405834,40.10025));
#183792=CARTESIAN_POINT('Origin',(3.37204232425085E-16,-5.1215921760681E-17,
40.10025));
#183793=CARTESIAN_POINT('Origin',(0.127469380511362,-0.141569089253444,
-1.7949843886783E-17));
#183794=CARTESIAN_POINT('',(-44.4639627407373,-40.291874912258,39.116));
#183795=CARTESIAN_POINT('',(-44.1438051688456,-40.003603739714,39.3548010137695));
#183796=CARTESIAN_POINT('Origin',(-44.4355515544744,-40.2662933652435,39.5550297832866));
#183797=CARTESIAN_POINT('',(-43.8790236243775,-39.7651933655051,39.92499));
#183798=CARTESIAN_POINT('',(-44.1438051688456,-40.003603739714,39.3548010137695));
#183799=CARTESIAN_POINT('',(-46.4355828792672,-42.0671296588093,39.92499));
#183800=CARTESIAN_POINT('',(-46.6286417147359,-42.2409606150528,39.92499));
#183801=CARTESIAN_POINT('',(-46.1708016982804,-41.8287196134097,39.3548010137695));
#183802=CARTESIAN_POINT('',(-46.4355828792672,-42.0671296588093,39.92499));
#183803=CARTESIAN_POINT('',(-45.8506444546184,-41.5404487355903,39.116));
#183804=CARTESIAN_POINT('Origin',(-45.8790557323879,-41.5660303649976,39.5550293907227));
#183805=CARTESIAN_POINT('',(-45.552361324237,-41.271873399607,39.116));
#183806=CARTESIAN_POINT('',(0.127469380511367,-0.141569089253444,39.116));
#183807=CARTESIAN_POINT('',(-45.458696662815,-41.187537358697,39.3343017080178));
#183808=CARTESIAN_POINT('',(-45.5523613247134,-41.271873399078,39.116));
#183809=CARTESIAN_POINT('',(-45.2134885052211,-40.9667509419045,39.5248017080178));
#183810=CARTESIAN_POINT('Origin',(-45.2353576819754,-40.986441346282,39.1947747614315));
#183811=CARTESIAN_POINT('',(-45.1011189764871,-40.8655729637766,39.5248017080178));
#183812=CARTESIAN_POINT('',(0.127469380511367,-0.141569089253444,39.5248017080178));
#183813=CARTESIAN_POINT('',(-44.8559107663287,-40.644786499655,39.3343017080178));
#183814=CARTESIAN_POINT('Origin',(-45.0792483253096,-40.8458798501216,39.1947728911967));
#183815=CARTESIAN_POINT('',(-44.7622460653207,-40.5604504240595,39.116));
#183816=CARTESIAN_POINT('',(-44.8559107663287,-40.644786499655,39.3343017080178));
#183817=CARTESIAN_POINT('',(0.127469380511367,-0.141569089253444,39.116));
#183818=CARTESIAN_POINT('Origin',(-0.127469380511362,0.141569089253444,
1.7949843886783E-17));
#183819=CARTESIAN_POINT('',(-46.1055832156411,-41.2573105570834,39.116));
#183820=CARTESIAN_POINT('',(-46.4257404597083,-41.5455814344528,39.3548010137695));
#183821=CARTESIAN_POINT('Origin',(-46.1339944931974,-41.2828921862988,39.5550293912464));
#183822=CARTESIAN_POINT('',(-46.6905216405927,-41.7839914799662,39.92499));
#183823=CARTESIAN_POINT('',(-46.4257404597083,-41.5455814344528,39.3548010137695));
#183824=CARTESIAN_POINT('',(-44.1339623850449,-39.4820551873928,39.92499));
#183825=CARTESIAN_POINT('',(-0.127469380511352,0.141569089253448,39.92499));
#183826=CARTESIAN_POINT('',(-44.3987439293951,-39.7204655617327,39.3548010137695));
#183827=CARTESIAN_POINT('',(-44.1339623850449,-39.4820551873928,39.92499));
#183828=CARTESIAN_POINT('',(-44.7189015017601,-40.0087367337511,39.116));
#183829=CARTESIAN_POINT('Origin',(-44.6904903152715,-39.9831551865335,39.5550297827315));
#183830=CARTESIAN_POINT('',(-45.0171848258473,-40.2773122461036,39.116));
#183831=CARTESIAN_POINT('',(-45.0720719232486,-40.3267328095857,39.116));
#183832=CARTESIAN_POINT('',(-45.1108495273515,-40.3616483211481,39.3343017080178));
#183833=CARTESIAN_POINT('',(-45.0171848263434,-40.2773122455526,39.116));
#183834=CARTESIAN_POINT('',(-45.3560577375098,-40.5824347852697,39.5248017080178));
#183835=CARTESIAN_POINT('Origin',(-45.3341886054736,-40.562744421318,39.1947745585619));
#183836=CARTESIAN_POINT('',(-45.4684272662438,-40.6836127633977,39.5248017080178));
#183837=CARTESIAN_POINT('',(-45.4688201750668,-40.6839665400909,39.5248017080178));
#183838=CARTESIAN_POINT('',(-45.7136354238378,-40.9043991801901,39.3343017080178));
#183839=CARTESIAN_POINT('Origin',(-45.4902978619858,-40.7033058269843,39.1947728594229));
#183840=CARTESIAN_POINT('',(-45.8073000857361,-40.9887352205711,39.116));
#183841=CARTESIAN_POINT('',(-45.7136354238378,-40.9043991801901,39.3343017080178));
#183842=CARTESIAN_POINT('',(-46.1059706796546,-41.2576594312482,39.116));
#183843=CARTESIAN_POINT('Origin',(-47.0244087227343,-34.4007037410861,40.10025));
#183844=CARTESIAN_POINT('',(-47.7640607692765,-34.6837837831344,40.10025));
#183845=CARTESIAN_POINT('',(-50.8527980281387,-36.9278827595324,40.10025));
#183846=CARTESIAN_POINT('',(-47.145339660541,-34.2342565846634,40.10025));
#183847=CARTESIAN_POINT('',(-50.8348823336488,-36.9525415975209,40.10025));
#183848=CARTESIAN_POINT('Origin',(7.08388135731919E-17,8.64078680660324E-17,
40.10025));
#183849=CARTESIAN_POINT('',(-47.7461450747866,-34.7084426211229,40.10025));
#183850=CARTESIAN_POINT('',(-47.6889451092153,-34.6668844135349,40.10025));
#183851=CARTESIAN_POINT('Origin',(3.32162311137368E-16,-4.49896674990063E-17,
40.10025));
#183852=CARTESIAN_POINT('Origin',(0.111973090561715,-0.154117737428428,
-1.57677042678046E-17));
#183853=CARTESIAN_POINT('',(-48.4320322672532,-35.4234021096007,39.116));
#183854=CARTESIAN_POINT('',(-48.0834960093685,-35.1701756956956,39.3548010137695));
#183855=CARTESIAN_POINT('Origin',(-48.401102720643,-35.4009304786164,39.555029783284));
#183856=CARTESIAN_POINT('',(-47.7952442958628,-34.9607485664063,39.92499));
#183857=CARTESIAN_POINT('',(-48.0834960093685,-35.1701756956956,39.3548010137695));
#183858=CARTESIAN_POINT('',(-50.5784163149358,-36.9828414016744,39.92499));
#183859=CARTESIAN_POINT('',(-50.7885878366283,-37.1355399503595,39.92499));
#183860=CARTESIAN_POINT('',(-50.2901649972901,-36.773414561399,39.3548010137695));
#183861=CARTESIAN_POINT('',(-50.5784163149359,-36.9828414016744,39.92499));
#183862=CARTESIAN_POINT('',(-49.9416290966439,-36.5201884062951,39.116));
#183863=CARTESIAN_POINT('Origin',(-49.9725587428701,-36.5426601096545,39.555029390725));
#183864=CARTESIAN_POINT('',(-49.6169062253186,-36.2842634313414,39.116));
#183865=CARTESIAN_POINT('',(0.111973090561721,-0.154117737428428,39.116));
#183866=CARTESIAN_POINT('',(-49.5149391519579,-36.2101800152084,39.3343017080178));
#183867=CARTESIAN_POINT('',(-49.6169062257371,-36.2842634307653,39.116));
#183868=CARTESIAN_POINT('',(-49.2479958054501,-36.0162343214024,39.5248017080178));
#183869=CARTESIAN_POINT('Origin',(-49.2718033882782,-36.0335309082465,39.1947747614342));
#183870=CARTESIAN_POINT('',(-49.1256658701817,-35.9273564209818,39.5248017080178));
#183871=CARTESIAN_POINT('',(0.111973090561721,-0.154117737428428,39.5248017080178));
#183872=CARTESIAN_POINT('',(-48.8587224664502,-35.7334106856004,39.3343017080178));
#183873=CARTESIAN_POINT('Origin',(-49.1018565378149,-35.9100572938239,39.1947728911913));
#183874=CARTESIAN_POINT('',(-48.7567553500946,-35.6593272391099,39.116));
#183875=CARTESIAN_POINT('',(-48.8587224664502,-35.7334106856004,39.3343017080178));
#183876=CARTESIAN_POINT('',(0.111973090561721,-0.154117737428428,39.116));
#183877=CARTESIAN_POINT('Origin',(-0.111973090561715,0.154117737428428,
1.57677042678046E-17));
#183878=CARTESIAN_POINT('',(-50.1655752777673,-36.2119529314382,39.116));
#183879=CARTESIAN_POINT('',(-50.5141111787691,-36.4651790860527,39.3548010137695));
#183880=CARTESIAN_POINT('Origin',(-50.1965049237625,-36.2344246346299,39.5550293912453));
#183881=CARTESIAN_POINT('',(-50.8023624963252,-36.6746059264515,39.92499));
#183882=CARTESIAN_POINT('',(-50.5141111787691,-36.4651790860527,39.3548010137695));
#183883=CARTESIAN_POINT('',(-48.0191904766738,-34.6525130919795,39.92499));
#183884=CARTESIAN_POINT('',(-0.111973090561705,0.154117737428431,39.92499));
#183885=CARTESIAN_POINT('',(-48.3074421900765,-34.8619402214106,39.3548010137695));
#183886=CARTESIAN_POINT('',(-48.0191904766738,-34.6525130919795,39.92499));
#183887=CARTESIAN_POINT('',(-48.6559784483767,-35.1151666347439,39.116));
#183888=CARTESIAN_POINT('Origin',(-48.625048901522,-35.092695003582,39.555029782732));
#183889=CARTESIAN_POINT('',(-48.9807015307823,-35.3510917648528,39.116));
#183890=CARTESIAN_POINT('',(-49.0404538064756,-35.3945043333728,39.116));
#183891=CARTESIAN_POINT('',(-49.0826686475736,-35.4251752107435,39.3343017080178));
#183892=CARTESIAN_POINT('',(-48.980701531218,-35.3510917642531,39.116));
#183893=CARTESIAN_POINT('',(-49.3496120513051,-35.6191209461249,39.5248017080178));
#183894=CARTESIAN_POINT('Origin',(-49.325804517179,-35.6018243948132,39.1947745585582));
#183895=CARTESIAN_POINT('',(-49.4719419865735,-35.7079988465456,39.5248017080178));
#183896=CARTESIAN_POINT('',(-49.4723697227349,-35.7083096150576,39.5248017080178));
#183897=CARTESIAN_POINT('',(-49.7388853330813,-35.9019445403516,39.3343017080178));
#183898=CARTESIAN_POINT('Origin',(-49.4957512585773,-35.7252979297056,39.1947728594226));
#183899=CARTESIAN_POINT('',(-49.8408524068606,-35.9760279559084,39.116));
#183900=CARTESIAN_POINT('',(-49.7388853330813,-35.9019445403516,39.3343017080178));
#183901=CARTESIAN_POINT('',(-50.1659970864927,-36.2122593934159,39.116));
#183902=CARTESIAN_POINT('Origin',(-50.3626567888877,-29.2968639067299,40.10025));
#183903=CARTESIAN_POINT('',(-51.1278468659049,-29.5010785149108,40.10025));
#183904=CARTESIAN_POINT('',(-54.4342359163065,-31.4100231232058,40.10025));
#183905=CARTESIAN_POINT('',(-50.4655267888877,-29.1186878401553,40.10025));
#183906=CARTESIAN_POINT('',(-54.4189959163065,-31.4364195775132,40.10025));
#183907=CARTESIAN_POINT('Origin',(7.92193830068373E-17,7.35029228183466E-17,
40.10025));
#183908=CARTESIAN_POINT('',(-51.1126068659049,-29.5274749692182,40.10025));
#183909=CARTESIAN_POINT('',(-51.0513762321546,-29.4921234463398,40.10025));
#183910=CARTESIAN_POINT('Origin',(3.27798830811897E-16,-3.82704970255191E-17,
40.10025));
#183911=CARTESIAN_POINT('Origin',(0.095249999999999,-0.164977839420936,
-1.34128103812638E-17));
#183912=CARTESIAN_POINT('',(-51.8694703131948,-30.1668231006072,39.116));
#183913=CARTESIAN_POINT('',(-51.4963740054945,-29.9514158469227,39.3548010137695));
#183914=CARTESIAN_POINT('Origin',(-51.8363612768256,-30.1477075895468,39.5550297832895));
#183915=CARTESIAN_POINT('',(-51.1878102690446,-29.7732664900071,39.92499));
#183916=CARTESIAN_POINT('',(-51.4963740054945,-29.9514158469227,39.3548010137695));
#183917=CARTESIAN_POINT('',(-54.167102037244,-31.4933613949856,39.92499));
#183918=CARTESIAN_POINT('',(-54.3920835619873,-31.6232545388588,39.92499));
#183919=CARTESIAN_POINT('',(-53.8585387246954,-31.3152122841226,39.3548010137695));
#183920=CARTESIAN_POINT('',(-54.167102037244,-31.4933613949856,39.92499));
#183921=CARTESIAN_POINT('',(-53.4854427993288,-31.0998052504797,39.116));
#183922=CARTESIAN_POINT('Origin',(-53.5185519423378,-31.1189208231085,39.5550293907208));
#183923=CARTESIAN_POINT('',(-53.1378379187909,-30.8991154799509,39.116));
#183924=CARTESIAN_POINT('',(0.0952500000000046,-0.164977839420936,39.116));
#183925=CARTESIAN_POINT('',(-53.0286856060847,-30.8360963620059,39.3343017080178));
#183926=CARTESIAN_POINT('',(-53.1378379191466,-30.8991154793348,39.116));
#183927=CARTESIAN_POINT('',(-52.7429317578289,-30.6711163007934,39.5248017080178));
#183928=CARTESIAN_POINT('Origin',(-52.7684169058718,-30.685829565079,39.194774761439));
#183929=CARTESIAN_POINT('',(-52.6119816883961,-30.595512242956,39.5248017080178));
#183930=CARTESIAN_POINT('',(0.0952500000000046,-0.164977839420936,39.5248017080178));
#183931=CARTESIAN_POINT('',(-52.3262277788843,-30.4305321463774,39.3343017080178));
#183932=CARTESIAN_POINT('Origin',(-52.5864945348662,-30.5807966351507,39.1947728911897));
#183933=CARTESIAN_POINT('',(-52.2170754202458,-30.3675130027348,39.116));
#183934=CARTESIAN_POINT('',(-52.3262277788843,-30.4305321463774,39.3343017080178));
#183935=CARTESIAN_POINT('',(0.0952500000000046,-0.164977839420936,39.116));
#183936=CARTESIAN_POINT('Origin',(-0.095249999999999,0.164977839420936,
1.34128103812638E-17));
#183937=CARTESIAN_POINT('',(-53.6759427993288,-30.7698495716378,39.116));
#183938=CARTESIAN_POINT('',(-54.0490387249981,-30.9852566047565,39.3548010137695));
#183939=CARTESIAN_POINT('Origin',(-53.7090519420885,-30.7889651441227,39.555029391246));
#183940=CARTESIAN_POINT('',(-54.3576020374704,-31.1634057157515,39.92499));
#183941=CARTESIAN_POINT('',(-54.0490387249981,-30.9852566047565,39.3548010137695));
#183942=CARTESIAN_POINT('',(-51.3783102687787,-29.4433108116258,39.92499));
#183943=CARTESIAN_POINT('',(-0.0952499999999886,0.164977839420939,39.92499));
#183944=CARTESIAN_POINT('',(-51.6868740051412,-29.6214601686927,39.3548010137695));
#183945=CARTESIAN_POINT('',(-51.3783102687787,-29.4433108116258,39.92499));
#183946=CARTESIAN_POINT('',(-52.0599703131948,-29.8368674217653,39.116));
#183947=CARTESIAN_POINT('Origin',(-52.0268612765596,-29.8177519105513,39.5550297827285));
#183948=CARTESIAN_POINT('',(-52.407575419875,-30.0375573245352,39.116));
#183949=CARTESIAN_POINT('',(-52.4715382154241,-30.0744862609072,39.116));
#183950=CARTESIAN_POINT('',(-52.5167277788843,-30.1005764675355,39.3343017080178));
#183951=CARTESIAN_POINT('',(-52.4075754202458,-30.0375573238929,39.116));
#183952=CARTESIAN_POINT('',(-52.8024816883961,-30.2655565641141,39.5248017080178));
#183953=CARTESIAN_POINT('Origin',(-52.7769965925041,-30.2508433300763,39.1947745585587));
#183954=CARTESIAN_POINT('',(-52.9334317578289,-30.3411606219516,39.5248017080178));
#183955=CARTESIAN_POINT('',(-52.9338896349619,-30.3414249774375,39.5248017080178));
#183956=CARTESIAN_POINT('',(-53.2191856060847,-30.506140683164,39.3343017080178));
#183957=CARTESIAN_POINT('Origin',(-52.9589188467305,-30.3558761923113,39.1947728594283));
#183958=CARTESIAN_POINT('',(-53.3283379191466,-30.569159800493,39.116));
#183959=CARTESIAN_POINT('',(-53.2191856060847,-30.506140683164,39.3343017080178));
#183960=CARTESIAN_POINT('',(-53.6763943313415,-30.7701102637668,39.116));
#183961=CARTESIAN_POINT('Origin',(-53.1491210481985,-23.8720415006487,40.10025));
#183962=CARTESIAN_POINT('',(-53.9314655730806,-23.9951532569804,40.10025));
#183963=CARTESIAN_POINT('',(-57.419280924679,-25.5480287005715,40.10025));
#183964=CARTESIAN_POINT('',(-53.2328030451449,-23.6840886581933,40.10025));
#183965=CARTESIAN_POINT('',(-57.4068835917981,-25.5758735661205,40.10025));
#183966=CARTESIAN_POINT('Origin',(8.62051087089598E-17,5.97926641667876E-17,
40.10025));
#183967=CARTESIAN_POINT('',(-53.9190682401996,-24.0229981225294,40.10025));
#183968=CARTESIAN_POINT('',(-53.854477793907,-23.994240603043,40.10025));
#183969=CARTESIAN_POINT('Origin',(3.24161598652235E-16,-3.1132026978004E-17,
40.10025));
#183970=CARTESIAN_POINT('Origin',(0.0774833305059389,-0.174030409680916,
-1.0910962937375E-17));
#183971=CARTESIAN_POINT('',(-54.7386155880005,-24.5797300649098,39.116));
#183972=CARTESIAN_POINT('',(-54.3450469517071,-24.4045020183943,39.3548010137695));
#183973=CARTESIAN_POINT('Origin',(-54.7036898113999,-24.5641801073105,39.5550297832868));
#183974=CARTESIAN_POINT('',(-54.0195518811807,-24.2595822754869,39.92499));
#183975=CARTESIAN_POINT('',(-54.3450469517071,-24.4045020183942,39.3548010137695));
#183976=CARTESIAN_POINT('',(-57.1623216544372,-25.6588335304438,39.92499));
#183977=CARTESIAN_POINT('',(-57.3996482375658,-25.7644981330389,39.92499));
#183978=CARTESIAN_POINT('',(-56.8368270312096,-25.5139139879309,39.3548010137695));
#183979=CARTESIAN_POINT('',(-57.1623216544372,-25.6588335304438,39.92499));
#183980=CARTESIAN_POINT('',(-56.4432587981558,-25.3386861202874,39.116));
#183981=CARTESIAN_POINT('Origin',(-56.4781846872462,-25.3542361279703,39.5550293907216));
#183982=CARTESIAN_POINT('',(-56.0765803402172,-25.1754303533067,39.116));
#183983=CARTESIAN_POINT('',(0.0774833305059444,-0.174030409680916,39.116));
#183984=CARTESIAN_POINT('',(-55.9614386837454,-25.1241659841932,39.3343017080178));
#183985=CARTESIAN_POINT('',(-56.0765803405064,-25.1754303526572,39.116));
#183986=CARTESIAN_POINT('',(-55.6600051127009,-24.9899591116492,39.5248017080178));
#183987=CARTESIAN_POINT('Origin',(-55.6868886053382,-25.0019278517709,39.194774761431));
#183988=CARTESIAN_POINT('',(-55.5218696254674,-24.9284572302738,39.5248017080178));
#183989=CARTESIAN_POINT('',(0.0774833305059445,-0.174030409680916,39.5248017080178));
#183990=CARTESIAN_POINT('',(-55.2204359898058,-24.7942503289604,39.3343017080178));
#183991=CARTESIAN_POINT('Origin',(-55.4949838933598,-24.9164863690987,39.1947728911928));
#183992=CARTESIAN_POINT('',(-55.1052942849673,-24.742985939091,39.116));
#183993=CARTESIAN_POINT('',(-55.2204359898058,-24.7942503289604,39.3343017080178));
#183994=CARTESIAN_POINT('',(0.0774833305059444,-0.174030409680916,39.116));
#183995=CARTESIAN_POINT('Origin',(-0.0774833305059389,0.174030409680916,
1.0910962937375E-17));
#183996=CARTESIAN_POINT('',(-56.5982254591677,-24.9906253009256,39.116));
#183997=CARTESIAN_POINT('',(-56.9917936924674,-25.1658531680168,39.3548010137695));
#183998=CARTESIAN_POINT('Origin',(-56.633151347996,-25.0061753084918,39.5550293912444));
#183999=CARTESIAN_POINT('',(-57.3172883156331,-25.3107727106687,39.92499));
#184000=CARTESIAN_POINT('',(-56.9917936924674,-25.1658531680168,39.3548010137695));
#184001=CARTESIAN_POINT('',(-54.1745185419761,-23.9115214566112,39.92499));
#184002=CARTESIAN_POINT('',(-0.0774833305059281,0.174030409680918,39.92499));
#184003=CARTESIAN_POINT('',(-54.5000136124315,-24.0564411996782,39.3548010137695));
#184004=CARTESIAN_POINT('',(-54.1745185419761,-23.9115214566111,39.92499));
#184005=CARTESIAN_POINT('',(-54.8935822490124,-24.231669245548,39.116));
#184006=CARTESIAN_POINT('Origin',(-54.858656472134,-24.2161192878251,39.5550297827315));
#184007=CARTESIAN_POINT('',(-55.2602609456776,-24.3949251204066,39.116));
#184008=CARTESIAN_POINT('',(-55.3277334713091,-24.4249658234763,39.116));
#184009=CARTESIAN_POINT('',(-55.3754026508176,-24.4461895095986,39.3343017080178));
#184010=CARTESIAN_POINT('',(-55.2602609459792,-24.3949251197292,39.116));
#184011=CARTESIAN_POINT('',(-55.6768362864793,-24.580396410912,39.5248017080178));
#184012=CARTESIAN_POINT('Origin',(-55.6499528488661,-24.5684276954198,39.1947745585575));
#184013=CARTESIAN_POINT('',(-55.8149717737128,-24.6418982922874,39.5248017080178));
#184014=CARTESIAN_POINT('',(-55.8154547752196,-24.6421133384133,39.5248017080178));
#184015=CARTESIAN_POINT('',(-56.1164053447573,-24.7761051648314,39.3343017080178));
#184016=CARTESIAN_POINT('Origin',(-55.8418574376333,-24.6538691229782,39.1947728594331));
#184017=CARTESIAN_POINT('',(-56.2315470015183,-24.8273695332954,39.116));
#184018=CARTESIAN_POINT('',(-56.1164053447573,-24.7761051648314,39.3343017080178));
#184019=CARTESIAN_POINT('',(-56.5987017673884,-24.9908373670084,39.116));
#184020=CARTESIAN_POINT('Origin',(-55.3532724151366,-18.1856720123405,40.10025));
#184021=CARTESIAN_POINT('',(-56.1441998575528,-18.2263320786579,40.10025));
#184022=CARTESIAN_POINT('',(-59.7752282754838,-19.406124729225,40.10025));
#184023=CARTESIAN_POINT('',(-55.4168495715593,-17.9900016446779,40.10025));
#184024=CARTESIAN_POINT('',(-59.7658094374952,-19.4351129318417,40.10025));
#184025=CARTESIAN_POINT('Origin',(9.17194536069053E-17,4.54273045741979E-17,
40.10025));
#184026=CARTESIAN_POINT('',(-56.1347810195643,-18.2553202812746,40.10025));
#184027=CARTESIAN_POINT('',(-56.0675384271754,-18.2334718385816,40.10025));
#184028=CARTESIAN_POINT('Origin',(3.21290464935061E-16,-2.36524679281224E-17,
40.10025));
#184029=CARTESIAN_POINT('Origin',(0.0588677374284264,-0.181176266354227,
-8.28957270027842E-18));
#184030=CARTESIAN_POINT('',(-57.0080331356323,-18.7233363629821,39.116));
#184031=CARTESIAN_POINT('',(-56.5983041910847,-18.5902073587819,39.3548010137695));
#184032=CARTESIAN_POINT('Origin',(-56.9716732729182,-18.711522327434,39.5550297832862));
#184033=CARTESIAN_POINT('',(-56.2594439785882,-18.4801050009132,39.92499));
#184034=CARTESIAN_POINT('',(-56.5983041910847,-18.5902073587819,39.3548010137695));
#184035=CARTESIAN_POINT('',(-59.5312589135997,-19.5431821162863,39.92499));
#184036=CARTESIAN_POINT('',(-59.778330355405,-19.6234604941055,39.92499));
#184037=CARTESIAN_POINT('',(-59.1923991668986,-19.4330799109589,39.3548010137695));
#184038=CARTESIAN_POINT('',(-59.5312589135997,-19.5431821162863,39.92499));
#184039=CARTESIAN_POINT('',(-58.7826706420789,-19.2999510425003,39.116));
#184040=CARTESIAN_POINT('Origin',(-58.8190306219019,-19.3117651160994,39.5550293907208));
#184041=CARTESIAN_POINT('',(-58.4009360126569,-19.1759179434153,39.116));
#184042=CARTESIAN_POINT('',(0.0588677374284319,-0.181176266354227,39.116));
#184043=CARTESIAN_POINT('',(-58.2810665285031,-19.136969986288,39.3343017080178));
#184044=CARTESIAN_POINT('',(-58.4009360128768,-19.1759179427383,39.116));
#184045=CARTESIAN_POINT('',(-57.9672558039533,-19.0350067009927,39.5248017080178));
#184046=CARTESIAN_POINT('Origin',(-57.9952431000167,-19.0440997849308,39.1947747614299));
#184047=CARTESIAN_POINT('',(-57.823448340224,-18.9882808235617,39.5248017080178));
#184048=CARTESIAN_POINT('',(0.0588677374284319,-0.181176266354227,39.5248017080178));
#184049=CARTESIAN_POINT('',(-57.5096375484038,-18.8863175164089,39.3343017080178));
#184050=CARTESIAN_POINT('Origin',(-57.7954585952486,-18.9791858642781,39.1947728911906));
#184051=CARTESIAN_POINT('',(-57.3897680139785,-18.8473695436959,39.116));
#184052=CARTESIAN_POINT('',(-57.5096375484038,-18.8863175164089,39.3343017080178));
#184053=CARTESIAN_POINT('',(0.0588677374284319,-0.181176266354227,39.116));
#184054=CARTESIAN_POINT('Origin',(-0.0588677374284264,0.181176266354227,
8.28957270027842E-18));
#184055=CARTESIAN_POINT('',(-58.9004061169358,-18.9375985097918,39.116));
#184056=CARTESIAN_POINT('',(-59.3101346419425,-19.0707273776749,39.3548010137695));
#184057=CARTESIAN_POINT('Origin',(-58.9367660964857,-18.9494125833022,39.555029391244));
#184058=CARTESIAN_POINT('',(-59.6489943885963,-19.1808295831477,39.92499));
#184059=CARTESIAN_POINT('',(-59.3101346419425,-19.0707273776749,39.3548010137695));
#184060=CARTESIAN_POINT('',(-56.3771794532808,-18.1177524687103,39.92499));
#184061=CARTESIAN_POINT('',(-0.0588677374284154,0.181176266354229,39.92499));
#184062=CARTESIAN_POINT('',(-56.7160396657231,-18.2278548267456,39.3548010137695));
#184063=CARTESIAN_POINT('',(-56.3771794532808,-18.1177524687103,39.92499));
#184064=CARTESIAN_POINT('',(-57.1257686104892,-18.3609838302737,39.116));
#184065=CARTESIAN_POINT('Origin',(-57.0894087474847,-18.3491697946312,39.555029782729));
#184066=CARTESIAN_POINT('',(-57.5075034886062,-18.4850170116927,39.116));
#184067=CARTESIAN_POINT('',(-57.57774650121,-18.5078403492306,39.116));
#184068=CARTESIAN_POINT('',(-57.6273730232606,-18.5239649837004,39.3343017080178));
#184069=CARTESIAN_POINT('',(-57.5075034888354,-18.4850170109874,39.116));
#184070=CARTESIAN_POINT('',(-57.9411838150808,-18.6259282908533,39.5248017080178));
#184071=CARTESIAN_POINT('Origin',(-57.913196576314,-18.6168352256579,39.1947745585584));
#184072=CARTESIAN_POINT('',(-58.0849912788101,-18.6726541682842,39.5248017080178));
#184073=CARTESIAN_POINT('',(-58.0854941128252,-18.6728175489597,39.5248017080178));
#184074=CARTESIAN_POINT('',(-58.3988020033599,-18.7746174535796,39.3343017080178));
#184075=CARTESIAN_POINT('Origin',(-58.1129809527835,-18.6817491043774,39.1947728594267));
#184076=CARTESIAN_POINT('',(-58.5186714877337,-18.8135654100299,39.116));
#184077=CARTESIAN_POINT('',(-58.3988020033599,-18.7746174535796,39.3343017080178));
#184078=CARTESIAN_POINT('',(-58.900901982832,-18.9377596263882,39.116));
#184079=CARTESIAN_POINT('Origin',(-56.9509617460775,-12.3000564958686,40.10025));
#184080=CARTESIAN_POINT('',(-57.7418065394567,-12.2578193919764,40.10025));
#184081=CARTESIAN_POINT('',(-61.4762657165316,-13.0516031943525,40.10025));
#184082=CARTESIAN_POINT('',(-56.9937374973464,-12.0988124084936,40.10025));
#184083=CARTESIAN_POINT('',(-61.4699285681955,-13.0814171332228,40.10025));
#184084=CARTESIAN_POINT('Origin',(9.57020013840216E-17,3.05642339264188E-17,
40.10025));
#184085=CARTESIAN_POINT('',(-57.7354693911205,-12.2876333308468,40.10025));
#184086=CARTESIAN_POINT('',(-57.6663113765489,-12.2729333410575,40.10025));
#184087=CARTESIAN_POINT('Origin',(3.19216886402203E-16,-1.59137674900232E-17,
40.10025));
#184088=CARTESIAN_POINT('Origin',(0.039607177100782,-0.18633711793979,-5.57736016997301E-18));
#184089=CARTESIAN_POINT('',(-58.6528587425323,-12.6618058697516,39.116));
#184090=CARTESIAN_POINT('',(-58.2314585657881,-12.5722344970957,39.3548010137695));
#184091=CARTESIAN_POINT('Origin',(-58.6154631599693,-12.6538571933003,39.5550297832852));
#184092=CARTESIAN_POINT('',(-57.882945834721,-12.4981558287388,39.92499));
#184093=CARTESIAN_POINT('',(-58.2314585657881,-12.5722344970957,39.3548010137695));
#184094=CARTESIAN_POINT('',(-61.2479592423879,-13.213411509189,39.92499));
#184095=CARTESIAN_POINT('',(-61.5020685764505,-13.2674241155256,39.92499));
#184096=CARTESIAN_POINT('',(-60.8994469905094,-13.1393329438486,39.3548010137695));
#184097=CARTESIAN_POINT('',(-61.2479592423878,-13.213411509189,39.92499));
#184098=CARTESIAN_POINT('',(-60.4780472453828,-13.0497616623171,39.116));
#184099=CARTESIAN_POINT('Origin',(-60.5154429483886,-13.0577103643693,39.5550293907236));
#184100=CARTESIAN_POINT('',(-60.0854388089606,-12.966310163716,39.116));
#184101=CARTESIAN_POINT('',(0.0396071771007875,-0.18633711793979,39.116));
#184102=CARTESIAN_POINT('',(-59.9621548122772,-12.9401053405446,39.3343017080178));
#184103=CARTESIAN_POINT('',(-60.0854388091086,-12.96631016302,39.116));
#184104=CARTESIAN_POINT('',(-59.6394051101894,-12.8715027735888,39.5248017080178));
#184105=CARTESIAN_POINT('Origin',(-59.6681895750049,-12.8776205756127,39.1947747614269));
#184106=CARTESIAN_POINT('',(-59.4915012546306,-12.8400648385935,39.5248017080178));
#184107=CARTESIAN_POINT('',(0.0396071771007876,-0.18633711793979,39.5248017080178));
#184108=CARTESIAN_POINT('',(-59.1687514833561,-12.7714622569316,39.3343017080178));
#184109=CARTESIAN_POINT('Origin',(-59.4627141582876,-12.8339454274776,39.1947728911936));
#184110=CARTESIAN_POINT('',(-59.0454674350475,-12.7452574235144,39.116));
#184111=CARTESIAN_POINT('',(-59.1687514833561,-12.7714622569316,39.3343017080178));
#184112=CARTESIAN_POINT('',(0.0396071771007875,-0.18633711793979,39.116));
#184113=CARTESIAN_POINT('Origin',(-0.039607177100782,0.18633711793979,5.57736016997301E-18));
#184114=CARTESIAN_POINT('',(-60.5572615995844,-12.6770874264375,39.116));
#184115=CARTESIAN_POINT('',(-60.9786613448368,-12.766658707377,39.3548010137695));
#184116=CARTESIAN_POINT('Origin',(-60.5946573023114,-12.6850361284304,39.5550293912429));
#184117=CARTESIAN_POINT('',(-61.3271735966834,-12.8407372728674,39.92499));
#184118=CARTESIAN_POINT('',(-60.9786613448368,-12.766658707377,39.3548010137695));
#184119=CARTESIAN_POINT('',(-57.9621601888121,-12.1254815933788,39.92499));
#184120=CARTESIAN_POINT('',(-0.0396071771007709,0.186337117939791,39.92499));
#184121=CARTESIAN_POINT('',(-58.3106729198427,-12.1995602619073,39.3548010137695));
#184122=CARTESIAN_POINT('',(-57.9621601888121,-12.1254815933788,39.92499));
#184123=CARTESIAN_POINT('',(-58.7320730967339,-12.289131633872,39.116));
#184124=CARTESIAN_POINT('Origin',(-58.6946775138732,-12.2811829573575,39.5550297827297));
#184125=CARTESIAN_POINT('',(-59.1246817890949,-12.3725831883604,39.116));
#184126=CARTESIAN_POINT('',(-59.1969256915255,-12.3879391031043,39.116));
#184127=CARTESIAN_POINT('',(-59.2479658375577,-12.398788021052,39.3343017080178));
#184128=CARTESIAN_POINT('',(-59.1246817892491,-12.3725831876348,39.116));
#184129=CARTESIAN_POINT('',(-59.5707156088321,-12.4673906027139,39.5248017080178));
#184130=CARTESIAN_POINT('Origin',(-59.5419312029551,-12.4612728133403,39.19477455856));
#184131=CARTESIAN_POINT('',(-59.718619464391,-12.4988285377092,39.5248017080178));
#184132=CARTESIAN_POINT('',(-59.7191366217597,-12.4989384629014,39.5248017080178));
#184133=CARTESIAN_POINT('',(-60.0413691664788,-12.567431104665,39.3343017080178));
#184134=CARTESIAN_POINT('Origin',(-59.7474064876957,-12.5049479331832,39.1947728594283));
#184135=CARTESIAN_POINT('',(-60.1646531633101,-12.5936359271404,39.116));
#184136=CARTESIAN_POINT('',(-60.0413691664788,-12.567431104665,39.3343017080178));
#184137=CARTESIAN_POINT('',(-60.5577715903455,-12.6771958283202,39.116));
#184138=CARTESIAN_POINT('Origin',(-57.9246844223735,-6.27967898647569,40.10025));
#184139=CARTESIAN_POINT('',(-58.7067819056643,-6.15500747092277,40.10025));
#184140=CARTESIAN_POINT('',(-62.5037563256535,-6.55408556365905,40.10025));
#184141=CARTESIAN_POINT('',(-57.9461901084062,-6.07506605172262,40.10025));
#184142=CARTESIAN_POINT('',(-62.5005702980931,-6.58439859102987,40.10025));
#184143=CARTESIAN_POINT('Origin',(9.81091184134694E-17,1.53662951357646E-17,
40.10025));
#184144=CARTESIAN_POINT('',(-58.7035958781039,-6.1853204982936,40.10025));
#184145=CARTESIAN_POINT('',(-58.6332801510296,-6.1779300175723,40.10025));
#184146=CARTESIAN_POINT('Origin',(3.17963581613999E-16,-8.00071248513326E-18,
40.10025));
#184147=CARTESIAN_POINT('Origin',(0.0199126722524868,-0.189456421067656,
-2.80404091450773E-18));
#184148=CARTESIAN_POINT('',(-59.6550713551493,-6.46154998175879,39.116));
#184149=CARTESIAN_POINT('',(-59.2266168947286,-6.41651760335012,39.3548010137695));
#184150=CARTESIAN_POINT('Origin',(-59.6170497665656,-6.45755375176711,39.5550297832845));
#184151=CARTESIAN_POINT('',(-58.8722700235037,-6.3792742458964,39.92499));
#184152=CARTESIAN_POINT('',(-59.2266168947286,-6.41651760335012,39.3548010137695));
#184153=CARTESIAN_POINT('',(-62.293614112757,-6.73887200051292,39.92499));
#184154=CARTESIAN_POINT('',(-62.5519772640372,-6.76602706194906,39.92499));
#184155=CARTESIAN_POINT('',(-61.9392677288637,-6.70162869542303,39.3548010137695));
#184156=CARTESIAN_POINT('',(-62.293614112757,-6.73887200051292,39.92499));
#184157=CARTESIAN_POINT('',(-61.5108137072212,-6.65659636252343,39.116));
#184158=CARTESIAN_POINT('Origin',(-61.5488354182644,-6.66059260538611,39.5550293907221));
#184159=CARTESIAN_POINT('',(-61.1116329639869,-6.61464077648877,39.116));
#184160=CARTESIAN_POINT('',(0.0199126722524923,-0.189456421067656,39.116));
#184161=CARTESIAN_POINT('',(-60.9862851800405,-6.60146619279907,39.3343017080178));
#184162=CARTESIAN_POINT('',(-61.1116329640613,-6.61464077578082,39.116));
#184163=CARTESIAN_POINT('',(-60.6581326136904,-6.56697596826238,39.5248017080178));
#184164=CARTESIAN_POINT('Origin',(-60.6873988786444,-6.57005146045401,39.1947747614342));
#184165=CARTESIAN_POINT('',(-60.5077528318944,-6.55117041629729,39.5248017080178));
#184166=CARTESIAN_POINT('',(0.0199126722524923,-0.189456421067656,39.5248017080178));
#184167=CARTESIAN_POINT('',(-60.1796001951996,-6.51668018436707,39.3343017080178));
#184168=CARTESIAN_POINT('Origin',(-60.4784837816391,-6.54809359889867,39.1947728911901));
#184169=CARTESIAN_POINT('',(-60.0542523588397,-6.50350559588426,39.116));
#184170=CARTESIAN_POINT('',(-60.1796001951996,-6.51668018436707,39.3343017080178));
#184171=CARTESIAN_POINT('',(0.0199126722524923,-0.189456421067656,39.116));
#184172=CARTESIAN_POINT('Origin',(-0.0199126722524868,0.189456421067656,
2.80404091450773E-18));
#184173=CARTESIAN_POINT('',(-61.5506390517262,-6.27768352038812,39.116));
#184174=CARTESIAN_POINT('',(-61.9790930734319,-6.322715852686,39.3548010137695));
#184175=CARTESIAN_POINT('Origin',(-61.5886607624846,-6.28167976322088,39.555029391244));
#184176=CARTESIAN_POINT('',(-62.3334394573092,-6.35995915792788,39.92499));
#184177=CARTESIAN_POINT('',(-61.9790930734319,-6.322715852686,39.3548010137695));
#184178=CARTESIAN_POINT('',(-58.9120953679531,-6.00036140429008,39.92499));
#184179=CARTESIAN_POINT('',(-0.0199126722524756,0.189456421067657,39.92499));
#184180=CARTESIAN_POINT('',(-59.2664422391598,-6.03760476191742,39.3548010137695));
#184181=CARTESIAN_POINT('',(-58.912095367953,-6.00036140429008,39.92499));
#184182=CARTESIAN_POINT('',(-59.6948966996543,-6.08263713962348,39.116));
#184183=CARTESIAN_POINT('Origin',(-59.6568751107679,-6.07864090959999,39.5550297827291));
#184184=CARTESIAN_POINT('',(-60.0940777032672,-6.12459275448644,39.116));
#184185=CARTESIAN_POINT('',(-60.1675309762115,-6.13231300382137,39.116));
#184186=CARTESIAN_POINT('',(-60.2194255397045,-6.13776734223176,39.3343017080178));
#184187=CARTESIAN_POINT('',(-60.0940777033447,-6.12459275374895,39.116));
#184188=CARTESIAN_POINT('',(-60.5475781763994,-6.17225757416198,39.5248017080178));
#184189=CARTESIAN_POINT('Origin',(-60.5183119713893,-6.16918208839119,39.1947745585571));
#184190=CARTESIAN_POINT('',(-60.6979579581954,-6.18806312612707,39.5248017080178));
#184191=CARTESIAN_POINT('',(-60.6984837728333,-6.18811839147248,39.5248017080178));
#184192=CARTESIAN_POINT('',(-61.0261105245454,-6.22255335066375,39.3343017080178));
#184193=CARTESIAN_POINT('Origin',(-60.7272269341776,-6.19113993560405,39.1947728594259));
#184194=CARTESIAN_POINT('',(-61.1514583085663,-6.23572793364551,39.116));
#184195=CARTESIAN_POINT('',(-61.0261105245454,-6.22255335066375,39.3343017080178));
#184196=CARTESIAN_POINT('',(-61.5511575797868,-6.27773801988339,39.116));
#184197=CARTESIAN_POINT('Origin',(-58.2637721346185,-0.1905,40.10025));
#184198=CARTESIAN_POINT('',(-58.2637721346185,0.01524,40.10025));
#184199=CARTESIAN_POINT('',(-58.9578504383728,-0.01524,40.10025));
#184200=CARTESIAN_POINT('Origin',(0.,-0.1905,0.));
#184201=CARTESIAN_POINT('',(-60.0036905223731,-0.1905,39.116));
#184202=CARTESIAN_POINT('',(-59.5728760150042,-0.1905,39.3548010137695));
#184203=CARTESIAN_POINT('Origin',(-59.9654595002513,-0.1905,39.5550297832875));
#184204=CARTESIAN_POINT('',(-59.2165773020941,-0.190499999468477,39.92499));
#184205=CARTESIAN_POINT('',(-59.5728760150042,-0.1905,39.3548010137695));
#184206=CARTESIAN_POINT('',(-62.6567671111299,-0.190499999999999,39.92499));
#184207=CARTESIAN_POINT('',(-62.9165533988763,-0.1905,39.92499));
#184208=CARTESIAN_POINT('',(-62.3004688883554,-0.190500000605399,39.3548010137695));
#184209=CARTESIAN_POINT('',(-62.6567671111299,-0.1905,39.92499));
#184210=CARTESIAN_POINT('',(-61.8696548221181,-0.1905,39.116));
#184211=CARTESIAN_POINT('Origin',(-61.9078859673759,-0.1905,39.5550293907204));
#184212=CARTESIAN_POINT('',(-61.4682752798284,-0.190500000712027,39.116));
#184213=CARTESIAN_POINT('',(5.50819412990574E-15,-0.1905,39.116));
#184214=CARTESIAN_POINT('',(-61.3422370451705,-0.1905,39.3343017080178));
#184215=CARTESIAN_POINT('',(-61.4682752798284,-0.1905,39.116));
#184216=CARTESIAN_POINT('',(-61.0122769227456,-0.1905,39.5248017080178));
#184217=CARTESIAN_POINT('Origin',(-61.04170434051,-0.190499486622401,39.1947747614337));
#184218=CARTESIAN_POINT('',(-60.8610688070707,-0.1905,39.5248017080178));
#184219=CARTESIAN_POINT('',(5.56576032196012E-15,-0.1905,39.5248017080178));
#184220=CARTESIAN_POINT('',(-60.5311086139135,-0.1905,39.3343017080178));
#184221=CARTESIAN_POINT('Origin',(-60.8316384807414,-0.190499486573508,
39.1947728911889));
#184222=CARTESIAN_POINT('',(-60.4050703266282,-0.1905,39.116));
#184223=CARTESIAN_POINT('',(-60.5311086139135,-0.1905,39.3343017080178));
#184224=CARTESIAN_POINT('',(5.50819412990574E-15,-0.1905,39.116));
#184225=CARTESIAN_POINT('Origin',(0.,0.1905,0.));
#184226=CARTESIAN_POINT('',(-61.8696548221181,0.1905,39.116));
#184227=CARTESIAN_POINT('',(-62.3004688883554,0.190500000000001,39.3548010137695));
#184228=CARTESIAN_POINT('Origin',(-61.9078859670881,0.1905,39.5550293912456));
#184229=CARTESIAN_POINT('',(-62.6567671111299,0.190500000452307,39.92499));
#184230=CARTESIAN_POINT('',(-62.3004688883554,0.1905,39.3548010137695));
#184231=CARTESIAN_POINT('',(-59.2165773020941,0.1905,39.92499));
#184232=CARTESIAN_POINT('',(1.12442271988212E-14,0.1905,39.92499));
#184233=CARTESIAN_POINT('',(-59.5728760150042,0.190499999293399,39.3548010137695));
#184234=CARTESIAN_POINT('',(-59.2165773020941,0.1905,39.92499));
#184235=CARTESIAN_POINT('',(-60.003690522373,0.1905,39.116));
#184236=CARTESIAN_POINT('Origin',(-59.9654594999476,0.1905,39.5550297827329));
#184237=CARTESIAN_POINT('',(-60.4050703266283,0.190499999257743,39.116));
#184238=CARTESIAN_POINT('',(-60.4789282006568,0.1905,39.116));
#184239=CARTESIAN_POINT('',(-60.5311086139135,0.1905,39.3343017080178));
#184240=CARTESIAN_POINT('',(-60.4050703266282,0.1905,39.116));
#184241=CARTESIAN_POINT('',(-60.8610688070707,0.1905,39.5248017080178));
#184242=CARTESIAN_POINT('Origin',(-60.8316414495934,0.190499486502559,39.1947745585556));
#184243=CARTESIAN_POINT('',(-61.0122769227456,0.1905,39.5248017080178));
#184244=CARTESIAN_POINT('',(-61.0128056337175,0.1905,39.5248017080178));
#184245=CARTESIAN_POINT('',(-61.3422370451705,0.1905,39.3343017080178));
#184246=CARTESIAN_POINT('Origin',(-61.0417071743819,0.190499486688105,39.1947728594266));
#184247=CARTESIAN_POINT('',(-61.4682752798284,0.1905,39.116));
#184248=CARTESIAN_POINT('',(-61.3422370451705,0.1905,39.3343017080178));
#184249=CARTESIAN_POINT('',(-61.8701762063762,0.1905,39.116));
#184250=CARTESIAN_POINT('Origin',(-57.9645097668784,5.90076614434116,40.10025));
#184251=CARTESIAN_POINT('',(-58.7035958781038,6.18532049829439,40.10025));
#184252=CARTESIAN_POINT('',(-62.500570298093,6.58439859103072,40.10025));
#184253=CARTESIAN_POINT('',(-57.9430040808457,6.10537907909423,40.10025));
#184254=CARTESIAN_POINT('',(-62.5037563256534,6.55408556365989,40.10025));
#184255=CARTESIAN_POINT('Origin',(9.81091184134687E-17,-1.53662951357666E-17,
40.10025));
#184256=CARTESIAN_POINT('',(-58.7067819056642,6.15500747092357,40.10025));
#184257=CARTESIAN_POINT('',(-58.6364661785899,6.14761699020227,40.10025));
#184258=CARTESIAN_POINT('Origin',(3.17963581613999E-16,8.00071248513429E-18,
40.10025));
#184259=CARTESIAN_POINT('Origin',(-0.0199126722524893,-0.189456421067656,
2.8040409145081E-18));
#184260=CARTESIAN_POINT('',(-59.6948966996542,6.08263713962429,39.116));
#184261=CARTESIAN_POINT('',(-59.2664422392335,6.03760476121561,39.3548010137695));
#184262=CARTESIAN_POINT('Origin',(-59.6568751110713,6.0786409096327,39.5550297832861));
#184263=CARTESIAN_POINT('',(-58.9120953678974,6.00036140481904,39.92499));
#184264=CARTESIAN_POINT('',(-59.2664422392335,6.03760476121561,39.3548010137695));
#184265=CARTESIAN_POINT('',(-62.3334394572618,6.35995915837845,39.92499));
#184266=CARTESIAN_POINT('',(-62.5918026085421,6.38711421981459,39.92499));
#184267=CARTESIAN_POINT('',(-61.9790930734951,6.322715852085,39.3548010137695));
#184268=CARTESIAN_POINT('',(-62.3334394572618,6.35995915837845,39.92499));
#184269=CARTESIAN_POINT('',(-61.5506390517261,6.27768352038895,39.116));
#184270=CARTESIAN_POINT('Origin',(-61.5886607627699,6.2816797632517,39.5550293907212));
#184271=CARTESIAN_POINT('',(-61.1514583086406,6.23572793293842,39.116));
#184272=CARTESIAN_POINT('',(-0.0199126722524838,-0.189456421067656,39.116));
#184273=CARTESIAN_POINT('',(-61.0261105245453,6.22255335066458,39.3343017080178));
#184274=CARTESIAN_POINT('',(-61.1514583085662,6.23572793364634,39.116));
#184275=CARTESIAN_POINT('',(-60.6979579581953,6.18806312612789,39.5248017080178));
#184276=CARTESIAN_POINT('Origin',(-60.7272241158223,6.19113963944987,39.1947747614314));
#184277=CARTESIAN_POINT('',(-60.5475781763993,6.1722575741628,39.5248017080178));
#184278=CARTESIAN_POINT('',(-0.0199126722524838,-0.189456421067656,39.5248017080178));
#184279=CARTESIAN_POINT('',(-60.2194255397045,6.13776734223257,39.3343017080178));
#184280=CARTESIAN_POINT('Origin',(-60.518309018805,6.16918177799158,39.1947728911969));
#184281=CARTESIAN_POINT('',(-60.0940777033446,6.12459275374976,39.116));
#184282=CARTESIAN_POINT('',(-60.2194255397045,6.13776734223257,39.3343017080178));
#184283=CARTESIAN_POINT('',(-0.0199126722524838,-0.189456421067656,39.116));
#184284=CARTESIAN_POINT('Origin',(0.0199126722524893,0.189456421067656,
-2.8040409145081E-18));
#184285=CARTESIAN_POINT('',(-61.5108137072212,6.65659636252426,39.116));
#184286=CARTESIAN_POINT('',(-61.9392677289269,6.70162869482215,39.3548010137695));
#184287=CARTESIAN_POINT('Origin',(-61.5488354179797,6.66059260535702,39.555029391244));
#184288=CARTESIAN_POINT('',(-62.2936141127096,6.73887200096387,39.92499));
#184289=CARTESIAN_POINT('',(-61.9392677289269,6.70162869482215,39.3548010137695));
#184290=CARTESIAN_POINT('',(-58.872270023448,6.37927424642618,39.92499));
#184291=CARTESIAN_POINT('',(0.0199126722525006,0.189456421067655,39.92499));
#184292=CARTESIAN_POINT('',(-59.2266168948024,6.4165176026483,39.3548010137695));
#184293=CARTESIAN_POINT('',(-58.872270023448,6.37927424642618,39.92499));
#184294=CARTESIAN_POINT('',(-59.6550713551492,6.4615499817596,39.116));
#184295=CARTESIAN_POINT('Origin',(-59.6170497662618,6.457553751736,39.5550297827272));
#184296=CARTESIAN_POINT('',(-60.0542523589172,6.50350559514732,39.116));
#184297=CARTESIAN_POINT('',(-60.1277056317064,6.5112258459575,39.116));
#184298=CARTESIAN_POINT('',(-60.1796001951995,6.51668018436788,39.3343017080178));
#184299=CARTESIAN_POINT('',(-60.0542523588397,6.50350559588507,39.116));
#184300=CARTESIAN_POINT('',(-60.5077528318943,6.55117041629811,39.5248017080178));
#184301=CARTESIAN_POINT('Origin',(-60.4784867342325,6.54809390915823,39.1947745585609));
#184302=CARTESIAN_POINT('',(-60.6581326136904,6.5669759682632,39.5248017080178));
#184303=CARTESIAN_POINT('',(-60.6586584283283,6.56703123360861,39.5248017080178));
#184304=CARTESIAN_POINT('',(-60.9862851800404,6.60146619279989,39.3343017080178));
#184305=CARTESIAN_POINT('Origin',(-60.6874016969804,6.57005175673997,39.1947728594192));
#184306=CARTESIAN_POINT('',(-61.1116329640612,6.61464077578165,39.116));
#184307=CARTESIAN_POINT('',(-60.9862851800404,6.60146619279989,39.3343017080178));
#184308=CARTESIAN_POINT('',(-61.5113322352818,6.65665086201954,39.116));
#184309=CARTESIAN_POINT('Origin',(-57.0301761002789,11.9273822599898,40.10025));
#184310=CARTESIAN_POINT('',(-57.7354693911204,12.2876333308475,40.10025));
#184311=CARTESIAN_POINT('',(-61.4699285681953,13.0814171332237,40.10025));
#184312=CARTESIAN_POINT('',(-56.9874003490101,12.1286263473648,40.10025));
#184313=CARTESIAN_POINT('',(-61.4762657165315,13.0516031943533,40.10025));
#184314=CARTESIAN_POINT('Origin',(9.5702001384024E-17,-3.05642339264207E-17,
40.10025));
#184315=CARTESIAN_POINT('',(-57.7418065394565,12.2578193919772,40.10025));
#184316=CARTESIAN_POINT('',(-57.6726485248849,12.2431194021879,40.10025));
#184317=CARTESIAN_POINT('Origin',(3.19216886402205E-16,1.59137674900242E-17,
40.10025));
#184318=CARTESIAN_POINT('Origin',(-0.0396071771007845,-0.18633711793979,
5.57736016997337E-18));
#184319=CARTESIAN_POINT('',(-58.7320730967337,12.2891316338728,39.116));
#184320=CARTESIAN_POINT('',(-58.3106729199895,12.1995602612169,39.3548010137695));
#184321=CARTESIAN_POINT('Origin',(-58.6946775141716,12.2811829574217,39.5550297832871));
#184322=CARTESIAN_POINT('',(-57.9621601887014,12.1254815938998,39.92499));
#184323=CARTESIAN_POINT('',(-58.3106729199895,12.1995602612169,39.3548010137695));
#184324=CARTESIAN_POINT('',(-61.3271735965892,12.8407372733103,39.92499));
#184325=CARTESIAN_POINT('',(-61.5812829306519,12.8947498796469,39.92499));
#184326=CARTESIAN_POINT('',(-60.9786613449624,12.7666587067861,39.3548010137695));
#184327=CARTESIAN_POINT('',(-61.3271735965892,12.8407372733103,39.92499));
#184328=CARTESIAN_POINT('',(-60.5572615995842,12.6770874264384,39.116));
#184329=CARTESIAN_POINT('Origin',(-60.594657302592,12.6850361284909,39.5550293907194));
#184330=CARTESIAN_POINT('',(-60.164653163458,12.5936359264449,39.116));
#184331=CARTESIAN_POINT('',(-0.039607177100779,-0.18633711793979,39.116));
#184332=CARTESIAN_POINT('',(-60.0413691664786,12.5674311046659,39.3343017080178));
#184333=CARTESIAN_POINT('',(-60.1646531633099,12.5936359271413,39.116));
#184334=CARTESIAN_POINT('',(-59.7186194643908,12.49882853771,39.5248017080178));
#184335=CARTESIAN_POINT('Origin',(-59.7474037157301,12.5049473440517,39.1947747614238));
#184336=CARTESIAN_POINT('',(-59.570715608832,12.4673906027147,39.5248017080178));
#184337=CARTESIAN_POINT('',(-0.0396071771007789,-0.18633711793979,39.5248017080178));
#184338=CARTESIAN_POINT('',(-59.2479658375575,12.3987880210528,39.3343017080178));
#184339=CARTESIAN_POINT('Origin',(-59.5419282989946,12.4612721960127,39.1947728911921));
#184340=CARTESIAN_POINT('',(-59.1246817892489,12.3725831876356,39.116));
#184341=CARTESIAN_POINT('',(-59.2479658375575,12.3987880210528,39.3343017080178));
#184342=CARTESIAN_POINT('',(-0.039607177100779,-0.18633711793979,39.116));
#184343=CARTESIAN_POINT('Origin',(0.0396071771007845,0.18633711793979,-5.57736016997337E-18));
#184344=CARTESIAN_POINT('',(-60.4780472453826,13.0497616623179,39.116));
#184345=CARTESIAN_POINT('',(-60.8994469906351,13.1393329432574,39.3548010137695));
#184346=CARTESIAN_POINT('Origin',(-60.5154429481093,13.0577103643107,39.5550293912437));
#184347=CARTESIAN_POINT('',(-61.2479592422936,13.2134115096323,39.92499));
#184348=CARTESIAN_POINT('',(-60.8994469906351,13.1393329432574,39.3548010137695));
#184349=CARTESIAN_POINT('',(-57.8829458346104,12.4981558292591,39.92499));
#184350=CARTESIAN_POINT('',(0.0396071771007956,0.186337117939789,39.92499));
#184351=CARTESIAN_POINT('',(-58.2314585659347,12.5722344964058,39.3548010137695));
#184352=CARTESIAN_POINT('',(-57.8829458346104,12.4981558292591,39.92499));
#184353=CARTESIAN_POINT('',(-58.6528587425321,12.6618058697524,39.116));
#184354=CARTESIAN_POINT('Origin',(-58.6154631596727,12.6538571932381,39.555029782732));
#184355=CARTESIAN_POINT('',(-59.0454674352016,12.7452574227896,39.116));
#184356=CARTESIAN_POINT('',(-59.1177113373237,12.7606133389847,39.116));
#184357=CARTESIAN_POINT('',(-59.168751483356,12.7714622569324,39.3343017080178));
#184358=CARTESIAN_POINT('',(-59.0454674350473,12.7452574235152,39.116));
#184359=CARTESIAN_POINT('',(-59.4915012546304,12.8400648385943,39.5248017080178));
#184360=CARTESIAN_POINT('Origin',(-59.4627170622777,12.8339460446681,39.1947745585593));
#184361=CARTESIAN_POINT('',(-59.6394051101892,12.8715027735896,39.5248017080178));
#184362=CARTESIAN_POINT('',(-59.6399222675579,12.8716126987817,39.5248017080178));
#184363=CARTESIAN_POINT('',(-59.962154812277,12.9401053405454,39.3343017080178));
#184364=CARTESIAN_POINT('Origin',(-59.6681923469416,12.8776211648741,39.19477285943));
#184365=CARTESIAN_POINT('',(-60.0854388091084,12.9663101630208,39.116));
#184366=CARTESIAN_POINT('',(-59.962154812277,12.9401053405454,39.3343017080178));
#184367=CARTESIAN_POINT('',(-60.4785572361438,13.0498700642006,39.116));
#184368=CARTESIAN_POINT('Origin',(-55.4710078899932,17.8233194796328,40.10025));
#184369=CARTESIAN_POINT('',(-56.1347810195641,18.2553202812753,40.10025));
#184370=CARTESIAN_POINT('',(-59.765809437495,19.4351129318425,40.10025));
#184371=CARTESIAN_POINT('',(-55.4074307335705,18.0189898472954,40.10025));
#184372=CARTESIAN_POINT('',(-59.7752282754835,19.4061247292258,40.10025));
#184373=CARTESIAN_POINT('Origin',(9.1719453606903E-17,-4.54273045741998E-17,
40.10025));
#184374=CARTESIAN_POINT('',(-56.1441998575526,18.2263320786586,40.10025));
#184375=CARTESIAN_POINT('',(-56.0769572651637,18.2044836359657,40.10025));
#184376=CARTESIAN_POINT('Origin',(3.2129046493506E-16,2.36524679281234E-17,
40.10025));
#184377=CARTESIAN_POINT('Origin',(-0.0588677374284288,-0.181176266354226,
8.28957270027876E-18));
#184378=CARTESIAN_POINT('',(-57.1257686104889,18.3609838302744,39.116));
#184379=CARTESIAN_POINT('',(-56.7160396659413,18.2278548260742,39.3548010137695));
#184380=CARTESIAN_POINT('Origin',(-57.0894087477764,18.3491697947268,39.5550297832891));
#184381=CARTESIAN_POINT('',(-56.3771794531162,18.1177524692168,39.92499));
#184382=CARTESIAN_POINT('',(-56.7160396659413,18.2278548260742,39.3548010137695));
#184383=CARTESIAN_POINT('',(-59.6489943884562,19.1808295835786,39.92499));
#184384=CARTESIAN_POINT('',(-59.8960658302616,19.2611079613979,39.92499));
#184385=CARTESIAN_POINT('',(-59.3101346421292,19.0707273771002,39.3548010137695));
#184386=CARTESIAN_POINT('',(-59.6489943884562,19.1808295835786,39.92499));
#184387=CARTESIAN_POINT('',(-58.9004061169356,18.9375985097926,39.116));
#184388=CARTESIAN_POINT('Origin',(-58.9367660967581,18.9494125833916,39.5550293907212));
#184389=CARTESIAN_POINT('',(-58.5186714879534,18.8135654093536,39.116));
#184390=CARTESIAN_POINT('',(-0.0588677374284233,-0.181176266354226,39.116));
#184391=CARTESIAN_POINT('',(-58.3988020033597,18.7746174535804,39.3343017080178));
#184392=CARTESIAN_POINT('',(-58.5186714877334,18.8135654100307,39.116));
#184393=CARTESIAN_POINT('',(-58.0849912788099,18.672654168285,39.5248017080178));
#184394=CARTESIAN_POINT('Origin',(-58.1129782575873,18.681748228725,39.1947747614283));
#184395=CARTESIAN_POINT('',(-57.9411838150806,18.6259282908541,39.5248017080178));
#184396=CARTESIAN_POINT('',(-0.0588677374284233,-0.181176266354226,39.5248017080178));
#184397=CARTESIAN_POINT('',(-57.6273730232604,18.5239649837012,39.3343017080178));
#184398=CARTESIAN_POINT('Origin',(-57.9131937527875,18.6168343081648,39.1947728911954));
#184399=CARTESIAN_POINT('',(-57.5075034888351,18.4850170109882,39.116));
#184400=CARTESIAN_POINT('',(-57.6273730232604,18.5239649837012,39.3343017080178));
#184401=CARTESIAN_POINT('',(-0.0588677374284233,-0.181176266354226,39.116));
#184402=CARTESIAN_POINT('Origin',(0.0588677374284288,0.181176266354226,
-8.28957270027876E-18));
#184403=CARTESIAN_POINT('',(-58.7826706420787,19.2999510425011,39.116));
#184404=CARTESIAN_POINT('',(-59.1923991670854,19.4330799103842,39.3548010137695));
#184405=CARTESIAN_POINT('Origin',(-58.8190306216277,19.3117651160112,39.5550293912458));
#184406=CARTESIAN_POINT('',(-59.5312589134596,19.5431821167172,39.92499));
#184407=CARTESIAN_POINT('',(-59.1923991670854,19.4330799103842,39.3548010137695));
#184408=CARTESIAN_POINT('',(-56.2594439784237,18.4801050014195,39.92499));
#184409=CARTESIAN_POINT('',(0.0588677374284398,0.181176266354225,39.92499));
#184410=CARTESIAN_POINT('',(-56.5983041913027,18.5902073581107,39.3548010137695));
#184411=CARTESIAN_POINT('',(-56.2594439784237,18.4801050014195,39.92499));
#184412=CARTESIAN_POINT('',(-57.0080331356321,18.7233363629829,39.116));
#184413=CARTESIAN_POINT('Origin',(-56.9716732726289,18.7115223273408,39.5550297827311));
#184414=CARTESIAN_POINT('',(-57.3897680142075,18.847369542991,39.116));
#184415=CARTESIAN_POINT('',(-57.4600110263529,18.8701928819399,39.116));
#184416=CARTESIAN_POINT('',(-57.5096375484035,18.8863175164097,39.3343017080178));
#184417=CARTESIAN_POINT('',(-57.3897680139783,18.8473695436966,39.116));
#184418=CARTESIAN_POINT('',(-57.8234483402237,18.9882808235625,39.5248017080178));
#184419=CARTESIAN_POINT('Origin',(-57.7954614188134,18.9791867816362,39.1947745585618));
#184420=CARTESIAN_POINT('',(-57.967255803953,19.0350067009935,39.5248017080178));
#184421=CARTESIAN_POINT('',(-57.9677586379681,19.0351700816689,39.5248017080178));
#184422=CARTESIAN_POINT('',(-58.2810665285028,19.1369699862888,39.3343017080178));
#184423=CARTESIAN_POINT('Origin',(-57.9952457951704,19.0441006607093,39.1947728594272));
#184424=CARTESIAN_POINT('',(-58.4009360128765,19.1759179427391,39.116));
#184425=CARTESIAN_POINT('',(-58.2810665285028,19.1369699862888,39.3343017080178));
#184426=CARTESIAN_POINT('',(-58.7831665079749,19.3001121590974,39.116));
#184427=CARTESIAN_POINT('Origin',(-53.30408770921,23.5239806812876,40.10025));
#184428=CARTESIAN_POINT('',(-53.9190682401993,24.0229981225301,40.10025));
#184429=CARTESIAN_POINT('',(-57.4068835917977,25.5758735661212,40.10025));
#184430=CARTESIAN_POINT('',(-53.2204057122636,23.7119335237429,40.10025));
#184431=CARTESIAN_POINT('',(-57.4192809246787,25.5480287005723,40.10025));
#184432=CARTESIAN_POINT('Origin',(8.62051087089599E-17,-5.97926641667894E-17,
40.10025));
#184433=CARTESIAN_POINT('',(-53.9314655730802,23.9951532569811,40.10025));
#184434=CARTESIAN_POINT('',(-53.8668751267876,23.9663957374948,40.10025));
#184435=CARTESIAN_POINT('Origin',(3.24161598652236E-16,3.1132026978005E-17,
40.10025));
#184436=CARTESIAN_POINT('Origin',(-0.0774833305059413,-0.174030409680915,
1.09109629373753E-17));
#184437=CARTESIAN_POINT('',(-54.893582249012,24.2316692455487,39.116));
#184438=CARTESIAN_POINT('',(-54.5000136127187,24.0564411990331,39.3548010137695));
#184439=CARTESIAN_POINT('Origin',(-54.8586564724104,24.216119287949,39.5550297832847));
#184440=CARTESIAN_POINT('',(-54.1745185417597,23.9115214570974,39.92499));
#184441=CARTESIAN_POINT('',(-54.5000136127187,24.0564411990331,39.3548010137695));
#184442=CARTESIAN_POINT('',(-57.3172883154488,25.3107727110827,39.92499));
#184443=CARTESIAN_POINT('',(-57.5546148985774,25.4164373136778,39.92499));
#184444=CARTESIAN_POINT('',(-56.991793692713,25.1658531674651,39.3548010137695));
#184445=CARTESIAN_POINT('',(-57.3172883154488,25.3107727110827,39.92499));
#184446=CARTESIAN_POINT('',(-56.5982254591674,24.9906253009263,39.116));
#184447=CARTESIAN_POINT('Origin',(-56.6331513482564,25.0061753086086,39.5550293907245));
#184448=CARTESIAN_POINT('',(-56.2315470018074,24.8273695326461,39.116));
#184449=CARTESIAN_POINT('',(-0.0774833305059357,-0.174030409680915,39.116));
#184450=CARTESIAN_POINT('',(-56.116405344757,24.7761051648322,39.3343017080178));
#184451=CARTESIAN_POINT('',(-56.231547001518,24.8273695332961,39.116));
#184452=CARTESIAN_POINT('',(-55.8149717737125,24.6418982922882,39.5248017080178));
#184453=CARTESIAN_POINT('Origin',(-55.8418548487323,24.653867970398,39.1947747614342));
#184454=CARTESIAN_POINT('',(-55.676836286479,24.5803964109127,39.5248017080178));
#184455=CARTESIAN_POINT('',(-0.0774833305059357,-0.174030409680915,39.5248017080178));
#184456=CARTESIAN_POINT('',(-55.3754026508173,24.4461895095993,39.3343017080178));
#184457=CARTESIAN_POINT('Origin',(-55.6499501367158,24.5684264878159,39.1947728911866));
#184458=CARTESIAN_POINT('',(-55.2602609459789,24.3949251197299,39.116));
#184459=CARTESIAN_POINT('',(-55.3754026508173,24.4461895095993,39.3343017080178));
#184460=CARTESIAN_POINT('',(-0.0774833305059357,-0.174030409680915,39.116));
#184461=CARTESIAN_POINT('Origin',(0.0774833305059413,0.174030409680915,
-1.09109629373753E-17));
#184462=CARTESIAN_POINT('',(-56.4432587981555,25.3386861202881,39.116));
#184463=CARTESIAN_POINT('',(-56.8368270314552,25.5139139873794,39.3548010137695));
#184464=CARTESIAN_POINT('Origin',(-56.4781846869828,25.354236127854,39.5550293912465));
#184465=CARTESIAN_POINT('',(-57.162321654253,25.6588335308577,39.92499));
#184466=CARTESIAN_POINT('',(-56.8368270314552,25.5139139873794,39.3548010137695));
#184467=CARTESIAN_POINT('',(-54.0195518809639,24.2595822759737,39.92499));
#184468=CARTESIAN_POINT('',(0.077483330505952,0.174030409680913,39.92499));
#184469=CARTESIAN_POINT('',(-54.3450469519945,24.4045020177487,39.3548010137695));
#184470=CARTESIAN_POINT('',(-54.0195518809639,24.2595822759737,39.92499));
#184471=CARTESIAN_POINT('',(-54.7386155880002,24.5797300649105,39.116));
#184472=CARTESIAN_POINT('Origin',(-54.7036898111205,24.564180107187,39.5550297827293));
#184473=CARTESIAN_POINT('',(-55.1052942852684,24.7429859384148,39.116));
#184474=CARTESIAN_POINT('',(-55.1727668102969,24.7730266428388,39.116));
#184475=CARTESIAN_POINT('',(-55.2204359898054,24.7942503289612,39.3343017080178));
#184476=CARTESIAN_POINT('',(-55.105294284967,24.7429859390917,39.116));
#184477=CARTESIAN_POINT('',(-55.5218696254671,24.9284572302746,39.5248017080178));
#184478=CARTESIAN_POINT('Origin',(-55.4949866055697,24.9164875765756,39.1947745585588));
#184479=CARTESIAN_POINT('',(-55.6600051127006,24.98995911165,39.5248017080178));
#184480=CARTESIAN_POINT('',(-55.6604881142074,24.9901741577759,39.5248017080178));
#184481=CARTESIAN_POINT('',(-55.9614386837451,25.124165984194,39.3343017080178));
#184482=CARTESIAN_POINT('Origin',(-55.6868911941801,25.0019290044704,39.1947728594209));
#184483=CARTESIAN_POINT('',(-56.0765803405061,25.1754303526579,39.116));
#184484=CARTESIAN_POINT('',(-55.9614386837451,25.124165984194,39.3343017080178));
#184485=CARTESIAN_POINT('',(-56.4437351063762,25.338898186371,39.116));
#184486=CARTESIAN_POINT('Origin',(-50.5531567888873,28.9669082278887,40.10025));
#184487=CARTESIAN_POINT('',(-51.1126068659045,29.5274749692189,40.10025));
#184488=CARTESIAN_POINT('',(-54.4189959163061,31.4364195775139,40.10025));
#184489=CARTESIAN_POINT('',(-50.4502867888873,29.1450842944633,40.10025));
#184490=CARTESIAN_POINT('',(-54.434235916306,31.4100231232066,40.10025));
#184491=CARTESIAN_POINT('Origin',(7.92193830068374E-17,-7.35029228183484E-17,
40.10025));
#184492=CARTESIAN_POINT('',(-51.1278468659044,29.5010785149116,40.10025));
#184493=CARTESIAN_POINT('',(-51.0666162321541,29.4657269920332,40.10025));
#184494=CARTESIAN_POINT('Origin',(3.27798830811898E-16,3.82704970255201E-17,
40.10025));
#184495=CARTESIAN_POINT('Origin',(-0.0952500000000014,-0.164977839420935,
1.34128103812642E-17));
#184496=CARTESIAN_POINT('',(-52.0599703131944,29.836867421766,39.116));
#184497=CARTESIAN_POINT('',(-51.686874005494,29.6214601680816,39.3548010137695));
#184498=CARTESIAN_POINT('Origin',(-52.0268612768248,29.8177519107055,39.5550297832886));
#184499=CARTESIAN_POINT('',(-51.3783102685123,29.4433108120871,39.92499));
#184500=CARTESIAN_POINT('',(-51.686874005494,29.6214601680816,39.3548010137695));
#184501=CARTESIAN_POINT('',(-54.3576020372436,31.1634057161445,39.92499));
#184502=CARTESIAN_POINT('',(-54.5825835619868,31.2932988600177,39.92499));
#184503=CARTESIAN_POINT('',(-54.0490387253,30.9852566042336,39.3548010137695));
#184504=CARTESIAN_POINT('',(-54.3576020372436,31.1634057161445,39.92499));
#184505=CARTESIAN_POINT('',(-53.6759427993284,30.7698495716385,39.116));
#184506=CARTESIAN_POINT('Origin',(-53.7090519423364,30.7889651442668,39.5550293907229));
#184507=CARTESIAN_POINT('',(-53.328337919502,30.5691597998774,39.116));
#184508=CARTESIAN_POINT('',(-0.0952499999999959,-0.164977839420935,39.116));
#184509=CARTESIAN_POINT('',(-53.2191856060843,30.5061406831648,39.3343017080178));
#184510=CARTESIAN_POINT('',(-53.3283379191462,30.5691598004937,39.116));
#184511=CARTESIAN_POINT('',(-52.9334317578285,30.3411606219523,39.5248017080178));
#184512=CARTESIAN_POINT('Origin',(-52.958916392492,30.3558747754329,39.1947747614341));
#184513=CARTESIAN_POINT('',(-52.8024816883957,30.2655565641149,39.5248017080178));
#184514=CARTESIAN_POINT('',(-0.0952499999999958,-0.164977839420935,39.5248017080178));
#184515=CARTESIAN_POINT('',(-52.5167277788839,30.1005764675362,39.3343017080178));
#184516=CARTESIAN_POINT('Origin',(-52.7769940214391,30.2508418455903,39.1947728911909));
#184517=CARTESIAN_POINT('',(-52.4075754202454,30.0375573238936,39.116));
#184518=CARTESIAN_POINT('',(-52.5167277788839,30.1005764675362,39.3343017080178));
#184519=CARTESIAN_POINT('',(-0.0952499999999959,-0.164977839420935,39.116));
#184520=CARTESIAN_POINT('Origin',(0.0952500000000014,0.164977839420935,
-1.34128103812642E-17));
#184521=CARTESIAN_POINT('',(-53.4854427993284,31.0998052504804,39.116));
#184522=CARTESIAN_POINT('',(-53.8585387249976,31.3152122835991,39.3548010137695));
#184523=CARTESIAN_POINT('Origin',(-53.5185519420879,31.1189208229652,39.5550293912461));
#184524=CARTESIAN_POINT('',(-54.1671020370176,31.4933613953778,39.92499));
#184525=CARTESIAN_POINT('',(-53.8585387249976,31.3152122835991,39.3548010137695));
#184526=CARTESIAN_POINT('',(-51.1878102687783,29.7732664904684,39.92499));
#184527=CARTESIAN_POINT('',(0.0952500000000119,0.164977839420932,39.92499));
#184528=CARTESIAN_POINT('',(-51.4963740058469,29.9514158463123,39.3548010137695));
#184529=CARTESIAN_POINT('',(-51.1878102687783,29.7732664904684,39.92499));
#184530=CARTESIAN_POINT('',(-51.8694703131944,30.1668231006079,39.116));
#184531=CARTESIAN_POINT('Origin',(-51.8363612765597,30.1477075893942,39.5550297827294));
#184532=CARTESIAN_POINT('',(-52.2170754206163,30.3675130020931,39.116));
#184533=CARTESIAN_POINT('',(-52.2810382154237,30.4044419397498,39.116));
#184534=CARTESIAN_POINT('',(-52.3262277788839,30.4305321463781,39.3343017080178));
#184535=CARTESIAN_POINT('',(-52.2170754202454,30.3675130027355,39.116));
#184536=CARTESIAN_POINT('',(-52.6119816883956,30.5955122429567,39.5248017080178));
#184537=CARTESIAN_POINT('Origin',(-52.5864971060013,30.5807981195153,39.1947745585587));
#184538=CARTESIAN_POINT('',(-52.7429317578285,30.6711163007942,39.5248017080178));
#184539=CARTESIAN_POINT('',(-52.7433896349615,30.6713806562801,39.5248017080178));
#184540=CARTESIAN_POINT('',(-53.0286856060843,30.8360963620066,39.3343017080178));
#184541=CARTESIAN_POINT('Origin',(-52.7684193600402,30.6858309820706,39.1947728594246));
#184542=CARTESIAN_POINT('',(-53.1378379191462,30.8991154793356,39.116));
#184543=CARTESIAN_POINT('',(-53.0286856060843,30.8360963620066,39.3343017080178));
#184544=CARTESIAN_POINT('',(-53.4858943313411,31.1000659426095,39.116));
#184545=CARTESIAN_POINT('Origin',(-47.2483549038573,34.0924682662299,40.10025));
#184546=CARTESIAN_POINT('',(-47.7461450747862,34.7084426211235,40.10025));
#184547=CARTESIAN_POINT('',(-50.8348823336483,36.9525415975216,40.10025));
#184548=CARTESIAN_POINT('',(-47.1274239660506,34.2589154226526,40.10025));
#184549=CARTESIAN_POINT('',(-50.8527980281382,36.9278827595331,40.10025));
#184550=CARTESIAN_POINT('Origin',(7.08388135731921E-17,-8.6407868066034E-17,
40.10025));
#184551=CARTESIAN_POINT('',(-47.764060769276,34.683783783135,40.10025));
#184552=CARTESIAN_POINT('',(-47.7068608037047,34.642225575547,40.10025));
#184553=CARTESIAN_POINT('Origin',(3.32162311137369E-16,4.49896674990071E-17,
40.10025));
#184554=CARTESIAN_POINT('Origin',(-0.111973090561717,-0.154117737428427,
1.57677042678049E-17));
#184555=CARTESIAN_POINT('',(-48.6559784483762,35.1151666347445,39.116));
#184556=CARTESIAN_POINT('',(-48.3074421904915,34.8619402208394,39.3548010137695));
#184557=CARTESIAN_POINT('Origin',(-48.6250489017688,35.0926950037622,39.5550297832907));
#184558=CARTESIAN_POINT('',(-48.0191904763611,34.6525130924099,39.92499));
#184559=CARTESIAN_POINT('',(-48.3074421904915,34.8619402208394,39.3548010137695));
#184560=CARTESIAN_POINT('',(-50.8023624960588,36.6746059268182,39.92499));
#184561=CARTESIAN_POINT('',(-51.0125340177512,36.8273044755034,39.92499));
#184562=CARTESIAN_POINT('',(-50.5141111791242,36.465179085564,39.3548010137695));
#184563=CARTESIAN_POINT('',(-50.8023624960588,36.6746059268182,39.92499));
#184564=CARTESIAN_POINT('',(-50.1655752777668,36.2119529314389,39.116));
#184565=CARTESIAN_POINT('Origin',(-50.1965049239947,36.2344246347996,39.5550293907213));
#184566=CARTESIAN_POINT('',(-49.8408524072783,35.9760279553334,39.116));
#184567=CARTESIAN_POINT('',(-0.111973090561712,-0.154117737428427,39.116));
#184568=CARTESIAN_POINT('',(-49.7388853330808,35.9019445403522,39.3343017080178));
#184569=CARTESIAN_POINT('',(-49.8408524068601,35.9760279559091,39.116));
#184570=CARTESIAN_POINT('',(-49.471941986573,35.7079988465462,39.5248017080178));
#184571=CARTESIAN_POINT('Origin',(-49.4957489658884,35.7252962640518,39.1947747614325));
#184572=CARTESIAN_POINT('',(-49.3496120513046,35.6191209461256,39.5248017080178));
#184573=CARTESIAN_POINT('',(-0.111973090561712,-0.154117737428427,39.5248017080178));
#184574=CARTESIAN_POINT('',(-49.0826686475732,35.4251752107442,39.3343017080178));
#184575=CARTESIAN_POINT('Origin',(-49.3258021153708,35.6018226497106,39.1947728911869));
#184576=CARTESIAN_POINT('',(-48.9807015312175,35.3510917642538,39.116));
#184577=CARTESIAN_POINT('',(-49.0826686475732,35.4251752107442,39.3343017080178));
#184578=CARTESIAN_POINT('',(-0.111973090561712,-0.154117737428427,39.116));
#184579=CARTESIAN_POINT('Origin',(0.111973090561717,0.154117737428427,-1.57677042678049E-17));
#184580=CARTESIAN_POINT('',(-49.9416290966434,36.5201884062957,39.116));
#184581=CARTESIAN_POINT('',(-50.2901649976452,36.7734145609102,39.3548010137695));
#184582=CARTESIAN_POINT('Origin',(-49.9725587426391,36.5426601094878,39.5550293912443));
#184583=CARTESIAN_POINT('',(-50.5784163146694,36.9828414020412,39.92499));
#184584=CARTESIAN_POINT('',(-50.2901649976452,36.7734145609102,39.3548010137695));
#184585=CARTESIAN_POINT('',(-47.7952442955499,34.960748566837,39.92499));
#184586=CARTESIAN_POINT('',(0.111973090561728,0.154117737428423,39.92499));
#184587=CARTESIAN_POINT('',(-48.0834960097837,35.1701756951242,39.3548010137695));
#184588=CARTESIAN_POINT('',(-47.7952442955499,34.960748566837,39.92499));
#184589=CARTESIAN_POINT('',(-48.4320322672528,35.4234021096014,39.116));
#184590=CARTESIAN_POINT('Origin',(-48.4011027203979,35.4009304784394,39.5550297827317));
#184591=CARTESIAN_POINT('',(-48.7567553505297,35.659327238511,39.116));
#184592=CARTESIAN_POINT('',(-48.8165076253516,35.7027398082303,39.116));
#184593=CARTESIAN_POINT('',(-48.8587224664497,35.733410685601,39.3343017080178));
#184594=CARTESIAN_POINT('',(-48.7567553500941,35.6593272391106,39.116));
#184595=CARTESIAN_POINT('',(-49.1256658701812,35.9273564209824,39.5248017080178));
#184596=CARTESIAN_POINT('Origin',(-49.101858939706,35.9100590388132,39.1947745585612));
#184597=CARTESIAN_POINT('',(-49.2479958054496,36.0162343214031,39.5248017080178));
#184598=CARTESIAN_POINT('',(-49.248423541611,36.0165450899151,39.5248017080178));
#184599=CARTESIAN_POINT('',(-49.5149391519574,36.2101800152091,39.3343017080178));
#184600=CARTESIAN_POINT('Origin',(-49.2718056808913,36.0335325740096,39.1947728594319));
#184601=CARTESIAN_POINT('',(-49.6169062257367,36.284263430766,39.116));
#184602=CARTESIAN_POINT('',(-49.5149391519574,36.2101800152091,39.3343017080178));
#184603=CARTESIAN_POINT('',(-49.9420509053688,36.5204948682734,39.116));
#184604=CARTESIAN_POINT('Origin',(-43.4258901551468,38.8445040879385,40.10025));
#184605=CARTESIAN_POINT('',(-43.8565665267053,39.5091373124626,40.10025));
#184606=CARTESIAN_POINT('',(-46.6938111422601,42.0638038389704,40.10025));
#184607=CARTESIAN_POINT('',(-43.2882232241945,38.9973987043323,40.10025));
#184608=CARTESIAN_POINT('',(-46.7142062431419,42.0411527846899,40.10025));
#184609=CARTESIAN_POINT('Origin',(6.11552196804844E-17,-9.83661106291793E-17,
40.10025));
#184610=CARTESIAN_POINT('',(-43.8769616275871,39.486486258182,40.10025));
#184611=CARTESIAN_POINT('',(-43.8244190249875,39.4391766863034,40.10025));
#184612=CARTESIAN_POINT('Origin',(3.37204232425086E-16,5.12159217606818E-17,
40.10025));
#184613=CARTESIAN_POINT('Origin',(-0.127469380511364,-0.141569089253443,
1.79498438867833E-17));
#184614=CARTESIAN_POINT('',(-44.7189015017595,40.0087367337517,39.116));
#184615=CARTESIAN_POINT('',(-44.3987439298677,39.7204655612078,39.3548010137695));
#184616=CARTESIAN_POINT('Origin',(-44.6904903154964,39.9831551867371,39.5550297832859));
#184617=CARTESIAN_POINT('',(-44.1339623846887,39.4820551877883,39.92499));
#184618=CARTESIAN_POINT('',(-44.3987439298677,39.7204655612078,39.3548010137695));
#184619=CARTESIAN_POINT('',(-46.6905216402894,41.7839914803031,39.92499));
#184620=CARTESIAN_POINT('',(-46.8835804757581,41.9578224365465,39.92499));
#184621=CARTESIAN_POINT('',(-46.425740460113,41.5455814340033,39.3548010137695));
#184622=CARTESIAN_POINT('',(-46.6905216402894,41.7839914803031,39.92499));
#184623=CARTESIAN_POINT('',(-46.1055832156406,41.2573105570841,39.116));
#184624=CARTESIAN_POINT('Origin',(-46.1339944934112,41.2828921864924,39.5550293907205));
#184625=CARTESIAN_POINT('',(-45.8073000862117,40.9887352200428,39.116));
#184626=CARTESIAN_POINT('',(-0.127469380511358,-0.141569089253443,39.116));
#184627=CARTESIAN_POINT('',(-45.7136354238372,40.9043991801907,39.3343017080178));
#184628=CARTESIAN_POINT('',(-45.8073000857355,40.9887352205717,39.116));
#184629=CARTESIAN_POINT('',(-45.4684272662432,40.6836127633983,39.5248017080178));
#184630=CARTESIAN_POINT('Origin',(-45.4902957559641,40.7033039308033,39.1947747614306));
#184631=CARTESIAN_POINT('',(-45.3560577375092,40.5824347852704,39.5248017080178));
#184632=CARTESIAN_POINT('',(-0.127469380511358,-0.141569089253443,39.5248017080178));
#184633=CARTESIAN_POINT('',(-45.1108495273509,40.3616483211488,39.3343017080178));
#184634=CARTESIAN_POINT('Origin',(-45.3341863992356,40.562742434718,39.1947728911902));
#184635=CARTESIAN_POINT('',(-45.0171848263429,40.2773122455532,39.116));
#184636=CARTESIAN_POINT('',(-45.1108495273509,40.3616483211488,39.3343017080178));
#184637=CARTESIAN_POINT('',(-0.127469380511358,-0.141569089253443,39.116));
#184638=CARTESIAN_POINT('Origin',(0.127469380511364,0.141569089253443,-1.79498438867833E-17));
#184639=CARTESIAN_POINT('',(-45.8506444546178,41.5404487355909,39.116));
#184640=CARTESIAN_POINT('',(-46.170801698685,41.8287196129603,39.3548010137695));
#184641=CARTESIAN_POINT('Origin',(-45.8790557321747,41.5660303648068,39.5550293912447));
#184642=CARTESIAN_POINT('',(-46.4355828789641,42.067129659146,39.92499));
#184643=CARTESIAN_POINT('',(-46.170801698685,41.8287196129603,39.3548010137695));
#184644=CARTESIAN_POINT('',(-43.8790236240217,39.7651933659003,39.92499));
#184645=CARTESIAN_POINT('',(0.127469380511373,0.141569089253439,39.92499));
#184646=CARTESIAN_POINT('',(-44.1438051693171,40.0036037391903,39.3548010137695));
#184647=CARTESIAN_POINT('',(-43.8790236240217,39.7651933659002,39.92499));
#184648=CARTESIAN_POINT('',(-44.4639627407368,40.2918749122586,39.116));
#184649=CARTESIAN_POINT('Origin',(-44.4355515542491,40.2662933650416,39.555029782734));
#184650=CARTESIAN_POINT('',(-44.7622460658166,40.5604504235087,39.116));
#184651=CARTESIAN_POINT('',(-44.8171331622253,40.6098709880932,39.116));
#184652=CARTESIAN_POINT('',(-44.8559107663282,40.6447864996556,39.3343017080178));
#184653=CARTESIAN_POINT('',(-44.7622460653202,40.5604504240601,39.116));
#184654=CARTESIAN_POINT('',(-45.1011189764865,40.8655729637772,39.5248017080178));
#184655=CARTESIAN_POINT('Origin',(-45.0792505316453,40.8458818366207,39.194774558559));
#184656=CARTESIAN_POINT('',(-45.2134885052205,40.9667509419051,39.5248017080178));
#184657=CARTESIAN_POINT('',(-45.2138814140435,40.9671047185984,39.5248017080178));
#184658=CARTESIAN_POINT('',(-45.4586966628145,41.1875373586976,39.3343017080178));
#184659=CARTESIAN_POINT('Origin',(-45.2353597879103,40.9864432425637,39.1947728594292));
#184660=CARTESIAN_POINT('',(-45.5523613247128,41.2718733990786,39.116));
#184661=CARTESIAN_POINT('',(-45.4586966628145,41.1875373586976,39.3343017080178));
#184662=CARTESIAN_POINT('',(-45.8510319186313,41.5407976097557,39.116));
#184663=CARTESIAN_POINT('Origin',(-39.1276422664447,43.1709513941247,40.10025));
#184664=CARTESIAN_POINT('',(-39.4864862581813,43.8769616275878,40.10025));
#184665=CARTESIAN_POINT('',(-42.0411527846891,46.7142062431426,40.10025));
#184666=CARTESIAN_POINT('',(-38.974747650051,43.308618325077,40.10025));
#184667=CARTESIAN_POINT('',(-42.0638038389696,46.6938111422608,40.10025));
#184668=CARTESIAN_POINT('Origin',(5.02746968098233E-17,-1.09246633499839E-16,
40.10025));
#184669=CARTESIAN_POINT('',(-39.5091373124618,43.856566526706,40.10025));
#184670=CARTESIAN_POINT('',(-39.4618277405832,43.8040239241063,40.10025));
#184671=CARTESIAN_POINT('Origin',(3.4286935433033E-16,5.68810436659258E-17,
40.10025));
#184672=CARTESIAN_POINT('Origin',(-0.141569089253445,-0.127469380511361,
1.99353212598918E-17));
#184673=CARTESIAN_POINT('',(-40.2918749122578,44.4639627407375,39.116));
#184674=CARTESIAN_POINT('',(-40.0036037397139,44.1438051688457,39.3548010137695));
#184675=CARTESIAN_POINT('Origin',(-40.2662933652429,44.435551554474,39.5550297832848));
#184676=CARTESIAN_POINT('',(-39.765193365504,43.8790236243784,39.92499));
#184677=CARTESIAN_POINT('',(-40.0036037397139,44.1438051688457,39.3548010137695));
#184678=CARTESIAN_POINT('',(-42.0671296588092,46.4355828792674,39.92499));
#184679=CARTESIAN_POINT('',(-42.2409606150526,46.6286417147361,39.92499));
#184680=CARTESIAN_POINT('',(-41.8287196134094,46.1708016982806,39.3548010137695));
#184681=CARTESIAN_POINT('',(-42.0671296588092,46.4355828792674,39.92499));
#184682=CARTESIAN_POINT('',(-41.5404487355902,45.8506444546186,39.116));
#184683=CARTESIAN_POINT('Origin',(-41.5660303649983,45.8790557323889,39.5550293907209));
#184684=CARTESIAN_POINT('',(-41.2718733996071,45.552361324237,39.116));
#184685=CARTESIAN_POINT('',(-0.141569089253439,-0.127469380511361,39.116));
#184686=CARTESIAN_POINT('',(-41.1875373586968,45.4586966628152,39.3343017080178));
#184687=CARTESIAN_POINT('',(-41.2718733990778,45.5523613247135,39.116));
#184688=CARTESIAN_POINT('',(-40.9667509419044,45.2134885052212,39.5248017080178));
#184689=CARTESIAN_POINT('Origin',(-40.9864413462806,45.2353576819744,39.1947747614277));
#184690=CARTESIAN_POINT('',(-40.8655729637765,45.1011189764872,39.5248017080178));
#184691=CARTESIAN_POINT('',(-0.141569089253439,-0.127469380511361,39.5248017080178));
#184692=CARTESIAN_POINT('',(-40.6447864996549,44.8559107663289,39.3343017080178));
#184693=CARTESIAN_POINT('Origin',(-40.8458798501211,45.0792483253095,39.1947728911976));
#184694=CARTESIAN_POINT('',(-40.5604504240593,44.7622460653209,39.116));
#184695=CARTESIAN_POINT('',(-40.6447864996549,44.8559107663289,39.3343017080178));
#184696=CARTESIAN_POINT('',(-0.141569089253439,-0.127469380511361,39.116));
#184697=CARTESIAN_POINT('Origin',(0.141569089253445,0.127469380511361,-1.99353212598918E-17));
#184698=CARTESIAN_POINT('',(-41.2573105570833,46.1055832156413,39.116));
#184699=CARTESIAN_POINT('',(-41.5455814344526,46.4257404597085,39.3548010137695));
#184700=CARTESIAN_POINT('Origin',(-41.2828921862987,46.1339944931977,39.5550293912461));
#184701=CARTESIAN_POINT('',(-41.7839914799654,46.6905216405934,39.92499));
#184702=CARTESIAN_POINT('',(-41.5455814344526,46.4257404597085,39.3548010137695));
#184703=CARTESIAN_POINT('',(-39.4820551873926,44.1339623850451,39.92499));
#184704=CARTESIAN_POINT('',(0.141569089253454,0.127469380511357,39.92499));
#184705=CARTESIAN_POINT('',(-39.7204655617323,44.3987439293954,39.3548010137695));
#184706=CARTESIAN_POINT('',(-39.4820551873926,44.1339623850451,39.92499));
#184707=CARTESIAN_POINT('',(-40.0087367337509,44.7189015017602,39.116));
#184708=CARTESIAN_POINT('Origin',(-39.9831551865335,44.6904903152718,39.5550297827328));
#184709=CARTESIAN_POINT('',(-40.2773122461034,45.0171848258474,39.116));
#184710=CARTESIAN_POINT('',(-40.3267328095855,45.0720719232487,39.116));
#184711=CARTESIAN_POINT('',(-40.361648321148,45.1108495273516,39.3343017080178));
#184712=CARTESIAN_POINT('',(-40.2773122455524,45.0171848263436,39.116));
#184713=CARTESIAN_POINT('',(-40.5824347852696,45.3560577375099,39.5248017080178));
#184714=CARTESIAN_POINT('Origin',(-40.5627444213194,45.3341886054756,39.1947745585574));
#184715=CARTESIAN_POINT('',(-40.6836127633975,45.4684272662439,39.5248017080178));
#184716=CARTESIAN_POINT('',(-40.6839665400907,45.4688201750669,39.5248017080178));
#184717=CARTESIAN_POINT('',(-40.9043991801899,45.7136354238379,39.3343017080178));
#184718=CARTESIAN_POINT('Origin',(-40.7033058269857,45.4902978619877,39.1947728594267));
#184719=CARTESIAN_POINT('',(-40.988735220571,45.8073000857362,39.116));
#184720=CARTESIAN_POINT('',(-40.9043991801899,45.7136354238379,39.3343017080178));
#184721=CARTESIAN_POINT('',(-41.2576594312481,46.1059706796548,39.116));
#184722=CARTESIAN_POINT('Origin',(-34.4007037410859,47.0244087227344,40.10025));
#184723=CARTESIAN_POINT('',(-34.6837837831342,47.7640607692766,40.10025));
#184724=CARTESIAN_POINT('',(-36.9278827595322,50.8527980281388,40.10025));
#184725=CARTESIAN_POINT('',(-34.2342565846632,47.1453396605411,40.10025));
#184726=CARTESIAN_POINT('',(-36.9525415975208,50.8348823336489,40.10025));
#184727=CARTESIAN_POINT('Origin',(3.83164542466798E-17,-1.18930227392547E-16,
40.10025));
#184728=CARTESIAN_POINT('',(-34.7084426211227,47.7461450747867,40.10025));
#184729=CARTESIAN_POINT('',(-34.6668844135347,47.6889451092154,40.10025));
#184730=CARTESIAN_POINT('Origin',(3.49095608592005E-16,6.19229649536422E-17,
40.10025));
#184731=CARTESIAN_POINT('Origin',(-0.154117737428428,-0.111973090561715,
2.17023830815427E-17));
#184732=CARTESIAN_POINT('',(-35.4234021096005,48.4320322672534,39.116));
#184733=CARTESIAN_POINT('',(-35.1701756956954,48.0834960093687,39.3548010137695));
#184734=CARTESIAN_POINT('Origin',(-35.400930478617,48.4011027206441,39.5550297832863));
#184735=CARTESIAN_POINT('',(-34.9607485664064,47.7952442958627,39.92499));
#184736=CARTESIAN_POINT('',(-35.1701756956954,48.0834960093687,39.3548010137695));
#184737=CARTESIAN_POINT('',(-36.9828414016742,50.578416314936,39.92499));
#184738=CARTESIAN_POINT('',(-37.1355399503593,50.7885878366284,39.92499));
#184739=CARTESIAN_POINT('',(-36.7734145613992,50.29016499729,39.3548010137695));
#184740=CARTESIAN_POINT('',(-36.9828414016742,50.578416314936,39.92499));
#184741=CARTESIAN_POINT('',(-36.5201884062949,49.941629096644,39.116));
#184742=CARTESIAN_POINT('Origin',(-36.5426601096559,49.9725587428724,39.5550293907199));
#184743=CARTESIAN_POINT('',(-36.2842634313413,49.6169062253187,39.116));
#184744=CARTESIAN_POINT('',(-0.154117737428423,-0.111973090561715,39.116));
#184745=CARTESIAN_POINT('',(-36.2101800152082,49.514939151958,39.3343017080178));
#184746=CARTESIAN_POINT('',(-36.2842634307651,49.6169062257373,39.116));
#184747=CARTESIAN_POINT('',(-36.0162343214022,49.2479958054502,39.5248017080178));
#184748=CARTESIAN_POINT('Origin',(-36.0335309082442,49.2718033882756,39.194774761429));
#184749=CARTESIAN_POINT('',(-35.9273564209816,49.1256658701818,39.5248017080178));
#184750=CARTESIAN_POINT('',(-0.154117737428423,-0.111973090561715,39.5248017080178));
#184751=CARTESIAN_POINT('',(-35.7334106856002,48.8587224664504,39.3343017080178));
#184752=CARTESIAN_POINT('Origin',(-35.910057293824,49.1018565378156,39.1947728911897));
#184753=CARTESIAN_POINT('',(-35.6593272391098,48.7567553500947,39.116));
#184754=CARTESIAN_POINT('',(-35.7334106856002,48.8587224664504,39.3343017080178));
#184755=CARTESIAN_POINT('',(-0.154117737428423,-0.111973090561715,39.116));
#184756=CARTESIAN_POINT('Origin',(0.154117737428428,0.111973090561715,-2.17023830815427E-17));
#184757=CARTESIAN_POINT('',(-36.211952931438,50.1655752777675,39.116));
#184758=CARTESIAN_POINT('',(-36.4651790860525,50.5141111787693,39.3548010137695));
#184759=CARTESIAN_POINT('Origin',(-36.2344246346303,50.1965049237634,39.5550293912439));
#184760=CARTESIAN_POINT('',(-36.6746059264512,50.8023624963254,39.92499));
#184761=CARTESIAN_POINT('',(-36.4651790860525,50.5141111787693,39.3548010137695));
#184762=CARTESIAN_POINT('',(-34.6525130919793,48.0191904766739,39.92499));
#184763=CARTESIAN_POINT('',(0.154117737428437,0.11197309056171,39.92499));
#184764=CARTESIAN_POINT('',(-34.8619402214104,48.3074421900766,39.3548010137695));
#184765=CARTESIAN_POINT('',(-34.6525130919793,48.0191904766739,39.92499));
#184766=CARTESIAN_POINT('',(-35.1151666347437,48.6559784483768,39.116));
#184767=CARTESIAN_POINT('Origin',(-35.0926950035808,48.6250489015207,39.5550297827299));
#184768=CARTESIAN_POINT('',(-35.3510917648529,48.9807015307823,39.116));
#184769=CARTESIAN_POINT('',(-35.3945043333726,49.0404538064757,39.116));
#184770=CARTESIAN_POINT('',(-35.4251752107434,49.0826686475738,39.3343017080178));
#184771=CARTESIAN_POINT('',(-35.3510917642529,48.9807015312181,39.116));
#184772=CARTESIAN_POINT('',(-35.6191209461248,49.3496120513052,39.5248017080178));
#184773=CARTESIAN_POINT('Origin',(-35.6018243948127,49.3258045171787,39.1947745585588));
#184774=CARTESIAN_POINT('',(-35.7079988465454,49.4719419865736,39.5248017080178));
#184775=CARTESIAN_POINT('',(-35.7083096150574,49.472369722735,39.5248017080178));
#184776=CARTESIAN_POINT('',(-35.9019445403514,49.7388853330814,39.3343017080178));
#184777=CARTESIAN_POINT('Origin',(-35.7252979297055,49.4957512585776,39.1947728594227));
#184778=CARTESIAN_POINT('',(-35.9760279559083,49.8408524068607,39.116));
#184779=CARTESIAN_POINT('',(-35.9019445403514,49.7388853330814,39.3343017080178));
#184780=CARTESIAN_POINT('',(-36.2122593934157,50.1659970864929,39.116));
#184781=CARTESIAN_POINT('Origin',(-29.2968639067297,50.3626567888878,40.10025));
#184782=CARTESIAN_POINT('',(-29.5010785149107,51.127846865905,40.10025));
#184783=CARTESIAN_POINT('',(-31.4100231232056,54.4342359163066,40.10025));
#184784=CARTESIAN_POINT('',(-29.1186878401551,50.4655267888878,40.10025));
#184785=CARTESIAN_POINT('',(-31.436419577513,54.4189959163066,40.10025));
#184786=CARTESIAN_POINT('Origin',(2.54115089989943E-17,-1.27310796826193E-16,
40.10025));
#184787=CARTESIAN_POINT('',(-29.527474969218,51.112606865905,40.10025));
#184788=CARTESIAN_POINT('',(-29.4921234463396,51.0513762321547,40.10025));
#184789=CARTESIAN_POINT('Origin',(3.55814779065493E-16,6.6286445279113E-17,
40.10025));
#184790=CARTESIAN_POINT('Origin',(-0.164977839420936,-0.0952499999999985,
2.32316690526366E-17));
#184791=CARTESIAN_POINT('',(-30.166823100607,51.8694703131949,39.116));
#184792=CARTESIAN_POINT('',(-29.9514158469225,51.4963740054946,39.3548010137695));
#184793=CARTESIAN_POINT('Origin',(-30.1477075895458,51.8363612768244,39.5550297832863));
#184794=CARTESIAN_POINT('',(-29.7732664900073,51.1878102690445,39.92499));
#184795=CARTESIAN_POINT('',(-29.9514158469225,51.4963740054946,39.3548010137695));
#184796=CARTESIAN_POINT('',(-31.4933613949854,54.1671020372441,39.92499));
#184797=CARTESIAN_POINT('',(-31.6232545388586,54.3920835619874,39.92499));
#184798=CARTESIAN_POINT('',(-31.3152122841225,53.8585387246954,39.3548010137695));
#184799=CARTESIAN_POINT('',(-31.4933613949854,54.1671020372441,39.92499));
#184800=CARTESIAN_POINT('',(-31.0998052504795,53.4854427993289,39.116));
#184801=CARTESIAN_POINT('Origin',(-31.118920823109,53.5185519423391,39.5550293907184));
#184802=CARTESIAN_POINT('',(-30.8991154799509,53.1378379187909,39.116));
#184803=CARTESIAN_POINT('',(-0.164977839420931,-0.0952499999999985,39.116));
#184804=CARTESIAN_POINT('',(-30.8360963620057,53.0286856060848,39.3343017080178));
#184805=CARTESIAN_POINT('',(-30.8991154793346,53.1378379191467,39.116));
#184806=CARTESIAN_POINT('',(-30.6711163007932,52.742931757829,39.5248017080178));
#184807=CARTESIAN_POINT('Origin',(-30.6858295650774,52.7684169058696,39.1947747614331));
#184808=CARTESIAN_POINT('',(-30.5955122429558,52.6119816883962,39.5248017080178));
#184809=CARTESIAN_POINT('',(-0.164977839420931,-0.0952499999999985,39.5248017080178));
#184810=CARTESIAN_POINT('',(-30.4305321463772,52.3262277788844,39.3343017080178));
#184811=CARTESIAN_POINT('Origin',(-30.5807966351501,52.5864945348654,39.1947728911916));
#184812=CARTESIAN_POINT('',(-30.3675130027346,52.2170754202459,39.116));
#184813=CARTESIAN_POINT('',(-30.4305321463772,52.3262277788844,39.3343017080178));
#184814=CARTESIAN_POINT('',(-0.164977839420931,-0.0952499999999985,39.116));
#184815=CARTESIAN_POINT('Origin',(0.164977839420936,0.0952499999999985,
-2.32316690526366E-17));
#184816=CARTESIAN_POINT('',(-30.7698495716376,53.6759427993289,39.116));
#184817=CARTESIAN_POINT('',(-30.9852566047563,54.0490387249982,39.3548010137695));
#184818=CARTESIAN_POINT('Origin',(-30.788965144123,53.7090519420896,39.5550293912436));
#184819=CARTESIAN_POINT('',(-31.1634057157511,54.3576020374707,39.92499));
#184820=CARTESIAN_POINT('',(-30.9852566047563,54.0490387249982,39.3548010137695));
#184821=CARTESIAN_POINT('',(-29.4433108116256,51.3783102687788,39.92499));
#184822=CARTESIAN_POINT('',(0.164977839420945,0.0952499999999936,39.92499));
#184823=CARTESIAN_POINT('',(-29.6214601686921,51.6868740051415,39.3548010137695));
#184824=CARTESIAN_POINT('',(-29.4433108116256,51.3783102687788,39.92499));
#184825=CARTESIAN_POINT('',(-29.8368674217651,52.0599703131949,39.116));
#184826=CARTESIAN_POINT('Origin',(-29.8177519105508,52.026861276559,39.5550297827274));
#184827=CARTESIAN_POINT('',(-30.0375573245351,52.407575419875,39.116));
#184828=CARTESIAN_POINT('',(-30.074486260907,52.4715382154242,39.116));
#184829=CARTESIAN_POINT('',(-30.1005764675353,52.5167277788844,39.3343017080178));
#184830=CARTESIAN_POINT('',(-30.0375573238927,52.4075754202459,39.116));
#184831=CARTESIAN_POINT('',(-30.2655565641139,52.8024816883962,39.5248017080178));
#184832=CARTESIAN_POINT('Origin',(-30.2508433300758,52.7769965925036,39.1947745585601));
#184833=CARTESIAN_POINT('',(-30.3411606219514,52.933431757829,39.5248017080178));
#184834=CARTESIAN_POINT('',(-30.3414249774373,52.933889634962,39.5248017080178));
#184835=CARTESIAN_POINT('',(-30.5061406831638,53.2191856060848,39.3343017080178));
#184836=CARTESIAN_POINT('Origin',(-30.3558761923107,52.9589188467299,39.1947728594266));
#184837=CARTESIAN_POINT('',(-30.5691598004928,53.3283379191467,39.116));
#184838=CARTESIAN_POINT('',(-30.5061406831638,53.2191856060848,39.3343017080178));
#184839=CARTESIAN_POINT('',(-30.7701102637667,53.6763943313416,39.116));
#184840=CARTESIAN_POINT('Origin',(-23.8720415006485,53.1491210481985,40.10025));
#184841=CARTESIAN_POINT('',(-23.9951532569802,53.9314655730806,40.10025));
#184842=CARTESIAN_POINT('',(-25.5480287005713,57.4192809246791,40.10025));
#184843=CARTESIAN_POINT('',(-23.6840886581931,53.232803045145,40.10025));
#184844=CARTESIAN_POINT('',(-25.5758735661203,57.4068835917982,40.10025));
#184845=CARTESIAN_POINT('Origin',(1.17012503474357E-17,-1.34296522528313E-16,
40.10025));
#184846=CARTESIAN_POINT('',(-24.0229981225292,53.9190682401997,40.10025));
#184847=CARTESIAN_POINT('',(-23.9942406030429,53.8544777939071,40.10025));
#184848=CARTESIAN_POINT('Origin',(3.6295324911301E-16,6.99236774387753E-17,
40.10025));
#184849=CARTESIAN_POINT('Origin',(-0.174030409680916,-0.0774833305059384,
2.45064239960505E-17));
#184850=CARTESIAN_POINT('',(-24.5797300649096,54.7386155880006,39.116));
#184851=CARTESIAN_POINT('',(-24.4045020183941,54.3450469517072,39.3548010137695));
#184852=CARTESIAN_POINT('Origin',(-24.5641801073101,54.7036898113994,39.5550297832858));
#184853=CARTESIAN_POINT('',(-24.2595822754869,54.0195518811807,39.92499));
#184854=CARTESIAN_POINT('',(-24.4045020183941,54.3450469517072,39.3548010137695));
#184855=CARTESIAN_POINT('',(-25.6588335304436,57.1623216544373,39.92499));
#184856=CARTESIAN_POINT('',(-25.7644981330387,57.3996482375659,39.92499));
#184857=CARTESIAN_POINT('',(-25.5139139879313,56.8368270312094,39.3548010137695));
#184858=CARTESIAN_POINT('',(-25.6588335304436,57.1623216544373,39.92499));
#184859=CARTESIAN_POINT('',(-25.3386861202872,56.4432587981559,39.116));
#184860=CARTESIAN_POINT('Origin',(-25.3542361279707,56.4781846872474,39.5550293907191));
#184861=CARTESIAN_POINT('',(-25.1754303533072,56.076580340217,39.116));
#184862=CARTESIAN_POINT('',(-0.174030409680911,-0.0774833305059384,39.116));
#184863=CARTESIAN_POINT('',(-25.1241659841931,55.9614386837455,39.3343017080178));
#184864=CARTESIAN_POINT('',(-25.175430352657,56.0765803405065,39.116));
#184865=CARTESIAN_POINT('',(-24.9899591116491,55.660005112701,39.5248017080178));
#184866=CARTESIAN_POINT('Origin',(-25.00192785177,55.6868886053366,39.1947747614285));
#184867=CARTESIAN_POINT('',(-24.9284572302736,55.5218696254675,39.5248017080178));
#184868=CARTESIAN_POINT('',(-0.174030409680911,-0.0774833305059384,39.5248017080178));
#184869=CARTESIAN_POINT('',(-24.7942503289602,55.2204359898058,39.3343017080178));
#184870=CARTESIAN_POINT('Origin',(-24.9164863690984,55.4949838933597,39.1947728911931));
#184871=CARTESIAN_POINT('',(-24.7429859390908,55.1052942849674,39.116));
#184872=CARTESIAN_POINT('',(-24.7942503289602,55.2204359898058,39.3343017080178));
#184873=CARTESIAN_POINT('',(-0.174030409680911,-0.0774833305059384,39.116));
#184874=CARTESIAN_POINT('Origin',(0.174030409680916,0.0774833305059384,
-2.45064239960505E-17));
#184875=CARTESIAN_POINT('',(-24.9906253009254,56.5982254591678,39.116));
#184876=CARTESIAN_POINT('',(-25.1658531680166,56.9917936924675,39.3548010137695));
#184877=CARTESIAN_POINT('Origin',(-25.0061753084915,56.6331513479959,39.5550293912447));
#184878=CARTESIAN_POINT('',(-25.3107727106682,57.3172883156333,39.92499));
#184879=CARTESIAN_POINT('',(-25.1658531680166,56.9917936924675,39.3548010137695));
#184880=CARTESIAN_POINT('',(-23.911521456611,54.1745185419762,39.92499));
#184881=CARTESIAN_POINT('',(0.174030409680924,0.0774833305059332,39.92499));
#184882=CARTESIAN_POINT('',(-24.0564411996771,54.500013612432,39.3548010137695));
#184883=CARTESIAN_POINT('',(-23.911521456611,54.1745185419762,39.92499));
#184884=CARTESIAN_POINT('',(-24.2316692455478,54.8935822490125,39.116));
#184885=CARTESIAN_POINT('Origin',(-24.216119287825,54.8586564721344,39.5550297827321));
#184886=CARTESIAN_POINT('',(-24.3949251204065,55.2602609456776,39.116));
#184887=CARTESIAN_POINT('',(-24.4249658234761,55.3277334713092,39.116));
#184888=CARTESIAN_POINT('',(-24.4461895095984,55.3754026508177,39.3343017080178));
#184889=CARTESIAN_POINT('',(-24.394925119729,55.2602609459793,39.116));
#184890=CARTESIAN_POINT('',(-24.5803964109118,55.6768362864794,39.5248017080178));
#184891=CARTESIAN_POINT('Origin',(-24.5684276954195,55.649952848866,39.1947745585588));
#184892=CARTESIAN_POINT('',(-24.6418982922872,55.8149717737129,39.5248017080178));
#184893=CARTESIAN_POINT('',(-24.6421133384131,55.8154547752197,39.5248017080178));
#184894=CARTESIAN_POINT('',(-24.7761051648312,56.1164053447574,39.3343017080178));
#184895=CARTESIAN_POINT('Origin',(-24.653869122976,55.8418574376289,39.1947728594248));
#184896=CARTESIAN_POINT('',(-24.8273695332952,56.2315470015184,39.116));
#184897=CARTESIAN_POINT('',(-24.7761051648312,56.1164053447574,39.3343017080178));
#184898=CARTESIAN_POINT('',(-24.9908373670083,56.5987017673885,39.116));
#184899=CARTESIAN_POINT('Origin',(-18.1856720123403,55.3532724151367,40.10025));
#184900=CARTESIAN_POINT('',(-18.2263320786577,56.1441998575529,40.10025));
#184901=CARTESIAN_POINT('',(-19.4061247292248,59.7752282754838,40.10025));
#184902=CARTESIAN_POINT('',(-17.9900016446778,55.4168495715594,40.10025));
#184903=CARTESIAN_POINT('',(-19.4351129318415,59.7658094374953,40.10025));
#184904=CARTESIAN_POINT('Origin',(-2.66410924515479E-18,-1.3981086742626E-16,
40.10025));
#184905=CARTESIAN_POINT('',(-18.2553202812744,56.1347810195644,40.10025));
#184906=CARTESIAN_POINT('',(-18.2334718385814,56.0675384271755,40.10025));
#184907=CARTESIAN_POINT('Origin',(3.7043280816289E-16,7.27948111559483E-17,
40.10025));
#184908=CARTESIAN_POINT('Origin',(-0.181176266354227,-0.0588677374284257,
2.55126814298649E-17));
#184909=CARTESIAN_POINT('',(-18.7233363629819,57.0080331356324,39.116));
#184910=CARTESIAN_POINT('',(-18.5902073587817,56.5983041910847,39.3548010137695));
#184911=CARTESIAN_POINT('Origin',(-18.7115223274338,56.9716732729184,39.5550297832861));
#184912=CARTESIAN_POINT('',(-18.4801050009129,56.2594439785883,39.92499));
#184913=CARTESIAN_POINT('',(-18.5902073587817,56.5983041910847,39.3548010137695));
#184914=CARTESIAN_POINT('',(-19.5431821162861,59.5312589135997,39.92499));
#184915=CARTESIAN_POINT('',(-19.6234604941053,59.7783303554051,39.92499));
#184916=CARTESIAN_POINT('',(-19.4330799109589,59.1923991668986,39.3548010137695));
#184917=CARTESIAN_POINT('',(-19.5431821162861,59.5312589135997,39.92499));
#184918=CARTESIAN_POINT('',(-19.2999510425001,58.782670642079,39.116));
#184919=CARTESIAN_POINT('Origin',(-19.3117651160997,58.8190306219038,39.5550293907171));
#184920=CARTESIAN_POINT('',(-19.1759179434146,58.4009360126571,39.116));
#184921=CARTESIAN_POINT('',(-0.181176266354222,-0.0588677374284257,39.116));
#184922=CARTESIAN_POINT('',(-19.1369699862878,58.2810665285032,39.3343017080178));
#184923=CARTESIAN_POINT('',(-19.1759179427381,58.4009360128769,39.116));
#184924=CARTESIAN_POINT('',(-19.0350067009925,57.9672558039534,39.5248017080178));
#184925=CARTESIAN_POINT('Origin',(-19.0440997849299,57.9952431000144,39.1947747614259));
#184926=CARTESIAN_POINT('',(-18.9882808235615,57.8234483402241,39.5248017080178));
#184927=CARTESIAN_POINT('',(-0.181176266354222,-0.0588677374284257,39.5248017080178));
#184928=CARTESIAN_POINT('',(-18.8863175164087,57.5096375484038,39.3343017080178));
#184929=CARTESIAN_POINT('Origin',(-18.9791858642783,57.79545859525,39.1947728911881));
#184930=CARTESIAN_POINT('',(-18.8473695436957,57.3897680139786,39.116));
#184931=CARTESIAN_POINT('',(-18.8863175164087,57.5096375484038,39.3343017080178));
#184932=CARTESIAN_POINT('',(-0.181176266354222,-0.0588677374284257,39.116));
#184933=CARTESIAN_POINT('Origin',(0.181176266354227,0.0588677374284257,
-2.55126814298649E-17));
#184934=CARTESIAN_POINT('',(-18.9375985097916,58.9004061169359,39.116));
#184935=CARTESIAN_POINT('',(-19.0707273776747,59.3101346419425,39.3548010137695));
#184936=CARTESIAN_POINT('Origin',(-18.9494125833019,58.9367660964855,39.5550293912448));
#184937=CARTESIAN_POINT('',(-19.1808295831467,59.6489943885966,39.92499));
#184938=CARTESIAN_POINT('',(-19.0707273776747,59.3101346419425,39.3548010137695));
#184939=CARTESIAN_POINT('',(-18.1177524687101,56.3771794532809,39.92499));
#184940=CARTESIAN_POINT('',(0.181176266354235,0.0588677374284204,39.92499));
#184941=CARTESIAN_POINT('',(-18.2278548267452,56.7160396657232,39.3548010137695));
#184942=CARTESIAN_POINT('',(-18.1177524687101,56.3771794532809,39.92499));
#184943=CARTESIAN_POINT('',(-18.3609838302735,57.1257686104892,39.116));
#184944=CARTESIAN_POINT('Origin',(-18.3491697946313,57.0894087474858,39.5550297827304));
#184945=CARTESIAN_POINT('',(-18.4850170116926,57.5075034886062,39.116));
#184946=CARTESIAN_POINT('',(-18.5078403492304,57.57774650121,39.116));
#184947=CARTESIAN_POINT('',(-18.5239649837002,57.6273730232607,39.3343017080178));
#184948=CARTESIAN_POINT('',(-18.4850170109872,57.5075034888354,39.116));
#184949=CARTESIAN_POINT('',(-18.6259282908531,57.9411838150809,39.5248017080178));
#184950=CARTESIAN_POINT('Origin',(-18.6168352256568,57.9131965763112,39.1947745585637));
#184951=CARTESIAN_POINT('',(-18.672654168284,58.0849912788102,39.5248017080178));
#184952=CARTESIAN_POINT('',(-18.6728175489595,58.0854941128253,39.5248017080178));
#184953=CARTESIAN_POINT('',(-18.7746174535794,58.39880200336,39.3343017080178));
#184954=CARTESIAN_POINT('Origin',(-18.6817491043762,58.1129809527805,39.1947728594212));
#184955=CARTESIAN_POINT('',(-18.8135654100297,58.5186714877337,39.116));
#184956=CARTESIAN_POINT('',(-18.7746174535794,58.39880200336,39.3343017080178));
#184957=CARTESIAN_POINT('',(-18.937759626388,58.900901982832,39.116));
#184958=CARTESIAN_POINT('Origin',(-12.3000564958684,56.9509617460776,40.10025));
#184959=CARTESIAN_POINT('',(-12.2578193919762,57.7418065394567,40.10025));
#184960=CARTESIAN_POINT('',(-13.0516031943522,61.4762657165317,40.10025));
#184961=CARTESIAN_POINT('',(-12.0988124084934,56.9937374973464,40.10025));
#184962=CARTESIAN_POINT('',(-13.0814171332226,61.4699285681956,40.10025));
#184963=CARTESIAN_POINT('Origin',(-1.75271798929367E-17,-1.43793415203377E-16,
40.10025));
#184964=CARTESIAN_POINT('',(-12.2876333308465,57.7354693911206,40.10025));
#184965=CARTESIAN_POINT('',(-12.2729333410573,57.666311376549,40.10025));
#184966=CARTESIAN_POINT('Origin',(3.78171508600986E-16,7.48683896888049E-17,
40.10025));
#184967=CARTESIAN_POINT('Origin',(-0.18633711793979,-0.0396071771007813,
2.62394165870617E-17));
#184968=CARTESIAN_POINT('',(-12.6618058697513,58.6528587425324,39.116));
#184969=CARTESIAN_POINT('',(-12.5722344970954,58.2314585657882,39.3548010137695));
#184970=CARTESIAN_POINT('Origin',(-12.6538571933003,58.6154631599705,39.5550297832875));
#184971=CARTESIAN_POINT('',(-12.498155828738,57.8829458347212,39.92499));
#184972=CARTESIAN_POINT('',(-12.5722344970954,58.2314585657882,39.3548010137695));
#184973=CARTESIAN_POINT('',(-13.2134115091888,61.2479592423879,39.92499));
#184974=CARTESIAN_POINT('',(-13.2674241155254,61.5020685764506,39.92499));
#184975=CARTESIAN_POINT('',(-13.1393329438483,60.8994469905095,39.3548010137695));
#184976=CARTESIAN_POINT('',(-13.2134115091888,61.2479592423879,39.92499));
#184977=CARTESIAN_POINT('',(-13.0497616623169,60.4780472453829,39.116));
#184978=CARTESIAN_POINT('Origin',(-13.0577103643692,60.5154429483896,39.5550293907215));
#184979=CARTESIAN_POINT('',(-12.9663101637159,60.0854388089606,39.116));
#184980=CARTESIAN_POINT('',(-0.186337117939785,-0.0396071771007813,39.116));
#184981=CARTESIAN_POINT('',(-12.9401053405444,59.9621548122773,39.3343017080178));
#184982=CARTESIAN_POINT('',(-12.9663101630198,60.0854388091086,39.116));
#184983=CARTESIAN_POINT('',(-12.8715027735886,59.6394051101895,39.5248017080178));
#184984=CARTESIAN_POINT('Origin',(-12.8776205756126,59.6681895750056,39.1947747614283));
#184985=CARTESIAN_POINT('',(-12.8400648385932,59.4915012546306,39.5248017080178));
#184986=CARTESIAN_POINT('',(-0.186337117939785,-0.0396071771007813,39.5248017080178));
#184987=CARTESIAN_POINT('',(-12.7714622569314,59.1687514833562,39.3343017080178));
#184988=CARTESIAN_POINT('Origin',(-12.833945427478,59.4627141582908,39.1947728911885));
#184989=CARTESIAN_POINT('',(-12.7452574235141,59.0454674350476,39.116));
#184990=CARTESIAN_POINT('',(-12.7714622569314,59.1687514833562,39.3343017080178));
#184991=CARTESIAN_POINT('',(-0.186337117939785,-0.0396071771007813,39.116));
#184992=CARTESIAN_POINT('Origin',(0.18633711793979,0.0396071771007813,-2.62394165870617E-17));
#184993=CARTESIAN_POINT('',(-12.6770874264373,60.5572615995844,39.116));
#184994=CARTESIAN_POINT('',(-12.7666587073768,60.9786613448369,39.3548010137695));
#184995=CARTESIAN_POINT('Origin',(-12.6850361284299,60.5946573023103,39.5550293912455));
#184996=CARTESIAN_POINT('',(-12.8407372728669,61.3271735966835,39.92499));
#184997=CARTESIAN_POINT('',(-12.7666587073768,60.9786613448369,39.3548010137695));
#184998=CARTESIAN_POINT('',(-12.1254815933786,57.9621601888122,39.92499));
#184999=CARTESIAN_POINT('',(0.186337117939797,0.0396071771007757,39.92499));
#185000=CARTESIAN_POINT('',(-12.1995602619069,58.3106729198428,39.3548010137695));
#185001=CARTESIAN_POINT('',(-12.1254815933786,57.9621601888122,39.92499));
#185002=CARTESIAN_POINT('',(-12.2891316338718,58.7320730967339,39.116));
#185003=CARTESIAN_POINT('Origin',(-12.2811829573572,58.694677513873,39.5550297827296));
#185004=CARTESIAN_POINT('',(-12.3725831883604,59.1246817890949,39.116));
#185005=CARTESIAN_POINT('',(-12.387939103104,59.1969256915255,39.116));
#185006=CARTESIAN_POINT('',(-12.3987880210518,59.2479658375578,39.3343017080178));
#185007=CARTESIAN_POINT('',(-12.3725831876346,59.1246817892491,39.116));
#185008=CARTESIAN_POINT('',(-12.4673906027137,59.5707156088322,39.5248017080178));
#185009=CARTESIAN_POINT('Origin',(-12.4612728133405,59.5419312029573,39.1947745585561));
#185010=CARTESIAN_POINT('',(-12.498828537709,59.718619464391,39.5248017080178));
#185011=CARTESIAN_POINT('',(-12.4989384629011,59.7191366217597,39.5248017080178));
#185012=CARTESIAN_POINT('',(-12.5674311046648,60.0413691664788,39.3343017080178));
#185013=CARTESIAN_POINT('Origin',(-12.5049479331823,59.7474064876929,39.1947728594233));
#185014=CARTESIAN_POINT('',(-12.5936359271402,60.1646531633102,39.116));
#185015=CARTESIAN_POINT('',(-12.5674311046648,60.0413691664788,39.3343017080178));
#185016=CARTESIAN_POINT('',(-12.67719582832,60.5577715903456,39.116));
#185017=CARTESIAN_POINT('Origin',(-6.27967898647548,57.9246844223736,40.10025));
#185018=CARTESIAN_POINT('',(-6.15500747092256,58.7067819056644,40.10025));
#185019=CARTESIAN_POINT('',(-6.55408556365883,62.5037563256535,40.10025));
#185020=CARTESIAN_POINT('',(-6.07506605172241,57.9461901084062,40.10025));
#185021=CARTESIAN_POINT('',(-6.58439859102965,62.5005702980932,40.10025));
#185022=CARTESIAN_POINT('Origin',(-3.27251186835868E-17,-1.46200532232821E-16,
40.10025));
#185023=CARTESIAN_POINT('',(-6.18532049829339,58.7035958781039,40.10025));
#185024=CARTESIAN_POINT('',(-6.17793001757209,58.6332801510296,40.10025));
#185025=CARTESIAN_POINT('Origin',(3.86084563605879E-16,7.61216944770113E-17,
40.10025));
#185026=CARTESIAN_POINT('Origin',(-0.189456421067656,-0.0199126722524861,
2.66786672051798E-17));
#185027=CARTESIAN_POINT('',(-6.46154998175858,59.6550713551493,39.116));
#185028=CARTESIAN_POINT('',(-6.41651760334991,59.2266168947287,39.3548010137695));
#185029=CARTESIAN_POINT('Origin',(-6.45755375176684,59.617049766565,39.5550297832836));
#185030=CARTESIAN_POINT('',(-6.37927424589634,58.8722700235037,39.92499));
#185031=CARTESIAN_POINT('',(-6.4165176033499,59.2266168947287,39.3548010137695));
#185032=CARTESIAN_POINT('',(-6.7388720005127,62.293614112757,39.92499));
#185033=CARTESIAN_POINT('',(-6.76602706194884,62.5519772640373,39.92499));
#185034=CARTESIAN_POINT('',(-6.70162869542298,61.9392677288637,39.3548010137695));
#185035=CARTESIAN_POINT('',(-6.7388720005127,62.293614112757,39.92499));
#185036=CARTESIAN_POINT('',(-6.65659636252321,61.5108137072213,39.116));
#185037=CARTESIAN_POINT('Origin',(-6.66059260538601,61.5488354182655,39.55502939072));
#185038=CARTESIAN_POINT('',(-6.61464077648821,61.1116329639869,39.116));
#185039=CARTESIAN_POINT('',(-0.189456421067651,-0.0199126722524861,39.116));
#185040=CARTESIAN_POINT('',(-6.60146619279885,60.9862851800405,39.3343017080178));
#185041=CARTESIAN_POINT('',(-6.6146407757806,61.1116329640613,39.116));
#185042=CARTESIAN_POINT('',(-6.56697596826216,60.6581326136905,39.5248017080178));
#185043=CARTESIAN_POINT('Origin',(-6.57005146045362,60.6873988786426,39.1947747614312));
#185044=CARTESIAN_POINT('',(-6.55117041629707,60.5077528318944,39.5248017080178));
#185045=CARTESIAN_POINT('',(-0.189456421067651,-0.0199126722524861,39.5248017080178));
#185046=CARTESIAN_POINT('',(-6.51668018436685,60.1796001951996,39.3343017080178));
#185047=CARTESIAN_POINT('Origin',(-6.54809359889826,60.4784837816373,39.1947728911934));
#185048=CARTESIAN_POINT('',(-6.50350559588404,60.0542523588398,39.116));
#185049=CARTESIAN_POINT('',(-6.51668018436685,60.1796001951996,39.3343017080178));
#185050=CARTESIAN_POINT('',(-0.189456421067651,-0.0199126722524861,39.116));
#185051=CARTESIAN_POINT('Origin',(0.189456421067656,0.0199126722524861,
-2.66786672051798E-17));
#185052=CARTESIAN_POINT('',(-6.2776835203879,61.5506390517263,39.116));
#185053=CARTESIAN_POINT('',(-6.32271585268577,61.979093073432,39.3548010137695));
#185054=CARTESIAN_POINT('Origin',(-6.28167976322052,61.5886607624834,39.5550293912467));
#185055=CARTESIAN_POINT('',(-6.35995915792738,62.3334394573093,39.92499));
#185056=CARTESIAN_POINT('',(-6.32271585268577,61.979093073432,39.3548010137695));
#185057=CARTESIAN_POINT('',(-6.00036140428986,58.9120953679531,39.92499));
#185058=CARTESIAN_POINT('',(0.189456421067662,0.0199126722524805,39.92499));
#185059=CARTESIAN_POINT('',(-6.03760476191729,59.2664422391598,39.3548010137695));
#185060=CARTESIAN_POINT('',(-6.00036140428986,58.9120953679531,39.92499));
#185061=CARTESIAN_POINT('',(-6.08263713962327,59.6948966996543,39.116));
#185062=CARTESIAN_POINT('Origin',(-6.07864090959991,59.6568751107691,39.5550297827311));
#185063=CARTESIAN_POINT('',(-6.12459275448616,60.0940777032672,39.116));
#185064=CARTESIAN_POINT('',(-6.13231300382116,60.1675309762115,39.116));
#185065=CARTESIAN_POINT('',(-6.13776734223154,60.2194255397046,39.3343017080178));
#185066=CARTESIAN_POINT('',(-6.12459275374873,60.0940777033447,39.116));
#185067=CARTESIAN_POINT('',(-6.17225757416176,60.5475781763994,39.5248017080178));
#185068=CARTESIAN_POINT('Origin',(-6.16918208839087,60.5183119713883,39.1947745585589));
#185069=CARTESIAN_POINT('',(-6.18806312612685,60.6979579581955,39.5248017080178));
#185070=CARTESIAN_POINT('',(-6.18811839147226,60.6984837728334,39.5248017080178));
#185071=CARTESIAN_POINT('',(-6.22255335066353,61.0261105245455,39.3343017080178));
#185072=CARTESIAN_POINT('Origin',(-6.19113993560366,60.7272269341761,39.1947728594228));
#185073=CARTESIAN_POINT('',(-6.23572793364529,61.1514583085663,39.116));
#185074=CARTESIAN_POINT('',(-6.22255335066353,61.0261105245455,39.3343017080178));
#185075=CARTESIAN_POINT('',(-6.27773801988317,61.5511575797869,39.116));
#185076=CARTESIAN_POINT('Origin',(-0.190499999999384,58.2637721346185,40.10025));
#185077=CARTESIAN_POINT('',(0.0152400000006159,58.2637721346185,40.10025));
#185078=CARTESIAN_POINT('',(-0.0152399999993768,58.9578504383728,40.10025));
#185079=CARTESIAN_POINT('Origin',(-0.1905,1.99538158514885E-15,2.68256207625279E-17));
#185080=CARTESIAN_POINT('',(-0.190499999999366,60.0036905223731,39.116));
#185081=CARTESIAN_POINT('',(-0.19049999999937,59.5728760150042,39.3548010137695));
#185082=CARTESIAN_POINT('Origin',(-0.190499999999367,59.9654595002486,39.5550297832821));
#185083=CARTESIAN_POINT('',(-0.190499999467978,59.2165773020941,39.92499));
#185084=CARTESIAN_POINT('',(-0.19049999999937,59.5728760150042,39.3548010137695));
#185085=CARTESIAN_POINT('',(-0.190499999999337,62.6567671111299,39.92499));
#185086=CARTESIAN_POINT('',(-0.190499999999335,62.9165533988763,39.92499));
#185087=CARTESIAN_POINT('',(-0.190500000605309,62.3004688883555,39.3548010137695));
#185088=CARTESIAN_POINT('',(-0.190499999999338,62.6567671111299,39.92499));
#185089=CARTESIAN_POINT('',(-0.190499999999346,61.8696548221181,39.116));
#185090=CARTESIAN_POINT('Origin',(-0.190499999999346,61.9078859673755,39.5550293907214));
#185091=CARTESIAN_POINT('',(-0.190500000711194,61.4682752798284,39.116));
#185092=CARTESIAN_POINT('',(-0.190499999999995,1.99538158514885E-15,39.116));
#185093=CARTESIAN_POINT('',(-0.190499999999352,61.3422370451705,39.3343017080178));
#185094=CARTESIAN_POINT('',(-0.190499999999351,61.4682752798284,39.116));
#185095=CARTESIAN_POINT('',(-0.190499999999355,61.0122769227456,39.5248017080178));
#185096=CARTESIAN_POINT('Origin',(-0.190499486621753,61.0417043405088,39.1947747614311));
#185097=CARTESIAN_POINT('',(-0.190499999999357,60.8610688070707,39.5248017080178));
#185098=CARTESIAN_POINT('',(-0.190499999999994,1.99538158514885E-15,39.5248017080178));
#185099=CARTESIAN_POINT('',(-0.19049999999936,60.5311086139135,39.3343017080178));
#185100=CARTESIAN_POINT('Origin',(-0.190499486572862,60.831638480743,39.1947728911869));
#185101=CARTESIAN_POINT('',(-0.190499999999362,60.4050703266283,39.116));
#185102=CARTESIAN_POINT('',(-0.19049999999936,60.5311086139135,39.3343017080178));
#185103=CARTESIAN_POINT('',(-0.190499999999995,1.99538158514885E-15,39.116));
#185104=CARTESIAN_POINT('Origin',(0.1905,-1.99538158514885E-15,-2.68256207625279E-17));
#185105=CARTESIAN_POINT('',(0.190500000000654,61.8696548221181,39.116));
#185106=CARTESIAN_POINT('',(0.190500000000659,62.3004688883554,39.3548010137695));
#185107=CARTESIAN_POINT('Origin',(0.190500000000654,61.9078859670887,39.5550293912442));
#185108=CARTESIAN_POINT('',(0.190500000452942,62.6567671111299,39.92499));
#185109=CARTESIAN_POINT('',(0.190500000000658,62.3004688883554,39.3548010137695));
#185110=CARTESIAN_POINT('',(0.190500000000626,59.2165773020941,39.92499));
#185111=CARTESIAN_POINT('',(0.190500000000006,-7.61749518455946E-15,39.92499));
#185112=CARTESIAN_POINT('',(0.190499999294509,59.5728760150042,39.3548010137695));
#185113=CARTESIAN_POINT('',(0.190500000000626,59.2165773020941,39.92499));
#185114=CARTESIAN_POINT('',(0.190500000000634,60.0036905223731,39.116));
#185115=CARTESIAN_POINT('Origin',(0.190500000000634,59.9654594999465,39.5550297827309));
#185116=CARTESIAN_POINT('',(0.190499999259078,60.4050703266283,39.116));
#185117=CARTESIAN_POINT('',(0.190500000000639,60.4789282006569,39.116));
#185118=CARTESIAN_POINT('',(0.19050000000064,60.5311086139135,39.3343017080178));
#185119=CARTESIAN_POINT('',(0.190500000000638,60.4050703266283,39.116));
#185120=CARTESIAN_POINT('',(0.190500000000643,60.8610688070707,39.5248017080178));
#185121=CARTESIAN_POINT('Origin',(0.190499486503203,60.8316414495916,39.1947745585591));
#185122=CARTESIAN_POINT('',(0.190500000000645,61.0122769227456,39.5248017080178));
#185123=CARTESIAN_POINT('',(0.190500000000645,61.0128056337175,39.5248017080178));
#185124=CARTESIAN_POINT('',(0.190500000000648,61.3422370451705,39.3343017080178));
#185125=CARTESIAN_POINT('Origin',(0.190499486688745,61.0417071743813,39.1947728594256));
#185126=CARTESIAN_POINT('',(0.190500000000649,61.4682752798284,39.116));
#185127=CARTESIAN_POINT('',(0.190500000000648,61.3422370451705,39.3343017080178));
#185128=CARTESIAN_POINT('',(0.190500000000654,61.8701762063762,39.116));
#185129=CARTESIAN_POINT('Origin',(5.90076614434134,57.9645097668784,40.10025));
#185130=CARTESIAN_POINT('',(6.18532049829458,58.7035958781038,40.10025));
#185131=CARTESIAN_POINT('',(6.58439859103091,62.500570298093,40.10025));
#185132=CARTESIAN_POINT('',(6.10537907909441,57.9430040808457,40.10025));
#185133=CARTESIAN_POINT('',(6.55408556366009,62.5037563256534,40.10025));
#185134=CARTESIAN_POINT('Origin',(5.63142687537637E-15,5.54868405209867E-15,
40.10025));
#185135=CARTESIAN_POINT('',(6.15500747092375,58.7067819056642,40.10025));
#185136=CARTESIAN_POINT('',(6.14761699020245,58.6364661785899,40.10025));
#185137=CARTESIAN_POINT('Origin',(5.65479388299727E-15,5.32882958889813E-15,
40.10025));
#185138=CARTESIAN_POINT('Origin',(-0.189456421067656,0.0199126722524899,
2.66786672051798E-17));
#185139=CARTESIAN_POINT('',(6.08263713962448,59.6948966996542,39.116));
#185140=CARTESIAN_POINT('',(6.03760476121579,59.2664422392335,39.3548010137695));
#185141=CARTESIAN_POINT('Origin',(6.07864090963279,59.6568751110704,39.5550297832848));
#185142=CARTESIAN_POINT('',(6.00036140481959,58.9120953678974,39.92499));
#185143=CARTESIAN_POINT('',(6.03760476121579,59.2664422392335,39.3548010137695));
#185144=CARTESIAN_POINT('',(6.35995915837865,62.3334394572618,39.92499));
#185145=CARTESIAN_POINT('',(6.38711421981479,62.5918026085421,39.92499));
#185146=CARTESIAN_POINT('',(6.32271585208515,61.9790930734951,39.3548010137695));
#185147=CARTESIAN_POINT('',(6.35995915837864,62.3334394572618,39.92499));
#185148=CARTESIAN_POINT('',(6.27768352038914,61.5506390517261,39.116));
#185149=CARTESIAN_POINT('Origin',(6.28167976325196,61.5886607627705,39.5550293907198));
#185150=CARTESIAN_POINT('',(6.23572793293866,61.1514583086406,39.116));
#185151=CARTESIAN_POINT('',(-0.18945642106765,0.0199126722524899,39.116));
#185152=CARTESIAN_POINT('',(6.22255335066477,61.0261105245453,39.3343017080178));
#185153=CARTESIAN_POINT('',(6.23572793364653,61.1514583085662,39.116));
#185154=CARTESIAN_POINT('',(6.18806312612808,60.6979579581953,39.5248017080178));
#185155=CARTESIAN_POINT('Origin',(6.19113963945,60.7272241158218,39.1947747614305));
#185156=CARTESIAN_POINT('',(6.17225757416298,60.5475781763993,39.5248017080178));
#185157=CARTESIAN_POINT('',(-0.18945642106765,0.0199126722524899,39.5248017080178));
#185158=CARTESIAN_POINT('',(6.13776734223276,60.2194255397044,39.3343017080178));
#185159=CARTESIAN_POINT('Origin',(6.16918177799204,60.5183090188076,39.1947728911921));
#185160=CARTESIAN_POINT('',(6.12459275374995,60.0940777033446,39.116));
#185161=CARTESIAN_POINT('',(6.13776734223276,60.2194255397044,39.3343017080178));
#185162=CARTESIAN_POINT('',(-0.18945642106765,0.0199126722524899,39.116));
#185163=CARTESIAN_POINT('Origin',(0.189456421067656,-0.0199126722524899,
-2.66786672051798E-17));
#185164=CARTESIAN_POINT('',(6.65659636252446,61.5108137072211,39.116));
#185165=CARTESIAN_POINT('',(6.70162869482234,61.9392677289268,39.3548010137695));
#185166=CARTESIAN_POINT('Origin',(6.66059260535715,61.548835417979,39.5550293912451));
#185167=CARTESIAN_POINT('',(6.73887200096445,62.2936141127095,39.92499));
#185168=CARTESIAN_POINT('',(6.70162869482234,61.9392677289269,39.3548010137695));
#185169=CARTESIAN_POINT('',(6.37927424642637,58.872270023448,39.92499));
#185170=CARTESIAN_POINT('',(0.189456421067661,-0.0199126722524955,39.92499));
#185171=CARTESIAN_POINT('',(6.41651760264858,59.2266168948024,39.3548010137695));
#185172=CARTESIAN_POINT('',(6.37927424642637,58.872270023448,39.92499));
#185173=CARTESIAN_POINT('',(6.46154998175979,59.6550713551492,39.116));
#185174=CARTESIAN_POINT('Origin',(6.45755375173627,59.6170497662626,39.555029782729));
#185175=CARTESIAN_POINT('',(6.50350559514777,60.0542523589171,39.116));
#185176=CARTESIAN_POINT('',(6.51122584595768,60.1277056317064,39.116));
#185177=CARTESIAN_POINT('',(6.51668018436807,60.1796001951995,39.3343017080178));
#185178=CARTESIAN_POINT('',(6.50350559588526,60.0542523588396,39.116));
#185179=CARTESIAN_POINT('',(6.5511704162983,60.5077528318943,39.5248017080178));
#185180=CARTESIAN_POINT('Origin',(6.54809390915835,60.4784867342318,39.1947745585617));
#185181=CARTESIAN_POINT('',(6.56697596826339,60.6581326136904,39.5248017080178));
#185182=CARTESIAN_POINT('',(6.5670312336088,60.6586584283283,39.5248017080178));
#185183=CARTESIAN_POINT('',(6.60146619280008,60.9862851800404,39.3343017080178));
#185184=CARTESIAN_POINT('Origin',(6.57005175674075,60.6874016969861,39.1947728594294));
#185185=CARTESIAN_POINT('',(6.61464077578184,61.1116329640612,39.116));
#185186=CARTESIAN_POINT('',(6.60146619280008,60.9862851800404,39.3343017080178));
#185187=CARTESIAN_POINT('',(6.65665086201973,61.5113322352818,39.116));
#185188=CARTESIAN_POINT('Origin',(11.92738225999,57.0301761002789,40.10025));
#185189=CARTESIAN_POINT('',(12.2876333308477,57.7354693911203,40.10025));
#185190=CARTESIAN_POINT('',(13.0814171332239,61.4699285681953,40.10025));
#185191=CARTESIAN_POINT('',(12.128626347365,56.9874003490101,40.10025));
#185192=CARTESIAN_POINT('',(13.0516031943535,61.4762657165314,40.10025));
#185193=CARTESIAN_POINT('Origin',(5.61622893658571E-15,5.55109116912811E-15,
40.10025));
#185194=CARTESIAN_POINT('',(12.2578193919774,57.7418065394565,40.10025));
#185195=CARTESIAN_POINT('',(12.2431194021881,57.6726485248849,40.10025));
#185196=CARTESIAN_POINT('Origin',(5.66270693800216E-15,5.32757628410993E-15,
40.10025));
#185197=CARTESIAN_POINT('Origin',(-0.18633711793979,0.0396071771007852,
2.62394165870616E-17));
#185198=CARTESIAN_POINT('',(12.289131633873,58.7320730967337,39.116));
#185199=CARTESIAN_POINT('',(12.1995602612171,58.3106729199895,39.3548010137695));
#185200=CARTESIAN_POINT('Origin',(12.2811829574215,58.6946775141693,39.5550297832828));
#185201=CARTESIAN_POINT('',(12.1254815939001,57.9621601887014,39.92499));
#185202=CARTESIAN_POINT('',(12.1995602612171,58.3106729199895,39.3548010137695));
#185203=CARTESIAN_POINT('',(12.8407372733105,61.3271735965892,39.92499));
#185204=CARTESIAN_POINT('',(12.8947498796471,61.5812829306519,39.92499));
#185205=CARTESIAN_POINT('',(12.7666587067863,60.9786613449624,39.3548010137695));
#185206=CARTESIAN_POINT('',(12.8407372733105,61.3271735965892,39.92499));
#185207=CARTESIAN_POINT('',(12.6770874264386,60.5572615995842,39.116));
#185208=CARTESIAN_POINT('Origin',(12.685036128491,60.5946573025912,39.5550293907214));
#185209=CARTESIAN_POINT('',(12.5936359264456,60.1646531634578,39.116));
#185210=CARTESIAN_POINT('',(-0.186337117939784,0.0396071771007852,39.116));
#185211=CARTESIAN_POINT('',(12.5674311046661,60.0413691664786,39.3343017080178));
#185212=CARTESIAN_POINT('',(12.5936359271415,60.1646531633099,39.116));
#185213=CARTESIAN_POINT('',(12.4988285377103,59.7186194643908,39.5248017080178));
#185214=CARTESIAN_POINT('Origin',(12.5049473440533,59.7474037157363,39.1947747614349));
#185215=CARTESIAN_POINT('',(12.4673906027149,59.5707156088319,39.5248017080178));
#185216=CARTESIAN_POINT('',(-0.186337117939784,0.0396071771007852,39.5248017080178));
#185217=CARTESIAN_POINT('',(12.398788021053,59.2479658375575,39.3343017080178));
#185218=CARTESIAN_POINT('Origin',(12.4612721960133,59.5419282989966,39.1947728911891));
#185219=CARTESIAN_POINT('',(12.3725831876358,59.1246817892489,39.116));
#185220=CARTESIAN_POINT('',(12.398788021053,59.2479658375575,39.3343017080178));
#185221=CARTESIAN_POINT('',(-0.186337117939784,0.0396071771007852,39.116));
#185222=CARTESIAN_POINT('Origin',(0.18633711793979,-0.0396071771007852,
-2.62394165870616E-17));
#185223=CARTESIAN_POINT('',(13.0497616623182,60.4780472453826,39.116));
#185224=CARTESIAN_POINT('',(13.1393329432576,60.8994469906351,39.3548010137695));
#185225=CARTESIAN_POINT('Origin',(13.0577103643107,60.5154429481081,39.555029391246));
#185226=CARTESIAN_POINT('',(13.2134115096326,61.2479592422935,39.92499));
#185227=CARTESIAN_POINT('',(13.1393329432576,60.8994469906351,39.3548010137695));
#185228=CARTESIAN_POINT('',(12.4981558292594,57.8829458346104,39.92499));
#185229=CARTESIAN_POINT('',(0.186337117939794,-0.0396071771007907,39.92499));
#185230=CARTESIAN_POINT('',(12.5722344964052,58.2314585659349,39.3548010137695));
#185231=CARTESIAN_POINT('',(12.4981558292594,57.8829458346104,39.92499));
#185232=CARTESIAN_POINT('',(12.6618058697526,58.6528587425321,39.116));
#185233=CARTESIAN_POINT('Origin',(12.6538571932381,58.6154631596714,39.5550297827299));
#185234=CARTESIAN_POINT('',(12.74525742279,59.0454674352015,39.116));
#185235=CARTESIAN_POINT('',(12.7606133389849,59.1177113373237,39.116));
#185236=CARTESIAN_POINT('',(12.7714622569326,59.1687514833559,39.3343017080178));
#185237=CARTESIAN_POINT('',(12.7452574235154,59.0454674350473,39.116));
#185238=CARTESIAN_POINT('',(12.8400648385945,59.4915012546304,39.5248017080178));
#185239=CARTESIAN_POINT('Origin',(12.8339460446679,59.4627170622758,39.1947745585633));
#185240=CARTESIAN_POINT('',(12.8715027735898,59.6394051101892,39.5248017080178));
#185241=CARTESIAN_POINT('',(12.871612698782,59.6399222675579,39.5248017080178));
#185242=CARTESIAN_POINT('',(12.9401053405456,59.962154812277,39.3343017080178));
#185243=CARTESIAN_POINT('Origin',(12.8776211648729,59.668192346935,39.1947728594185));
#185244=CARTESIAN_POINT('',(12.966310163021,60.0854388091083,39.116));
#185245=CARTESIAN_POINT('',(12.9401053405456,59.962154812277,39.3343017080178));
#185246=CARTESIAN_POINT('',(13.0498700642008,60.4785572361437,39.116));
#185247=CARTESIAN_POINT('Origin',(17.823319479633,55.4710078899932,40.10025));
#185248=CARTESIAN_POINT('',(18.2553202812755,56.134781019564,40.10025));
#185249=CARTESIAN_POINT('',(19.4351129318427,59.7658094374949,40.10025));
#185250=CARTESIAN_POINT('',(18.0189898472955,55.4074307335705,40.10025));
#185251=CARTESIAN_POINT('',(19.406124729226,59.7752282754835,40.10025));
#185252=CARTESIAN_POINT('Origin',(5.60136586593793E-15,5.55507371690523E-15,
40.10025));
#185253=CARTESIAN_POINT('',(18.2263320786588,56.1441998575526,40.10025));
#185254=CARTESIAN_POINT('',(18.2044836359659,56.0769572651636,40.10025));
#185255=CARTESIAN_POINT('Origin',(5.67044563844026E-15,5.32550270557707E-15,
40.10025));
#185256=CARTESIAN_POINT('Origin',(-0.181176266354226,0.0588677374284294,
2.55126814298647E-17));
#185257=CARTESIAN_POINT('',(18.3609838302746,57.1257686104889,39.116));
#185258=CARTESIAN_POINT('',(18.2278548260744,56.7160396659412,39.3548010137695));
#185259=CARTESIAN_POINT('Origin',(18.3491697947263,57.0894087477743,39.5550297832854));
#185260=CARTESIAN_POINT('',(18.1177524692166,56.3771794531163,39.92499));
#185261=CARTESIAN_POINT('',(18.2278548260744,56.7160396659412,39.3548010137695));
#185262=CARTESIAN_POINT('',(19.1808295835788,59.6489943884562,39.92499));
#185263=CARTESIAN_POINT('',(19.261107961398,59.8960658302615,39.92499));
#185264=CARTESIAN_POINT('',(19.0707273771003,59.3101346421292,39.3548010137695));
#185265=CARTESIAN_POINT('',(19.1808295835788,59.6489943884562,39.92499));
#185266=CARTESIAN_POINT('',(18.9375985097928,58.9004061169355,39.116));
#185267=CARTESIAN_POINT('Origin',(18.9494125833917,58.9367660967579,39.555029390722));
#185268=CARTESIAN_POINT('',(18.8135654093542,58.5186714879532,39.116));
#185269=CARTESIAN_POINT('',(-0.181176266354221,0.0588677374284294,39.116));
#185270=CARTESIAN_POINT('',(18.7746174535806,58.3988020033596,39.3343017080178));
#185271=CARTESIAN_POINT('',(18.8135654100308,58.5186714877334,39.116));
#185272=CARTESIAN_POINT('',(18.6726541682852,58.0849912788098,39.5248017080178));
#185273=CARTESIAN_POINT('Origin',(18.6817482287252,58.1129782575874,39.1947747614284));
#185274=CARTESIAN_POINT('',(18.6259282908542,57.9411838150805,39.5248017080178));
#185275=CARTESIAN_POINT('',(-0.181176266354221,0.0588677374284294,39.5248017080178));
#185276=CARTESIAN_POINT('',(18.5239649837014,57.6273730232603,39.3343017080178));
#185277=CARTESIAN_POINT('Origin',(18.6168343081661,57.913193752791,39.1947728911888));
#185278=CARTESIAN_POINT('',(18.4850170109884,57.5075034888351,39.116));
#185279=CARTESIAN_POINT('',(18.5239649837014,57.6273730232603,39.3343017080178));
#185280=CARTESIAN_POINT('',(-0.181176266354221,0.0588677374284294,39.116));
#185281=CARTESIAN_POINT('Origin',(0.181176266354226,-0.0588677374284294,
-2.55126814298647E-17));
#185282=CARTESIAN_POINT('',(19.2999510425012,58.7826706420786,39.116));
#185283=CARTESIAN_POINT('',(19.4330799103844,59.1923991670853,39.3548010137695));
#185284=CARTESIAN_POINT('Origin',(19.3117651160114,58.8190306216277,39.5550293912458));
#185285=CARTESIAN_POINT('',(19.5431821167173,59.5312589134596,39.92499));
#185286=CARTESIAN_POINT('',(19.4330799103844,59.1923991670853,39.3548010137695));
#185287=CARTESIAN_POINT('',(18.4801050014197,56.2594439784237,39.92499));
#185288=CARTESIAN_POINT('',(0.18117626635423,-0.0588677374284347,39.92499));
#185289=CARTESIAN_POINT('',(18.5902073581112,56.5983041913026,39.3548010137695));
#185290=CARTESIAN_POINT('',(18.4801050014197,56.2594439784237,39.92499));
#185291=CARTESIAN_POINT('',(18.7233363629831,57.008033135632,39.116));
#185292=CARTESIAN_POINT('Origin',(18.7115223273417,56.9716732726309,39.5550297827351));
#185293=CARTESIAN_POINT('',(18.8473695429913,57.3897680142074,39.116));
#185294=CARTESIAN_POINT('',(18.8701928819401,57.4600110263528,39.116));
#185295=CARTESIAN_POINT('',(18.8863175164099,57.5096375484035,39.3343017080178));
#185296=CARTESIAN_POINT('',(18.8473695436968,57.3897680139782,39.116));
#185297=CARTESIAN_POINT('',(18.9882808235627,57.8234483402237,39.5248017080178));
#185298=CARTESIAN_POINT('Origin',(18.979186781637,57.7954614188152,39.1947745585588));
#185299=CARTESIAN_POINT('',(19.0350067009936,57.967255803953,39.5248017080178));
#185300=CARTESIAN_POINT('',(19.0351700816691,57.9677586379681,39.5248017080178));
#185301=CARTESIAN_POINT('',(19.136969986289,58.2810665285028,39.3343017080178));
#185302=CARTESIAN_POINT('Origin',(19.0441006607092,57.9952457951693,39.1947728594247));
#185303=CARTESIAN_POINT('',(19.1759179427393,58.4009360128765,39.116));
#185304=CARTESIAN_POINT('',(19.136969986289,58.2810665285028,39.3343017080178));
#185305=CARTESIAN_POINT('',(19.3001121590976,58.7831665079748,39.116));
#185306=CARTESIAN_POINT('Origin',(23.5239806812878,53.30408770921,40.10025));
#185307=CARTESIAN_POINT('',(24.0229981225303,53.9190682401992,40.10025));
#185308=CARTESIAN_POINT('',(25.5758735661215,57.4068835917977,40.10025));
#185309=CARTESIAN_POINT('',(23.7119335237431,53.2204057122635,40.10025));
#185310=CARTESIAN_POINT('',(25.5480287005725,57.4192809246786,40.10025));
#185311=CARTESIAN_POINT('Origin',(5.58700050634534E-15,5.56058806180318E-15,
40.10025));
#185312=CARTESIAN_POINT('',(23.9951532569813,53.9314655730802,40.10025));
#185313=CARTESIAN_POINT('',(23.966395737495,53.8668751267876,40.10025));
#185314=CARTESIAN_POINT('Origin',(5.67792519749014E-15,5.3226315718599E-15,
40.10025));
#185315=CARTESIAN_POINT('Origin',(-0.174030409680915,0.0774833305059419,
2.45064239960503E-17));
#185316=CARTESIAN_POINT('',(24.2316692455489,54.893582249012,39.116));
#185317=CARTESIAN_POINT('',(24.0564411990333,54.5000136127186,39.3548010137695));
#185318=CARTESIAN_POINT('Origin',(24.216119287949,54.8586564724098,39.5550297832835));
#185319=CARTESIAN_POINT('',(23.9115214570975,54.1745185417596,39.92499));
#185320=CARTESIAN_POINT('',(24.0564411990333,54.5000136127186,39.3548010137695));
#185321=CARTESIAN_POINT('',(25.3107727110829,57.3172883154487,39.92499));
#185322=CARTESIAN_POINT('',(25.416437313678,57.5546148985773,39.92499));
#185323=CARTESIAN_POINT('',(25.1658531674639,56.9917936927136,39.3548010137695));
#185324=CARTESIAN_POINT('',(25.3107727110829,57.3172883154487,39.92499));
#185325=CARTESIAN_POINT('',(24.9906253009265,56.5982254591673,39.116));
#185326=CARTESIAN_POINT('Origin',(25.0061753086094,56.6331513482574,39.5550293907218));
#185327=CARTESIAN_POINT('',(24.827369532646,56.2315470018075,39.116));
#185328=CARTESIAN_POINT('',(-0.174030409680909,0.0774833305059419,39.116));
#185329=CARTESIAN_POINT('',(24.7761051648324,56.1164053447569,39.3343017080178));
#185330=CARTESIAN_POINT('',(24.8273695332963,56.2315470015179,39.116));
#185331=CARTESIAN_POINT('',(24.6418982922884,55.8149717737124,39.5248017080178));
#185332=CARTESIAN_POINT('Origin',(24.6538679703961,55.8418548487275,39.1947747614258));
#185333=CARTESIAN_POINT('',(24.5803964109129,55.6768362864789,39.5248017080178));
#185334=CARTESIAN_POINT('',(-0.174030409680909,0.0774833305059419,39.5248017080178));
#185335=CARTESIAN_POINT('',(24.4461895095995,55.3754026508172,39.3343017080178));
#185336=CARTESIAN_POINT('Origin',(24.5684264878148,55.6499501367125,39.1947728911925));
#185337=CARTESIAN_POINT('',(24.3949251197301,55.2602609459788,39.116));
#185338=CARTESIAN_POINT('',(24.4461895095995,55.3754026508172,39.3343017080178));
#185339=CARTESIAN_POINT('',(-0.174030409680909,0.0774833305059419,39.116));
#185340=CARTESIAN_POINT('Origin',(0.174030409680915,-0.0774833305059419,
-2.45064239960503E-17));
#185341=CARTESIAN_POINT('',(25.3386861202883,56.4432587981554,39.116));
#185342=CARTESIAN_POINT('',(25.5139139873796,56.8368270314551,39.3548010137695));
#185343=CARTESIAN_POINT('Origin',(25.3542361278548,56.4781846869841,39.5550293912436));
#185344=CARTESIAN_POINT('',(25.6588335308583,57.1623216542527,39.92499));
#185345=CARTESIAN_POINT('',(25.5139139873796,56.8368270314551,39.3548010137695));
#185346=CARTESIAN_POINT('',(24.2595822759739,54.0195518809638,39.92499));
#185347=CARTESIAN_POINT('',(0.174030409680918,-0.077483330505947,39.92499));
#185348=CARTESIAN_POINT('',(24.4045020177506,54.3450469519937,39.3548010137695));
#185349=CARTESIAN_POINT('',(24.2595822759739,54.0195518809638,39.92499));
#185350=CARTESIAN_POINT('',(24.5797300649108,54.7386155880001,39.116));
#185351=CARTESIAN_POINT('Origin',(24.5641801071874,54.7036898111209,39.5550297827301));
#185352=CARTESIAN_POINT('',(24.7429859384139,55.1052942852688,39.116));
#185353=CARTESIAN_POINT('',(24.773026642839,55.1727668102968,39.116));
#185354=CARTESIAN_POINT('',(24.7942503289613,55.2204359898053,39.3343017080178));
#185355=CARTESIAN_POINT('',(24.7429859390919,55.1052942849669,39.116));
#185356=CARTESIAN_POINT('',(24.9284572302748,55.521869625467,39.5248017080178));
#185357=CARTESIAN_POINT('Origin',(24.9164875765758,55.4949866055697,39.1947745585588));
#185358=CARTESIAN_POINT('',(24.9899591116502,55.6600051127005,39.5248017080178));
#185359=CARTESIAN_POINT('',(24.9901741577761,55.6604881142073,39.5248017080178));
#185360=CARTESIAN_POINT('',(25.1241659841942,55.961438683745,39.3343017080178));
#185361=CARTESIAN_POINT('Origin',(25.0019290044727,55.6868911941847,39.1947728594294));
#185362=CARTESIAN_POINT('',(25.1754303526582,56.076580340506,39.116));
#185363=CARTESIAN_POINT('',(25.1241659841942,55.961438683745,39.3343017080178));
#185364=CARTESIAN_POINT('',(25.3388981863712,56.4437351063761,39.116));
#185365=CARTESIAN_POINT('Origin',(28.9669082278889,50.5531567888872,40.10025));
#185366=CARTESIAN_POINT('',(29.5274749692191,51.1126068659043,40.10025));
#185367=CARTESIAN_POINT('',(31.4364195775141,54.4189959163059,40.10025));
#185368=CARTESIAN_POINT('',(29.1450842944635,50.4502867888872,40.10025));
#185369=CARTESIAN_POINT('',(31.4100231232068,54.4342359163059,40.10025));
#185370=CARTESIAN_POINT('Origin',(5.57329024769379E-15,5.5675737875053E-15,
40.10025));
#185371=CARTESIAN_POINT('',(29.5010785149117,51.1278468659043,40.10025));
#185372=CARTESIAN_POINT('',(29.4657269920333,51.0666162321541,40.10025));
#185373=CARTESIAN_POINT('Origin',(5.68506366753766E-15,5.31899433970023E-15,
40.10025));
#185374=CARTESIAN_POINT('Origin',(-0.164977839420934,0.0952500000000019,
2.32316690526363E-17));
#185375=CARTESIAN_POINT('',(29.8368674217662,52.0599703131943,39.116));
#185376=CARTESIAN_POINT('',(29.6214601680818,51.6868740054939,39.3548010137695));
#185377=CARTESIAN_POINT('Origin',(29.817751910705,52.0268612768237,39.5550297832864));
#185378=CARTESIAN_POINT('',(29.4433108120868,51.3783102685125,39.92499));
#185379=CARTESIAN_POINT('',(29.6214601680818,51.6868740054939,39.3548010137695));
#185380=CARTESIAN_POINT('',(31.1634057161447,54.3576020372435,39.92499));
#185381=CARTESIAN_POINT('',(31.2932988600179,54.5825835619867,39.92499));
#185382=CARTESIAN_POINT('',(30.9852566042334,54.0490387253001,39.3548010137695));
#185383=CARTESIAN_POINT('',(31.1634057161447,54.3576020372435,39.92499));
#185384=CARTESIAN_POINT('',(30.7698495716387,53.6759427993283,39.116));
#185385=CARTESIAN_POINT('Origin',(30.788965144268,53.709051942338,39.555029390719));
#185386=CARTESIAN_POINT('',(30.5691597998772,53.3283379195021,39.116));
#185387=CARTESIAN_POINT('',(-0.164977839420929,0.0952500000000019,39.116));
#185388=CARTESIAN_POINT('',(30.506140683165,53.2191856060842,39.3343017080178));
#185389=CARTESIAN_POINT('',(30.5691598004939,53.3283379191461,39.116));
#185390=CARTESIAN_POINT('',(30.3411606219525,52.9334317578284,39.5248017080178));
#185391=CARTESIAN_POINT('Origin',(30.3558747754311,52.9589163924886,39.1947747614277));
#185392=CARTESIAN_POINT('',(30.265556564115,52.8024816883956,39.5248017080178));
#185393=CARTESIAN_POINT('',(-0.164977839420929,0.0952500000000019,39.5248017080178));
#185394=CARTESIAN_POINT('',(30.1005764675364,52.5167277788838,39.3343017080178));
#185395=CARTESIAN_POINT('Origin',(30.2508418455894,52.776994021437,39.1947728911944));
#185396=CARTESIAN_POINT('',(30.0375573238938,52.4075754202453,39.116));
#185397=CARTESIAN_POINT('',(30.1005764675364,52.5167277788838,39.3343017080178));
#185398=CARTESIAN_POINT('',(-0.164977839420929,0.0952500000000019,39.116));
#185399=CARTESIAN_POINT('Origin',(0.164977839420934,-0.0952500000000019,
-2.32316690526363E-17));
#185400=CARTESIAN_POINT('',(31.0998052504806,53.4854427993283,39.116));
#185401=CARTESIAN_POINT('',(31.3152122835993,53.8585387249975,39.3548010137695));
#185402=CARTESIAN_POINT('Origin',(31.1189208229657,53.5185519420882,39.5550293912452));
#185403=CARTESIAN_POINT('',(31.4933613953778,54.1671020370175,39.92499));
#185404=CARTESIAN_POINT('',(31.3152122835993,53.8585387249975,39.3548010137695));
#185405=CARTESIAN_POINT('',(29.7732664904686,51.1878102687781,39.92499));
#185406=CARTESIAN_POINT('',(0.164977839420937,-0.0952500000000068,39.92499));
#185407=CARTESIAN_POINT('',(29.9514158463121,51.496374005847,39.3548010137695));
#185408=CARTESIAN_POINT('',(29.7732664904686,51.1878102687781,39.92499));
#185409=CARTESIAN_POINT('',(30.1668231006081,51.8694703131943,39.116));
#185410=CARTESIAN_POINT('Origin',(30.1477075893947,51.83636127656,39.5550297827307));
#185411=CARTESIAN_POINT('',(30.3675130020937,52.2170754206159,39.116));
#185412=CARTESIAN_POINT('',(30.40444193975,52.2810382154236,39.116));
#185413=CARTESIAN_POINT('',(30.4305321463783,52.3262277788838,39.3343017080178));
#185414=CARTESIAN_POINT('',(30.3675130027357,52.2170754202453,39.116));
#185415=CARTESIAN_POINT('',(30.5955122429569,52.6119816883956,39.5248017080178));
#185416=CARTESIAN_POINT('Origin',(30.5807981195143,52.5864971059991,39.1947745585629));
#185417=CARTESIAN_POINT('',(30.6711163007943,52.7429317578284,39.5248017080178));
#185418=CARTESIAN_POINT('',(30.6713806562803,52.7433896349613,39.5248017080178));
#185419=CARTESIAN_POINT('',(30.8360963620068,53.0286856060842,39.3343017080178));
#185420=CARTESIAN_POINT('Origin',(30.6858309820708,52.7684193600401,39.1947728594248));
#185421=CARTESIAN_POINT('',(30.8991154793358,53.1378379191461,39.116));
#185422=CARTESIAN_POINT('',(30.8360963620068,53.0286856060842,39.3343017080178));
#185423=CARTESIAN_POINT('',(31.1000659426097,53.4858943313409,39.116));
#185424=CARTESIAN_POINT('Origin',(34.09246826623,47.2483549038572,40.10025));
#185425=CARTESIAN_POINT('',(34.7084426211237,47.7461450747861,40.10025));
#185426=CARTESIAN_POINT('',(36.9525415975218,50.8348823336482,40.10025));
#185427=CARTESIAN_POINT('',(34.2589154226527,47.1274239660506,40.10025));
#185428=CARTESIAN_POINT('',(36.9278827595333,50.8527980281381,40.10025));
#185429=CARTESIAN_POINT('Origin',(5.5603853024461E-15,5.57595435693894E-15,
40.10025));
#185430=CARTESIAN_POINT('',(34.6837837831351,47.7640607692759,40.10025));
#185431=CARTESIAN_POINT('',(34.6422255755471,47.7068608037046,40.10025));
#185432=CARTESIAN_POINT('Origin',(5.69178283801114E-15,5.31463085937477E-15,
40.10025));
#185433=CARTESIAN_POINT('Origin',(-0.154117737428426,0.111973090561718,
2.17023830815424E-17));
#185434=CARTESIAN_POINT('',(35.1151666347447,48.6559784483761,39.116));
#185435=CARTESIAN_POINT('',(34.8619402208396,48.3074421904914,39.3548010137695));
#185436=CARTESIAN_POINT('Origin',(35.0926950037606,48.6250489017661,39.5550297832849));
#185437=CARTESIAN_POINT('',(34.65251309241,48.019190476361,39.92499));
#185438=CARTESIAN_POINT('',(34.8619402208396,48.3074421904914,39.3548010137695));
#185439=CARTESIAN_POINT('',(36.6746059268184,50.8023624960587,39.92499));
#185440=CARTESIAN_POINT('',(36.8273044755035,51.0125340177511,39.92499));
#185441=CARTESIAN_POINT('',(36.4651790855635,50.5141111791246,39.3548010137695));
#185442=CARTESIAN_POINT('',(36.6746059268184,50.8023624960587,39.92499));
#185443=CARTESIAN_POINT('',(36.2119529314391,50.1655752777668,39.116));
#185444=CARTESIAN_POINT('Origin',(36.2344246347994,50.1965049239941,39.555029390722));
#185445=CARTESIAN_POINT('',(35.9760279553336,49.8408524072782,39.116));
#185446=CARTESIAN_POINT('',(-0.154117737428421,0.111973090561718,39.116));
#185447=CARTESIAN_POINT('',(35.9019445403524,49.7388853330807,39.3343017080178));
#185448=CARTESIAN_POINT('',(35.9760279559093,49.84085240686,39.116));
#185449=CARTESIAN_POINT('',(35.7079988465464,49.4719419865729,39.5248017080178));
#185450=CARTESIAN_POINT('Origin',(35.7252962640545,49.4957489658917,39.194774761439));
#185451=CARTESIAN_POINT('',(35.6191209461258,49.3496120513045,39.5248017080178));
#185452=CARTESIAN_POINT('',(-0.154117737428421,0.111973090561718,39.5248017080178));
#185453=CARTESIAN_POINT('',(35.4251752107443,49.0826686475731,39.3343017080178));
#185454=CARTESIAN_POINT('Origin',(35.6018226497084,49.3258021153674,39.1947728911938));
#185455=CARTESIAN_POINT('',(35.3510917642539,48.9807015312174,39.116));
#185456=CARTESIAN_POINT('',(35.4251752107443,49.0826686475731,39.3343017080178));
#185457=CARTESIAN_POINT('',(-0.154117737428421,0.111973090561718,39.116));
#185458=CARTESIAN_POINT('Origin',(0.154117737428426,-0.111973090561718,
-2.17023830815424E-17));
#185459=CARTESIAN_POINT('',(36.5201884062959,49.9416290966433,39.116));
#185460=CARTESIAN_POINT('',(36.7734145609104,50.2901649976451,39.3548010137695));
#185461=CARTESIAN_POINT('Origin',(36.5426601094884,49.9725587426398,39.5550293912424));
#185462=CARTESIAN_POINT('',(36.9828414020408,50.5784163146696,39.92499));
#185463=CARTESIAN_POINT('',(36.7734145609104,50.2901649976451,39.3548010137695));
#185464=CARTESIAN_POINT('',(34.9607485668371,47.7952442955498,39.92499));
#185465=CARTESIAN_POINT('',(0.154117737428429,-0.111973090561722,39.92499));
#185466=CARTESIAN_POINT('',(35.1701756951245,48.0834960097835,39.3548010137695));
#185467=CARTESIAN_POINT('',(34.9607485668371,47.7952442955498,39.92499));
#185468=CARTESIAN_POINT('',(35.4234021096015,48.4320322672527,39.116));
#185469=CARTESIAN_POINT('Origin',(35.4009304784386,48.4011027203966,39.5550297827295));
#185470=CARTESIAN_POINT('',(35.6593272385114,48.7567553505295,39.116));
#185471=CARTESIAN_POINT('',(35.7027398082304,48.8165076253515,39.116));
#185472=CARTESIAN_POINT('',(35.7334106856012,48.8587224664496,39.3343017080178));
#185473=CARTESIAN_POINT('',(35.6593272391108,48.756755350094,39.116));
#185474=CARTESIAN_POINT('',(35.9273564209826,49.1256658701811,39.5248017080178));
#185475=CARTESIAN_POINT('Origin',(35.9100590388139,49.1018589397066,39.1947745585602));
#185476=CARTESIAN_POINT('',(36.0162343214032,49.2479958054495,39.5248017080178));
#185477=CARTESIAN_POINT('',(36.0165450899153,49.2484235416109,39.5248017080178));
#185478=CARTESIAN_POINT('',(36.2101800152092,49.5149391519573,39.3343017080178));
#185479=CARTESIAN_POINT('Origin',(36.0335325740085,49.2718056808895,39.194772859428));
#185480=CARTESIAN_POINT('',(36.2842634307661,49.6169062257365,39.116));
#185481=CARTESIAN_POINT('',(36.2101800152092,49.5149391519573,39.3343017080178));
#185482=CARTESIAN_POINT('',(36.5204948682736,49.9420509053687,39.116));
#185483=CARTESIAN_POINT('Origin',(38.8445040879387,43.4258901551466,40.10025));
#185484=CARTESIAN_POINT('',(39.5091373124628,43.8565665267052,40.10025));
#185485=CARTESIAN_POINT('',(42.0638038389706,46.6938111422599,40.10025));
#185486=CARTESIAN_POINT('',(38.9973987043324,43.2882232241943,40.10025));
#185487=CARTESIAN_POINT('',(42.04115278469,46.7142062431418,40.10025));
#185488=CARTESIAN_POINT('Origin',(5.54842705988295E-15,5.58563795083165E-15,
40.10025));
#185489=CARTESIAN_POINT('',(39.4864862581822,43.876961627587,40.10025));
#185490=CARTESIAN_POINT('',(39.4391766863035,43.8244190249873,40.10025));
#185491=CARTESIAN_POINT('Origin',(5.69800909227282E-15,5.30958893808705E-15,
40.10025));
#185492=CARTESIAN_POINT('Origin',(-0.141569089253442,0.127469380511364,
1.99353212598914E-17));
#185493=CARTESIAN_POINT('',(40.0087367337519,44.7189015017594,39.116));
#185494=CARTESIAN_POINT('',(39.7204655612079,44.3987439298676,39.3548010137695));
#185495=CARTESIAN_POINT('Origin',(39.9831551867375,44.6904903154966,39.5550297832865));
#185496=CARTESIAN_POINT('',(39.4820551877886,44.1339623846886,39.92499));
#185497=CARTESIAN_POINT('',(39.7204655612079,44.3987439298676,39.3548010137695));
#185498=CARTESIAN_POINT('',(41.7839914803032,46.6905216402892,39.92499));
#185499=CARTESIAN_POINT('',(41.9578224365467,46.883580475758,39.92499));
#185500=CARTESIAN_POINT('',(41.5455814340041,46.4257404601123,39.3548010137695));
#185501=CARTESIAN_POINT('',(41.7839914803032,46.6905216402892,39.92499));
#185502=CARTESIAN_POINT('',(41.2573105570842,46.1055832156404,39.116));
#185503=CARTESIAN_POINT('Origin',(41.2828921864919,46.1339944934103,39.5550293907218));
#185504=CARTESIAN_POINT('',(40.988735220043,45.8073000862116,39.116));
#185505=CARTESIAN_POINT('',(-0.141569089253437,0.127469380511364,39.116));
#185506=CARTESIAN_POINT('',(40.9043991801909,45.7136354238371,39.3343017080178));
#185507=CARTESIAN_POINT('',(40.9887352205719,45.8073000857354,39.116));
#185508=CARTESIAN_POINT('',(40.6836127633984,45.4684272662431,39.5248017080178));
#185509=CARTESIAN_POINT('Origin',(40.7033039308025,45.4902957559628,39.194774761428));
#185510=CARTESIAN_POINT('',(40.5824347852705,45.3560577375091,39.5248017080178));
#185511=CARTESIAN_POINT('',(-0.141569089253437,0.127469380511364,39.5248017080178));
#185512=CARTESIAN_POINT('',(40.3616483211489,45.1108495273508,39.3343017080178));
#185513=CARTESIAN_POINT('Origin',(40.5627424347173,45.3341863992345,39.1947728911927));
#185514=CARTESIAN_POINT('',(40.2773122455534,45.0171848263428,39.116));
#185515=CARTESIAN_POINT('',(40.3616483211489,45.1108495273508,39.3343017080178));
#185516=CARTESIAN_POINT('',(-0.141569089253437,0.127469380511364,39.116));
#185517=CARTESIAN_POINT('Origin',(0.141569089253442,-0.127469380511364,
-1.99353212598914E-17));
#185518=CARTESIAN_POINT('',(41.5404487355911,45.8506444546177,39.116));
#185519=CARTESIAN_POINT('',(41.8287196129605,46.1708016986849,39.3548010137695));
#185520=CARTESIAN_POINT('Origin',(41.566030364806,45.8790557321734,39.5550293912477));
#185521=CARTESIAN_POINT('',(42.0671296591463,46.4355828789639,39.92499));
#185522=CARTESIAN_POINT('',(41.8287196129605,46.1708016986849,39.3548010137695));
#185523=CARTESIAN_POINT('',(39.7651933659004,43.8790236240215,39.92499));
#185524=CARTESIAN_POINT('',(0.141569089253444,-0.127469380511368,39.92499));
#185525=CARTESIAN_POINT('',(40.0036037391898,44.1438051693176,39.3548010137695));
#185526=CARTESIAN_POINT('',(39.7651933659004,43.8790236240215,39.92499));
#185527=CARTESIAN_POINT('',(40.2918749122587,44.4639627407367,39.116));
#185528=CARTESIAN_POINT('Origin',(40.2662933650396,44.4355515542463,39.5550297827278));
#185529=CARTESIAN_POINT('',(40.5604504235094,44.762246065816,39.116));
#185530=CARTESIAN_POINT('',(40.6098709880934,44.8171331622252,39.116));
#185531=CARTESIAN_POINT('',(40.6447864996558,44.8559107663281,39.3343017080178));
#185532=CARTESIAN_POINT('',(40.5604504240602,44.76224606532,39.116));
#185533=CARTESIAN_POINT('',(40.8655729637774,45.1011189764864,39.5248017080178));
#185534=CARTESIAN_POINT('Origin',(40.8458818366199,45.079250531644,39.1947745585614));
#185535=CARTESIAN_POINT('',(40.9667509419053,45.2134885052204,39.5248017080178));
#185536=CARTESIAN_POINT('',(40.9671047185986,45.2138814140433,39.5248017080178));
#185537=CARTESIAN_POINT('',(41.1875373586978,45.4586966628144,39.3343017080178));
#185538=CARTESIAN_POINT('Origin',(40.9864432425615,45.2353597879075,39.194772859423));
#185539=CARTESIAN_POINT('',(41.2718733990788,45.5523613247127,39.116));
#185540=CARTESIAN_POINT('',(41.1875373586978,45.4586966628144,39.3343017080178));
#185541=CARTESIAN_POINT('',(41.5407976097559,45.8510319186312,39.116));
#185542=CARTESIAN_POINT('Origin',(43.1709513941248,39.1276422664446,40.10025));
#185543=CARTESIAN_POINT('',(43.8769616275879,39.4864862581812,40.10025));
#185544=CARTESIAN_POINT('',(46.7142062431428,42.041152784689,40.10025));
#185545=CARTESIAN_POINT('',(43.3086183250771,38.9747476500508,40.10025));
#185546=CARTESIAN_POINT('',(46.6938111422609,42.0638038389695,40.10025));
#185547=CARTESIAN_POINT('Origin',(5.5375465370123E-15,5.59651847370231E-15,
40.10025));
#185548=CARTESIAN_POINT('',(43.8565665267061,39.5091373124617,40.10025));
#185549=CARTESIAN_POINT('',(43.8040239241064,39.461827740583,40.10025));
#185550=CARTESIAN_POINT('Origin',(5.70367421417806E-15,5.3039238161818E-15,
40.10025));
#185551=CARTESIAN_POINT('Origin',(-0.127469380511361,0.141569089253445,
1.79498438867829E-17));
#185552=CARTESIAN_POINT('',(44.4639627407376,40.2918749122577,39.116));
#185553=CARTESIAN_POINT('',(44.1438051688458,40.0036037397138,39.3548010137695));
#185554=CARTESIAN_POINT('Origin',(44.4355515544746,40.2662933652431,39.5550297832857));
#185555=CARTESIAN_POINT('',(43.8790236243778,39.7651933655047,39.92499));
#185556=CARTESIAN_POINT('',(44.1438051688458,40.0036037397138,39.3548010137695));
#185557=CARTESIAN_POINT('',(46.4355828792675,42.067129658809,39.92499));
#185558=CARTESIAN_POINT('',(46.6286417147362,42.2409606150525,39.92499));
#185559=CARTESIAN_POINT('',(46.1708016982805,41.8287196134095,39.3548010137695));
#185560=CARTESIAN_POINT('',(46.4355828792675,42.067129658809,39.92499));
#185561=CARTESIAN_POINT('',(45.8506444546187,41.54044873559,39.116));
#185562=CARTESIAN_POINT('Origin',(45.8790557323893,41.5660303649984,39.5550293907199));
#185563=CARTESIAN_POINT('',(45.5523613242375,41.2718733996065,39.116));
#185564=CARTESIAN_POINT('',(-0.127469380511355,0.141569089253445,39.116));
#185565=CARTESIAN_POINT('',(45.4586966628153,41.1875373586967,39.3343017080178));
#185566=CARTESIAN_POINT('',(45.5523613247136,41.2718733990777,39.116));
#185567=CARTESIAN_POINT('',(45.2134885052213,40.9667509419042,39.5248017080178));
#185568=CARTESIAN_POINT('Origin',(45.2353576819756,40.9864413462816,39.1947747614304));
#185569=CARTESIAN_POINT('',(45.1011189764874,40.8655729637763,39.5248017080178));
#185570=CARTESIAN_POINT('',(-0.127469380511355,0.141569089253445,39.5248017080178));
#185571=CARTESIAN_POINT('',(44.855910766329,40.6447864996547,39.3343017080178));
#185572=CARTESIAN_POINT('Origin',(45.0792483253111,40.8458798501223,39.1947728911937));
#185573=CARTESIAN_POINT('',(44.762246065321,40.5604504240592,39.116));
#185574=CARTESIAN_POINT('',(44.855910766329,40.6447864996547,39.3343017080178));
#185575=CARTESIAN_POINT('',(-0.127469380511355,0.141569089253445,39.116));
#185576=CARTESIAN_POINT('Origin',(0.127469380511361,-0.141569089253445,
-1.79498438867829E-17));
#185577=CARTESIAN_POINT('',(46.1055832156414,41.2573105570831,39.116));
#185578=CARTESIAN_POINT('',(46.4257404597086,41.5455814344525,39.3548010137695));
#185579=CARTESIAN_POINT('Origin',(46.1339944931977,41.2828921862985,39.5550293912464));
#185580=CARTESIAN_POINT('',(46.690521640593,41.7839914799658,39.92499));
#185581=CARTESIAN_POINT('',(46.4257404597086,41.5455814344525,39.3548010137695));
#185582=CARTESIAN_POINT('',(44.1339623850452,39.4820551873925,39.92499));
#185583=CARTESIAN_POINT('',(0.127469380511362,-0.141569089253449,39.92499));
#185584=CARTESIAN_POINT('',(44.3987439293955,39.7204655617323,39.3548010137695));
#185585=CARTESIAN_POINT('',(44.1339623850452,39.4820551873925,39.92499));
#185586=CARTESIAN_POINT('',(44.7189015017603,40.0087367337508,39.116));
#185587=CARTESIAN_POINT('Origin',(44.6904903152708,39.9831551865323,39.5550297827294));
#185588=CARTESIAN_POINT('',(45.0171848258473,40.2773122461036,39.116));
#185589=CARTESIAN_POINT('',(45.0720719232488,40.3267328095854,39.116));
#185590=CARTESIAN_POINT('',(45.1108495273517,40.3616483211478,39.3343017080178));
#185591=CARTESIAN_POINT('',(45.0171848263437,40.2773122455523,39.116));
#185592=CARTESIAN_POINT('',(45.3560577375101,40.5824347852694,39.5248017080178));
#185593=CARTESIAN_POINT('Origin',(45.3341886054765,40.5627444213201,39.1947745585557));
#185594=CARTESIAN_POINT('',(45.4684272662441,40.6836127633974,39.5248017080178));
#185595=CARTESIAN_POINT('',(45.468820175067,40.6839665400906,39.5248017080178));
#185596=CARTESIAN_POINT('',(45.7136354238381,40.9043991801898,39.3343017080178));
#185597=CARTESIAN_POINT('Origin',(45.4902978619848,40.7033058269827,39.1947728594193));
#185598=CARTESIAN_POINT('',(45.8073000857364,40.9887352205708,39.116));
#185599=CARTESIAN_POINT('',(45.7136354238381,40.9043991801898,39.3343017080178));
#185600=CARTESIAN_POINT('',(46.1059706796549,41.2576594312479,39.116));
#185601=CARTESIAN_POINT('Origin',(47.0244087227346,34.4007037410858,40.10025));
#185602=CARTESIAN_POINT('',(47.7640607692767,34.683783783134,40.10025));
#185603=CARTESIAN_POINT('',(50.8527980281389,36.9278827595321,40.10025));
#185604=CARTESIAN_POINT('',(47.1453396605412,34.2342565846631,40.10025));
#185605=CARTESIAN_POINT('',(50.8348823336491,36.9525415975206,40.10025));
#185606=CARTESIAN_POINT('Origin',(5.52786294311959E-15,5.60847671626546E-15,
40.10025));
#185607=CARTESIAN_POINT('',(47.7461450747869,34.7084426211226,40.10025));
#185608=CARTESIAN_POINT('',(47.6889451092156,34.6668844135346,40.10025));
#185609=CARTESIAN_POINT('Origin',(5.70871613546578E-15,5.29769756192013E-15,
40.10025));
#185610=CARTESIAN_POINT('Origin',(-0.111973090561714,0.154117737428429,
1.57677042678044E-17));
#185611=CARTESIAN_POINT('',(48.4320322672535,35.4234021096004,39.116));
#185612=CARTESIAN_POINT('',(48.0834960093688,35.1701756956953,39.3548010137695));
#185613=CARTESIAN_POINT('Origin',(48.4011027206445,35.400930478617,39.555029783287));
#185614=CARTESIAN_POINT('',(47.795244295863,34.960748566406,39.92499));
#185615=CARTESIAN_POINT('',(48.0834960093688,35.1701756956953,39.3548010137695));
#185616=CARTESIAN_POINT('',(50.5784163149361,36.982841401674,39.92499));
#185617=CARTESIAN_POINT('',(50.7885878366285,37.1355399503592,39.92499));
#185618=CARTESIAN_POINT('',(50.2901649972898,36.7734145613995,39.3548010137695));
#185619=CARTESIAN_POINT('',(50.5784163149361,36.982841401674,39.92499));
#185620=CARTESIAN_POINT('',(49.9416290966442,36.5201884062947,39.116));
#185621=CARTESIAN_POINT('Origin',(49.9725587428723,36.5426601096556,39.5550293907206));
#185622=CARTESIAN_POINT('',(49.6169062253194,36.2842634313403,39.116));
#185623=CARTESIAN_POINT('',(-0.111973090561709,0.154117737428429,39.116));
#185624=CARTESIAN_POINT('',(49.5149391519582,36.2101800152081,39.3343017080178));
#185625=CARTESIAN_POINT('',(49.6169062257374,36.284263430765,39.116));
#185626=CARTESIAN_POINT('',(49.2479958054503,36.0162343214021,39.5248017080178));
#185627=CARTESIAN_POINT('Origin',(49.271803388278,36.0335309082458,39.1947747614336));
#185628=CARTESIAN_POINT('',(49.1256658701819,35.9273564209815,39.5248017080178));
#185629=CARTESIAN_POINT('',(-0.111973090561709,0.154117737428429,39.5248017080178));
#185630=CARTESIAN_POINT('',(48.8587224664505,35.7334106856,39.3343017080178));
#185631=CARTESIAN_POINT('Origin',(49.1018565378157,35.9100572938239,39.1947728911905));
#185632=CARTESIAN_POINT('',(48.7567553500948,35.6593272391096,39.116));
#185633=CARTESIAN_POINT('',(48.8587224664505,35.7334106856,39.3343017080178));
#185634=CARTESIAN_POINT('',(-0.111973090561709,0.154117737428429,39.116));
#185635=CARTESIAN_POINT('Origin',(0.111973090561714,-0.154117737428429,
-1.57677042678044E-17));
#185636=CARTESIAN_POINT('',(50.1655752777676,36.2119529314379,39.116));
#185637=CARTESIAN_POINT('',(50.5141111787694,36.4651790860523,39.3548010137695));
#185638=CARTESIAN_POINT('Origin',(50.1965049237639,36.2344246346304,39.5550293912429));
#185639=CARTESIAN_POINT('',(50.8023624963257,36.6746059264508,39.92499));
#185640=CARTESIAN_POINT('',(50.5141111787694,36.4651790860523,39.3548010137695));
#185641=CARTESIAN_POINT('',(48.0191904766741,34.6525130919791,39.92499));
#185642=CARTESIAN_POINT('',(0.111973090561715,-0.154117737428432,39.92499));
#185643=CARTESIAN_POINT('',(48.3074421900769,34.8619402214101,39.3548010137695));
#185644=CARTESIAN_POINT('',(48.0191904766741,34.6525130919791,39.92499));
#185645=CARTESIAN_POINT('',(48.6559784483769,35.1151666347435,39.116));
#185646=CARTESIAN_POINT('Origin',(48.6250489015221,35.0926950035815,39.5550297827322));
#185647=CARTESIAN_POINT('',(48.9807015307826,35.3510917648525,39.116));
#185648=CARTESIAN_POINT('',(49.0404538064758,35.3945043333724,39.116));
#185649=CARTESIAN_POINT('',(49.0826686475739,35.4251752107432,39.3343017080178));
#185650=CARTESIAN_POINT('',(48.9807015312183,35.3510917642528,39.116));
#185651=CARTESIAN_POINT('',(49.3496120513054,35.6191209461246,39.5248017080178));
#185652=CARTESIAN_POINT('Origin',(49.3258045171785,35.6018243948122,39.1947745585601));
#185653=CARTESIAN_POINT('',(49.4719419865737,35.7079988465452,39.5248017080178));
#185654=CARTESIAN_POINT('',(49.4723697227352,35.7083096150572,39.5248017080178));
#185655=CARTESIAN_POINT('',(49.7388853330816,35.9019445403512,39.3343017080178));
#185656=CARTESIAN_POINT('Origin',(49.4957512585809,35.7252979297077,39.194772859431));
#185657=CARTESIAN_POINT('',(49.8408524068608,35.9760279559081,39.116));
#185658=CARTESIAN_POINT('',(49.7388853330816,35.9019445403512,39.3343017080178));
#185659=CARTESIAN_POINT('',(50.165997086493,36.2122593934156,39.116));
#185660=CARTESIAN_POINT('Origin',(50.3626567888879,29.2968639067295,40.10025));
#185661=CARTESIAN_POINT('',(51.1278468659051,29.5010785149105,40.10025));
#185662=CARTESIAN_POINT('',(54.4342359163067,31.4100231232054,40.10025));
#185663=CARTESIAN_POINT('',(50.4655267888879,29.1186878401549,40.10025));
#185664=CARTESIAN_POINT('',(54.4189959163067,31.4364195775128,40.10025));
#185665=CARTESIAN_POINT('Origin',(5.51948237368594E-15,5.62138166151314E-15,
40.10025));
#185666=CARTESIAN_POINT('',(51.1126068659051,29.5274749692178,40.10025));
#185667=CARTESIAN_POINT('',(51.0513762321548,29.4921234463394,40.10025));
#185668=CARTESIAN_POINT('Origin',(5.71307961579125E-15,5.29097839144664E-15,
40.10025));
#185669=CARTESIAN_POINT('Origin',(-0.0952499999999979,0.164977839420937,
1.34128103812637E-17));
#185670=CARTESIAN_POINT('',(51.869470313195,30.1668231006068,39.116));
#185671=CARTESIAN_POINT('',(51.4963740054947,29.9514158469224,39.3548010137695));
#185672=CARTESIAN_POINT('Origin',(51.836361276822,30.1477075895442,39.5550297832805));
#185673=CARTESIAN_POINT('',(51.1878102690448,29.7732664900068,39.92499));
#185674=CARTESIAN_POINT('',(51.4963740054947,29.9514158469224,39.3548010137695));
#185675=CARTESIAN_POINT('',(54.1671020372442,31.4933613949852,39.92499));
#185676=CARTESIAN_POINT('',(54.3920835619875,31.6232545388584,39.92499));
#185677=CARTESIAN_POINT('',(53.8585387246958,31.315212284122,39.3548010137695));
#185678=CARTESIAN_POINT('',(54.1671020372442,31.4933613949852,39.92499));
#185679=CARTESIAN_POINT('',(53.4854427993291,31.0998052504793,39.116));
#185680=CARTESIAN_POINT('Origin',(53.5185519423382,31.1189208231082,39.5550293907202));
#185681=CARTESIAN_POINT('',(53.137837918791,30.8991154799507,39.116));
#185682=CARTESIAN_POINT('',(-0.0952499999999924,0.164977839420937,39.116));
#185683=CARTESIAN_POINT('',(53.028685606085,30.8360963620055,39.3343017080178));
#185684=CARTESIAN_POINT('',(53.1378379191468,30.8991154793345,39.116));
#185685=CARTESIAN_POINT('',(52.7429317578291,30.671116300793,39.5248017080178));
#185686=CARTESIAN_POINT('Origin',(52.7684169058672,30.6858295650758,39.1947747614281));
#185687=CARTESIAN_POINT('',(52.6119816883963,30.5955122429556,39.5248017080178));
#185688=CARTESIAN_POINT('',(-0.0952499999999923,0.164977839420937,39.5248017080178));
#185689=CARTESIAN_POINT('',(52.3262277788845,30.430532146377,39.3343017080178));
#185690=CARTESIAN_POINT('Origin',(52.5864945348652,30.5807966351497,39.1947728911925));
#185691=CARTESIAN_POINT('',(52.217075420246,30.3675130027344,39.116));
#185692=CARTESIAN_POINT('',(52.3262277788845,30.430532146377,39.3343017080178));
#185693=CARTESIAN_POINT('',(-0.0952499999999924,0.164977839420937,39.116));
#185694=CARTESIAN_POINT('Origin',(0.0952499999999979,-0.164977839420937,
-1.34128103812637E-17));
#185695=CARTESIAN_POINT('',(53.675942799329,30.7698495716374,39.116));
#185696=CARTESIAN_POINT('',(54.0490387249983,30.9852566047561,39.3548010137695));
#185697=CARTESIAN_POINT('Origin',(53.7090519420883,30.7889651441222,39.5550293912471));
#185698=CARTESIAN_POINT('',(54.3576020374704,31.1634057157515,39.92499));
#185699=CARTESIAN_POINT('',(54.0490387249983,30.9852566047561,39.3548010137695));
#185700=CARTESIAN_POINT('',(51.3783102687789,29.4433108116255,39.92499));
#185701=CARTESIAN_POINT('',(0.0952499999999987,-0.16497783942094,39.92499));
#185702=CARTESIAN_POINT('',(51.6868740051415,29.6214601686922,39.3548010137695));
#185703=CARTESIAN_POINT('',(51.3783102687789,29.4433108116255,39.92499));
#185704=CARTESIAN_POINT('',(52.059970313195,29.8368674217649,39.116));
#185705=CARTESIAN_POINT('Origin',(52.0268612765588,29.8177519105504,39.5550297827267));
#185706=CARTESIAN_POINT('',(52.4075754198752,30.0375573245348,39.116));
#185707=CARTESIAN_POINT('',(52.4715382154243,30.0744862609068,39.116));
#185708=CARTESIAN_POINT('',(52.5167277788845,30.1005764675351,39.3343017080178));
#185709=CARTESIAN_POINT('',(52.407575420246,30.0375573238925,39.116));
#185710=CARTESIAN_POINT('',(52.8024816883963,30.2655565641137,39.5248017080178));
#185711=CARTESIAN_POINT('Origin',(52.7769965925056,30.2508433300767,39.1947745585566));
#185712=CARTESIAN_POINT('',(52.9334317578291,30.3411606219512,39.5248017080178));
#185713=CARTESIAN_POINT('',(52.9338896349621,30.3414249774371,39.5248017080178));
#185714=CARTESIAN_POINT('',(53.219185606085,30.5061406831637,39.3343017080178));
#185715=CARTESIAN_POINT('Origin',(52.9589188467291,30.3558761923099,39.1947728594246));
#185716=CARTESIAN_POINT('',(53.3283379191468,30.5691598004926,39.116));
#185717=CARTESIAN_POINT('',(53.219185606085,30.5061406831637,39.3343017080178));
#185718=CARTESIAN_POINT('',(53.6763943313417,30.7701102637665,39.116));
#185719=CARTESIAN_POINT('Origin',(53.1491210481986,23.8720415006483,40.10025));
#185720=CARTESIAN_POINT('',(53.9314655730807,23.9951532569801,40.10025));
#185721=CARTESIAN_POINT('',(57.4192809246792,25.5480287005711,40.10025));
#185722=CARTESIAN_POINT('',(53.2328030451451,23.6840886581929,40.10025));
#185723=CARTESIAN_POINT('',(57.4068835917983,25.5758735661201,40.10025));
#185724=CARTESIAN_POINT('Origin',(5.51249664798382E-15,5.6350919201647E-15,
40.10025));
#185725=CARTESIAN_POINT('',(53.9190682401998,24.022998122529,40.10025));
#185726=CARTESIAN_POINT('',(53.8544777939072,23.9942406030427,40.10025));
#185727=CARTESIAN_POINT('Origin',(5.71671684795091E-15,5.28383992139913E-15,
40.10025));
#185728=CARTESIAN_POINT('Origin',(-0.0774833305059378,0.174030409680916,
1.09109629373748E-17));
#185729=CARTESIAN_POINT('',(54.7386155880007,24.5797300649095,39.116));
#185730=CARTESIAN_POINT('',(54.3450469517073,24.4045020183939,39.3548010137695));
#185731=CARTESIAN_POINT('Origin',(54.7036898113993,24.5641801073098,39.5550297832851));
#185732=CARTESIAN_POINT('',(54.0195518811806,24.259582275487,39.92499));
#185733=CARTESIAN_POINT('',(54.3450469517073,24.4045020183939,39.3548010137695));
#185734=CARTESIAN_POINT('',(57.1623216544374,25.6588335304434,39.92499));
#185735=CARTESIAN_POINT('',(57.399648237566,25.7644981330385,39.92499));
#185736=CARTESIAN_POINT('',(56.8368270312096,25.5139139879309,39.3548010137695));
#185737=CARTESIAN_POINT('',(57.1623216544374,25.6588335304434,39.92499));
#185738=CARTESIAN_POINT('',(56.443258798156,25.338686120287,39.116));
#185739=CARTESIAN_POINT('Origin',(56.4781846872468,25.3542361279702,39.5550293907207));
#185740=CARTESIAN_POINT('',(56.0765803402173,25.1754303533066,39.116));
#185741=CARTESIAN_POINT('',(-0.0774833305059323,0.174030409680916,39.116));
#185742=CARTESIAN_POINT('',(55.9614386837456,25.1241659841929,39.3343017080178));
#185743=CARTESIAN_POINT('',(56.0765803405066,25.1754303526568,39.116));
#185744=CARTESIAN_POINT('',(55.6600051127011,24.9899591116489,39.5248017080178));
#185745=CARTESIAN_POINT('Origin',(55.6868886053399,25.0019278517712,39.1947747614349));
#185746=CARTESIAN_POINT('',(55.5218696254676,24.9284572302735,39.5248017080178));
#185747=CARTESIAN_POINT('',(-0.0774833305059322,0.174030409680916,39.5248017080178));
#185748=CARTESIAN_POINT('',(55.2204359898059,24.79425032896,39.3343017080178));
#185749=CARTESIAN_POINT('Origin',(55.4949838933612,24.9164863690989,39.1947728911908));
#185750=CARTESIAN_POINT('',(55.1052942849675,24.7429859390906,39.116));
#185751=CARTESIAN_POINT('',(55.2204359898059,24.79425032896,39.3343017080178));
#185752=CARTESIAN_POINT('',(-0.0774833305059323,0.174030409680916,39.116));
#185753=CARTESIAN_POINT('Origin',(0.0774833305059378,-0.174030409680916,
-1.09109629373748E-17));
#185754=CARTESIAN_POINT('',(56.5982254591679,24.9906253009252,39.116));
#185755=CARTESIAN_POINT('',(56.9917936924676,25.1658531680164,39.3548010137695));
#185756=CARTESIAN_POINT('Origin',(56.633151347996,25.0061753084914,39.5550293912448));
#185757=CARTESIAN_POINT('',(57.317288315633,25.3107727106689,39.92499));
#185758=CARTESIAN_POINT('',(56.9917936924676,25.1658531680164,39.3548010137695));
#185759=CARTESIAN_POINT('',(54.1745185419763,23.9115214566108,39.92499));
#185760=CARTESIAN_POINT('',(0.0774833305059383,-0.174030409680919,39.92499));
#185761=CARTESIAN_POINT('',(54.5000136124317,24.0564411996777,39.3548010137695));
#185762=CARTESIAN_POINT('',(54.1745185419763,23.9115214566108,39.92499));
#185763=CARTESIAN_POINT('',(54.8935822490125,24.2316692455476,39.116));
#185764=CARTESIAN_POINT('Origin',(54.858656472133,24.2161192878242,39.5550297827294));
#185765=CARTESIAN_POINT('',(55.2602609456778,24.3949251204062,39.116));
#185766=CARTESIAN_POINT('',(55.3277334713093,24.4249658234759,39.116));
#185767=CARTESIAN_POINT('',(55.3754026508178,24.4461895095982,39.3343017080178));
#185768=CARTESIAN_POINT('',(55.2602609459794,24.3949251197288,39.116));
#185769=CARTESIAN_POINT('',(55.6768362864795,24.5803964109116,39.5248017080178));
#185770=CARTESIAN_POINT('Origin',(55.6499528488663,24.5684276954194,39.1947745585578));
#185771=CARTESIAN_POINT('',(55.814971773713,24.641898292287,39.5248017080178));
#185772=CARTESIAN_POINT('',(55.8154547752198,24.6421133384129,39.5248017080178));
#185773=CARTESIAN_POINT('',(56.1164053447575,24.776105164831,39.3343017080178));
#185774=CARTESIAN_POINT('Origin',(55.8418574376285,24.6538691229756,39.1947728594241));
#185775=CARTESIAN_POINT('',(56.2315470015185,24.827369533295,39.116));
#185776=CARTESIAN_POINT('',(56.1164053447575,24.776105164831,39.3343017080178));
#185777=CARTESIAN_POINT('',(56.5987017673886,24.9908373670081,39.116));
#185778=CARTESIAN_POINT('Origin',(55.3532724151367,18.1856720123401,40.10025));
#185779=CARTESIAN_POINT('',(56.144199857553,18.2263320786575,40.10025));
#185780=CARTESIAN_POINT('',(59.7752282754839,19.4061247292246,40.10025));
#185781=CARTESIAN_POINT('',(55.4168495715594,17.9900016446776,40.10025));
#185782=CARTESIAN_POINT('',(59.7658094374954,19.4351129318413,40.10025));
#185783=CARTESIAN_POINT('Origin',(5.50698230308587E-15,5.64945727975729E-15,
40.10025));
#185784=CARTESIAN_POINT('',(56.1347810195644,18.2553202812742,40.10025));
#185785=CARTESIAN_POINT('',(56.0675384271755,18.2334718385813,40.10025));
#185786=CARTESIAN_POINT('Origin',(5.71958798166808E-15,5.27636036234925E-15,
40.10025));
#185787=CARTESIAN_POINT('Origin',(-0.0588677374284251,0.181176266354228,
8.28957270027824E-18));
#185788=CARTESIAN_POINT('',(57.0080331356325,18.7233363629817,39.116));
#185789=CARTESIAN_POINT('',(56.5983041910848,18.5902073587815,39.3548010137695));
#185790=CARTESIAN_POINT('Origin',(56.9716732729192,18.7115223274338,39.5550297832882));
#185791=CARTESIAN_POINT('',(56.2594439785883,18.4801050009129,39.92499));
#185792=CARTESIAN_POINT('',(56.5983041910848,18.5902073587815,39.3548010137695));
#185793=CARTESIAN_POINT('',(59.5312589135998,19.5431821162859,39.92499));
#185794=CARTESIAN_POINT('',(59.7783303554051,19.6234604941051,39.92499));
#185795=CARTESIAN_POINT('',(59.1923991668989,19.433079910958,39.3548010137695));
#185796=CARTESIAN_POINT('',(59.5312589135998,19.5431821162859,39.92499));
#185797=CARTESIAN_POINT('',(58.7826706420791,19.2999510424999,39.116));
#185798=CARTESIAN_POINT('Origin',(58.8190306219008,19.3117651160986,39.5550293907231));
#185799=CARTESIAN_POINT('',(58.4009360126571,19.1759179434146,39.116));
#185800=CARTESIAN_POINT('',(-0.0588677374284196,0.181176266354228,39.116));
#185801=CARTESIAN_POINT('',(58.2810665285032,19.1369699862876,39.3343017080178));
#185802=CARTESIAN_POINT('',(58.4009360128769,19.1759179427379,39.116));
#185803=CARTESIAN_POINT('',(57.9672558039534,19.0350067009923,39.5248017080178));
#185804=CARTESIAN_POINT('Origin',(57.9952431000171,19.0440997849305,39.1947747614319));
#185805=CARTESIAN_POINT('',(57.8234483402241,18.9882808235613,39.5248017080178));
#185806=CARTESIAN_POINT('',(-0.0588677374284196,0.181176266354228,39.5248017080178));
#185807=CARTESIAN_POINT('',(57.5096375484039,18.8863175164085,39.3343017080178));
#185808=CARTESIAN_POINT('Origin',(57.7954585952484,18.9791858642776,39.1947728911916));
#185809=CARTESIAN_POINT('',(57.3897680139787,18.8473695436955,39.116));
#185810=CARTESIAN_POINT('',(57.5096375484039,18.8863175164085,39.3343017080178));
#185811=CARTESIAN_POINT('',(-0.0588677374284196,0.181176266354228,39.116));
#185812=CARTESIAN_POINT('Origin',(0.0588677374284251,-0.181176266354228,
-8.28957270027824E-18));
#185813=CARTESIAN_POINT('',(58.9004061169359,18.9375985097914,39.116));
#185814=CARTESIAN_POINT('',(59.3101346419426,19.0707273776745,39.3548010137695));
#185815=CARTESIAN_POINT('Origin',(58.9367660964832,18.949412583301,39.5550293912495));
#185816=CARTESIAN_POINT('',(59.6489943885965,19.180829583147,39.92499));
#185817=CARTESIAN_POINT('',(59.3101346419426,19.0707273776745,39.3548010137695));
#185818=CARTESIAN_POINT('',(56.377179453281,18.1177524687099,39.92499));
#185819=CARTESIAN_POINT('',(0.0588677374284254,-0.181176266354229,39.92499));
#185820=CARTESIAN_POINT('',(56.7160396657233,18.2278548267449,39.3548010137695));
#185821=CARTESIAN_POINT('',(56.377179453281,18.1177524687099,39.92499));
#185822=CARTESIAN_POINT('',(57.1257686104893,18.3609838302733,39.116));
#185823=CARTESIAN_POINT('Origin',(57.0894087474837,18.3491697946304,39.5550297827266));
#185824=CARTESIAN_POINT('',(57.5075034886064,18.4850170116922,39.116));
#185825=CARTESIAN_POINT('',(57.5777465012101,18.5078403492302,39.116));
#185826=CARTESIAN_POINT('',(57.6273730232608,18.5239649837,39.3343017080178));
#185827=CARTESIAN_POINT('',(57.5075034888355,18.485017010987,39.116));
#185828=CARTESIAN_POINT('',(57.941183815081,18.6259282908529,39.5248017080178));
#185829=CARTESIAN_POINT('Origin',(57.9131965763113,18.6168352256566,39.194774558563));
#185830=CARTESIAN_POINT('',(58.0849912788103,18.6726541682838,39.5248017080178));
#185831=CARTESIAN_POINT('',(58.0854941128254,18.6728175489593,39.5248017080178));
#185832=CARTESIAN_POINT('',(58.3988020033601,18.7746174535792,39.3343017080178));
#185833=CARTESIAN_POINT('Origin',(58.1129809527781,18.6817491043752,39.1947728594169));
#185834=CARTESIAN_POINT('',(58.5186714877338,18.8135654100295,39.116));
#185835=CARTESIAN_POINT('',(58.3988020033601,18.7746174535792,39.3343017080178));
#185836=CARTESIAN_POINT('',(58.9009019828321,18.9377596263878,39.116));
#185837=CARTESIAN_POINT('Origin',(56.9509617460776,12.3000564958682,40.10025));
#185838=CARTESIAN_POINT('',(57.7418065394567,12.257819391976,40.10025));
#185839=CARTESIAN_POINT('',(61.4762657165317,13.0516031943521,40.10025));
#185840=CARTESIAN_POINT('',(56.9937374973465,12.0988124084933,40.10025));
#185841=CARTESIAN_POINT('',(61.4699285681956,13.0814171332224,40.10025));
#185842=CARTESIAN_POINT('Origin',(5.50299975530876E-15,5.66432035040507E-15,
40.10025));
#185843=CARTESIAN_POINT('',(57.7354693911206,12.2876333308464,40.10025));
#185844=CARTESIAN_POINT('',(57.666311376549,12.2729333410571,40.10025));
#185845=CARTESIAN_POINT('Origin',(5.72166156020094E-15,5.26862166191115E-15,
40.10025));
#185846=CARTESIAN_POINT('Origin',(-0.0396071771007808,0.18633711793979,
5.57736016997284E-18));
#185847=CARTESIAN_POINT('',(58.6528587425324,12.6618058697512,39.116));
#185848=CARTESIAN_POINT('',(58.2314585657882,12.5722344970953,39.3548010137695));
#185849=CARTESIAN_POINT('Origin',(58.6154631599691,12.6538571932999,39.5550297832851));
#185850=CARTESIAN_POINT('',(57.8829458347212,12.4981558287379,39.92499));
#185851=CARTESIAN_POINT('',(58.2314585657882,12.5722344970953,39.3548010137695));
#185852=CARTESIAN_POINT('',(61.2479592423879,13.2134115091886,39.92499));
#185853=CARTESIAN_POINT('',(61.5020685764506,13.2674241155252,39.92499));
#185854=CARTESIAN_POINT('',(60.8994469905094,13.1393329438488,39.3548010137695));
#185855=CARTESIAN_POINT('',(61.2479592423879,13.2134115091886,39.92499));
#185856=CARTESIAN_POINT('',(60.4780472453829,13.0497616623167,39.116));
#185857=CARTESIAN_POINT('Origin',(60.5154429483898,13.0577103643691,39.5550293907213));
#185858=CARTESIAN_POINT('',(60.0854388089607,12.9663101637158,39.116));
#185859=CARTESIAN_POINT('',(-0.0396071771007753,0.18633711793979,39.116));
#185860=CARTESIAN_POINT('',(59.9621548122773,12.9401053405442,39.3343017080178));
#185861=CARTESIAN_POINT('',(60.0854388091086,12.9663101630196,39.116));
#185862=CARTESIAN_POINT('',(59.6394051101895,12.8715027735884,39.5248017080178));
#185863=CARTESIAN_POINT('Origin',(59.6681895750054,12.8776205756125,39.1947747614281));
#185864=CARTESIAN_POINT('',(59.4915012546306,12.8400648385931,39.5248017080178));
#185865=CARTESIAN_POINT('',(-0.0396071771007752,0.18633711793979,39.5248017080178));
#185866=CARTESIAN_POINT('',(59.1687514833562,12.7714622569312,39.3343017080178));
#185867=CARTESIAN_POINT('Origin',(59.4627141582885,12.8339454274774,39.194772891192));
#185868=CARTESIAN_POINT('',(59.0454674350476,12.745257423514,39.116));
#185869=CARTESIAN_POINT('',(59.1687514833562,12.7714622569312,39.3343017080178));
#185870=CARTESIAN_POINT('',(-0.0396071771007753,0.18633711793979,39.116));
#185871=CARTESIAN_POINT('Origin',(0.0396071771007808,-0.18633711793979,
-5.57736016997284E-18));
#185872=CARTESIAN_POINT('',(60.5572615995845,12.6770874264371,39.116));
#185873=CARTESIAN_POINT('',(60.9786613448369,12.7666587073766,39.3548010137695));
#185874=CARTESIAN_POINT('Origin',(60.5946573023102,12.6850361284297,39.5550293912459));
#185875=CARTESIAN_POINT('',(61.3271735966836,12.8407372728665,39.92499));
#185876=CARTESIAN_POINT('',(60.9786613448369,12.7666587073766,39.3548010137695));
#185877=CARTESIAN_POINT('',(57.9621601888122,12.1254815933784,39.92499));
#185878=CARTESIAN_POINT('',(0.0396071771007809,-0.186337117939792,39.92499));
#185879=CARTESIAN_POINT('',(58.3106729198429,12.1995602619065,39.3548010137695));
#185880=CARTESIAN_POINT('',(57.9621601888122,12.1254815933784,39.92499));
#185881=CARTESIAN_POINT('',(58.7320730967339,12.2891316338716,39.116));
#185882=CARTESIAN_POINT('Origin',(58.6946775138724,12.2811829573569,39.5550297827283));
#185883=CARTESIAN_POINT('',(59.124681789095,12.3725831883596,39.116));
#185884=CARTESIAN_POINT('',(59.1969256915255,12.3879391031039,39.116));
#185885=CARTESIAN_POINT('',(59.2479658375578,12.3987880210516,39.3343017080178));
#185886=CARTESIAN_POINT('',(59.1246817892492,12.3725831876344,39.116));
#185887=CARTESIAN_POINT('',(59.5707156088322,12.4673906027135,39.5248017080178));
#185888=CARTESIAN_POINT('Origin',(59.5419312029547,12.4612728133398,39.1947745585609));
#185889=CARTESIAN_POINT('',(59.7186194643911,12.4988285377088,39.5248017080178));
#185890=CARTESIAN_POINT('',(59.7191366217598,12.498938462901,39.5248017080178));
#185891=CARTESIAN_POINT('',(60.0413691664789,12.5674311046646,39.3343017080178));
#185892=CARTESIAN_POINT('Origin',(59.7474064876886,12.5049479331813,39.1947728594153));
#185893=CARTESIAN_POINT('',(60.1646531633102,12.59363592714,39.116));
#185894=CARTESIAN_POINT('',(60.0413691664789,12.5674311046646,39.3343017080178));
#185895=CARTESIAN_POINT('',(60.5577715903456,12.6771958283198,39.116));
#185896=CARTESIAN_POINT('Origin',(57.9246844223736,6.27967898647528,40.10025));
#185897=CARTESIAN_POINT('',(58.7067819056644,6.15500747092236,40.10025));
#185898=CARTESIAN_POINT('',(62.5037563256536,6.55408556365861,40.10025));
#185899=CARTESIAN_POINT('',(57.9461901084063,6.07506605172221,40.10025));
#185900=CARTESIAN_POINT('',(62.5005702980932,6.58439859102944,40.10025));
#185901=CARTESIAN_POINT('Origin',(5.50059263827931E-15,5.67951828919572E-15,
40.10025));
#185902=CARTESIAN_POINT('',(58.703595878104,6.18532049829319,40.10025));
#185903=CARTESIAN_POINT('',(58.6332801510296,6.17793001757189,40.10025));
#185904=CARTESIAN_POINT('Origin',(5.72291486498914E-15,5.26070860690626E-15,
40.10025));
#185905=CARTESIAN_POINT('Origin',(-0.0199126722524855,0.189456421067656,
2.80404091450755E-18));
#185906=CARTESIAN_POINT('',(59.6550713551494,6.46154998175838,39.116));
#185907=CARTESIAN_POINT('',(59.2266168947287,6.4165176033497,39.3548010137695));
#185908=CARTESIAN_POINT('Origin',(59.6170497665651,6.45755375176664,39.5550297832836));
#185909=CARTESIAN_POINT('',(58.8722700235037,6.37927424589616,39.92499));
#185910=CARTESIAN_POINT('',(59.2266168947287,6.4165176033497,39.3548010137695));
#185911=CARTESIAN_POINT('',(62.293614112757,6.73887200051248,39.92499));
#185912=CARTESIAN_POINT('',(62.5519772640373,6.76602706194862,39.92499));
#185913=CARTESIAN_POINT('',(61.9392677288637,6.70162869542306,39.3548010137695));
#185914=CARTESIAN_POINT('',(62.293614112757,6.73887200051248,39.92499));
#185915=CARTESIAN_POINT('',(61.5108137072213,6.656596362523,39.116));
#185916=CARTESIAN_POINT('Origin',(61.5488354182638,6.66059260538561,39.5550293907231));
#185917=CARTESIAN_POINT('',(61.1116329639869,6.61464077648856,39.116));
#185918=CARTESIAN_POINT('',(-0.0199126722524799,0.189456421067656,39.116));
#185919=CARTESIAN_POINT('',(60.9862851800405,6.60146619279864,39.3343017080178));
#185920=CARTESIAN_POINT('',(61.1116329640613,6.6146407757804,39.116));
#185921=CARTESIAN_POINT('',(60.6581326136905,6.56697596826196,39.5248017080178));
#185922=CARTESIAN_POINT('Origin',(60.6873988786453,6.57005146045368,39.1947747614359));
#185923=CARTESIAN_POINT('',(60.5077528318945,6.55117041629687,39.5248017080178));
#185924=CARTESIAN_POINT('',(-0.0199126722524799,0.189456421067656,39.5248017080178));
#185925=CARTESIAN_POINT('',(60.1796001951996,6.51668018436665,39.3343017080178));
#185926=CARTESIAN_POINT('Origin',(60.4784837816392,6.54809359889824,39.1947728911902));
#185927=CARTESIAN_POINT('',(60.0542523588398,6.50350559588384,39.116));
#185928=CARTESIAN_POINT('',(60.1796001951996,6.51668018436665,39.3343017080178));
#185929=CARTESIAN_POINT('',(-0.0199126722524799,0.189456421067656,39.116));
#185930=CARTESIAN_POINT('Origin',(0.0199126722524855,-0.189456421067656,
-2.80404091450755E-18));
#185931=CARTESIAN_POINT('',(61.5506390517263,6.27768352038769,39.116));
#185932=CARTESIAN_POINT('',(61.979093073432,6.32271585268557,39.3548010137695));
#185933=CARTESIAN_POINT('Origin',(61.5886607624852,6.2816797632205,39.5550293912434));
#185934=CARTESIAN_POINT('',(62.3334394573093,6.35995915792716,39.92499));
#185935=CARTESIAN_POINT('',(61.979093073432,6.32271585268557,39.3548010137695));
#185936=CARTESIAN_POINT('',(58.9120953679531,6.00036140428966,39.92499));
#185937=CARTESIAN_POINT('',(0.0199126722524855,-0.189456421067657,39.92499));
#185938=CARTESIAN_POINT('',(59.2664422391598,6.03760476191703,39.3548010137695));
#185939=CARTESIAN_POINT('',(58.9120953679531,6.00036140428966,39.92499));
#185940=CARTESIAN_POINT('',(59.6948966996543,6.08263713962306,39.116));
#185941=CARTESIAN_POINT('Origin',(59.6568751107691,6.0786409095997,39.5550297827316));
#185942=CARTESIAN_POINT('',(60.0940777032672,6.12459275448621,39.116));
#185943=CARTESIAN_POINT('',(60.1675309762116,6.13231300382095,39.116));
#185944=CARTESIAN_POINT('',(60.2194255397046,6.13776734223133,39.3343017080178));
#185945=CARTESIAN_POINT('',(60.0940777033448,6.12459275374853,39.116));
#185946=CARTESIAN_POINT('',(60.5475781763994,6.17225757416155,39.5248017080178));
#185947=CARTESIAN_POINT('Origin',(60.5183119713874,6.16918208839056,39.1947745585607));
#185948=CARTESIAN_POINT('',(60.6979579581955,6.18806312612664,39.5248017080178));
#185949=CARTESIAN_POINT('',(60.6984837728334,6.18811839147206,39.5248017080178));
#185950=CARTESIAN_POINT('',(61.0261105245455,6.22255335066333,39.3343017080178));
#185951=CARTESIAN_POINT('Origin',(60.7272269341789,6.19113993560376,39.194772859427));
#185952=CARTESIAN_POINT('',(61.1514583085663,6.23572793364508,39.116));
#185953=CARTESIAN_POINT('',(61.0261105245455,6.22255335066333,39.3343017080178));
#185954=CARTESIAN_POINT('',(61.5511575797869,6.27773801988296,39.116));
#185955=CARTESIAN_POINT('Origin',(57.9430040808458,-6.10537907909383,39.92499));
#185956=CARTESIAN_POINT('Ctrl Pts',(62.2936141127569,-6.73887200051333,
39.92499));
#185957=CARTESIAN_POINT('Ctrl Pts',(62.3041663177862,-6.7399810819533,39.9348354642028));
#185958=CARTESIAN_POINT('Ctrl Pts',(62.3147747227683,-6.74025426844094,
39.9446440828477));
#185959=CARTESIAN_POINT('Ctrl Pts',(62.3253809467545,-6.73970068257582,
39.9543641760359));
#185960=CARTESIAN_POINT('Ctrl Pts',(62.3356425316169,-6.73916508495494,
39.9637684240747));
#185961=CARTESIAN_POINT('Ctrl Pts',(62.3459033574861,-6.737855436376,39.9730909636437));
#185962=CARTESIAN_POINT('Ctrl Pts',(62.3561113603689,-6.73573381164702,
39.9822808977187));
#185963=CARTESIAN_POINT('Ctrl Pts',(62.3657675025234,-6.73372688529553,
39.99097400947));
#185964=CARTESIAN_POINT('Ctrl Pts',(62.3753772873532,-6.73099321743661,
39.9995492765056));
#185965=CARTESIAN_POINT('Ctrl Pts',(62.3848821415168,-6.72746117704375,
40.0079462328753));
#185966=CARTESIAN_POINT('Ctrl Pts',(62.3936367996101,-6.72420791239824,
40.0156804369753));
#185967=CARTESIAN_POINT('Ctrl Pts',(62.4023029415068,-6.72027708243395,
40.0232638017489));
#185968=CARTESIAN_POINT('Ctrl Pts',(62.4108128192462,-6.71558140885914,
40.0306257270037));
#185969=CARTESIAN_POINT('Ctrl Pts',(62.4132812112908,-6.71421937245263,
40.0327611416698));
#185970=CARTESIAN_POINT('Ctrl Pts',(62.4157362792982,-6.71279278199377,
40.0348777427294));
#185971=CARTESIAN_POINT('Ctrl Pts',(62.4181758915949,-6.71129899689598,
40.0369733168701));
#185972=CARTESIAN_POINT('Ctrl Pts',(62.4208205881801,-6.70967963780669,
40.039245053974));
#185973=CARTESIAN_POINT('Ctrl Pts',(62.4234440047029,-6.70798448411175,
40.041487875195));
#185974=CARTESIAN_POINT('Ctrl Pts',(62.4260429761973,-6.70621108803123,
40.04369857016));
#185975=CARTESIAN_POINT('Ctrl Pts',(62.4331758738576,-6.70134398857268,
40.0497658398386));
#185976=CARTESIAN_POINT('Ctrl Pts',(62.4400912556838,-6.69585818364696,
40.0555581699984));
#185977=CARTESIAN_POINT('Ctrl Pts',(62.4466864116142,-6.6897680133389,40.0609828468886));
#185978=CARTESIAN_POINT('Ctrl Pts',(62.4527206212313,-6.68419583814993,
40.0659461317306));
#185979=CARTESIAN_POINT('Ctrl Pts',(62.4584752900418,-6.67811620689287,
40.0706039980709));
#185980=CARTESIAN_POINT('Ctrl Pts',(62.4638645712592,-6.67150703079124,
40.0748843180607));
#185981=CARTESIAN_POINT('Ctrl Pts',(62.466511768588,-6.66826062508022,40.0769867972572));
#185982=CARTESIAN_POINT('Ctrl Pts',(62.4690703232302,-6.66488629457962,
40.0789976708176));
#185983=CARTESIAN_POINT('Ctrl Pts',(62.4715267736418,-6.66138078591716,
40.08090504915));
#185984=CARTESIAN_POINT('Ctrl Pts',(62.4719928611813,-6.66071564979253,
40.0812669556105));
#185985=CARTESIAN_POINT('Ctrl Pts',(62.472455189938,-6.66004526560994,40.0816253922033));
#185986=CARTESIAN_POINT('Ctrl Pts',(62.4729136358129,-6.65936969820862,
40.081980198914));
#185987=CARTESIAN_POINT('Ctrl Pts',(62.4733577552542,-6.6587152422886,40.082323917915));
#185988=CARTESIAN_POINT('Ctrl Pts',(62.4737982306999,-6.65805592206456,
40.0826642303499));
#185989=CARTESIAN_POINT('Ctrl Pts',(62.4742349489459,-6.65739180030914,
40.08300099161));
#185990=CARTESIAN_POINT('Ctrl Pts',(62.4789942144022,-6.65015433826465,
40.086670946431));
#185991=CARTESIAN_POINT('Ctrl Pts',(62.4833100626573,-6.64234165497574,
40.0899175831873));
#185992=CARTESIAN_POINT('Ctrl Pts',(62.4870273554119,-6.63406423386325,
40.0925642067057));
#185993=CARTESIAN_POINT('Ctrl Pts',(62.4885971912258,-6.63056862752634,
40.0936818922524));
#185994=CARTESIAN_POINT('Ctrl Pts',(62.4900605069388,-6.62699051141436,
40.0946930094789));
#185995=CARTESIAN_POINT('Ctrl Pts',(62.4914070226221,-6.62333954252002,
40.0955863397546));
#185996=CARTESIAN_POINT('Ctrl Pts',(62.4936745213867,-6.61719140213073,
40.0970906856167));
#185997=CARTESIAN_POINT('Ctrl Pts',(62.4956084911391,-6.61083770188526,
40.0982599215483));
#185998=CARTESIAN_POINT('Ctrl Pts',(62.4971561593216,-6.6043306253614,40.0990497370454));
#185999=CARTESIAN_POINT('Ctrl Pts',(62.4975430763672,-6.60270385623043,
40.0992471909196));
#186000=CARTESIAN_POINT('Ctrl Pts',(62.4979056188877,-6.60106746196549,
40.0994209989363));
#186001=CARTESIAN_POINT('Ctrl Pts',(62.4982426563689,-6.59942221845739,
40.0995705982975));
#186002=CARTESIAN_POINT('Ctrl Pts',(62.4987482125908,-6.59695435319524,
40.0997949973393));
#186003=CARTESIAN_POINT('Ctrl Pts',(62.4991963674669,-6.59446659126598,
40.0999649129781));
#186004=CARTESIAN_POINT('Ctrl Pts',(62.4995849724118,-6.59196174500292,
40.1000786629733));
#186005=CARTESIAN_POINT('Ctrl Pts',(62.4999735773567,-6.58945689873986,
40.1001924129685));
#186006=CARTESIAN_POINT('Ctrl Pts',(62.5003026407462,-6.5869349761765,40.10025));
#186007=CARTESIAN_POINT('Ctrl Pts',(62.5005702980931,-6.58439859103029,
40.10025));
#186008=CARTESIAN_POINT('Ctrl Pts',(58.7035958781039,-6.18532049829399,
40.10025));
#186009=CARTESIAN_POINT('Ctrl Pts',(58.7026899760169,-6.19390281910185,
40.10025));
#186010=CARTESIAN_POINT('Ctrl Pts',(58.7025003609928,-6.20248552904425,
40.099578633424));
#186011=CARTESIAN_POINT('Ctrl Pts',(58.7029569544314,-6.21093474935507,
40.0983063763365));
#186012=CARTESIAN_POINT('Ctrl Pts',(58.7032518669435,-6.21639207873545,
40.0974846287991));
#186013=CARTESIAN_POINT('Ctrl Pts',(58.7038154335199,-6.22179377937535,
40.0964130309337));
#186014=CARTESIAN_POINT('Ctrl Pts',(58.7046202140516,-6.22710604846857,
40.0951176960923));
#186015=CARTESIAN_POINT('Ctrl Pts',(58.7056869045458,-6.23414715684634,
40.0934008039614));
#186016=CARTESIAN_POINT('Ctrl Pts',(58.7071827955652,-6.24102913891637,
40.0912909372156));
#186017=CARTESIAN_POINT('Ctrl Pts',(58.7090548163569,-6.24767922440741,
40.0888630467851));
#186018=CARTESIAN_POINT('Ctrl Pts',(58.7099908267528,-6.25100426715293,
40.0876491015699));
#186019=CARTESIAN_POINT('Ctrl Pts',(58.7110208470228,-6.25427153376657,
40.0863558569271));
#186020=CARTESIAN_POINT('Ctrl Pts',(58.7121380880307,-6.25747333351513,
40.0849936342771));
#186021=CARTESIAN_POINT('Ctrl Pts',(58.7126967085347,-6.25907423338942,
40.0843125229521));
#186022=CARTESIAN_POINT('Ctrl Pts',(58.7132771324571,-6.26065878288339,
40.0836141747074));
#186023=CARTESIAN_POINT('Ctrl Pts',(58.7138784999415,-6.26222612320511,
40.0828999161609));
#186024=CARTESIAN_POINT('Ctrl Pts',(58.7140288418127,-6.26261795828554,
40.0827213515243));
#186025=CARTESIAN_POINT('Ctrl Pts',(58.7141804926178,-6.26300871814006,
40.0825417925841));
#186026=CARTESIAN_POINT('Ctrl Pts',(58.7143334388436,-6.2633983900505,40.082361260236));
#186027=CARTESIAN_POINT('Ctrl Pts',(58.7147922775208,-6.26456740578181,
40.0818196631917));
#186028=CARTESIAN_POINT('Ctrl Pts',(58.715262775183,-6.26572662828366,40.0812693052021));
#186029=CARTESIAN_POINT('Ctrl Pts',(58.7157445651924,-6.26687572965161,
40.0807107531874));
#186030=CARTESIAN_POINT('Ctrl Pts',(58.7191382318078,-6.27496985131128,
40.0767763849182));
#186031=CARTESIAN_POINT('Ctrl Pts',(58.7230632421217,-6.28260716192743,
40.0724140586138));
#186032=CARTESIAN_POINT('Ctrl Pts',(58.7274000190312,-6.2897833958941,40.067722122377));
#186033=CARTESIAN_POINT('Ctrl Pts',(58.729503351146,-6.2932638616134,40.0654465383722));
#186034=CARTESIAN_POINT('Ctrl Pts',(58.731704109697,-6.29663597408912,40.063092800068));
#186035=CARTESIAN_POINT('Ctrl Pts',(58.7339915094194,-6.29989941779144,
40.0606689262479));
#186036=CARTESIAN_POINT('Ctrl Pts',(58.7374933585782,-6.30489552208934,
40.0569581447805));
#186037=CARTESIAN_POINT('Ctrl Pts',(58.7411954596217,-6.30963480180868,
40.0530843804605));
#186038=CARTESIAN_POINT('Ctrl Pts',(58.745053462885,-6.31410463171043,40.0490800251458));
#186039=CARTESIAN_POINT('Ctrl Pts',(58.7468451395591,-6.31618044384063,
40.0472203818218));
#186040=CARTESIAN_POINT('Ctrl Pts',(58.7486702031823,-6.31819823791525,
40.0453323608818));
#186041=CARTESIAN_POINT('Ctrl Pts',(58.7505249478605,-6.32015576082315,
40.0434201572162));
#186042=CARTESIAN_POINT('Ctrl Pts',(58.750667106732,-6.32030579724101,40.0432735943397));
#186043=CARTESIAN_POINT('Ctrl Pts',(58.7508094261759,-6.32045551058188,
40.0431268995707));
#186044=CARTESIAN_POINT('Ctrl Pts',(58.7509519047346,-6.32060490093997,
40.0429800745037));
#186045=CARTESIAN_POINT('Ctrl Pts',(58.7529532989256,-6.32270338507381,
40.0409176249753));
#186046=CARTESIAN_POINT('Ctrl Pts',(58.7549876922215,-6.32473679726626,
40.0388310783332));
#186047=CARTESIAN_POINT('Ctrl Pts',(58.757049379421,-6.32670504964984,40.036725739981));
#186048=CARTESIAN_POINT('Ctrl Pts',(58.7644422230598,-6.33376285265574,
40.0291763710714));
#186049=CARTESIAN_POINT('Ctrl Pts',(58.7722418109928,-6.34003880538934,
40.0213310894588));
#186050=CARTESIAN_POINT('Ctrl Pts',(58.7803396486561,-6.34560292136761,
40.013283755131));
#186051=CARTESIAN_POINT('Ctrl Pts',(58.7892383587482,-6.35171732586278,
40.004440543131));
#186052=CARTESIAN_POINT('Ctrl Pts',(58.7984976730914,-6.35697262978531,
39.9953528710581));
#186053=CARTESIAN_POINT('Ctrl Pts',(58.8080148760673,-6.36142852992911,
39.9861103629531));
#186054=CARTESIAN_POINT('Ctrl Pts',(58.8182910667897,-6.36623978380624,
39.9761307737523));
#186055=CARTESIAN_POINT('Ctrl Pts',(58.8288688921894,-6.37011968263873,
39.9659696935969));
#186056=CARTESIAN_POINT('Ctrl Pts',(58.8396533761932,-6.37309732669947,
39.9557128217455));
#186057=CARTESIAN_POINT('Ctrl Pts',(58.8503473894546,-6.37604999138532,
39.9455419945126));
#186058=CARTESIAN_POINT('Ctrl Pts',(58.861246040348,-6.37811557911247,39.9352756289323));
#186059=CARTESIAN_POINT('Ctrl Pts',(58.872270023448,-6.37927424642578,39.92499));
#186060=CARTESIAN_POINT('Origin',(0.00159301378019908,0.0151565136854131,
39.92499));
#186061=CARTESIAN_POINT('Ctrl Pts',(62.5037563256535,-6.55408556365946,
40.10025));
#186062=CARTESIAN_POINT('Ctrl Pts',(62.5046505412978,-6.54554330587368,
40.10025));
#186063=CARTESIAN_POINT('Ctrl Pts',(62.5048232320879,-6.53700226086583,
40.0995859581841));
#186064=CARTESIAN_POINT('Ctrl Pts',(62.5043472028589,-6.52859457177331,
40.0983275959619));
#186065=CARTESIAN_POINT('Ctrl Pts',(62.5040430428431,-6.52322245869402,
40.0975235624066));
#186066=CARTESIAN_POINT('Ctrl Pts',(62.5034749678471,-6.5179047148956,40.0964777059489));
#186067=CARTESIAN_POINT('Ctrl Pts',(62.5026702669707,-6.5126735674084,40.095214991596));
#186068=CARTESIAN_POINT('Ctrl Pts',(62.5015720117389,-6.50553410072647,
40.0934916398701));
#186069=CARTESIAN_POINT('Ctrl Pts',(62.5000273428098,-6.49855818190772,
40.091364392163));
#186070=CARTESIAN_POINT('Ctrl Pts',(62.4980940659029,-6.49182203260176,
40.0889118607712));
#186071=CARTESIAN_POINT('Ctrl Pts',(62.4971274274495,-6.48845395794878,
40.0876855950754));
#186072=CARTESIAN_POINT('Ctrl Pts',(62.4960636607366,-6.48514561818735,
40.0863782327526));
#186073=CARTESIAN_POINT('Ctrl Pts',(62.494910155573,-6.48190505740164,40.0850006373333));
#186074=CARTESIAN_POINT('Ctrl Pts',(62.4943334029912,-6.48028477700878,
40.0843118396237));
#186075=CARTESIAN_POINT('Ctrl Pts',(62.4937342176673,-6.47868142404681,
40.0836054919164));
#186076=CARTESIAN_POINT('Ctrl Pts',(62.4931135352114,-6.47709589524266,
40.0828829920417));
#186077=CARTESIAN_POINT('Ctrl Pts',(62.4929583645974,-6.47669951304162,
40.0827023670731));
#186078=CARTESIAN_POINT('Ctrl Pts',(62.4928018504535,-6.47630424448174,
40.0825207326932));
#186079=CARTESIAN_POINT('Ctrl Pts',(62.4926440074816,-6.47591010283074,
40.0823381109275));
#186080=CARTESIAN_POINT('Ctrl Pts',(62.4921704785661,-6.47472767787775,
40.0817902456303));
#186081=CARTESIAN_POINT('Ctrl Pts',(62.4916849899864,-6.47355539694469,
40.0812334935553));
#186082=CARTESIAN_POINT('Ctrl Pts',(62.4911879405752,-6.47239360181811,
40.0806684524227));
#186083=CARTESIAN_POINT('Ctrl Pts',(62.4877530207469,-6.46436487665163,
40.0767636676136));
#186084=CARTESIAN_POINT('Ctrl Pts',(62.4837949925046,-6.45678933786372,
40.0724404510887));
#186085=CARTESIAN_POINT('Ctrl Pts',(62.4794326364364,-6.4496685356396,40.0677949937407));
#186086=CARTESIAN_POINT('Ctrl Pts',(62.4772645574451,-6.4461295164806,40.0654862141904));
#186087=CARTESIAN_POINT('Ctrl Pts',(62.474996003895,-6.44270272394338,40.0630972003215));
#186088=CARTESIAN_POINT('Ctrl Pts',(62.4726384024734,-6.43938822718924,
40.0606363359906));
#186089=CARTESIAN_POINT('Ctrl Pts',(62.4674371815967,-6.43207595228354,
40.0552073017123));
#186090=CARTESIAN_POINT('Ctrl Pts',(62.461813233051,-6.4253038174399,40.0494204304519));
#186091=CARTESIAN_POINT('Ctrl Pts',(62.4558957623411,-6.41913840445425,
40.0434049749851));
#186092=CARTESIAN_POINT('Ctrl Pts',(62.4537340356675,-6.41688610134064,
40.0412074532442));
#186093=CARTESIAN_POINT('Ctrl Pts',(62.4515361835425,-6.41470741397467,
40.0389814735788));
#186094=CARTESIAN_POINT('Ctrl Pts',(62.4493074469123,-6.41260146153638,
40.0367321210017));
#186095=CARTESIAN_POINT('Ctrl Pts',(62.4418213564087,-6.4055277901409,40.029176783714));
#186096=CARTESIAN_POINT('Ctrl Pts',(62.4339335724863,-6.39923601079879,
40.0213235332573));
#186097=CARTESIAN_POINT('Ctrl Pts',(62.4257522463025,-6.39365709371028,
40.0132649215854));
#186098=CARTESIAN_POINT('Ctrl Pts',(62.4167599996848,-6.38752520296383,
40.0044075527527));
#186099=CARTESIAN_POINT('Ctrl Pts',(62.4074126717505,-6.38225398283454,
39.9953016253712));
#186100=CARTESIAN_POINT('Ctrl Pts',(62.3978127557447,-6.37778536209576,
39.9860353422349));
#186101=CARTESIAN_POINT('Ctrl Pts',(62.3874732348828,-6.3729724660949,39.9760551582683));
#186102=CARTESIAN_POINT('Ctrl Pts',(62.3768396913512,-6.36908997057771,
39.9658879738141));
#186103=CARTESIAN_POINT('Ctrl Pts',(62.3660067738148,-6.36611161569942,
39.9556174643237));
#186104=CARTESIAN_POINT('Ctrl Pts',(62.3553201372421,-6.36317347866826,
39.9454856413893));
#186105=CARTESIAN_POINT('Ctrl Pts',(62.3444380411296,-6.36111515612444,
39.9352519465108));
#186106=CARTESIAN_POINT('Ctrl Pts',(62.3334394572619,-6.35995915837802,
39.92499));
#186107=CARTESIAN_POINT('Ctrl Pts',(58.912095367953,-6.00036140429046,39.92499));
#186108=CARTESIAN_POINT('Ctrl Pts',(58.9015696628156,-5.99925510810136,
39.9348107241714));
#186109=CARTESIAN_POINT('Ctrl Pts',(58.8909945468917,-5.99898299131194,
39.9446038383152));
#186110=CARTESIAN_POINT('Ctrl Pts',(58.8804276387814,-5.99953795195244,
39.9543158069359));
#186111=CARTESIAN_POINT('Ctrl Pts',(58.8702243592831,-6.00007381527843,
39.963693567136));
#186112=CARTESIAN_POINT('Ctrl Pts',(58.8600274754076,-6.00138095727599,
39.9729968320952));
#186113=CARTESIAN_POINT('Ctrl Pts',(58.8498890377538,-6.00349883563849,
39.9821731151294));
#186114=CARTESIAN_POINT('Ctrl Pts',(58.8403050390087,-6.00550089396953,
39.9908475764307));
#186115=CARTESIAN_POINT('Ctrl Pts',(58.8307723843936,-6.00822762538385,
39.9994093733799));
#186116=CARTESIAN_POINT('Ctrl Pts',(58.8213500689115,-6.0117515363934,40.0077966115792));
#186117=CARTESIAN_POINT('Ctrl Pts',(58.8126722744237,-6.01499699931519,
40.0155211172544));
#186118=CARTESIAN_POINT('Ctrl Pts',(58.8040875818627,-6.01891888228866,
40.0230979940969));
#186119=CARTESIAN_POINT('Ctrl Pts',(58.7956642413131,-6.02360485257075,
40.0304554104694));
#186120=CARTESIAN_POINT('Ctrl Pts',(58.7931525711953,-6.02500211431762,
40.0326492435145));
#186121=CARTESIAN_POINT('Ctrl Pts',(58.7906554330116,-6.02646752363586,
40.0348233715043));
#186122=CARTESIAN_POINT('Ctrl Pts',(58.7881751602884,-6.02800395803705,
40.0369753512356));
#186123=CARTESIAN_POINT('Ctrl Pts',(58.7857202298425,-6.02952469386352,
40.0391053430352));
#186124=CARTESIAN_POINT('Ctrl Pts',(58.783284225042,-6.03111319985504,40.041211089324));
#186125=CARTESIAN_POINT('Ctrl Pts',(58.7808720541407,-6.0327702554203,40.0432881154904));
#186126=CARTESIAN_POINT('Ctrl Pts',(58.7807043164937,-6.03288548382362,
40.043432547828));
#186127=CARTESIAN_POINT('Ctrl Pts',(58.7805366835715,-6.0330010380091,40.0435768364421));
#186128=CARTESIAN_POINT('Ctrl Pts',(58.7803691562898,-6.03311691890562,
40.0437209807855));
#186129=CARTESIAN_POINT('Ctrl Pts',(58.7730241465597,-6.03819756191435,
40.0500407968421));
#186130=CARTESIAN_POINT('Ctrl Pts',(58.7659160498048,-6.04393622206,40.0560490279346));
#186131=CARTESIAN_POINT('Ctrl Pts',(58.7591607781928,-6.05034076157591,
40.0616647108616));
#186132=CARTESIAN_POINT('Ctrl Pts',(58.7528636909919,-6.05631090550629,
40.0668995033488));
#186133=CARTESIAN_POINT('Ctrl Pts',(58.746872812682,-6.06286038933354,40.0717933267486));
#186134=CARTESIAN_POINT('Ctrl Pts',(58.7413107827875,-6.07000150504443,
40.0762460303077));
#186135=CARTESIAN_POINT('Ctrl Pts',(58.739276120295,-6.07261381755741,40.0778748868751));
#186136=CARTESIAN_POINT('Ctrl Pts',(58.7372991657062,-6.07530531160687,
40.0794443522249));
#186137=CARTESIAN_POINT('Ctrl Pts',(58.735387140493,-6.07807653793555,40.0809482021492));
#186138=CARTESIAN_POINT('Ctrl Pts',(58.7349273623043,-6.07874292528918,
40.0813098278168));
#186139=CARTESIAN_POINT('Ctrl Pts',(58.7344713442223,-6.07941450700183,
40.0816679525672));
#186140=CARTESIAN_POINT('Ctrl Pts',(58.7340192051468,-6.08009121771075,
40.082022419258));
#186141=CARTESIAN_POINT('Ctrl Pts',(58.7335811954175,-6.08074678121001,
40.0823658088648));
#186142=CARTESIAN_POINT('Ctrl Pts',(58.7331468260468,-6.08140715812707,
40.0827057654616));
#186143=CARTESIAN_POINT('Ctrl Pts',(58.7327162055066,-6.08207228526541,
40.0830421470151));
#186144=CARTESIAN_POINT('Ctrl Pts',(58.7279982598321,-6.08935952173594,
40.0867275956805));
#186145=CARTESIAN_POINT('Ctrl Pts',(58.7237275533352,-6.09722197243172,
40.089982343203));
#186146=CARTESIAN_POINT('Ctrl Pts',(58.7200553115704,-6.1055470990915,40.0926299529354));
#186147=CARTESIAN_POINT('Ctrl Pts',(58.7185323234526,-6.10899977726292,
40.0937279956083));
#186148=CARTESIAN_POINT('Ctrl Pts',(58.7171120447816,-6.11253167434582,
40.0947220371802));
#186149=CARTESIAN_POINT('Ctrl Pts',(58.7158039367398,-6.11613350280225,
40.0956014538692));
#186150=CARTESIAN_POINT('Ctrl Pts',(58.7135728221602,-6.12227679657149,
40.097101390674));
#186151=CARTESIAN_POINT('Ctrl Pts',(58.7116702942288,-6.12862250657786,
40.0982667904316));
#186152=CARTESIAN_POINT('Ctrl Pts',(58.7101471179289,-6.13511848061099,
40.0990539325582));
#186153=CARTESIAN_POINT('Ctrl Pts',(58.7093855297789,-6.13836646762756,
40.0994475036216));
#186154=CARTESIAN_POINT('Ctrl Pts',(58.7087202098052,-6.14165223896364,
40.0997467259952));
#186155=CARTESIAN_POINT('Ctrl Pts',(58.7081575578112,-6.14496923836494,
40.0999473488896));
#186156=CARTESIAN_POINT('Ctrl Pts',(58.7075949058173,-6.14828623776625,
40.100147971784));
#186157=CARTESIAN_POINT('Ctrl Pts',(58.7071349090267,-6.15163442139592,
40.10025));
#186158=CARTESIAN_POINT('Ctrl Pts',(58.7067819056643,-6.15500747092316,
40.10025));
#186159=CARTESIAN_POINT('Origin',(56.9874003490102,-12.1286263473644,39.92499));
#186160=CARTESIAN_POINT('Ctrl Pts',(61.2479592423878,-13.2134115091894,
39.92499));
#186161=CARTESIAN_POINT('Ctrl Pts',(61.2583377107546,-13.2156175207409,
39.9348354642018));
#186162=CARTESIAN_POINT('Ctrl Pts',(61.2688594460198,-13.2169980909548,
39.9446440828459));
#186163=CARTESIAN_POINT('Ctrl Pts',(61.2794654334802,-13.2175561899854,
39.9543641760333));
#186164=CARTESIAN_POINT('Ctrl Pts',(61.2897267895027,-13.2180961541208,
39.9637684240714));
#186165=CARTESIAN_POINT('Ctrl Pts',(61.3000683010468,-13.2178662282939,
39.9730909636398));
#186166=CARTESIAN_POINT('Ctrl Pts',(61.3104421535935,-13.2168232529018,
39.9822808977143));
#186167=CARTESIAN_POINT('Ctrl Pts',(61.3202551793177,-13.2158366624037,
39.9909740094652));
#186168=CARTESIAN_POINT('Ctrl Pts',(61.3300980668405,-13.2141224659043,
39.9995492765004));
#186169=CARTESIAN_POINT('Ctrl Pts',(61.3399200511722,-13.211603302198,40.0079462328697));
#186170=CARTESIAN_POINT('Ctrl Pts',(61.3489668090858,-13.2092829702341,
40.0156804369693));
#186171=CARTESIAN_POINT('Ctrl Pts',(61.3579963605654,-13.2062795322631,
40.0232638017425));
#186172=CARTESIAN_POINT('Ctrl Pts',(61.3669504518463,-13.2024991065229,
40.030625726997));
#186173=CARTESIAN_POINT('Ctrl Pts',(61.3695476933562,-13.2014025487205,
40.0327611416654));
#186174=CARTESIAN_POINT('Ctrl Pts',(61.3721384315552,-13.2002403977584,
40.0348777427272));
#186175=CARTESIAN_POINT('Ctrl Pts',(61.374720822464,-13.1990098046947,40.0369733168701));
#186176=CARTESIAN_POINT('Ctrl Pts',(61.3775203002416,-13.1976757626938,
40.039245053974));
#186177=CARTESIAN_POINT('Ctrl Pts',(61.3803065372249,-13.1962641169258,
40.041487875195));
#186178=CARTESIAN_POINT('Ctrl Pts',(61.3830766416486,-13.194772102191,40.0436985701601));
#186179=CARTESIAN_POINT('Ctrl Pts',(61.3906792149762,-13.1906772560436,
40.0497658398386));
#186180=CARTESIAN_POINT('Ctrl Pts',(61.3981301363758,-13.1859443571664,
40.0555581699984));
#186181=CARTESIAN_POINT('Ctrl Pts',(61.4053257594953,-13.1805769309629,
40.0609828468885));
#186182=CARTESIAN_POINT('Ctrl Pts',(61.41190936399,-13.1756660273912,40.0659461317304));
#186183=CARTESIAN_POINT('Ctrl Pts',(61.418268002635,-13.1702212276779,40.0706039980705));
#186184=CARTESIAN_POINT('Ctrl Pts',(61.4243186078271,-13.1642115906185,
40.0748843180601));
#186185=CARTESIAN_POINT('Ctrl Pts',(61.4272906453324,-13.1612596765262,
40.0769867972569));
#186186=CARTESIAN_POINT('Ctrl Pts',(61.4301878975266,-13.1581712727458,
40.0789976708174));
#186187=CARTESIAN_POINT('Ctrl Pts',(61.4329973166796,-13.154941736613,40.0809050491499));
#186188=CARTESIAN_POINT('Ctrl Pts',(61.4335303765997,-13.1543289635879,
40.0812669556104));
#186189=CARTESIAN_POINT('Ctrl Pts',(61.4340602468995,-13.1537105783544,
40.0816253922032));
#186190=CARTESIAN_POINT('Ctrl Pts',(61.4345867973822,-13.1530866324248,
40.0819801989139));
#186191=CARTESIAN_POINT('Ctrl Pts',(61.4350968931623,-13.1524821848055,
40.0823239179149));
#186192=CARTESIAN_POINT('Ctrl Pts',(61.4356038733673,-13.1518725186281,
40.0826642303498));
#186193=CARTESIAN_POINT('Ctrl Pts',(61.4361076188515,-13.1512576844883,
40.0830009916099));
#186194=CARTESIAN_POINT('Ctrl Pts',(61.4415973333395,-13.1445573487221,
40.0866709464312));
#186195=CARTESIAN_POINT('Ctrl Pts',(61.4467061867047,-13.137238593115,40.0899175831877));
#186196=CARTESIAN_POINT('Ctrl Pts',(61.4512683418496,-13.1293950794801,
40.0925642067061));
#186197=CARTESIAN_POINT('Ctrl Pts',(61.453194968297,-13.1260827149661,40.0936818922527));
#186198=CARTESIAN_POINT('Ctrl Pts',(61.4550242827916,-13.1226771582918,
40.094693009479));
#186199=CARTESIAN_POINT('Ctrl Pts',(61.4567450522889,-13.1191869390028,
40.0955863397545));
#186200=CARTESIAN_POINT('Ctrl Pts',(61.4596427851248,-13.1133094969312,
40.0970906856166));
#186201=CARTESIAN_POINT('Ctrl Pts',(61.4622303029113,-13.1071927578067,
40.0982599215483));
#186202=CARTESIAN_POINT('Ctrl Pts',(61.4644496675152,-13.1008831031057,
40.0990497370453));
#186203=CARTESIAN_POINT('Ctrl Pts',(61.4650045086662,-13.0993056894304,
40.0992471909196));
#186204=CARTESIAN_POINT('Ctrl Pts',(61.4655361149186,-13.097716155517,40.0994209989363));
#186205=CARTESIAN_POINT('Ctrl Pts',(61.4660432808488,-13.096115154835,40.0995705982975));
#186206=CARTESIAN_POINT('Ctrl Pts',(61.4668040297442,-13.0937136538119,
40.0997949973393));
#186207=CARTESIAN_POINT('Ctrl Pts',(61.4675097715123,-13.0912863650433,
40.0999649129781));
#186208=CARTESIAN_POINT('Ctrl Pts',(61.4681580753693,-13.0888358608678,
40.1000786629733));
#186209=CARTESIAN_POINT('Ctrl Pts',(61.4688063792262,-13.0863853566924,
40.1001924129685));
#186210=CARTESIAN_POINT('Ctrl Pts',(61.4693972526619,-13.0839116459751,
40.10025));
#186211=CARTESIAN_POINT('Ctrl Pts',(61.4699285681954,-13.0814171332233,
40.10025));
#186212=CARTESIAN_POINT('Ctrl Pts',(57.7354693911205,-12.2876333308471,
40.10025));
#186213=CARTESIAN_POINT('Ctrl Pts',(57.7336713548546,-12.2960739442505,
40.10025));
#186214=CARTESIAN_POINT('Ctrl Pts',(57.7325856410805,-12.3045898170426,
40.0995786334241));
#186215=CARTESIAN_POINT('Ctrl Pts',(57.7321565492375,-12.3130404786508,
40.0983063763366));
#186216=CARTESIAN_POINT('Ctrl Pts',(57.7318793999343,-12.3184987389617,
40.0974846287992));
#186217=CARTESIAN_POINT('Ctrl Pts',(57.7318752477672,-12.3239297572686,
40.0964130309338));
#186218=CARTESIAN_POINT('Ctrl Pts',(57.7321203363021,-12.3292970476683,
40.0951176960924));
#186219=CARTESIAN_POINT('Ctrl Pts',(57.7324451871157,-12.3364110836358,
40.0934008039614));
#186220=CARTESIAN_POINT('Ctrl Pts',(57.7332135204776,-12.3434117286774,
40.0912909372157));
#186221=CARTESIAN_POINT('Ctrl Pts',(57.7343801629266,-12.3502210637609,
40.0888630467851));
#186222=CARTESIAN_POINT('Ctrl Pts',(57.7349634841511,-12.3536257313026,
40.0876491015699));
#186223=CARTESIAN_POINT('Ctrl Pts',(57.735646339504,-12.3569827659239,40.0863558569271));
#186224=CARTESIAN_POINT('Ctrl Pts',(57.7364227809414,-12.3602838093641,
40.0849936342771));
#186225=CARTESIAN_POINT('Ctrl Pts',(57.7368110016602,-12.3619343310841,
40.0843125229521));
#186226=CARTESIAN_POINT('Ctrl Pts',(57.737222615436,-12.3635708710708,40.0836141747074));
#186227=CARTESIAN_POINT('Ctrl Pts',(57.7376568568912,-12.3651924853573,
40.0828999161609));
#186228=CARTESIAN_POINT('Ctrl Pts',(57.737765417255,-12.3655978889289,40.0827213515243));
#186229=CARTESIAN_POINT('Ctrl Pts',(57.7378753917741,-12.3660023599857,
40.0825417925842));
#186230=CARTESIAN_POINT('Ctrl Pts',(57.7379867683384,-12.3664058844666,
40.0823612602361));
#186231=CARTESIAN_POINT('Ctrl Pts',(57.7383208980314,-12.3676164579092,
40.0818196631917));
#186232=CARTESIAN_POINT('Ctrl Pts',(57.7386676465115,-12.3688185104665,
40.0812693052021));
#186233=CARTESIAN_POINT('Ctrl Pts',(57.7390266834247,-12.3700116777062,
40.0807107531875));
#186234=CARTESIAN_POINT('Ctrl Pts',(57.7415556930806,-12.3784161936765,
40.0767763849183));
#186235=CARTESIAN_POINT('Ctrl Pts',(57.7446608854351,-12.3864219416023,
40.072414058614));
#186236=CARTESIAN_POINT('Ctrl Pts',(57.7482237843182,-12.3940121800342,
40.0677221223773));
#186237=CARTESIAN_POINT('Ctrl Pts',(57.7499517864266,-12.397693437472,40.0654465383724));
#186238=CARTESIAN_POINT('Ctrl Pts',(57.751788007257,-12.4012771190722,40.0630928000681));
#186239=CARTESIAN_POINT('Ctrl Pts',(57.7537217536093,-12.4047617836665,
40.0606689262479));
#186240=CARTESIAN_POINT('Ctrl Pts',(57.7566821841674,-12.4100965616934,
40.0569581447806));
#186241=CARTESIAN_POINT('Ctrl Pts',(57.759868615088,-12.4151968540755,40.0530843804605));
#186242=CARTESIAN_POINT('Ctrl Pts',(57.7632382593551,-12.4200454689338,
40.0490800251457));
#186243=CARTESIAN_POINT('Ctrl Pts',(57.7648031395849,-12.4222971907574,
40.0472203818218));
#186244=CARTESIAN_POINT('Ctrl Pts',(57.7664072884048,-12.4244947022408,
40.0453323608818));
#186245=CARTESIAN_POINT('Ctrl Pts',(57.7680472557362,-12.4266353752444,
40.0434201572162));
#186246=CARTESIAN_POINT('Ctrl Pts',(57.7681729527704,-12.4267994493954,
40.0432735943397));
#186247=CARTESIAN_POINT('Ctrl Pts',(57.768298843268,-12.4269632190237,40.0431268995707));
#186248=CARTESIAN_POINT('Ctrl Pts',(57.7684249257697,-12.4271266840706,
40.0429800745037));
#186249=CARTESIAN_POINT('Ctrl Pts',(57.7701960047922,-12.4294228751479,
40.0409176249753));
#186250=CARTESIAN_POINT('Ctrl Pts',(57.7720067040171,-12.4316578001005,
40.0388310783333));
#186251=CARTESIAN_POINT('Ctrl Pts',(57.7738513586814,-12.4338307751863,
40.036725739981));
#186252=CARTESIAN_POINT('Ctrl Pts',(57.7804659622464,-12.4416226773929,
40.0291763710721));
#186253=CARTESIAN_POINT('Ctrl Pts',(57.7875668075252,-12.4486795287409,
40.0213310894602));
#186254=CARTESIAN_POINT('Ctrl Pts',(57.7950386758931,-12.4550596184359,
40.0132837551331));
#186255=CARTESIAN_POINT('Ctrl Pts',(57.8032495086137,-12.462070696074,40.004440543134));
#186256=CARTESIAN_POINT('Ctrl Pts',(57.8119087706201,-12.4682650727906,
39.995352871062));
#186257=CARTESIAN_POINT('Ctrl Pts',(57.820908068967,-12.4736913816486,39.9861103629579));
#186258=CARTESIAN_POINT('Ctrl Pts',(57.830625052666,-12.4795504333977,39.9761307737582));
#186259=CARTESIAN_POINT('Ctrl Pts',(57.8407393717675,-12.484514761572,39.9659696936041));
#186260=CARTESIAN_POINT('Ctrl Pts',(57.8511535286804,-12.4886033793272,
39.9557128217538));
#186261=CARTESIAN_POINT('Ctrl Pts',(57.8614803215187,-12.4926576977809,
39.9455419945182));
#186262=CARTESIAN_POINT('Ctrl Pts',(57.8721033557542,-12.4958511892331,
39.9352756289351));
#186263=CARTESIAN_POINT('Ctrl Pts',(57.8829458346105,-12.4981558292588,
39.92499));
#186264=CARTESIAN_POINT('Origin',(0.00316857416806278,0.0149069694351844,
39.92499));
#186265=CARTESIAN_POINT('Ctrl Pts',(61.4762657165316,-13.0516031943529,
40.10025));
#186266=CARTESIAN_POINT('Ctrl Pts',(61.4780479426482,-13.0432012029365,
40.10025));
#186267=CARTESIAN_POINT('Ctrl Pts',(61.4791124697294,-13.03472499777,40.0995859581842));
#186268=CARTESIAN_POINT('Ctrl Pts',(61.4795178910588,-13.0263136082746,
40.098327595962));
#186269=CARTESIAN_POINT('Ctrl Pts',(61.4797769359881,-13.0209391308135,
40.0975235624068));
#186270=CARTESIAN_POINT('Ctrl Pts',(61.4797678285537,-13.0155911381655,
40.096477705949));
#186271=CARTESIAN_POINT('Ctrl Pts',(61.4795143397209,-13.0103045333053,
40.0952149915961));
#186272=CARTESIAN_POINT('Ctrl Pts',(61.479168378327,-13.0030893784372,40.0934916398701));
#186273=CARTESIAN_POINT('Ctrl Pts',(61.4783613533299,-12.9959902125622,
40.0913643921631));
#186274=CARTESIAN_POINT('Ctrl Pts',(61.4771427864515,-12.9890888821228,
40.0889118607713));
#186275=CARTESIAN_POINT('Ctrl Pts',(61.4765335030122,-12.9856382169031,
40.0876855950754));
#186276=CARTESIAN_POINT('Ctrl Pts',(61.4758213793959,-12.9822368066732,
40.0863782327526));
#186277=CARTESIAN_POINT('Ctrl Pts',(61.4750129240934,-12.9788934238964,
40.0850006373334));
#186278=CARTESIAN_POINT('Ctrl Pts',(61.4746086964421,-12.977221732508,40.0843118396237));
#186279=CARTESIAN_POINT('Ctrl Pts',(61.4741803895393,-12.9755645309602,
40.0836054919164));
#186280=CARTESIAN_POINT('Ctrl Pts',(61.4737288401362,-12.9739228088655,
40.0828829920418));
#186281=CARTESIAN_POINT('Ctrl Pts',(61.4736159527854,-12.9735123783418,
40.0827023670731));
#186282=CARTESIAN_POINT('Ctrl Pts',(61.4735016128575,-12.9731029149215,
40.0825207326933));
#186283=CARTESIAN_POINT('Ctrl Pts',(61.4733858335871,-12.9726944333364,
40.0823381109275));
#186284=CARTESIAN_POINT('Ctrl Pts',(61.4730384957757,-12.9714689885812,
40.0817902456303));
#186285=CARTESIAN_POINT('Ctrl Pts',(61.4726782034777,-12.9702523821505,
40.0812334935553));
#186286=CARTESIAN_POINT('Ctrl Pts',(61.4723053176144,-12.9690449956481,
40.0806684524227));
#186287=CARTESIAN_POINT('Ctrl Pts',(61.46972844494,-12.9607012057873,40.0767636676137));
#186288=CARTESIAN_POINT('Ctrl Pts',(61.4665839586187,-12.952753439984,40.0724404510889));
#186289=CARTESIAN_POINT('Ctrl Pts',(61.4629898265073,-12.9452156558837,
40.0677949937411));
#186290=CARTESIAN_POINT('Ctrl Pts',(61.4612035527136,-12.9414693978765,
40.0654862141907));
#186291=CARTESIAN_POINT('Ctrl Pts',(61.459305623895,-12.9378242492507,40.0630972003217));
#186292=CARTESIAN_POINT('Ctrl Pts',(61.4573073969127,-12.9342814732027,
40.0606363359906));
#186293=CARTESIAN_POINT('Ctrl Pts',(61.4528990097271,-12.9264655800787,
40.0552073017123));
#186294=CARTESIAN_POINT('Ctrl Pts',(61.4480137506082,-12.9191426809994,
40.0494204304519));
#186295=CARTESIAN_POINT('Ctrl Pts',(61.4427731575668,-12.9123924986714,
40.0434049749851));
#186296=CARTESIAN_POINT('Ctrl Pts',(61.4408587028414,-12.9099265719427,
40.0412074532442));
#186297=CARTESIAN_POINT('Ctrl Pts',(61.4389006256227,-12.907530081549,40.0389814735788));
#186298=CARTESIAN_POINT('Ctrl Pts',(61.436904230217,-12.9052026993235,40.0367321210016));
#186299=CARTESIAN_POINT('Ctrl Pts',(61.4301985493013,-12.8973852687041,
40.0291767837142));
#186300=CARTESIAN_POINT('Ctrl Pts',(61.4230116455107,-12.8903034584557,
40.0213235332578));
#186301=CARTESIAN_POINT('Ctrl Pts',(61.415458293118,-12.8838999218055,40.0132649215862));
#186302=CARTESIAN_POINT('Ctrl Pts',(61.407156264085,-12.876861676478,40.0044075527538));
#186303=CARTESIAN_POINT('Ctrl Pts',(61.3984111343311,-12.8706422708196,
39.9953016253726));
#186304=CARTESIAN_POINT('Ctrl Pts',(61.3893309057287,-12.8651946651852,
39.9860353422365));
#186305=CARTESIAN_POINT('Ctrl Pts',(61.3795511104669,-12.8593273605057,
39.9760551582702));
#186306=CARTESIAN_POINT('Ctrl Pts',(61.3693816498897,-12.8543546257407,
39.9658879738164));
#186307=CARTESIAN_POINT('Ctrl Pts',(61.3589193990679,-12.8502602383793,
39.9556174643262));
#186308=CARTESIAN_POINT('Ctrl Pts',(61.3485984239564,-12.8462211390713,
39.945485641391));
#186309=CARTESIAN_POINT('Ctrl Pts',(61.3379910943966,-12.8430366034496,
39.9352519465116));
#186310=CARTESIAN_POINT('Ctrl Pts',(61.3271735965893,-12.8407372733098,
39.92499));
#186311=CARTESIAN_POINT('Ctrl Pts',(57.9621601888121,-12.1254815933792,
39.92499));
#186312=CARTESIAN_POINT('Ctrl Pts',(57.9518077840279,-12.1232811218132,
39.9348107241727));
#186313=CARTESIAN_POINT('Ctrl Pts',(57.9413190436441,-12.1219050950916,
39.9446038383178));
#186314=CARTESIAN_POINT('Ctrl Pts',(57.9307520129777,-12.1213524729335,
39.9543158069397));
#186315=CARTESIAN_POINT('Ctrl Pts',(57.9205486151411,-12.120818867618,39.9636935671407));
#186316=CARTESIAN_POINT('Ctrl Pts',(57.9102709573172,-12.1210529843536,
39.9729968321007));
#186317=CARTESIAN_POINT('Ctrl Pts',(57.899966680514,-12.1220995054494,39.9821731151357));
#186318=CARTESIAN_POINT('Ctrl Pts',(57.8902259118354,-12.123088795635,39.9908475764376));
#186319=CARTESIAN_POINT('Ctrl Pts',(57.8804604570545,-12.1248041559921,
39.9994093733873));
#186320=CARTESIAN_POINT('Ctrl Pts',(57.8707214089994,-12.1273238624914,
40.007796611587));
#186321=CARTESIAN_POINT('Ctrl Pts',(57.8617519091254,-12.129644469906,40.0155211172626));
#186322=CARTESIAN_POINT('Ctrl Pts',(57.8528042960076,-12.1326475236739,
40.0230979941055));
#186323=CARTESIAN_POINT('Ctrl Pts',(57.8439372821258,-12.1364273448781,
40.0304554104783));
#186324=CARTESIAN_POINT('Ctrl Pts',(57.8412933175801,-12.13755441126,40.0326492435204));
#186325=CARTESIAN_POINT('Ctrl Pts',(57.8386566820001,-12.1387507708942,
40.0348233715072));
#186326=CARTESIAN_POINT('Ctrl Pts',(57.8360293953471,-12.140019529449,40.0369753512355));
#186327=CARTESIAN_POINT('Ctrl Pts',(57.8334289530881,-12.1412753244186,
40.0391053430352));
#186328=CARTESIAN_POINT('Ctrl Pts',(57.8308402488866,-12.1426004965698,
40.041211089324));
#186329=CARTESIAN_POINT('Ctrl Pts',(57.8282680826381,-12.1439963340938,
40.0432881154904));
#186330=CARTESIAN_POINT('Ctrl Pts',(57.8280892192276,-12.1440933979054,
40.0434325478279));
#186331=CARTESIAN_POINT('Ctrl Pts',(57.8279104259146,-12.1441907966612,
40.0435768364421));
#186332=CARTESIAN_POINT('Ctrl Pts',(57.8277317035128,-12.1442885313808,
40.0437209807855));
#186333=CARTESIAN_POINT('Ctrl Pts',(57.8198958587084,-12.1485735795158,
40.0500407968421));
#186334=CARTESIAN_POINT('Ctrl Pts',(57.8122268475249,-12.1535378042502,
40.0560490279347));
#186335=CARTESIAN_POINT('Ctrl Pts',(57.8048391253239,-12.159201140868,40.0616647108618));
#186336=CARTESIAN_POINT('Ctrl Pts',(57.797952484255,-12.1644803548773,40.0668995033491));
#186337=CARTESIAN_POINT('Ctrl Pts',(57.7913098171235,-12.1703677426436,
40.071793326749));
#186338=CARTESIAN_POINT('Ctrl Pts',(57.7850318067593,-12.1768883481381,
40.0762460303082));
#186339=CARTESIAN_POINT('Ctrl Pts',(57.7827352293485,-12.179273669986,40.0778748868754));
#186340=CARTESIAN_POINT('Ctrl Pts',(57.7804877669872,-12.1817437717241,
40.0794443522251));
#186341=CARTESIAN_POINT('Ctrl Pts',(57.7782965440188,-12.1842999559275,
40.0809482021492));
#186342=CARTESIAN_POINT('Ctrl Pts',(57.7777696280971,-12.184914632834,40.0813098278169));
#186343=CARTESIAN_POINT('Ctrl Pts',(57.7772459087255,-12.1855348686824,
40.0816679525672));
#186344=CARTESIAN_POINT('Ctrl Pts',(57.7767255109847,-12.1861606108965,
40.0820224192581));
#186345=CARTESIAN_POINT('Ctrl Pts',(57.7762213756734,-12.1867667986664,
40.0823658088648));
#186346=CARTESIAN_POINT('Ctrl Pts',(57.7757203576392,-12.1873781540068,
40.0827057654617));
#186347=CARTESIAN_POINT('Ctrl Pts',(57.7752225713658,-12.1879946254058,
40.0830421470151));
#186348=CARTESIAN_POINT('Ctrl Pts',(57.7697687474619,-12.1947487820209,
40.0867275956804));
#186349=CARTESIAN_POINT('Ctrl Pts',(57.7646995864536,-12.2021217510015,
40.0899823432026));
#186350=CARTESIAN_POINT('Ctrl Pts',(57.7601772489173,-12.2100174179573,
40.092629952935));
#186351=CARTESIAN_POINT('Ctrl Pts',(57.7583017007441,-12.2132919863894,
40.0937279956081));
#186352=CARTESIAN_POINT('Ctrl Pts',(57.7565200187335,-12.2166560758241,
40.0947220371801));
#186353=CARTESIAN_POINT('Ctrl Pts',(57.7548425830507,-12.2201014385646,
40.0956014538693));
#186354=CARTESIAN_POINT('Ctrl Pts',(57.7519815416931,-12.2259778637494,
40.097101390674));
#186355=CARTESIAN_POINT('Ctrl Pts',(57.7494261286934,-12.2320899429714,
40.0982667904316));
#186356=CARTESIAN_POINT('Ctrl Pts',(57.7472322823296,-12.2383911161012,
40.0990539325583));
#186357=CARTESIAN_POINT('Ctrl Pts',(57.7461353591478,-12.2415417026661,
40.0994475036216));
#186358=CARTESIAN_POINT('Ctrl Pts',(57.745130227238,-12.2447399293285,40.0997467259952));
#186359=CARTESIAN_POINT('Ctrl Pts',(57.7442239366604,-12.2479799447118,
40.0999473488896));
#186360=CARTESIAN_POINT('Ctrl Pts',(57.7433176460829,-12.251219960095,40.100147971784));
#186361=CARTESIAN_POINT('Ctrl Pts',(57.7425101887133,-12.2545017192668,
40.10025));
#186362=CARTESIAN_POINT('Ctrl Pts',(57.7418065394566,-12.2578193919768,
40.10025));
#186363=CARTESIAN_POINT('Origin',(55.4074307335706,-18.018989847295,39.92499));
#186364=CARTESIAN_POINT('Ctrl Pts',(59.5312589135995,-19.5431821162867,
39.92499));
#186365=CARTESIAN_POINT('Ctrl Pts',(59.5413499366334,-19.5464608884255,
39.9348354642019));
#186366=CARTESIAN_POINT('Ctrl Pts',(59.551669723849,-19.5489337165495,39.9446440828461));
#186367=CARTESIAN_POINT('Ctrl Pts',(59.5621592733664,-19.5505973858259,
39.9543641760335));
#186368=CARTESIAN_POINT('Ctrl Pts',(59.5723079749857,-19.5522069957573,
39.9637684240717));
#186369=CARTESIAN_POINT('Ctrl Pts',(59.582616868441,-19.5530593117978,39.9730909636402));
#186370=CARTESIAN_POINT('Ctrl Pts',(59.5930429125531,-19.5531064127989,
39.9822808977148));
#186371=CARTESIAN_POINT('Ctrl Pts',(59.6029053082843,-19.5531509674456,
39.9909740094658));
#186372=CARTESIAN_POINT('Ctrl Pts',(59.6128734577652,-19.5524750234008,
39.999549276501));
#186373=CARTESIAN_POINT('Ctrl Pts',(59.6229049605502,-19.5509963368653,
40.0079462328704));
#186374=CARTESIAN_POINT('Ctrl Pts',(59.6321447001119,-19.5496343596248,
40.01568043697));
#186375=CARTESIAN_POINT('Ctrl Pts',(59.6414387315194,-19.5475912199415,
40.0232638017433));
#186376=CARTESIAN_POINT('Ctrl Pts',(59.6507389334447,-19.5447674611705,
40.0306257269978));
#186377=CARTESIAN_POINT('Ctrl Pts',(59.6534365684955,-19.5439483960903,
40.032761141666));
#186378=CARTESIAN_POINT('Ctrl Pts',(59.6561345922133,-19.5430634173955,
40.0348777427275));
#186379=CARTESIAN_POINT('Ctrl Pts',(59.658831468516,-19.5421094990028,40.0369733168701));
#186380=CARTESIAN_POINT('Ctrl Pts',(59.6617550558218,-19.5410753901336,
40.039245053974));
#186381=CARTESIAN_POINT('Ctrl Pts',(59.6646735866702,-19.539962718579,40.041487875195));
#186382=CARTESIAN_POINT('Ctrl Pts',(59.6675844741795,-19.5387684320155,
40.0436985701601));
#186383=CARTESIAN_POINT('Ctrl Pts',(59.6755734277899,-19.5354907031706,
40.0497658398386));
#186384=CARTESIAN_POINT('Ctrl Pts',(59.683478254909,-19.5315625649725,40.0555581699984));
#186385=CARTESIAN_POINT('Ctrl Pts',(59.6911955084649,-19.5269766895183,
40.0609828468885));
#186386=CARTESIAN_POINT('Ctrl Pts',(59.6982563764893,-19.5227808624506,
40.0659461317306));
#186387=CARTESIAN_POINT('Ctrl Pts',(59.7051493183936,-19.5180305486456,
40.0706039980709));
#186388=CARTESIAN_POINT('Ctrl Pts',(59.7117949558642,-19.5126862934691,
40.0748843180607));
#186389=CARTESIAN_POINT('Ctrl Pts',(59.7150592712806,-19.5100612127845,
40.0769867972572));
#186390=CARTESIAN_POINT('Ctrl Pts',(59.7182634781249,-19.5072925729229,
40.0789976708176));
#186391=CARTESIAN_POINT('Ctrl Pts',(59.7213950854346,-19.5043743927939,
40.0809050491499));
#186392=CARTESIAN_POINT('Ctrl Pts',(59.7219892774193,-19.5038206965379,
40.0812669556104));
#186393=CARTESIAN_POINT('Ctrl Pts',(59.7225808838923,-19.5032610854116,
40.0816253922032));
#186394=CARTESIAN_POINT('Ctrl Pts',(59.7231697699856,-19.5026955970359,
40.0819801989139));
#186395=CARTESIAN_POINT('Ctrl Pts',(59.7237402533884,-19.5021477801719,
40.0823239179149));
#186396=CARTESIAN_POINT('Ctrl Pts',(59.7243081837714,-19.5015944476713,
40.0826642303498));
#186397=CARTESIAN_POINT('Ctrl Pts',(59.724873437353,-19.5010356373986,40.0830009916099));
#186398=CARTESIAN_POINT('Ctrl Pts',(59.7310334544115,-19.4949458381921,
40.0866709464311));
#186399=CARTESIAN_POINT('Ctrl Pts',(59.7368793392201,-19.4882011960854,
40.0899175831876));
#186400=CARTESIAN_POINT('Ctrl Pts',(59.7422363728286,-19.4808775251054,
40.092564206706));
#186401=CARTESIAN_POINT('Ctrl Pts',(59.7444986813872,-19.4777846933726,
40.0936818922526));
#186402=CARTESIAN_POINT('Ctrl Pts',(59.7466739523114,-19.474589008127,40.094693009479));
#186403=CARTESIAN_POINT('Ctrl Pts',(59.7487501225121,-19.4712977780155,
40.0955863397545));
#186404=CARTESIAN_POINT('Ctrl Pts',(59.7522463412521,-19.4657554287468,
40.0970906856166));
#186405=CARTESIAN_POINT('Ctrl Pts',(59.7554590576862,-19.4599426670171,
40.0982599215483));
#186406=CARTESIAN_POINT('Ctrl Pts',(59.758325802888,-19.4538995640362,40.0990497370453));
#186407=CARTESIAN_POINT('Ctrl Pts',(59.7590424891885,-19.4523887882909,
40.0992471909196));
#186408=CARTESIAN_POINT('Ctrl Pts',(59.7597373347835,-19.4508635299952,
40.0994209989363));
#186409=CARTESIAN_POINT('Ctrl Pts',(59.7604090725467,-19.4493243130378,
40.0995705982975));
#186410=CARTESIAN_POINT('Ctrl Pts',(59.7614166791915,-19.4470154876015,
40.0997949973393));
#186411=CARTESIAN_POINT('Ctrl Pts',(59.7623722755974,-19.4446752658773,
40.0999649129781));
#186412=CARTESIAN_POINT('Ctrl Pts',(59.7632731754137,-19.442305952026,40.1000786629733));
#186413=CARTESIAN_POINT('Ctrl Pts',(59.76417407523,-19.4399366381748,40.1001924129685));
#186414=CARTESIAN_POINT('Ctrl Pts',(59.7650202849791,-19.4375382417959,
40.10025));
#186415=CARTESIAN_POINT('Ctrl Pts',(59.7658094374951,-19.4351129318421,
40.10025));
#186416=CARTESIAN_POINT('Ctrl Pts',(56.1347810195642,-18.2553202812749,
40.10025));
#186417=CARTESIAN_POINT('Ctrl Pts',(56.1321105487811,-18.2635267101472,
40.10025));
#186418=CARTESIAN_POINT('Ctrl Pts',(56.1301406315643,-18.2718824441048,
40.0995786334241));
#186419=CARTESIAN_POINT('Ctrl Pts',(56.1288305556598,-18.2802419597937,
40.0983063763366));
#186420=CARTESIAN_POINT('Ctrl Pts',(56.1279843810471,-18.2856413491926,
40.0974846287992));
#186421=CARTESIAN_POINT('Ctrl Pts',(56.1274125556283,-18.2910421817933,
40.0964130309338));
#186422=CARTESIAN_POINT('Ctrl Pts',(56.1270952669252,-18.2964056883424,
40.0951176960924));
#186423=CARTESIAN_POINT('Ctrl Pts',(56.1266747189247,-18.3035147090328,
40.0934008039614));
#186424=CARTESIAN_POINT('Ctrl Pts',(56.1267070766081,-18.3105573165141,
40.0912909372156));
#186425=CARTESIAN_POINT('Ctrl Pts',(56.1271555587355,-18.3174512966899,
40.0888630467851));
#186426=CARTESIAN_POINT('Ctrl Pts',(56.1273797997992,-18.3208982867778,
40.0876491015699));
#186427=CARTESIAN_POINT('Ctrl Pts',(56.127708008729,-18.3243083090328,40.0863558569271));
#186428=CARTESIAN_POINT('Ctrl Pts',(56.128135143741,-18.3276724292419,40.0849936342771));
#186429=CARTESIAN_POINT('Ctrl Pts',(56.128348711247,-18.3293544893464,40.0843125229521));
#186430=CARTESIAN_POINT('Ctrl Pts',(56.1285870051495,-18.3310250895513,
40.0836141747074));
#186431=CARTESIAN_POINT('Ctrl Pts',(56.1288493629352,-18.332683211057,40.0828999161609));
#186432=CARTESIAN_POINT('Ctrl Pts',(56.1289149523817,-18.3330977414334,
40.0827213515243));
#186433=CARTESIAN_POINT('Ctrl Pts',(56.1289820457108,-18.3335114922229,
40.0825417925842));
#186434=CARTESIAN_POINT('Ctrl Pts',(56.1290506323488,-18.3339244481756,
40.082361260236));
#186435=CARTESIAN_POINT('Ctrl Pts',(56.1292563922628,-18.3351633160336,
40.0818196631917));
#186436=CARTESIAN_POINT('Ctrl Pts',(56.1294755925119,-18.336395028707,40.0812693052021));
#186437=CARTESIAN_POINT('Ctrl Pts',(56.1297079426452,-18.3376191892285,
40.0807107531874));
#186438=CARTESIAN_POINT('Ctrl Pts',(56.1313445869829,-18.3462420178743,
40.0767763849181));
#186439=CARTESIAN_POINT('Ctrl Pts',(56.1335959402409,-18.3545284904606,
40.0724140586136));
#186440=CARTESIAN_POINT('Ctrl Pts',(56.1363459252322,-18.3624495731175,
40.0677221223766));
#186441=CARTESIAN_POINT('Ctrl Pts',(56.1376796649813,-18.3662912896464,
40.0654465383719));
#186442=CARTESIAN_POINT('Ctrl Pts',(56.1391312300712,-18.3700472768051,
40.0630928000678));
#186443=CARTESIAN_POINT('Ctrl Pts',(56.1406901365234,-18.3737149835763,
40.0606689262479));
#186444=CARTESIAN_POINT('Ctrl Pts',(56.1430767133842,-18.3793299863879,
40.0569581447805));
#186445=CARTESIAN_POINT('Ctrl Pts',(56.1457125629779,-18.3847354115622,
40.0530843804605));
#186446=CARTESIAN_POINT('Ctrl Pts',(56.1485569297209,-18.3899096889379,
40.0490800251457));
#186447=CARTESIAN_POINT('Ctrl Pts',(56.1498778683512,-18.3923126501193,
40.0472203818218));
#186448=CARTESIAN_POINT('Ctrl Pts',(56.1512435269776,-18.3946658026159,
40.0453323608818));
#186449=CARTESIAN_POINT('Ctrl Pts',(56.152650749137,-18.3969661720538,40.0434201572162));
#186450=CARTESIAN_POINT('Ctrl Pts',(56.1527586071708,-18.3971424863073,
40.0432735943397));
#186451=CARTESIAN_POINT('Ctrl Pts',(56.1528666894395,-18.3973185179286,
40.0431268995707));
#186452=CARTESIAN_POINT('Ctrl Pts',(56.1529749944979,-18.397494266707,40.0429800745037));
#186453=CARTESIAN_POINT('Ctrl Pts',(56.1544963540395,-18.399963007178,40.0409176249753));
#186454=CARTESIAN_POINT('Ctrl Pts',(56.1560635207938,-18.4023749585853,
40.0388310783332));
#186455=CARTESIAN_POINT('Ctrl Pts',(56.1576709325004,-18.4047288488035,
40.036725739981));
#186456=CARTESIAN_POINT('Ctrl Pts',(56.1634348250117,-18.4131694805007,
40.0291763710717));
#186457=CARTESIAN_POINT('Ctrl Pts',(56.1697591292905,-18.4209299141239,
40.0213310894594));
#186458=CARTESIAN_POINT('Ctrl Pts',(56.1765231650107,-18.4280560759386,
40.0132837551319));
#186459=CARTESIAN_POINT('Ctrl Pts',(56.1839561607595,-18.4358870118863,
40.0044405431325));
#186460=CARTESIAN_POINT('Ctrl Pts',(56.1919204977438,-18.4429525945098,
39.9953528710602));
#186461=CARTESIAN_POINT('Ctrl Pts',(56.2003032932669,-18.4492898603069,
39.9861103629557));
#186462=CARTESIAN_POINT('Ctrl Pts',(56.209354608637,-18.456132516931,39.9761307737561));
#186463=CARTESIAN_POINT('Ctrl Pts',(56.218894606845,-18.4621268842287,39.9659696936019));
#186464=CARTESIAN_POINT('Ctrl Pts',(56.2288243369859,-18.4672816799262,
39.9557128217517));
#186465=CARTESIAN_POINT('Ctrl Pts',(56.2386707668943,-18.4723932321846,
39.9455419945168));
#186466=CARTESIAN_POINT('Ctrl Pts',(56.2489017962821,-18.4766796388,39.9352756289344));
#186467=CARTESIAN_POINT('Ctrl Pts',(56.2594439784239,-18.4801050014191,
39.92499));
#186468=CARTESIAN_POINT('Origin',(0.00470941899427448,0.0144941013083399,
39.92499));
#186469=CARTESIAN_POINT('Ctrl Pts',(59.7752282754837,-19.4061247292254,
40.10025));
#186470=CARTESIAN_POINT('Ctrl Pts',(59.7778789856303,-19.3979550581542,
40.10025));
#186471=CARTESIAN_POINT('Ctrl Pts',(59.7798236858211,-19.3896365599065,
40.0995859581841));
#186472=CARTESIAN_POINT('Ctrl Pts',(59.781106115828,-19.3813136269513,40.098327595962));
#186473=CARTESIAN_POINT('Ctrl Pts',(59.7819255275519,-19.3759956690085,
40.0975235624068));
#186474=CARTESIAN_POINT('Ctrl Pts',(59.7824754874621,-19.3706760212377,
40.096477705949));
#186475=CARTESIAN_POINT('Ctrl Pts',(59.7827759879495,-19.365391880154,40.0952149915961));
#186476=CARTESIAN_POINT('Ctrl Pts',(59.783186110819,-19.3581800878463,40.0934916398701));
#186477=CARTESIAN_POINT('Ctrl Pts',(59.7831255716887,-19.351035454862,40.0913643921631));
#186478=CARTESIAN_POINT('Ctrl Pts',(59.7826350657124,-19.3440445557096,
40.0889118607713));
#186479=CARTESIAN_POINT('Ctrl Pts',(59.7823898127243,-19.3405491061334,
40.0876855950754));
#186480=CARTESIAN_POINT('Ctrl Pts',(59.7820371343799,-19.3370918919974,
40.0863782327527));
#186481=CARTESIAN_POINT('Ctrl Pts',(59.7815825865439,-19.3336823180309,
40.0850006373334));
#186482=CARTESIAN_POINT('Ctrl Pts',(59.7813553126259,-19.3319775310477,
40.0843118396238));
#186483=CARTESIAN_POINT('Ctrl Pts',(59.7811025767643,-19.330284637561,40.0836054919165));
#186484=CARTESIAN_POINT('Ctrl Pts',(59.7808251076837,-19.3286047092264,
40.0828829920418));
#186485=CARTESIAN_POINT('Ctrl Pts',(59.7807557404135,-19.3281847271428,
40.0827023670731));
#186486=CARTESIAN_POINT('Ctrl Pts',(59.7806848274338,-19.327765555029,40.0825207326933));
#186487=CARTESIAN_POINT('Ctrl Pts',(59.7806123803667,-19.3273472089195,
40.0823381109276));
#186488=CARTESIAN_POINT('Ctrl Pts',(59.7803950391653,-19.3260921705912,
40.0817902456304));
#186489=CARTESIAN_POINT('Ctrl Pts',(59.7801638905868,-19.3248445680577,
40.0812334935553));
#186490=CARTESIAN_POINT('Ctrl Pts',(59.7799192536869,-19.3236048185586,
40.0806684524227));
#186491=CARTESIAN_POINT('Ctrl Pts',(59.7782286609226,-19.3150373803107,
40.0767636676136));
#186492=CARTESIAN_POINT('Ctrl Pts',(59.7759321681721,-19.3068044648769,
40.0724404510887));
#186493=CARTESIAN_POINT('Ctrl Pts',(59.7731456380808,-19.29893228444,40.0677949937407));
#186494=CARTESIAN_POINT('Ctrl Pts',(59.7717607402744,-19.2950198323717,
40.0654862141904));
#186495=CARTESIAN_POINT('Ctrl Pts',(59.7702542302928,-19.291196264669,40.0630972003215));
#186496=CARTESIAN_POINT('Ctrl Pts',(59.7686372707431,-19.2874640247234,
40.0606363359906));
#186497=CARTESIAN_POINT('Ctrl Pts',(59.7650700164611,-19.2792301459417,
40.0552073017123));
#186498=CARTESIAN_POINT('Ctrl Pts',(59.7609769706902,-19.2714367138414,
40.0494204304519));
#186499=CARTESIAN_POINT('Ctrl Pts',(59.7564706723513,-19.2641757185812,
40.0434049749851));
#186500=CARTESIAN_POINT('Ctrl Pts',(59.7548244647406,-19.2615231854467,
40.0412074532442));
#186501=CARTESIAN_POINT('Ctrl Pts',(59.7531276155319,-19.2589351484755,
40.0389814735788));
#186502=CARTESIAN_POINT('Ctrl Pts',(59.7513854342766,-19.2564118357496,
40.0367321210016));
#186503=CARTESIAN_POINT('Ctrl Pts',(59.7455336317916,-19.2479362953112,
40.0291767837137));
#186504=CARTESIAN_POINT('Ctrl Pts',(59.7391263493539,-19.2401420439511,
40.0213235332568));
#186505=CARTESIAN_POINT('Ctrl Pts',(59.7322837268611,-19.2329840462261,
40.0132649215847));
#186506=CARTESIAN_POINT('Ctrl Pts',(59.7247628741796,-19.2251165588058,
40.0044075527517));
#186507=CARTESIAN_POINT('Ctrl Pts',(59.7167157560769,-19.2180171087279,
39.9953016253699));
#186508=CARTESIAN_POINT('Ctrl Pts',(59.7082546997619,-19.2116502033051,
39.9860353422333));
#186509=CARTESIAN_POINT('Ctrl Pts',(59.6991417795831,-19.2047927733646,
39.9760551582665));
#186510=CARTESIAN_POINT('Ctrl Pts',(59.6895478206977,-19.1987842816745,
39.9658879738121));
#186511=CARTESIAN_POINT('Ctrl Pts',(59.6795708631988,-19.1936187207947,
39.9556174643214));
#186512=CARTESIAN_POINT('Ctrl Pts',(59.6697286283139,-19.1885229124285,
39.9454856413877));
#186513=CARTESIAN_POINT('Ctrl Pts',(59.6595122814314,-19.1842470541687,
39.93525194651));
#186514=CARTESIAN_POINT('Ctrl Pts',(59.6489943884564,-19.1808295835782,
39.92499));
#186515=CARTESIAN_POINT('Ctrl Pts',(56.3771794532807,-18.1177524687107,
39.92499));
#186516=CARTESIAN_POINT('Ctrl Pts',(56.3671137719651,-18.1144819305952,
39.934810724172));
#186517=CARTESIAN_POINT('Ctrl Pts',(56.3568263239579,-18.1120170699781,
39.9446038383165));
#186518=CARTESIAN_POINT('Ctrl Pts',(56.3463749453368,-18.1103629196652,
39.9543158069377));
#186519=CARTESIAN_POINT('Ctrl Pts',(56.3362832197254,-18.1087656919994,
39.9636935671382));
#186520=CARTESIAN_POINT('Ctrl Pts',(56.3260373921244,-18.1079242184406,
39.9729968320977));
#186521=CARTESIAN_POINT('Ctrl Pts',(56.3156801719865,-18.1078879163649,
39.9821731151321));
#186522=CARTESIAN_POINT('Ctrl Pts',(56.3058893552755,-18.1078535995342,
39.9908475764337));
#186523=CARTESIAN_POINT('Ctrl Pts',(56.2959980926961,-18.1085387949861,
39.9994093733829));
#186524=CARTESIAN_POINT('Ctrl Pts',(56.2860490151176,-18.1100266905422,
40.0077966115823));
#186525=CARTESIAN_POINT('Ctrl Pts',(56.276886081576,-18.1113970173881,40.0155211172575));
#186526=CARTESIAN_POINT('Ctrl Pts',(56.2676735798242,-18.1134483398637,
40.0230979941));
#186527=CARTESIAN_POINT('Ctrl Pts',(56.2584600414709,-18.1162805994765,
40.0304554104726));
#186528=CARTESIAN_POINT('Ctrl Pts',(56.2557127503202,-18.1171251221205,
40.0326492435166));
#186529=CARTESIAN_POINT('Ctrl Pts',(56.2529655048694,-18.1180393245068,
40.0348233715053));
#186530=CARTESIAN_POINT('Ctrl Pts',(56.2502199893831,-18.119026506434,40.0369753512355));
#186531=CARTESIAN_POINT('Ctrl Pts',(56.2475025263006,-18.1200036017942,
40.0391053430352));
#186532=CARTESIAN_POINT('Ctrl Pts',(56.244789485083,-18.1210509212416,40.041211089324));
#186533=CARTESIAN_POINT('Ctrl Pts',(56.242085504679,-18.1221702476364,40.0432881154904));
#186534=CARTESIAN_POINT('Ctrl Pts',(56.2418974751699,-18.1222480834049,
40.0434325478279));
#186535=CARTESIAN_POINT('Ctrl Pts',(56.2417094803631,-18.1223262596099,
40.0435768364421));
#186536=CARTESIAN_POINT('Ctrl Pts',(56.2415215209613,-18.1224047773504,
40.0437209807855));
#186537=CARTESIAN_POINT('Ctrl Pts',(56.2332806922381,-18.1258472827275,
40.050040796842));
#186538=CARTESIAN_POINT('Ctrl Pts',(56.2251347899176,-18.1299826829656,
40.0560490279345));
#186539=CARTESIAN_POINT('Ctrl Pts',(56.2171955585583,-18.1348427679841,
40.0616647108616));
#186540=CARTESIAN_POINT('Ctrl Pts',(56.2097948151022,-18.1393732118985,
40.0668995033488));
#186541=CARTESIAN_POINT('Ctrl Pts',(56.2025731376006,-18.1445340001513,
40.0717933267485));
#186542=CARTESIAN_POINT('Ctrl Pts',(56.1956479299622,-18.1503626543107,
40.0762460303077));
#186543=CARTESIAN_POINT('Ctrl Pts',(56.1931145994154,-18.1524948514086,
40.0778748868751));
#186544=CARTESIAN_POINT('Ctrl Pts',(56.190621252949,-18.1547164978842,40.0794443522248));
#186545=CARTESIAN_POINT('Ctrl Pts',(56.1881748397225,-18.1570296338737,
40.0809482021491));
#186546=CARTESIAN_POINT('Ctrl Pts',(56.1875865590689,-18.1575858658042,
40.0813098278168));
#186547=CARTESIAN_POINT('Ctrl Pts',(56.1870008763867,-18.1581479603547,
40.0816679525671));
#186548=CARTESIAN_POINT('Ctrl Pts',(56.1864179215672,-18.1587158783113,
40.082022419258));
#186549=CARTESIAN_POINT('Ctrl Pts',(56.1858531840858,-18.1592660488318,
40.0823658088647));
#186550=CARTESIAN_POINT('Ctrl Pts',(56.1852910066466,-18.1598216844585,
40.0827057654616));
#186551=CARTESIAN_POINT('Ctrl Pts',(56.1847315084904,-18.1603827459285,
40.083042147015));
#186552=CARTESIAN_POINT('Ctrl Pts',(56.1786015595925,-18.1665298227358,
40.0867275956805));
#186553=CARTESIAN_POINT('Ctrl Pts',(56.1727894828609,-18.1733325302111,
40.089982343203));
#186554=CARTESIAN_POINT('Ctrl Pts',(56.1674665972292,-18.1807122308848,
40.0926299529355));
#186555=CARTESIAN_POINT('Ctrl Pts',(56.1652590378994,-18.1837728127196,
40.0937279956083));
#186556=CARTESIAN_POINT('Ctrl Pts',(56.1631354730308,-18.1869322368372,
40.0947220371802));
#186557=CARTESIAN_POINT('Ctrl Pts',(56.1611070880438,-18.1901833857453,
40.0956014538692));
#186558=CARTESIAN_POINT('Ctrl Pts',(56.1576474660761,-18.1957285590017,
40.097101390674));
#186559=CARTESIAN_POINT('Ctrl Pts',(56.1544671656478,-18.2015400422203,
40.0982667904316));
#186560=CARTESIAN_POINT('Ctrl Pts',(56.1516266854597,-18.2075773774753,
40.0990539325582));
#186561=CARTESIAN_POINT('Ctrl Pts',(56.1502064453657,-18.2105960451028,
40.0994475036216));
#186562=CARTESIAN_POINT('Ctrl Pts',(56.1488725139556,-18.2136716866511,
40.0997467259952));
#186563=CARTESIAN_POINT('Ctrl Pts',(56.1476325143037,-18.2167992197297,
40.0999473488896));
#186564=CARTESIAN_POINT('Ctrl Pts',(56.1463925146518,-18.2199267528083,
40.100147971784));
#186565=CARTESIAN_POINT('Ctrl Pts',(56.1452464433752,-18.223106131882,40.10025));
#186566=CARTESIAN_POINT('Ctrl Pts',(56.1441998575527,-18.2263320786583,
40.10025));
#186567=CARTESIAN_POINT('Origin',(53.2204057122638,-23.7119335237426,39.92499));
#186568=CARTESIAN_POINT('Ctrl Pts',(57.1623216544371,-25.6588335304441,
39.92499));
#186569=CARTESIAN_POINT('Ctrl Pts',(57.172014672778,-25.6631491402567,39.9348354642022));
#186570=CARTESIAN_POINT('Ctrl Pts',(57.182019446196,-25.6666871334685,39.9446440828466));
#186571=CARTESIAN_POINT('Ctrl Pts',(57.192277632071,-25.669438145482,39.9543641760343));
#186572=CARTESIAN_POINT('Ctrl Pts',(57.2022024879886,-25.6720997659862,
39.9637684240727));
#186573=CARTESIAN_POINT('Ctrl Pts',(57.2123658169611,-25.6740249857411,
39.9730909636413));
#186574=CARTESIAN_POINT('Ctrl Pts',(57.2227298227177,-25.6751616470869,
39.982280897716));
#186575=CARTESIAN_POINT('Ctrl Pts',(57.2325335339847,-25.6762368587286,
39.9909740094672));
#186576=CARTESIAN_POINT('Ctrl Pts',(57.2425177322922,-25.6766065729228,
39.9995492765025));
#186577=CARTESIAN_POINT('Ctrl Pts',(57.2526488462867,-25.6761845643571,
40.0079462328721));
#186578=CARTESIAN_POINT('Ctrl Pts',(57.2619803349765,-25.6757958639477,
40.0156804369718));
#186579=CARTESIAN_POINT('Ctrl Pts',(57.2714370189591,-25.6747354076178,
40.0232638017452));
#186580=CARTESIAN_POINT('Ctrl Pts',(57.2809814365703,-25.6728992535079,
40.0306257269999));
#186581=CARTESIAN_POINT('Ctrl Pts',(57.2837499093073,-25.6723666549984,
40.0327611416673));
#186582=CARTESIAN_POINT('Ctrl Pts',(57.2865256584311,-25.6717685445827,
40.0348777427281));
#186583=CARTESIAN_POINT('Ctrl Pts',(57.289307472586,-25.6711017521905,40.0369733168701));
#186584=CARTESIAN_POINT('Ctrl Pts',(57.2923231379855,-25.6703789063662,
40.039245053974));
#186585=CARTESIAN_POINT('Ctrl Pts',(57.2953419866643,-25.6695773996874,
40.041487875195));
#186586=CARTESIAN_POINT('Ctrl Pts',(57.2983617649664,-25.6686939261487,
40.0436985701601));
#186587=CARTESIAN_POINT('Ctrl Pts',(57.3066495702123,-25.6662692260894,
40.0497658398386));
#186588=CARTESIAN_POINT('Ctrl Pts',(57.3149216961106,-25.6631888860745,
40.0555581699984));
#186589=CARTESIAN_POINT('Ctrl Pts',(57.323076028258,-25.6594348051807,40.0609828468885));
#186590=CARTESIAN_POINT('Ctrl Pts',(57.3305367994639,-25.6560000249767,
40.0659461317305));
#186591=CARTESIAN_POINT('Ctrl Pts',(57.3378885241132,-25.6519962425126,
40.0706039980707));
#186592=CARTESIAN_POINT('Ctrl Pts',(57.3450563828671,-25.6473759219975,
40.0748843180604));
#186593=CARTESIAN_POINT('Ctrl Pts',(57.3485772116722,-25.6451064356535,
40.076986797257));
#186594=CARTESIAN_POINT('Ctrl Pts',(57.3520532672064,-25.6426878935081,
40.0789976708175));
#186595=CARTESIAN_POINT('Ctrl Pts',(57.3554727521281,-25.6401130415747,
40.08090504915));
#186596=CARTESIAN_POINT('Ctrl Pts',(57.3561215660858,-25.6396244884997,
40.0812669556105));
#186597=CARTESIAN_POINT('Ctrl Pts',(57.3567684269677,-25.6391297826973,
40.0816253922032));
#186598=CARTESIAN_POINT('Ctrl Pts',(57.3574131967122,-25.6386289474844,
40.0819801989139));
#186599=CARTESIAN_POINT('Ctrl Pts',(57.3580378174021,-25.6381437633719,
40.0823239179149));
#186600=CARTESIAN_POINT('Ctrl Pts',(57.3586604755991,-25.6376528269749,
40.0826642303498));
#186601=CARTESIAN_POINT('Ctrl Pts',(57.3592810442415,-25.6371561630115,
40.0830009916099));
#186602=CARTESIAN_POINT('Ctrl Pts',(57.3660438734345,-25.6317436214793,
40.086670946431));
#186603=CARTESIAN_POINT('Ctrl Pts',(57.3725627409489,-25.6256469885834,
40.0899175831874));
#186604=CARTESIAN_POINT('Ctrl Pts',(57.3786559602396,-25.6189233999304,
40.0925642067058));
#186605=CARTESIAN_POINT('Ctrl Pts',(57.3812291645836,-25.6160839866903,
40.0936818922525));
#186606=CARTESIAN_POINT('Ctrl Pts',(57.3837265592141,-25.6131331854695,
40.0946930094789));
#186607=CARTESIAN_POINT('Ctrl Pts',(57.3861353831632,-25.6100770039412,
40.0955863397546));
#186608=CARTESIAN_POINT('Ctrl Pts',(57.390191782503,-25.6049304706139,40.0970906856166));
#186609=CARTESIAN_POINT('Ctrl Pts',(57.3939944983914,-25.5994853721129,
40.0982599215483));
#186610=CARTESIAN_POINT('Ctrl Pts',(57.3974772155311,-25.593775030353,40.0990497370453));
#186611=CARTESIAN_POINT('Ctrl Pts',(57.398347894816,-25.592347444913,40.0992471909196));
#186612=CARTESIAN_POINT('Ctrl Pts',(57.3991983668799,-25.5909031732841,
40.0994209989363));
#186613=CARTESIAN_POINT('Ctrl Pts',(57.4000273167765,-25.5894426040343,
40.0995705982975));
#186614=CARTESIAN_POINT('Ctrl Pts',(57.4012707416215,-25.5872517501595,
40.0997949973393));
#186615=CARTESIAN_POINT('Ctrl Pts',(57.4024657229508,-25.5850242354385,
40.0999649129781));
#186616=CARTESIAN_POINT('Ctrl Pts',(57.4036093482795,-25.5827620706098,
40.1000786629733));
#186617=CARTESIAN_POINT('Ctrl Pts',(57.4047529736082,-25.5804999057811,
40.1001924129685));
#186618=CARTESIAN_POINT('Ctrl Pts',(57.4058452484196,-25.5782031010731,
40.10025));
#186619=CARTESIAN_POINT('Ctrl Pts',(57.4068835917979,-25.5758735661209,
40.10025));
#186620=CARTESIAN_POINT('Ctrl Pts',(53.9190682401995,-24.0229981225297,
40.10025));
#186621=CARTESIAN_POINT('Ctrl Pts',(53.9155545931359,-24.0308804555185,
40.10025));
#186622=CARTESIAN_POINT('Ctrl Pts',(53.9127220553017,-24.0389845034715,
40.0995786334241));
#186623=CARTESIAN_POINT('Ctrl Pts',(53.9105453488015,-24.0471612846374,
40.0983063763367));
#186624=CARTESIAN_POINT('Ctrl Pts',(53.9091394197453,-24.0524426462847,
40.0974846287993));
#186625=CARTESIAN_POINT('Ctrl Pts',(53.9080061861138,-24.0577541205273,
40.0964130309338));
#186626=CARTESIAN_POINT('Ctrl Pts',(53.9071299964541,-24.0630550795261,
40.0951176960923));
#186627=CARTESIAN_POINT('Ctrl Pts',(53.9059686572515,-24.0700811970212,
40.0934008039614));
#186628=CARTESIAN_POINT('Ctrl Pts',(53.9052646847386,-24.0770886066606,
40.0912909372156));
#186629=CARTESIAN_POINT('Ctrl Pts',(53.9049900928805,-24.0839917000392,
40.0888630467851));
#186630=CARTESIAN_POINT('Ctrl Pts',(53.9048527969514,-24.0874432467286,
40.0876491015698));
#186631=CARTESIAN_POINT('Ctrl Pts',(53.9048227635323,-24.0908688956999,
40.0863558569271));
#186632=CARTESIAN_POINT('Ctrl Pts',(53.9048959123383,-24.0942592346729,
40.0849936342771));
#186633=CARTESIAN_POINT('Ctrl Pts',(53.9049324867413,-24.0959544041594,
40.0843125229521));
#186634=CARTESIAN_POINT('Ctrl Pts',(53.9049948499728,-24.097640761137,40.0836141747074));
#186635=CARTESIAN_POINT('Ctrl Pts',(53.9050824496422,-24.0993172231358,
40.0828999161609));
#186636=CARTESIAN_POINT('Ctrl Pts',(53.9051043495595,-24.0997363386355,
40.0827213515243));
#186637=CARTESIAN_POINT('Ctrl Pts',(53.9051278266102,-24.1001548360174,
40.0825417925841));
#186638=CARTESIAN_POINT('Ctrl Pts',(53.9051528718723,-24.10057269901,40.082361260236));
#186639=CARTESIAN_POINT('Ctrl Pts',(53.9052280076585,-24.1018262879879,
40.0818196631917));
#186640=CARTESIAN_POINT('Ctrl Pts',(53.9053172580728,-24.1030741658756,
40.0812693052021));
#186641=CARTESIAN_POINT('Ctrl Pts',(53.9054203757497,-24.10431590752,40.0807107531874));
#186642=CARTESIAN_POINT('Ctrl Pts',(53.9061467233511,-24.1130625753258,
40.0767763849181));
#186643=CARTESIAN_POINT('Ctrl Pts',(53.907519571215,-24.1215389842446,40.0724140586136));
#186644=CARTESIAN_POINT('Ctrl Pts',(53.9094265129032,-24.1297041260871,
40.0677221223766));
#186645=CARTESIAN_POINT('Ctrl Pts',(53.9103513775613,-24.1336642110573,
40.0654465383719));
#186646=CARTESIAN_POINT('Ctrl Pts',(53.91140238326,-24.1375513523935,40.0630928000678));
#186647=CARTESIAN_POINT('Ctrl Pts',(53.9125693701071,-24.1413619171791,
40.0606689262478));
#186648=CARTESIAN_POINT('Ctrl Pts',(53.914355945435,-24.1471956256295,40.0569581447805));
#186649=CARTESIAN_POINT('Ctrl Pts',(53.916412334782,-24.1528469606265,40.0530843804605));
#186650=CARTESIAN_POINT('Ctrl Pts',(53.9187002605239,-24.158290210054,40.0490800251457));
#186651=CARTESIAN_POINT('Ctrl Pts',(53.9197627850745,-24.1608180832477,
40.0472203818218));
#186652=CARTESIAN_POINT('Ctrl Pts',(53.9208749910658,-24.1633010951263,
40.0453323608818));
#186653=CARTESIAN_POINT('Ctrl Pts',(53.9220340502327,-24.1657359576695,
40.0434201572162));
#186654=CARTESIAN_POINT('Ctrl Pts',(53.9221228875509,-24.1659225802895,
40.0432735943397));
#186655=CARTESIAN_POINT('Ctrl Pts',(53.9222119774187,-24.1661089452647,
40.0431268995707));
#186656=CARTESIAN_POINT('Ctrl Pts',(53.922301318421,-24.1662950522343,40.0429800745037));
#186657=CARTESIAN_POINT('Ctrl Pts',(53.9235562901482,-24.1689092940616,
40.0409176249753));
#186658=CARTESIAN_POINT('Ctrl Pts',(53.9248627542249,-24.1714718460792,
40.0388310783332));
#186659=CARTESIAN_POINT('Ctrl Pts',(53.9262153118348,-24.173980861716,40.036725739981));
#186660=CARTESIAN_POINT('Ctrl Pts',(53.9310653428793,-24.1829777455759,
40.029176371072));
#186661=CARTESIAN_POINT('Ctrl Pts',(53.9365438157564,-24.191356736539,40.02133108946));
#186662=CARTESIAN_POINT('Ctrl Pts',(53.9425259106375,-24.1991508947526,
40.0132837551329));
#186663=CARTESIAN_POINT('Ctrl Pts',(53.9490996319571,-24.2077158916369,
40.0044405431337));
#186664=CARTESIAN_POINT('Ctrl Pts',(53.9562817849761,-24.2155752681652,
39.9953528710616));
#186665=CARTESIAN_POINT('Ctrl Pts',(53.9639562340128,-24.222754058491,39.9861103629574));
#186666=CARTESIAN_POINT('Ctrl Pts',(53.9722427129487,-24.2305053504125,
39.9761307737578));
#186667=CARTESIAN_POINT('Ctrl Pts',(53.9811038680463,-24.2374640812912,
39.9659696936037));
#186668=CARTESIAN_POINT('Ctrl Pts',(53.9904403792137,-24.2436285779109,
39.9557128217535));
#186669=CARTESIAN_POINT('Ctrl Pts',(53.9996985666468,-24.2497413607387,
39.945541994518));
#186670=CARTESIAN_POINT('Ctrl Pts',(54.0094254978893,-24.25507371975,39.935275628935));
#186671=CARTESIAN_POINT('Ctrl Pts',(54.0195518809641,-24.2595822759734,
39.92499));
#186672=CARTESIAN_POINT('Origin',(0.00619866644047569,0.0139224327744755,
39.92499));
#186673=CARTESIAN_POINT('Ctrl Pts',(57.4192809246789,-25.5480287005719,
40.10025));
#186674=CARTESIAN_POINT('Ctrl Pts',(57.4227710771202,-25.5401808584722,
40.10025));
#186675=CARTESIAN_POINT('Ctrl Pts',(57.4255746438784,-25.5321112063511,
40.0995859581842));
#186676=CARTESIAN_POINT('Ctrl Pts',(57.4277200319911,-25.5239679177318,
40.0983275959622));
#186677=CARTESIAN_POINT('Ctrl Pts',(57.4290908328636,-25.5187647439669,
40.0975235624069));
#186678=CARTESIAN_POINT('Ctrl Pts',(57.4301938346425,-25.5135317242469,
40.0964777059491));
#186679=CARTESIAN_POINT('Ctrl Pts',(57.4310450321041,-25.5083079410947,
40.0952149915961));
#186680=CARTESIAN_POINT('Ctrl Pts',(57.4322067458449,-25.5011785252532,
40.0934916398701));
#186681=CARTESIAN_POINT('Ctrl Pts',(57.4328933558607,-25.4940667032537,
40.0913643921631));
#186682=CARTESIAN_POINT('Ctrl Pts',(57.4331362848728,-25.4870628291424,
40.0889118607713));
#186683=CARTESIAN_POINT('Ctrl Pts',(57.4332577493788,-25.4835608920868,
40.0876855950755));
#186684=CARTESIAN_POINT('Ctrl Pts',(57.4332683803241,-25.4800857520062,
40.0863782327527));
#186685=CARTESIAN_POINT('Ctrl Pts',(57.4331727200758,-25.4766473428559,
40.0850006373334));
#186686=CARTESIAN_POINT('Ctrl Pts',(57.4331248899517,-25.4749281382807,
40.0843118396238));
#186687=CARTESIAN_POINT('Ctrl Pts',(57.4330504941582,-25.4732181005505,
40.0836054919165));
#186688=CARTESIAN_POINT('Ctrl Pts',(57.4329501454094,-25.4715183716225,
40.0828829920418));
#186689=CARTESIAN_POINT('Ctrl Pts',(57.4329250582223,-25.4710934393905,
40.0827023670731));
#186690=CARTESIAN_POINT('Ctrl Pts',(57.4328983491282,-25.4706691511206,
40.0825207326933));
#186691=CARTESIAN_POINT('Ctrl Pts',(57.4328700280096,-25.4702455239743,
40.0823381109276));
#186692=CARTESIAN_POINT('Ctrl Pts',(57.4327850646539,-25.4689746425355,
40.0817902456304));
#186693=CARTESIAN_POINT('Ctrl Pts',(57.4326855923071,-25.4677097128935,
40.0812334935553));
#186694=CARTESIAN_POINT('Ctrl Pts',(57.4325718846637,-25.4664511833527,
40.0806684524227));
#186695=CARTESIAN_POINT('Ctrl Pts',(57.4317860942977,-25.4577539633646,
40.0767636676138));
#186696=CARTESIAN_POINT('Ctrl Pts',(57.4303627559733,-25.4493260998452,
40.0724404510891));
#186697=CARTESIAN_POINT('Ctrl Pts',(57.4284143577092,-25.4412057723284,
40.0677949937413));
#186698=CARTESIAN_POINT('Ctrl Pts',(57.4274460091201,-25.4371699918422,
40.0654862141908));
#186699=CARTESIAN_POINT('Ctrl Pts',(57.4263474236139,-25.4332098968697,
40.0630972003217));
#186700=CARTESIAN_POINT('Ctrl Pts',(57.4251294472437,-25.4293290842279,
40.0606363359906));
#186701=CARTESIAN_POINT('Ctrl Pts',(57.4224424094497,-25.4207674318875,
40.0552073017123));
#186702=CARTESIAN_POINT('Ctrl Pts',(57.4191864212928,-25.4125888532391,
40.0494204304519));
#186703=CARTESIAN_POINT('Ctrl Pts',(57.4154637896041,-25.4048965980304,
40.0434049749851));
#186704=CARTESIAN_POINT('Ctrl Pts',(57.4141038653033,-25.4020865201982,
40.0412074532442));
#186705=CARTESIAN_POINT('Ctrl Pts',(57.4126868351396,-25.3993352917241,
40.0389814735788));
#186706=CARTESIAN_POINT('Ctrl Pts',(57.4112179557371,-25.3966436944399,
40.0367321210016));
#186707=CARTESIAN_POINT('Ctrl Pts',(57.4062841452561,-25.3876029039781,
40.029176783714));
#186708=CARTESIAN_POINT('Ctrl Pts',(57.4007266836992,-25.3791816069558,
40.0213235332574));
#186709=CARTESIAN_POINT('Ctrl Pts',(57.3946697603108,-25.3713475726777,
40.0132649215856));
#186710=CARTESIAN_POINT('Ctrl Pts',(57.3880124840173,-25.3627370410036,
40.0044075527529));
#186711=CARTESIAN_POINT('Ctrl Pts',(57.3807515434765,-25.3548353295672,
39.9953016253715));
#186712=CARTESIAN_POINT('Ctrl Pts',(57.373002360553,-25.3476188815044,39.9860353422352));
#186713=CARTESIAN_POINT('Ctrl Pts',(57.3646561585183,-25.3398464577404,
39.9760551582687));
#186714=CARTESIAN_POINT('Ctrl Pts',(57.3557428147466,-25.3328680394176,
39.9658879738145));
#186715=CARTESIAN_POINT('Ctrl Pts',(57.3463604602058,-25.3266878999853,
39.955617464324));
#186716=CARTESIAN_POINT('Ctrl Pts',(57.3371047991303,-25.3205912133023,
39.9454856413896));
#186717=CARTESIAN_POINT('Ctrl Pts',(57.3273913673573,-25.3152708796011,
39.9352519465109));
#186718=CARTESIAN_POINT('Ctrl Pts',(57.317288315449,-25.3107727110823,39.92499));
#186719=CARTESIAN_POINT('Ctrl Pts',(54.1745185419759,-23.9115214566115,
39.92499));
#186720=CARTESIAN_POINT('Ctrl Pts',(54.1648498658388,-23.9072166846463,
39.9348107241722));
#186721=CARTESIAN_POINT('Ctrl Pts',(54.1548764216404,-23.9036899956623,
39.9446038383169));
#186722=CARTESIAN_POINT('Ctrl Pts',(54.1446552025549,-23.9009524404116,
39.9543158069384));
#186723=CARTESIAN_POINT('Ctrl Pts',(54.1347857162254,-23.8983090899562,
39.9636935671391));
#186724=CARTESIAN_POINT('Ctrl Pts',(54.1246839742778,-23.8964012454636,
39.9729968320988));
#186725=CARTESIAN_POINT('Ctrl Pts',(54.1143872866754,-23.8952825179497,
39.9821731151335));
#186726=CARTESIAN_POINT('Ctrl Pts',(54.1046536921683,-23.8942249700853,
39.9908475764352));
#186727=CARTESIAN_POINT('Ctrl Pts',(54.0947449925324,-23.8938724934877,
39.9994093733846));
#186728=CARTESIAN_POINT('Ctrl Pts',(54.0846948896055,-23.8943122764062,
40.0077966115842));
#186729=CARTESIAN_POINT('Ctrl Pts',(54.075438913413,-23.8947173090963,40.0155211172595));
#186730=CARTESIAN_POINT('Ctrl Pts',(54.0660624571234,-23.8957944255619,
40.0230979941022));
#186731=CARTESIAN_POINT('Ctrl Pts',(54.0566033397521,-23.8976480927551,
40.0304554104749));
#186732=CARTESIAN_POINT('Ctrl Pts',(54.0537828218966,-23.8982008188934,
40.0326492435181));
#186733=CARTESIAN_POINT('Ctrl Pts',(54.0509550659742,-23.898822847838,40.0348233715061));
#186734=CARTESIAN_POINT('Ctrl Pts',(54.0481214021002,-23.8995176373644,
40.0369753512356));
#186735=CARTESIAN_POINT('Ctrl Pts',(54.0453166912883,-23.9002053278539,
40.0391053430352));
#186736=CARTESIAN_POINT('Ctrl Pts',(54.042509037702,-23.9009633199466,40.041211089324));
#186737=CARTESIAN_POINT('Ctrl Pts',(54.0397028685177,-23.901793871638,40.0432881154904));
#186738=CARTESIAN_POINT('Ctrl Pts',(54.0395077330006,-23.9018516265783,
40.043432547828));
#186739=CARTESIAN_POINT('Ctrl Pts',(54.0393125964105,-23.9019097237176,
40.0435768364421));
#186740=CARTESIAN_POINT('Ctrl Pts',(54.0391174593312,-23.9019681642223,
40.0437209807855));
#186741=CARTESIAN_POINT('Ctrl Pts',(54.0305619349334,-23.9045304100322,
40.0500407968419));
#186742=CARTESIAN_POINT('Ctrl Pts',(54.0220283896864,-23.9077916774635,
40.0560490279343));
#186743=CARTESIAN_POINT('Ctrl Pts',(54.0136246330491,-23.9117952627741,
40.0616647108612));
#186744=CARTESIAN_POINT('Ctrl Pts',(54.0057908713001,-23.9155273001019,
40.0668995033481));
#186745=CARTESIAN_POINT('Ctrl Pts',(53.9980693056387,-23.9199049461648,
40.0717933267476));
#186746=CARTESIAN_POINT('Ctrl Pts',(53.9905727747505,-23.9249777890342,
40.0762460303065));
#186747=CARTESIAN_POINT('Ctrl Pts',(53.9878304467668,-23.9268335005847,
40.0778748868743));
#186748=CARTESIAN_POINT('Ctrl Pts',(53.9851185338205,-23.9287823509744,
40.0794443522245));
#186749=CARTESIAN_POINT('Ctrl Pts',(53.9824437337507,-23.9308270955484,
40.0809482021492));
#186750=CARTESIAN_POINT('Ctrl Pts',(53.9818005336912,-23.9313187883095,
40.0813098278168));
#186751=CARTESIAN_POINT('Ctrl Pts',(53.9811593045604,-23.9318165831365,
40.0816679525672));
#186752=CARTESIAN_POINT('Ctrl Pts',(53.9805201796371,-23.9323204546077,
40.0820224192581));
#186753=CARTESIAN_POINT('Ctrl Pts',(53.9799010273676,-23.9328085800954,
40.0823658088648));
#186754=CARTESIAN_POINT('Ctrl Pts',(53.9792838498571,-23.9333024083482,
40.0827057654617));
#186755=CARTESIAN_POINT('Ctrl Pts',(53.9786687697971,-23.9338019127823,
40.0830421470151));
#186756=CARTESIAN_POINT('Ctrl Pts',(53.9719298569081,-23.9392745611217,
40.0867275956808));
#186757=CARTESIAN_POINT('Ctrl Pts',(53.9654385427823,-23.9454324752048,
40.0899823432033));
#186758=CARTESIAN_POINT('Ctrl Pts',(53.9593734277039,-23.9522153560512,
40.0926299529359));
#186759=CARTESIAN_POINT('Ctrl Pts',(53.9568580436995,-23.9550284189139,
40.0937279956086));
#186760=CARTESIAN_POINT('Ctrl Pts',(53.9544158621939,-23.957948562403,40.0947220371803));
#186761=CARTESIAN_POINT('Ctrl Pts',(53.9520587513132,-23.9609698772113,
40.0956014538692));
#186762=CARTESIAN_POINT('Ctrl Pts',(53.9480384530775,-23.9661230444605,
40.097101390674));
#186763=CARTESIAN_POINT('Ctrl Pts',(53.9442681092575,-23.9715702598495,
40.0982667904316));
#186764=CARTESIAN_POINT('Ctrl Pts',(53.9408121161403,-23.9772776109211,
40.0990539325582));
#186765=CARTESIAN_POINT('Ctrl Pts',(53.9390841195817,-23.9801312864569,
40.0994475036216));
#186766=CARTESIAN_POINT('Ctrl Pts',(53.9374360035029,-23.9830506455186,
40.0997467259952));
#186767=CARTESIAN_POINT('Ctrl Pts',(53.9358758804724,-23.9860314303857,
40.0999473488896));
#186768=CARTESIAN_POINT('Ctrl Pts',(53.9343157574419,-23.9890122152529,
40.100147971784));
#186769=CARTESIAN_POINT('Ctrl Pts',(53.9328436288553,-23.9920543802862,
40.10025));
#186770=CARTESIAN_POINT('Ctrl Pts',(53.9314655730804,-23.9951532569808,
40.10025));
#186771=CARTESIAN_POINT('Origin',(50.4502867888875,-29.145084294463,39.92499));
#186772=CARTESIAN_POINT('Ctrl Pts',(54.1671020372438,-31.493361394986,39.92499));
#186773=CARTESIAN_POINT('Ctrl Pts',(54.176290852154,-31.4986665597479,39.9348354642018));
#186774=CARTESIAN_POINT('Ctrl Pts',(54.1858709973826,-31.5032309550533,
39.9446440828458));
#186775=CARTESIAN_POINT('Ctrl Pts',(54.1957854287835,-31.5070391691405,
39.9543641760331));
#186776=CARTESIAN_POINT('Ctrl Pts',(54.2053777002004,-31.5107236389463,
39.9637684240711));
#186777=CARTESIAN_POINT('Ctrl Pts',(54.2152841131307,-31.513700669305,39.9730909636394));
#186778=CARTESIAN_POINT('Ctrl Pts',(54.2254725303152,-31.5159144374962,
39.9822808977138));
#186779=CARTESIAN_POINT('Ctrl Pts',(54.2351101456051,-31.518008525889,39.9909740094647));
#186780=CARTESIAN_POINT('Ctrl Pts',(54.2450010037726,-31.5194198476563,
39.9995492764997));
#186781=CARTESIAN_POINT('Ctrl Pts',(54.255120730371,-31.520059140675,40.007946232869));
#186782=CARTESIAN_POINT('Ctrl Pts',(54.2644417304454,-31.52064797578,40.0156804369684));
#186783=CARTESIAN_POINT('Ctrl Pts',(54.2739574575936,-31.5205818213852,
40.0232638017416));
#186784=CARTESIAN_POINT('Ctrl Pts',(54.2836415202534,-31.5197533892257,
40.030625726996));
#186785=CARTESIAN_POINT('Ctrl Pts',(54.2864504987124,-31.5195130925472,
40.0327611416647));
#186786=CARTESIAN_POINT('Ctrl Pts',(54.2892735615563,-31.5192084034332,
40.0348777427268));
#186787=CARTESIAN_POINT('Ctrl Pts',(54.292109835428,-31.5188360425579,40.03697331687));
#186788=CARTESIAN_POINT('Ctrl Pts',(54.2951845386601,-31.5184323794286,
40.039245053974));
#186789=CARTESIAN_POINT('Ctrl Pts',(54.2982706300314,-31.5179508191004,
40.041487875195));
#186790=CARTESIAN_POINT('Ctrl Pts',(54.3013662138033,-31.5173878381076,
40.04369857016));
#186791=CARTESIAN_POINT('Ctrl Pts',(54.3098620677559,-31.515842732355,40.0497658398386));
#186792=CARTESIAN_POINT('Ctrl Pts',(54.3184108612912,-31.5136439393732,
40.0555581699984));
#186793=CARTESIAN_POINT('Ctrl Pts',(54.3269129314607,-31.5107627835357,
40.0609828468885));
#186794=CARTESIAN_POINT('Ctrl Pts',(54.3346918640778,-31.5081266823659,
40.0659461317305));
#186795=CARTESIAN_POINT('Ctrl Pts',(54.3424218244385,-31.504913297521,40.0706039980708));
#186796=CARTESIAN_POINT('Ctrl Pts',(54.3500333719155,-31.5010675328656,
40.0748843180606));
#186797=CARTESIAN_POINT('Ctrl Pts',(54.3537721391719,-31.4991785058297,
40.0769867972571));
#186798=CARTESIAN_POINT('Ctrl Pts',(54.3574819590038,-31.4971365594545,
40.0789976708176));
#186799=CARTESIAN_POINT('Ctrl Pts',(54.3611518569451,-31.4949332463334,
40.08090504915));
#186800=CARTESIAN_POINT('Ctrl Pts',(54.3618481843341,-31.4945151891293,
40.0812669556105));
#186801=CARTESIAN_POINT('Ctrl Pts',(54.3625432124818,-31.4940908087509,
40.0816253922033));
#186802=CARTESIAN_POINT('Ctrl Pts',(54.3632368016453,-31.4936601139562,
40.081980198914));
#186803=CARTESIAN_POINT('Ctrl Pts',(54.3639087161475,-31.4932428783739,
40.0823239179149));
#186804=CARTESIAN_POINT('Ctrl Pts',(54.3645792801848,-31.4928197168823,
40.0826642303499));
#186805=CARTESIAN_POINT('Ctrl Pts',(54.365248364808,-31.4923906407827,40.08300099161));
#186806=CARTESIAN_POINT('Ctrl Pts',(54.372539911164,-31.487714657862,40.0866709464311));
#186807=CARTESIAN_POINT('Ctrl Pts',(54.379660339308,-31.4823328301624,40.0899175831876));
#186808=CARTESIAN_POINT('Ctrl Pts',(54.3864229856957,-31.4762829888801,
40.092564206706));
#186809=CARTESIAN_POINT('Ctrl Pts',(54.3892788932594,-31.4737281033387,
40.0936818922527));
#186810=CARTESIAN_POINT('Ctrl Pts',(54.3920710496176,-31.4710545157388,
40.094693009479));
#186811=CARTESIAN_POINT('Ctrl Pts',(54.3947861357355,-31.4682668669586,
40.0955863397546));
#186812=CARTESIAN_POINT('Ctrl Pts',(54.3993582729152,-31.4635725360687,
40.0970906856166));
#186813=CARTESIAN_POINT('Ctrl Pts',(54.4037093249067,-31.4585547584352,
40.0982599215483));
#186814=CARTESIAN_POINT('Ctrl Pts',(54.4077698566065,-31.4532397415955,
40.0990497370454));
#186815=CARTESIAN_POINT('Ctrl Pts',(54.4087849895314,-31.4519109873856,
40.0992471909196));
#186816=CARTESIAN_POINT('Ctrl Pts',(54.4097817701143,-31.4505635261657,
40.0994209989363));
#186817=CARTESIAN_POINT('Ctrl Pts',(54.4107588499958,-31.4491976069258,
40.0995705982975));
#186818=CARTESIAN_POINT('Ctrl Pts',(54.4122244698181,-31.4471487280661,
40.0997949973393));
#186819=CARTESIAN_POINT('Ctrl Pts',(54.4136457436054,-31.4450583254658,
40.0999649129781));
#186820=CARTESIAN_POINT('Ctrl Pts',(54.4150195646481,-31.4429280944108,
40.1000786629733));
#186821=CARTESIAN_POINT('Ctrl Pts',(54.4163933856907,-31.4407978633559,
40.1001924129685));
#186822=CARTESIAN_POINT('Ctrl Pts',(54.4177197583729,-31.4386278145919,
40.10025));
#186823=CARTESIAN_POINT('Ctrl Pts',(54.4189959163063,-31.4364195775136,
40.10025));
#186824=CARTESIAN_POINT('Ctrl Pts',(51.1126068659047,-29.5274749692186,
40.10025));
#186825=CARTESIAN_POINT('Ctrl Pts',(51.1082885388132,-29.5349468458343,
40.10025));
#186826=CARTESIAN_POINT('Ctrl Pts',(51.104624414239,-29.5427104181375,40.0995786334242));
#186827=CARTESIAN_POINT('Ctrl Pts',(51.101604925595,-29.5506148782549,40.0983063763368));
#186828=CARTESIAN_POINT('Ctrl Pts',(51.0996546457482,-29.555720348447,40.0974846287994));
#186829=CARTESIAN_POINT('Ctrl Pts',(51.0979724198488,-29.5608842707082,
40.0964130309339));
#186830=CARTESIAN_POINT('Ctrl Pts',(51.0965469289497,-29.5660646037405,
40.0951176960924));
#186831=CARTESIAN_POINT('Ctrl Pts',(51.0946575224202,-29.5729308384266,
40.0934008039615));
#186832=CARTESIAN_POINT('Ctrl Pts',(51.0932249325813,-29.5798262755779,
40.0912909372157));
#186833=CARTESIAN_POINT('Ctrl Pts',(51.0922302752234,-29.5866628504238,
40.0888630467852));
#186834=CARTESIAN_POINT('Ctrl Pts',(51.0917329465444,-29.5900811378467,
40.08764910157));
#186835=CARTESIAN_POINT('Ctrl Pts',(51.0913449998289,-29.5934848814074,
40.0863558569272));
#186836=CARTESIAN_POINT('Ctrl Pts',(51.0910633609953,-29.596864293881,40.0849936342772));
#186837=CARTESIAN_POINT('Ctrl Pts',(51.0909225415785,-29.5985540001179,
40.0843125229522));
#186838=CARTESIAN_POINT('Ctrl Pts',(51.0908082908743,-29.6002376377882,
40.0836141747075));
#186839=CARTESIAN_POINT('Ctrl Pts',(51.0907201726671,-29.6019140726116,
40.082899916161));
#186840=CARTESIAN_POINT('Ctrl Pts',(51.0906981431153,-29.6023331813174,
40.0827213515244));
#186841=CARTESIAN_POINT('Ctrl Pts',(51.090677746668,-29.602751840147,40.0825417925842));
#186842=CARTESIAN_POINT('Ctrl Pts',(51.090658976153,-29.6031700319852,40.0823612602361));
#186843=CARTESIAN_POINT('Ctrl Pts',(51.0906026646081,-29.6044246074997,
40.0818196631918));
#186844=CARTESIAN_POINT('Ctrl Pts',(51.0905609873413,-29.6056749785904,
40.0812693052022));
#186845=CARTESIAN_POINT('Ctrl Pts',(51.0905337427829,-29.6069206965765,
40.0807107531875));
#186846=CARTESIAN_POINT('Ctrl Pts',(51.0903418356317,-29.6156953732194,
40.0767763849182));
#186847=CARTESIAN_POINT('Ctrl Pts',(51.0908211368931,-29.6242688491608,
40.0724140586136));
#186848=CARTESIAN_POINT('Ctrl Pts',(51.0918641424261,-29.6325885911862,
40.0677221223766));
#186849=CARTESIAN_POINT('Ctrl Pts',(51.0923699989825,-29.6366236570779,
40.0654465383719));
#186850=CARTESIAN_POINT('Ctrl Pts',(51.0930089302516,-29.6405993642578,
40.0630928000679));
#186851=CARTESIAN_POINT('Ctrl Pts',(51.0937712117414,-29.6445110377125,
40.0606689262479));
#186852=CARTESIAN_POINT('Ctrl Pts',(51.0949382114433,-29.6504995364712,
40.0569581447805));
#186853=CARTESIAN_POINT('Ctrl Pts',(51.0963926103116,-29.656334864082,40.0530843804605));
#186854=CARTESIAN_POINT('Ctrl Pts',(51.098099028059,-29.6619874481815,40.0490800251457));
#186855=CARTESIAN_POINT('Ctrl Pts',(51.0988914972888,-29.6646125374799,
40.0472203818218));
#186856=CARTESIAN_POINT('Ctrl Pts',(51.0997380650833,-29.6671982043427,
40.0453323608818));
#186857=CARTESIAN_POINT('Ctrl Pts',(51.1006362623629,-29.6697408831276,
40.0434201572162));
#186858=CARTESIAN_POINT('Ctrl Pts',(51.1007051056453,-29.6699357694378,
40.0432735943397));
#186859=CARTESIAN_POINT('Ctrl Pts',(51.1007742270251,-29.6701304259131,
40.0431268995707));
#186860=CARTESIAN_POINT('Ctrl Pts',(51.1008436251324,-29.6703248520469,
40.0429800745037));
#186861=CARTESIAN_POINT('Ctrl Pts',(51.1018184593124,-29.67305595305,40.0409176249753));
#186862=CARTESIAN_POINT('Ctrl Pts',(51.1028499068178,-29.6757410298218,
40.0388310783332));
#186863=CARTESIAN_POINT('Ctrl Pts',(51.1039327914267,-29.6783776815769,
40.036725739981));
#186864=CARTESIAN_POINT('Ctrl Pts',(51.10781582305,-29.6878322458584,40.0291763710714));
#186865=CARTESIAN_POINT('Ctrl Pts',(51.1123884412308,-29.6967379921839,
40.0213310894586));
#186866=CARTESIAN_POINT('Ctrl Pts',(51.1175230541902,-29.705114752369,40.0132837551307));
#186867=CARTESIAN_POINT('Ctrl Pts',(51.1231654780149,-29.7143199702922,
40.0044405431309));
#186868=CARTESIAN_POINT('Ctrl Pts',(51.129486757898,-29.7228870317522,39.9953528710581));
#186869=CARTESIAN_POINT('Ctrl Pts',(51.1363687775798,-29.7308286942781,
39.9861103629531));
#186870=CARTESIAN_POINT('Ctrl Pts',(51.1437996316847,-29.7394036967207,
39.9761307737529));
#186871=CARTESIAN_POINT('Ctrl Pts',(51.1518848590033,-29.747250549869,39.9659696935981));
#186872=CARTESIAN_POINT('Ctrl Pts',(51.160525858428,-29.7543572078959,39.9557128217472));
#186873=CARTESIAN_POINT('Ctrl Pts',(51.1690943687448,-29.761404248363,39.9455419945137));
#186874=CARTESIAN_POINT('Ctrl Pts',(51.1782106315453,-29.7677241373274,
39.9352756289329));
#186875=CARTESIAN_POINT('Ctrl Pts',(51.1878102687784,-29.7732664904681,
39.92499));
#186876=CARTESIAN_POINT('Origin',(0.00762000000000077,0.0131982271536777,
39.92499));
#186877=CARTESIAN_POINT('Ctrl Pts',(54.4342359163063,-31.4100231232062,
40.10025));
#186878=CARTESIAN_POINT('Ctrl Pts',(54.4385272722023,-31.4025830926774,
40.10025));
#186879=CARTESIAN_POINT('Ctrl Pts',(54.442158989064,-31.3948506994793,40.0995859581841));
#186880=CARTESIAN_POINT('Ctrl Pts',(54.4451438299616,-31.386976274769,40.0983275959619));
#186881=CARTESIAN_POINT('Ctrl Pts',(54.4470510012009,-31.3819448922437,
40.0975235624067));
#186882=CARTESIAN_POINT('Ctrl Pts',(54.4486949601301,-31.3768558346348,
40.096477705949));
#186883=CARTESIAN_POINT('Ctrl Pts',(54.4500875286681,-31.3717496422764,
40.0952149915961));
#186884=CARTESIAN_POINT('Ctrl Pts',(54.4519881053013,-31.3647807142729,
40.0934916398701));
#186885=CARTESIAN_POINT('Ctrl Pts',(54.4534143418203,-31.3577796218683,
40.0913643921631));
#186886=CARTESIAN_POINT('Ctrl Pts',(54.4543880442396,-31.3508395087086,
40.0889118607713));
#186887=CARTESIAN_POINT('Ctrl Pts',(54.4548748954493,-31.3473694521287,
40.0876855950755));
#186888=CARTESIAN_POINT('Ctrl Pts',(54.4552487192094,-31.3439144604654,
40.0863782327527));
#186889=CARTESIAN_POINT('Ctrl Pts',(54.4555129946225,-31.3404848880614,
40.0850006373334));
#186890=CARTESIAN_POINT('Ctrl Pts',(54.4556451323291,-31.3387701018594,
40.0843118396238));
#186891=CARTESIAN_POINT('Ctrl Pts',(54.4557498916996,-31.3370616554168,
40.0836054919165));
#186892=CARTESIAN_POINT('Ctrl Pts',(54.4558277627246,-31.3353607484812,
40.0828829920418));
#186893=CARTESIAN_POINT('Ctrl Pts',(54.4558472304808,-31.3349355217473,
40.0827023670731));
#186894=CARTESIAN_POINT('Ctrl Pts',(54.4558650179028,-31.3345107659124,
40.0825207326933));
#186895=CARTESIAN_POINT('Ctrl Pts',(54.4558811330249,-31.334086499077,40.0823381109276));
#186896=CARTESIAN_POINT('Ctrl Pts',(54.4559294783911,-31.3328136985707,
40.0817902456304));
#186897=CARTESIAN_POINT('Ctrl Pts',(54.4559627721159,-31.331545300654,40.0812334935553));
#186898=CARTESIAN_POINT('Ctrl Pts',(54.4559812395338,-31.3302817797845,
40.0806684524227));
#186899=CARTESIAN_POINT('Ctrl Pts',(54.4561088608496,-31.3215500666178,
40.0767636676136));
#186900=CARTESIAN_POINT('Ctrl Pts',(54.4555742713438,-31.3130195924484,
40.0724404510887));
#186901=CARTESIAN_POINT('Ctrl Pts',(54.4544853519657,-31.3047400858587,
40.0677949937407));
#186902=CARTESIAN_POINT('Ctrl Pts',(54.4539441620239,-31.3006251938107,
40.0654862141904));
#186903=CARTESIAN_POINT('Ctrl Pts',(54.4532655373259,-31.2965719591984,
40.0630972003215));
#186904=CARTESIAN_POINT('Ctrl Pts',(54.4524598885395,-31.2925850928564,
40.0606363359906));
#186905=CARTESIAN_POINT('Ctrl Pts',(54.4506825069818,-31.283789470212,40.0552073017124));
#186906=CARTESIAN_POINT('Ctrl Pts',(54.4482992497266,-31.2753153512347,
40.0494204304519));
#186907=CARTESIAN_POINT('Ctrl Pts',(54.4454010706198,-31.2672761140351,
40.0434049749851));
#186908=CARTESIAN_POINT('Ctrl Pts',(54.4443423292441,-31.264339279306,40.0412074532442));
#186909=CARTESIAN_POINT('Ctrl Pts',(54.4432206434044,-31.2614550023639,
40.0389814735788));
#186910=CARTESIAN_POINT('Ctrl Pts',(54.4420411592048,-31.2586246102246,
40.0367321210016));
#186911=CARTESIAN_POINT('Ctrl Pts',(54.4380793965876,-31.2491176225317,
40.0291767837142));
#186912=CARTESIAN_POINT('Ctrl Pts',(54.4334326446233,-31.2401615453397,
40.021323533258));
#186913=CARTESIAN_POINT('Ctrl Pts',(54.4282277812596,-31.2317373058274,
40.0132649215865));
#186914=CARTESIAN_POINT('Ctrl Pts',(54.4225070198661,-31.2224780686866,
40.0044075527541));
#186915=CARTESIAN_POINT('Ctrl Pts',(54.4161118092713,-31.2138606686957,
39.995301625373));
#186916=CARTESIAN_POINT('Ctrl Pts',(54.4091594014093,-31.2058737429081,
39.9860353422371));
#186917=CARTESIAN_POINT('Ctrl Pts',(54.4016713602548,-31.1972714816222,
39.9760551582709));
#186918=CARTESIAN_POINT('Ctrl Pts',(54.3935362880566,-31.1893995936782,
39.9658879738171));
#186919=CARTESIAN_POINT('Ctrl Pts',(54.3848513315137,-31.1822725865945,
39.9556174643271));
#186920=CARTESIAN_POINT('Ctrl Pts',(54.3762836512073,-31.1752418181694,
39.9454856413916));
#186921=CARTESIAN_POINT('Ctrl Pts',(54.3671795569349,-31.1689352997159,
39.9352519465119));
#186922=CARTESIAN_POINT('Ctrl Pts',(54.3576020372438,-31.1634057161441,
39.92499));
#186923=CARTESIAN_POINT('Ctrl Pts',(51.3783102687785,-29.4433108116262,
39.92499));
#186924=CARTESIAN_POINT('Ctrl Pts',(51.3691445298583,-29.4380189697933,
39.9348107241731));
#186925=CARTESIAN_POINT('Ctrl Pts',(51.3595943606098,-29.4334690915847,
39.9446038383186));
#186926=CARTESIAN_POINT('Ctrl Pts',(51.3497152868745,-29.4296781246241,
39.954315806941));
#186927=CARTESIAN_POINT('Ctrl Pts',(51.3401761719842,-29.4260176124798,
39.9636935671422));
#186928=CARTESIAN_POINT('Ctrl Pts',(51.3303291924883,-29.4230642997968,
39.9729968321024));
#186929=CARTESIAN_POINT('Ctrl Pts',(51.3202058500852,-29.4208754038575,
39.9821731151375));
#186930=CARTESIAN_POINT('Ctrl Pts',(51.3106361210799,-29.4188062116752,
39.9908475764395));
#186931=CARTESIAN_POINT('Ctrl Pts',(51.300818546174,-29.4174199248356,39.9994093733891));
#186932=CARTESIAN_POINT('Ctrl Pts',(51.2907775289294,-29.4168067767629,
40.0077966115889));
#186933=CARTESIAN_POINT('Ctrl Pts',(51.281529920498,-29.4162420776743,40.0155211172644));
#186934=CARTESIAN_POINT('Ctrl Pts',(51.2720922400877,-29.4163331870167,
40.0230979941072));
#186935=CARTESIAN_POINT('Ctrl Pts',(51.2624911797676,-29.4171879526248,
40.03045541048));
#186936=CARTESIAN_POINT('Ctrl Pts',(51.2596283373925,-29.4174428264743,
40.0326492435215));
#186937=CARTESIAN_POINT('Ctrl Pts',(51.2567510524854,-29.4177658668981,
40.0348233715077));
#186938=CARTESIAN_POINT('Ctrl Pts',(51.2538602864394,-29.4181606517643,
40.0369753512356));
#186939=CARTESIAN_POINT('Ctrl Pts',(51.2509990568967,-29.4185514029023,
40.0391053430352));
#186940=CARTESIAN_POINT('Ctrl Pts',(51.2481275521818,-29.4190117629202,
40.041211089324));
#186941=CARTESIAN_POINT('Ctrl Pts',(51.2452499391939,-29.41954444021,40.0432881154904));
#186942=CARTESIAN_POINT('Ctrl Pts',(51.2450498356145,-29.4195814815469,
40.043432547828));
#186943=CARTESIAN_POINT('Ctrl Pts',(51.2448496951983,-29.4196188630961,
40.0435768364421));
#186944=CARTESIAN_POINT('Ctrl Pts',(51.2446495184043,-29.4196565860786,
40.0437209807855));
#186945=CARTESIAN_POINT('Ctrl Pts',(51.2358730344471,-29.4213104998201,
40.050040796842));
#186946=CARTESIAN_POINT('Ctrl Pts',(51.2270453415809,-29.4236619033164,
40.0560490279344));
#186947=CARTESIAN_POINT('Ctrl Pts',(51.2182691329815,-29.4267651248008,
40.0616647108614));
#186948=CARTESIAN_POINT('Ctrl Pts',(51.2100881812722,-29.4296578665605,
40.0668995033484));
#186949=CARTESIAN_POINT('Ctrl Pts',(51.2019513265394,-29.4332044080278,
40.071793326748));
#186950=CARTESIAN_POINT('Ctrl Pts',(51.1939656059621,-29.4374658604798,
40.0762460303071));
#186951=CARTESIAN_POINT('Ctrl Pts',(51.1910443260617,-29.4390247549181,
40.0778748868747));
#186952=CARTESIAN_POINT('Ctrl Pts',(51.1881435589222,-29.4406794572086,
40.0794443522247));
#186953=CARTESIAN_POINT('Ctrl Pts',(51.1852696776793,-29.4424334077168,
40.0809482021492));
#186954=CARTESIAN_POINT('Ctrl Pts',(51.1845786052483,-29.4428551742197,
40.0813098278168));
#186955=CARTESIAN_POINT('Ctrl Pts',(51.1838888551095,-29.4432832153789,
40.0816679525672));
#186956=CARTESIAN_POINT('Ctrl Pts',(51.1832005624688,-29.4437175198434,
40.082022419258));
#186957=CARTESIAN_POINT('Ctrl Pts',(51.1825337789732,-29.4441382522934,
40.0823658088648));
#186958=CARTESIAN_POINT('Ctrl Pts',(51.1818683633172,-29.4445648626866,
40.0827057654616));
#186959=CARTESIAN_POINT('Ctrl Pts',(51.1812044402993,-29.4449973374096,
40.0830421470151));
#186960=CARTESIAN_POINT('Ctrl Pts',(51.1739303963596,-29.4497355978002,
40.0867275956805));
#186961=CARTESIAN_POINT('Ctrl Pts',(51.1668309650361,-29.4551812510951,
40.089982343203));
#186962=CARTESIAN_POINT('Ctrl Pts',(51.1600900711817,-29.4612929974515,
40.0926299529354));
#186963=CARTESIAN_POINT('Ctrl Pts',(51.1572944215756,-29.4638277208372,
40.0937279956083));
#186964=CARTESIAN_POINT('Ctrl Pts',(51.1545603804839,-29.4664765899953,
40.0947220371802));
#186965=CARTESIAN_POINT('Ctrl Pts',(51.151900368709,-29.4692349685472,40.0956014538692));
#186966=CARTESIAN_POINT('Ctrl Pts',(51.1473634414341,-29.4739396706106,
40.097101390674));
#186967=CARTESIAN_POINT('Ctrl Pts',(51.1430443628984,-29.4789629373382,
40.0982667904316));
#186968=CARTESIAN_POINT('Ctrl Pts',(51.1390107214365,-29.484277773294,40.0990539325582));
#186969=CARTESIAN_POINT('Ctrl Pts',(51.1369939007055,-29.4869351912719,
40.0994475036216));
#186970=CARTESIAN_POINT('Ctrl Pts',(51.1350496570625,-29.4896662827381,
40.0997467259952));
#186971=CARTESIAN_POINT('Ctrl Pts',(51.1331865036877,-29.492467661291,40.0999473488896));
#186972=CARTESIAN_POINT('Ctrl Pts',(51.1313233503129,-29.4952690398439,
40.100147971784));
#186973=CARTESIAN_POINT('Ctrl Pts',(51.1295412933646,-29.4981406602398,
40.10025));
#186974=CARTESIAN_POINT('Ctrl Pts',(51.1278468659047,-29.5010785149112,
40.10025));
#186975=CARTESIAN_POINT('Origin',(47.1274239660509,-34.2589154226522,39.92499));
#186976=CARTESIAN_POINT('Ctrl Pts',(50.5784163149356,-36.9828414016747,
39.92499));
#186977=CARTESIAN_POINT('Ctrl Pts',(50.5870002518364,-36.9890779968908,
39.9348354642022));
#186978=CARTESIAN_POINT('Ctrl Pts',(50.5960508068002,-36.9946187858199,
39.9446440828466));
#186979=CARTESIAN_POINT('Ctrl Pts',(50.6055128591424,-36.9994424783904,
39.9543641760342));
#186980=CARTESIAN_POINT('Ctrl Pts',(50.6146674511263,-37.0041094296755,
39.9637684240726));
#186981=CARTESIAN_POINT('Ctrl Pts',(50.6242084112817,-37.0081056536706,
39.9730909636412));
#186982=CARTESIAN_POINT('Ctrl Pts',(50.6341096134641,-37.0113722741994,
39.9822808977158));
#186983=CARTESIAN_POINT('Ctrl Pts',(50.6434755410477,-37.0144622960727,
39.9909740094668));
#186984=CARTESIAN_POINT('Ctrl Pts',(50.6531646927642,-37.0168997626763,
39.9995492765021));
#186985=CARTESIAN_POINT('Ctrl Pts',(50.663162158125,-37.0185933530509,40.0079462328715));
#186986=CARTESIAN_POINT('Ctrl Pts',(50.6723705467575,-37.0201532722694,
40.0156804369711));
#186987=CARTESIAN_POINT('Ctrl Pts',(50.6818410607745,-37.021082144611,40.0232638017444));
#186988=CARTESIAN_POINT('Ctrl Pts',(50.6915586678667,-37.0212705108774,
40.0306257269989));
#186989=CARTESIAN_POINT('Ctrl Pts',(50.6943773762892,-37.021325148771,40.0327611416667));
#186990=CARTESIAN_POINT('Ctrl Pts',(50.6972168227831,-37.0213172191965,
40.0348777427279));
#186991=CARTESIAN_POINT('Ctrl Pts',(50.7000764815586,-37.0212433695024,
40.0369733168701));
#186992=CARTESIAN_POINT('Ctrl Pts',(50.7031765355313,-37.0211633116858,
40.0392450539741));
#186993=CARTESIAN_POINT('Ctrl Pts',(50.7062960577322,-37.0210069737841,
40.041487875195));
#186994=CARTESIAN_POINT('Ctrl Pts',(50.7094335311103,-37.0207706534746,
40.0436985701601));
#186995=CARTESIAN_POINT('Ctrl Pts',(50.718044351416,-37.0201220705309,40.0497658398386));
#186996=CARTESIAN_POINT('Ctrl Pts',(50.7267761502172,-37.0188289150181,
40.0555581699984));
#186997=CARTESIAN_POINT('Ctrl Pts',(50.7355328079489,-37.0168522507831,
40.0609828468885));
#186998=CARTESIAN_POINT('Ctrl Pts',(50.7435446743638,-37.0150437103237,
40.0659461317307));
#186999=CARTESIAN_POINT('Ctrl Pts',(50.7515681793728,-37.0126559296146,
40.0706039980711));
#187000=CARTESIAN_POINT('Ctrl Pts',(50.7595400218662,-37.0096268558211,
40.0748843180609));
#187001=CARTESIAN_POINT('Ctrl Pts',(50.7634557648571,-37.0081389846688,
40.0769867972574));
#187002=CARTESIAN_POINT('Ctrl Pts',(50.7673587034243,-37.0064960060557,
40.0789976708176));
#187003=CARTESIAN_POINT('Ctrl Pts',(50.771238806215,-37.0046883717067,40.0809050491499));
#187004=CARTESIAN_POINT('Ctrl Pts',(50.7719750179269,-37.0043453906956,
40.0812669556104));
#187005=CARTESIAN_POINT('Ctrl Pts',(50.7727105984664,-37.0039959853415,
40.0816253922032));
#187006=CARTESIAN_POINT('Ctrl Pts',(50.7734454079409,-37.0036401497474,
40.0819801989139));
#187007=CARTESIAN_POINT('Ctrl Pts',(50.7741572546194,-37.0032954340157,
40.0823239179149));
#187008=CARTESIAN_POINT('Ctrl Pts',(50.7748683776572,-37.0029446836753,
40.0826642303498));
#187009=CARTESIAN_POINT('Ctrl Pts',(50.7755786476302,-37.0025878964869,
40.0830009916099));
#187010=CARTESIAN_POINT('Ctrl Pts',(50.7833190234413,-36.9986997032254,
40.0866709464311));
#187011=CARTESIAN_POINT('Ctrl Pts',(50.790962999314,-36.9940916451527,40.0899175831876));
#187012=CARTESIAN_POINT('Ctrl Pts',(50.7983209798294,-36.9887818345684,
40.092564206706));
#187013=CARTESIAN_POINT('Ctrl Pts',(50.8014283006921,-36.9865394685863,
40.0936818922526));
#187014=CARTESIAN_POINT('Ctrl Pts',(50.8044846273289,-36.9841723869924,
40.094693009479));
#187015=CARTESIAN_POINT('Ctrl Pts',(50.807476228564,-36.9816838130234,40.0955863397545));
#187016=CARTESIAN_POINT('Ctrl Pts',(50.8125140102918,-36.9774931166426,
40.0970906856166));
#187017=CARTESIAN_POINT('Ctrl Pts',(50.8173657273503,-36.9729576356982,
40.0982599215483));
#187018=CARTESIAN_POINT('Ctrl Pts',(50.8219595855749,-36.9680961762154,
40.0990497370453));
#187019=CARTESIAN_POINT('Ctrl Pts',(50.8231080501311,-36.9668808113447,
40.0992471909196));
#187020=CARTESIAN_POINT('Ctrl Pts',(50.8242402182962,-36.9656449236009,
40.0994209989363));
#187021=CARTESIAN_POINT('Ctrl Pts',(50.8253547230711,-36.9643886196681,
40.0995705982975));
#187022=CARTESIAN_POINT('Ctrl Pts',(50.8270264802333,-36.9625041637689,
40.0997949973393));
#187023=CARTESIAN_POINT('Ctrl Pts',(50.8286584747055,-36.9605737761776,
40.0999649129781));
#187024=CARTESIAN_POINT('Ctrl Pts',(50.8302474395913,-36.9585988181537,
40.1000786629733));
#187025=CARTESIAN_POINT('Ctrl Pts',(50.8318364044772,-36.9566238601298,
40.1001924129685));
#187026=CARTESIAN_POINT('Ctrl Pts',(50.833382343015,-36.9546043428193,40.10025));
#187027=CARTESIAN_POINT('Ctrl Pts',(50.83488233365,-36.9525415975223,40.10025));
#187028=CARTESIAN_POINT('Ctrl Pts',(47.7461450747864,-34.7084426211232,
40.10025));
#187029=CARTESIAN_POINT('Ctrl Pts',(47.7410693801618,-34.7154221779228,
40.10025));
#187030=CARTESIAN_POINT('Ctrl Pts',(47.7366138137628,-34.7227602152543,
40.099578633424));
#187031=CARTESIAN_POINT('Ctrl Pts',(47.7327846251243,-34.7303057514049,
40.0983063763365));
#187032=CARTESIAN_POINT('Ctrl Pts',(47.7303113621615,-34.7351793935412,
40.0974846287991));
#187033=CARTESIAN_POINT('Ctrl Pts',(47.7280985748135,-34.7401391868071,
40.0964130309337));
#187034=CARTESIAN_POINT('Ctrl Pts',(47.7261394006518,-34.7451421370594,
40.0951176960923));
#187035=CARTESIAN_POINT('Ctrl Pts',(47.7235426275288,-34.7517732610324,
40.0934008039614));
#187036=CARTESIAN_POINT('Ctrl Pts',(47.721397116118,-34.7584811778432,40.0912909372156));
#187037=CARTESIAN_POINT('Ctrl Pts',(47.7196932909345,-34.7651763312116,
40.0888630467851));
#187038=CARTESIAN_POINT('Ctrl Pts',(47.7188413783428,-34.7685239078958,
40.0876491015699));
#187039=CARTESIAN_POINT('Ctrl Pts',(47.7180997687562,-34.7718684539192,
40.0863558569271));
#187040=CARTESIAN_POINT('Ctrl Pts',(47.717466427977,-34.7751999143432,40.0849936342771));
#187041=CARTESIAN_POINT('Ctrl Pts',(47.7171497575873,-34.7768656445553,
40.0843125229521));
#187042=CARTESIAN_POINT('Ctrl Pts',(47.716860144702,-34.7785281166318,40.0836141747074));
#187043=CARTESIAN_POINT('Ctrl Pts',(47.7165972740597,-34.780186156909,40.0828999161609));
#187044=CARTESIAN_POINT('Ctrl Pts',(47.7165315563991,-34.7806006669783,
40.0827213515243));
#187045=CARTESIAN_POINT('Ctrl Pts',(47.7164675099217,-34.7810149003417,
40.0825417925842));
#187046=CARTESIAN_POINT('Ctrl Pts',(47.7164051292834,-34.7814288392281,
40.0823612602361));
#187047=CARTESIAN_POINT('Ctrl Pts',(47.7162179873684,-34.7826706558875,
40.0818196631917));
#187048=CARTESIAN_POINT('Ctrl Pts',(47.7160458390454,-34.7839098208538,
40.0812693052021));
#187049=CARTESIAN_POINT('Ctrl Pts',(47.7158885307488,-34.7851458668347,
40.0807107531874));
#187050=CARTESIAN_POINT('Ctrl Pts',(47.7147804714199,-34.7938524151211,
40.0767763849181));
#187051=CARTESIAN_POINT('Ctrl Pts',(47.7143609747538,-34.8024290252884,
40.0724140586137));
#187052=CARTESIAN_POINT('Ctrl Pts',(47.7145286167446,-34.8108122146619,
40.0677221223768));
#187053=CARTESIAN_POINT('Ctrl Pts',(47.714609922929,-34.8148780524491,40.065446538372));
#187054=CARTESIAN_POINT('Ctrl Pts',(47.7148297795039,-34.8188987667928,
40.0630928000679));
#187055=CARTESIAN_POINT('Ctrl Pts',(47.7151790039209,-34.8228686918039,
40.0606689262479));
#187056=CARTESIAN_POINT('Ctrl Pts',(47.7157136421037,-34.8289463696253,
40.0569581447805));
#187057=CARTESIAN_POINT('Ctrl Pts',(47.7165501157951,-34.8349017567796,
40.0530843804605));
#187058=CARTESIAN_POINT('Ctrl Pts',(47.7176563296782,-34.8407017446568,
40.0490800251457));
#187059=CARTESIAN_POINT('Ctrl Pts',(47.7181700611282,-34.8433952890321,
40.0472203818218));
#187060=CARTESIAN_POINT('Ctrl Pts',(47.7187417155521,-34.8460552817719,
40.0453323608818));
#187061=CARTESIAN_POINT('Ctrl Pts',(47.719369210107,-34.8486779186777,40.0434201572162));
#187062=CARTESIAN_POINT('Ctrl Pts',(47.7194173050922,-34.8488789334628,
40.0432735943397));
#187063=CARTESIAN_POINT('Ctrl Pts',(47.7194657006756,-34.8490797487412,
40.0431268995707));
#187064=CARTESIAN_POINT('Ctrl Pts',(47.7195143955479,-34.8492803638658,
40.0429800745037));
#187065=CARTESIAN_POINT('Ctrl Pts',(47.7201984116934,-34.8520984015307,
40.0409176249753));
#187066=CARTESIAN_POINT('Ctrl Pts',(47.7209435418727,-34.8548765847936,
40.0388310783332));
#187067=CARTESIAN_POINT('Ctrl Pts',(47.7217448891703,-34.8576119849586,
40.036725739981));
#187068=CARTESIAN_POINT('Ctrl Pts',(47.7246183780646,-34.8674206434752,
40.0291763710721));
#187069=CARTESIAN_POINT('Ctrl Pts',(47.7282350429864,-34.8767555719411,
40.0213310894601));
#187070=CARTESIAN_POINT('Ctrl Pts',(47.732465918129,-34.8856231565589,40.013283755133));
#187071=CARTESIAN_POINT('Ctrl Pts',(47.7371152248815,-34.8953677412259,
40.004440543134));
#187072=CARTESIAN_POINT('Ctrl Pts',(47.7425063743623,-34.9045486250982,
39.995352871062));
#187073=CARTESIAN_POINT('Ctrl Pts',(47.7485205638398,-34.9131661493068,
39.9861103629579));
#187074=CARTESIAN_POINT('Ctrl Pts',(47.7550143791198,-34.9224709127486,
39.9761307737586));
#187075=CARTESIAN_POINT('Ctrl Pts',(47.7622350952152,-34.9311199164006,
39.9659696936047));
#187076=CARTESIAN_POINT('Ctrl Pts',(47.7700859102973,-34.9390908738019,
39.9557128217548));
#187077=CARTESIAN_POINT('Ctrl Pts',(47.7778708651091,-34.9469949630621,
39.9455419945188));
#187078=CARTESIAN_POINT('Ctrl Pts',(47.7862765797886,-34.9542331399568,
39.9352756289355));
#187079=CARTESIAN_POINT('Ctrl Pts',(47.7952442955502,-34.9607485668366,
39.92499));
#187080=CARTESIAN_POINT('Origin',(0.00895784724493838,0.0123294189942775,
39.92499));
#187081=CARTESIAN_POINT('Ctrl Pts',(50.8527980281385,-36.9278827595327,
40.10025));
#187082=CARTESIAN_POINT('Ctrl Pts',(50.8578435704958,-36.9209320551068,
40.10025));
#187083=CARTESIAN_POINT('Ctrl Pts',(50.8622636476109,-36.9136216385502,
40.0995859581841));
#187084=CARTESIAN_POINT('Ctrl Pts',(50.8660552387518,-36.9061023515945,
40.0983275959619));
#187085=CARTESIAN_POINT('Ctrl Pts',(50.868477884991,-36.9012978851879,40.0975235624066));
#187086=CARTESIAN_POINT('Ctrl Pts',(50.8706447895124,-36.8964085464697,
40.0964777059489));
#187087=CARTESIAN_POINT('Ctrl Pts',(50.8725634718546,-36.8914758894166,
40.095214991596));
#187088=CARTESIAN_POINT('Ctrl Pts',(50.875182088265,-36.8847438022847,40.09349163987));
#187089=CARTESIAN_POINT('Ctrl Pts',(50.8773323251414,-36.8779301449084,
40.091364392163));
#187090=CARTESIAN_POINT('Ctrl Pts',(50.8790261328804,-36.8711298300322,
40.0889118607712));
#187091=CARTESIAN_POINT('Ctrl Pts',(50.87987303675,-36.8677296725942,40.0876855950753));
#187092=CARTESIAN_POINT('Ctrl Pts',(50.8806059576336,-36.86433268296,40.0863782327526));
#187093=CARTESIAN_POINT('Ctrl Pts',(50.8812272732514,-36.8609495224152,
40.0850006373333));
#187094=CARTESIAN_POINT('Ctrl Pts',(50.8815379310603,-36.8592579421429,
40.0843118396237));
#187095=CARTESIAN_POINT('Ctrl Pts',(50.8818206978293,-36.8575698050846,
40.0836054919164));
#187096=CARTESIAN_POINT('Ctrl Pts',(50.8820759354568,-36.8558863556338,
40.0828829920417));
#187097=CARTESIAN_POINT('Ctrl Pts',(50.8821397448637,-36.8554654932711,
40.082702367073));
#187098=CARTESIAN_POINT('Ctrl Pts',(50.882201833919,-36.855044923585,40.0825207326932));
#187099=CARTESIAN_POINT('Ctrl Pts',(50.8822622087211,-36.8546246654166,
40.0823381109275));
#187100=CARTESIAN_POINT('Ctrl Pts',(50.8824433331273,-36.8533638909115,
40.0817902456303));
#187101=CARTESIAN_POINT('Ctrl Pts',(50.8826090281505,-36.8521059215532,
40.0812334935552));
#187102=CARTESIAN_POINT('Ctrl Pts',(50.8827594682968,-36.850851252754,40.0806684524226));
#187103=CARTESIAN_POINT('Ctrl Pts',(50.8837991030487,-36.842180712886,40.0767636676137));
#187104=CARTESIAN_POINT('Ctrl Pts',(50.884159119436,-36.8336410897275,40.072440451089));
#187105=CARTESIAN_POINT('Ctrl Pts',(50.8839416093727,-36.8252931160723,
40.0677949937412));
#187106=CARTESIAN_POINT('Ctrl Pts',(50.8838335074683,-36.8211441960801,
40.0654862141907));
#187107=CARTESIAN_POINT('Ctrl Pts',(50.8835822787327,-36.8170422299141,
40.0630972003217));
#187108=CARTESIAN_POINT('Ctrl Pts',(50.8831977843866,-36.8129929908131,
40.0606363359906));
#187109=CARTESIAN_POINT('Ctrl Pts',(50.8823495324296,-36.804059764547,40.0552073017123));
#187110=CARTESIAN_POINT('Ctrl Pts',(50.8808651175412,-36.7953829494616,
40.0494204304519));
#187111=CARTESIAN_POINT('Ctrl Pts',(50.8788231440731,-36.7870848098363,
40.0434049749851));
#187112=CARTESIAN_POINT('Ctrl Pts',(50.8780771854145,-36.7840533947861,
40.0412074532442));
#187113=CARTESIAN_POINT('Ctrl Pts',(50.8772631333235,-36.7810676701177,
40.0389814735788));
#187114=CARTESIAN_POINT('Ctrl Pts',(50.8763859670025,-36.7781294934919,
40.0367321210017));
#187115=CARTESIAN_POINT('Ctrl Pts',(50.8734396581493,-36.7682604691142,
40.0291767837144));
#187116=CARTESIAN_POINT('Ctrl Pts',(50.8697545265642,-36.7588677364083,
40.0213235332583));
#187117=CARTESIAN_POINT('Ctrl Pts',(50.8654587487971,-36.7499455893927,
40.0132649215869));
#187118=CARTESIAN_POINT('Ctrl Pts',(50.8607371801626,-36.7401390929248,
40.0044075527547));
#187119=CARTESIAN_POINT('Ctrl Pts',(50.8552777667792,-36.7309004184172,
39.9953016253738));
#187120=CARTESIAN_POINT('Ctrl Pts',(50.8491983060139,-36.7222305213351,
39.986035342238));
#187121=CARTESIAN_POINT('Ctrl Pts',(50.8426504662856,-36.7128926707021,
39.9760551582722));
#187122=CARTESIAN_POINT('Ctrl Pts',(50.8353827952143,-36.7042135591887,
39.9658879738187));
#187123=CARTESIAN_POINT('Ctrl Pts',(50.8274903908706,-36.6962177694347,
39.955617464329));
#187124=CARTESIAN_POINT('Ctrl Pts',(50.819704560632,-36.6883299498379,39.9454856413929));
#187125=CARTESIAN_POINT('Ctrl Pts',(50.8113095502226,-36.6811063421681,
39.9352519465126));
#187126=CARTESIAN_POINT('Ctrl Pts',(50.8023624960591,-36.6746059268179,
39.92499));
#187127=CARTESIAN_POINT('Ctrl Pts',(48.0191904766736,-34.6525130919798,
39.92499));
#187128=CARTESIAN_POINT('Ctrl Pts',(48.0106280967258,-34.6462921588067,
39.9348107241721));
#187129=CARTESIAN_POINT('Ctrl Pts',(48.0016058360818,-34.640768940792,39.9446038383167));
#187130=CARTESIAN_POINT('Ctrl Pts',(47.9921771448978,-34.6359660967493,
39.9543158069381));
#187131=CARTESIAN_POINT('Ctrl Pts',(47.9830729139868,-34.6313285282533,
39.9636935671387));
#187132=CARTESIAN_POINT('Ctrl Pts',(47.9735885825119,-34.6273621044917,
39.9729968320983));
#187133=CARTESIAN_POINT('Ctrl Pts',(47.9637494987672,-34.6241270221289,
39.9821731151329));
#187134=CARTESIAN_POINT('Ctrl Pts',(47.9544484832181,-34.6210688561309,
39.9908475764345));
#187135=CARTESIAN_POINT('Ctrl Pts',(47.9448295964483,-34.6186639474976,
39.9994093733839));
#187136=CARTESIAN_POINT('Ctrl Pts',(47.9349076763732,-34.6170045862117,
40.0077966115834));
#187137=CARTESIAN_POINT('Ctrl Pts',(47.9257697544367,-34.6154763423053,
40.0155211172588));
#187138=CARTESIAN_POINT('Ctrl Pts',(47.9163742511081,-34.6145804463108,
40.0230979941014));
#187139=CARTESIAN_POINT('Ctrl Pts',(47.906736439066,-34.614426945342,40.0304554104741));
#187140=CARTESIAN_POINT('Ctrl Pts',(47.9038626380665,-34.6143811744517,
40.0326492435176));
#187141=CARTESIAN_POINT('Ctrl Pts',(47.9009673483056,-34.6144016870564,
40.0348233715058));
#187142=CARTESIAN_POINT('Ctrl Pts',(47.8980511519205,-34.6144921419175,
40.0369753512355));
#187143=CARTESIAN_POINT('Ctrl Pts',(47.8951647518766,-34.6145816725527,
40.0391053430351));
#187144=CARTESIAN_POINT('Ctrl Pts',(47.8922608568399,-34.6147393566952,
40.041211089324));
#187145=CARTESIAN_POINT('Ctrl Pts',(47.8893433277785,-34.6149683234595,
40.0432881154904));
#187146=CARTESIAN_POINT('Ctrl Pts',(47.8891404485133,-34.6149842453605,
40.043432547828));
#187147=CARTESIAN_POINT('Ctrl Pts',(47.8889374970514,-34.6150005017596,
40.0435768364421));
#187148=CARTESIAN_POINT('Ctrl Pts',(47.8887344737214,-34.6150170939189,
40.0437209807855));
#187149=CARTESIAN_POINT('Ctrl Pts',(47.8798331871998,-34.615744554967,40.050040796842));
#187150=CARTESIAN_POINT('Ctrl Pts',(47.8708080647647,-34.6171603320593,
40.0560490279345));
#187151=CARTESIAN_POINT('Ctrl Pts',(47.8617555581812,-34.6193291901736,
40.0616647108616));
#187152=CARTESIAN_POINT('Ctrl Pts',(47.8533170487304,-34.6213509428811,
40.0668995033487));
#187153=CARTESIAN_POINT('Ctrl Pts',(47.8448540540096,-34.6240275231021,
40.0717933267483));
#187154=CARTESIAN_POINT('Ctrl Pts',(47.836466636969,-34.6274308957718,40.0762460303074));
#187155=CARTESIAN_POINT('Ctrl Pts',(47.8333984113058,-34.6286758935245,
40.0778748868749));
#187156=CARTESIAN_POINT('Ctrl Pts',(47.8303405713848,-34.6300183184511,
40.0794443522248));
#187157=CARTESIAN_POINT('Ctrl Pts',(47.827299095813,-34.6314622582449,40.0809482021492));
#187158=CARTESIAN_POINT('Ctrl Pts',(47.8265677225446,-34.6318094775275,
40.0813098278168));
#187159=CARTESIAN_POINT('Ctrl Pts',(47.8258370084447,-34.6321630753104,
40.0816679525672));
#187160=CARTESIAN_POINT('Ctrl Pts',(47.8251070891649,-34.6325230544376,
40.082022419258));
#187161=CARTESIAN_POINT('Ctrl Pts',(47.8243999798625,-34.6328717842171,
40.0823658088648));
#187162=CARTESIAN_POINT('Ctrl Pts',(47.8236936164943,-34.633226502718,40.0827057654617));
#187163=CARTESIAN_POINT('Ctrl Pts',(47.822988124598,-34.6335872094465,40.0830421470151));
#187164=CARTESIAN_POINT('Ctrl Pts',(47.8152586455547,-34.6375391685162,
40.0867275956807));
#187165=CARTESIAN_POINT('Ctrl Pts',(47.8076288798881,-34.6422128973065,
40.0899823432032));
#187166=CARTESIAN_POINT('Ctrl Pts',(47.8002860619008,-34.6475865476014,
40.0926299529357));
#187167=CARTESIAN_POINT('Ctrl Pts',(47.7972407764157,-34.6498151605499,
40.0937279956085));
#187168=CARTESIAN_POINT('Ctrl Pts',(47.794244830465,-34.6521637338115,40.0947220371803));
#187169=CARTESIAN_POINT('Ctrl Pts',(47.7913110614419,-34.6546289547338,
40.0956014538692));
#187170=CARTESIAN_POINT('Ctrl Pts',(47.7863072126526,-34.6588336459111,
40.097101390674));
#187171=CARTESIAN_POINT('Ctrl Pts',(47.7814867201294,-34.6633779280159,
40.0982667904316));
#187172=CARTESIAN_POINT('Ctrl Pts',(47.7769196237425,-34.6682420184009,
40.0990539325582));
#187173=CARTESIAN_POINT('Ctrl Pts',(47.774636075549,-34.6706740635933,40.0994475036216));
#187174=CARTESIAN_POINT('Ctrl Pts',(47.7724170058821,-34.6731869650546,
40.0997467259952));
#187175=CARTESIAN_POINT('Ctrl Pts',(47.7702712352612,-34.6757782448035,
40.0999473488896));
#187176=CARTESIAN_POINT('Ctrl Pts',(47.7681254646404,-34.6783695245524,
40.100147971784));
#187177=CARTESIAN_POINT('Ctrl Pts',(47.7660530039194,-34.681039138237,40.10025));
#187178=CARTESIAN_POINT('Ctrl Pts',(47.7640607692763,-34.6837837831347,
40.10025));
#187179=CARTESIAN_POINT('Origin',(43.2882232241948,-38.997398704332,39.92499));
#187180=CARTESIAN_POINT('Ctrl Pts',(46.435582879267,-42.0671296588096,39.92499));
#187181=CARTESIAN_POINT('Ctrl Pts',(46.4434678907493,-42.0742293550377,
39.9348354642017));
#187182=CARTESIAN_POINT('Ctrl Pts',(46.4518896956739,-42.0806858315473,
39.9446440828457));
#187183=CARTESIAN_POINT('Ctrl Pts',(46.4607957007316,-42.0864721532159,
39.9543641760331));
#187184=CARTESIAN_POINT('Ctrl Pts',(46.4694123136567,-42.0920704538855,
39.9637684240712));
#187185=CARTESIAN_POINT('Ctrl Pts',(46.4784832882808,-42.0970420880505,
39.9730909636396));
#187186=CARTESIAN_POINT('Ctrl Pts',(46.4879887958175,-42.1013257711388,
39.9822808977141));
#187187=CARTESIAN_POINT('Ctrl Pts',(46.4969804206317,-42.1053778715664,
39.9909740094651));
#187188=CARTESIAN_POINT('Ctrl Pts',(46.5063617095226,-42.1088147776121,
39.9995492765003));
#187189=CARTESIAN_POINT('Ctrl Pts',(46.5161273793226,-42.1115441100121,
40.0079462328696));
#187190=CARTESIAN_POINT('Ctrl Pts',(46.5251222674796,-42.1140580225429,
40.0156804369692));
#187191=CARTESIAN_POINT('Ctrl Pts',(46.5344438074312,-42.1159717447011,
40.0232638017425));
#187192=CARTESIAN_POINT('Ctrl Pts',(46.5440884908184,-42.1171748456134,
40.030625726997));
#187193=CARTESIAN_POINT('Ctrl Pts',(46.5468860468469,-42.1175238194548,
40.0327611416654));
#187194=CARTESIAN_POINT('Ctrl Pts',(46.5497107674229,-42.117812736298,40.0348777427272));
#187195=CARTESIAN_POINT('Ctrl Pts',(46.5525624800842,-42.1180382068975,
40.0369733168701));
#187196=CARTESIAN_POINT('Ctrl Pts',(46.5556539199574,-42.1182826315239,
40.039245053974));
#187197=CARTESIAN_POINT('Ctrl Pts',(46.5587726948499,-42.1184532289193,
40.041487875195));
#187198=CARTESIAN_POINT('Ctrl Pts',(46.5619176830194,-42.118546158468,40.0436985701601));
#187199=CARTESIAN_POINT('Ctrl Pts',(46.5705491277288,-42.1188012043435,
40.0497658398386));
#187200=CARTESIAN_POINT('Ctrl Pts',(46.5793682643811,-42.1184278543821,
40.0555581699984));
#187201=CARTESIAN_POINT('Ctrl Pts',(46.5882835699004,-42.1173773384967,
40.0609828468885));
#187202=CARTESIAN_POINT('Ctrl Pts',(46.5964405904276,-42.1164161734954,
40.0659461317306));
#187203=CARTESIAN_POINT('Ctrl Pts',(46.6046697328848,-42.1148801579475,
40.070603998071));
#187204=CARTESIAN_POINT('Ctrl Pts',(46.6129145292195,-42.1127009621825,
40.0748843180608));
#187205=CARTESIAN_POINT('Ctrl Pts',(46.6169643462458,-42.1116305483415,
40.0769867972573));
#187206=CARTESIAN_POINT('Ctrl Pts',(46.6210176421369,-42.1104045383077,
40.0789976708176));
#187207=CARTESIAN_POINT('Ctrl Pts',(46.6250654385592,-42.1090123875508,
40.08090504915));
#187208=CARTESIAN_POINT('Ctrl Pts',(46.6258334685044,-42.1087482405044,
40.0812669556105));
#187209=CARTESIAN_POINT('Ctrl Pts',(46.6266015422614,-42.1084776383328,
40.0816253922032));
#187210=CARTESIAN_POINT('Ctrl Pts',(46.6273695213206,-42.1082005605485,
40.0819801989139));
#187211=CARTESIAN_POINT('Ctrl Pts',(46.6281135010342,-42.107932141445,40.0823239179149));
#187212=CARTESIAN_POINT('Ctrl Pts',(46.6288573918596,-42.10765764515,40.0826642303498));
#187213=CARTESIAN_POINT('Ctrl Pts',(46.6296010653159,-42.107377055908,40.0830009916099));
#187214=CARTESIAN_POINT('Ctrl Pts',(46.6377054654047,-42.1043192521647,
40.086670946431));
#187215=CARTESIAN_POINT('Ctrl Pts',(46.6457892400063,-42.1005354505678,
40.0899175831874));
#187216=CARTESIAN_POINT('Ctrl Pts',(46.6536619390749,-42.0960238460778,
40.0925642067057));
#187217=CARTESIAN_POINT('Ctrl Pts',(46.6569866287793,-42.0941185674855,
40.0936818922525));
#187218=CARTESIAN_POINT('Ctrl Pts',(46.6602736399407,-42.0920839261387,
40.0946930094789));
#187219=CARTESIAN_POINT('Ctrl Pts',(46.6635089796843,-42.0899216923179,
40.0955863397546));
#187220=CARTESIAN_POINT('Ctrl Pts',(46.6689572109695,-42.0862805445926,
40.0970906856166));
#187221=CARTESIAN_POINT('Ctrl Pts',(46.6742564366675,-42.0822770520157,
40.0982599215483));
#187222=CARTESIAN_POINT('Ctrl Pts',(46.679333290145,-42.0779224130572,40.0990497370454));
#187223=CARTESIAN_POINT('Ctrl Pts',(46.6806025035144,-42.0768337533176,
40.0992471909196));
#187224=CARTESIAN_POINT('Ctrl Pts',(46.6818576549905,-42.0757229796946,
40.0994209989363));
#187225=CARTESIAN_POINT('Ctrl Pts',(46.683097373911,-42.0745900553976,40.0995705982975));
#187226=CARTESIAN_POINT('Ctrl Pts',(46.6849569522919,-42.0728906689521,
40.0997949973393));
#187227=CARTESIAN_POINT('Ctrl Pts',(46.686781786976,-42.0711414461003,40.0999649129781));
#187228=CARTESIAN_POINT('Ctrl Pts',(46.6885684866733,-42.0693433991608,
40.1000786629733));
#187229=CARTESIAN_POINT('Ctrl Pts',(46.6903551863705,-42.0675453522213,
40.1001924129685));
#187230=CARTESIAN_POINT('Ctrl Pts',(46.692103753135,-42.0656984926165,40.10025));
#187231=CARTESIAN_POINT('Ctrl Pts',(46.6938111422604,-42.0638038389701,
40.10025));
#187232=CARTESIAN_POINT('Ctrl Pts',(43.8565665267056,-39.5091373124623,
40.10025));
#187233=CARTESIAN_POINT('Ctrl Pts',(43.8507890749204,-39.5155480799606,
40.10025));
#187234=CARTESIAN_POINT('Ctrl Pts',(43.8455908828145,-39.5223801852474,
40.099578633424));
#187235=CARTESIAN_POINT('Ctrl Pts',(43.8409939475736,-39.5294841269579,
40.0983063763364));
#187236=CARTESIAN_POINT('Ctrl Pts',(43.8380247990813,-39.5340725443955,
40.097484628799));
#187237=CARTESIAN_POINT('Ctrl Pts',(43.8353056940458,-39.5387738681337,
40.0964130309337));
#187238=CARTESIAN_POINT('Ctrl Pts',(43.8328343017437,-39.5435446222363,
40.0951176960924));
#187239=CARTESIAN_POINT('Ctrl Pts',(43.8295586128169,-39.5498679835144,
40.0934008039614));
#187240=CARTESIAN_POINT('Ctrl Pts',(43.8267236865061,-39.5563148866443,
40.0912909372156));
#187241=CARTESIAN_POINT('Ctrl Pts',(43.8243293609623,-39.562795265034,40.0888630467851));
#187242=CARTESIAN_POINT('Ctrl Pts',(43.8231321981904,-39.5660354542288,
40.0876491015699));
#187243=CARTESIAN_POINT('Ctrl Pts',(43.8220450509626,-39.5692841591686,
40.0863558569271));
#187244=CARTESIAN_POINT('Ctrl Pts',(43.8210669472518,-39.5725311673655,
40.0849936342771));
#187245=CARTESIAN_POINT('Ctrl Pts',(43.8205778953964,-39.574154671464,40.0843125229521));
#187246=CARTESIAN_POINT('Ctrl Pts',(43.8201160933895,-39.5757777635547,
40.0836141747074));
#187247=CARTESIAN_POINT('Ctrl Pts',(43.8196813503779,-39.5773992434495,
40.0828999161609));
#187248=CARTESIAN_POINT('Ctrl Pts',(43.8195726646249,-39.5778046134232,
40.0827213515243));
#187249=CARTESIAN_POINT('Ctrl Pts',(43.8194656698239,-39.578209882893,40.0825417925842));
#187250=CARTESIAN_POINT('Ctrl Pts',(43.8193603625175,-39.5786150336267,
40.0823612602361));
#187251=CARTESIAN_POINT('Ctrl Pts',(43.8190444405985,-39.5798304858276,
40.0818196631917));
#187252=CARTESIAN_POINT('Ctrl Pts',(43.8187437073123,-39.581044868119,40.0812693052021));
#187253=CARTESIAN_POINT('Ctrl Pts',(43.8184580587802,-39.5822576997161,
40.0807107531875));
#187254=CARTESIAN_POINT('Ctrl Pts',(43.8164459874034,-39.5908007288813,
40.0767763849181));
#187255=CARTESIAN_POINT('Ctrl Pts',(43.8151322889031,-39.5992865061389,
40.0724140586137));
#187256=CARTESIAN_POINT('Ctrl Pts',(43.8144227306311,-39.6076412948836,
40.0677221223767));
#187257=CARTESIAN_POINT('Ctrl Pts',(43.8140785956359,-39.6116933583964,
40.065446538372));
#187258=CARTESIAN_POINT('Ctrl Pts',(43.8138769687219,-39.6157150281161,
40.0630928000679));
#187259=CARTESIAN_POINT('Ctrl Pts',(43.8138093098903,-39.6196997093542,
40.0606689262479));
#187260=CARTESIAN_POINT('Ctrl Pts',(43.8137057289464,-39.6257999779282,
40.0569581447806));
#187261=CARTESIAN_POINT('Ctrl Pts',(43.8139151128799,-39.6318101761581,
40.0530843804606));
#187262=CARTESIAN_POINT('Ctrl Pts',(43.8144090029878,-39.637694021932,40.0490800251458));
#187263=CARTESIAN_POINT('Ctrl Pts',(43.8146383681089,-39.6404265103485,
40.0472203818218));
#187264=CARTESIAN_POINT('Ctrl Pts',(43.8149288459967,-39.6431316855282,
40.0453323608818));
#187265=CARTESIAN_POINT('Ctrl Pts',(43.8152787628653,-39.6458055463961,
40.0434201572162));
#187266=CARTESIAN_POINT('Ctrl Pts',(43.8153055826145,-39.6460104872961,
40.0432735943397));
#187267=CARTESIAN_POINT('Ctrl Pts',(43.8153327221694,-39.6462152612034,
40.0431268995707));
#187268=CARTESIAN_POINT('Ctrl Pts',(43.8153601802954,-39.6464198673375,
40.0429800745037));
#187269=CARTESIAN_POINT('Ctrl Pts',(43.8157458841823,-39.6492939666537,
40.0409176249753));
#187270=CARTESIAN_POINT('Ctrl Pts',(43.8161965332334,-39.6521348180506,
40.0388310783332));
#187271=CARTESIAN_POINT('Ctrl Pts',(43.816707563491,-39.6549389970088,40.036725739981));
#187272=CARTESIAN_POINT('Ctrl Pts',(43.8185400271111,-39.664994284047,40.0291763710714));
#187273=CARTESIAN_POINT('Ctrl Pts',(43.8211611138372,-39.6746561192254,
40.0213310894587));
#187274=CARTESIAN_POINT('Ctrl Pts',(43.8244418968104,-39.6839173731645,
40.0132837551308));
#187275=CARTESIAN_POINT('Ctrl Pts',(43.8280471477141,-39.694094560868,40.004440543131));
#187276=CARTESIAN_POINT('Ctrl Pts',(43.8324491002319,-39.7037886794691,
39.9953528710582));
#187277=CARTESIAN_POINT('Ctrl Pts',(43.8375295667881,-39.7129876499629,
39.9861103629532));
#187278=CARTESIAN_POINT('Ctrl Pts',(43.8430151956457,-39.7229202294697,
39.9761307737529));
#187279=CARTESIAN_POINT('Ctrl Pts',(43.8492922888431,-39.7322766233325,
39.965969693598));
#187280=CARTESIAN_POINT('Ctrl Pts',(43.8562669044119,-39.7410245486315,
39.9557128217471));
#187281=CARTESIAN_POINT('Ctrl Pts',(43.8631830101214,-39.7496990878244,
39.9455419945137));
#187282=CARTESIAN_POINT('Ctrl Pts',(43.870786081907,-39.7577762496646,39.9352756289329));
#187283=CARTESIAN_POINT('Ctrl Pts',(43.8790236240219,-39.7651933658999,
39.92499));
#187284=CARTESIAN_POINT('Origin',(0.0101975504409105,0.0113255271402792,
39.92499));
#187285=CARTESIAN_POINT('Ctrl Pts',(46.7142062431422,-42.0411527846896,
40.10025));
#187286=CARTESIAN_POINT('Ctrl Pts',(46.7199506919422,-42.0347675597394,
40.10025));
#187287=CARTESIAN_POINT('Ctrl Pts',(46.7251107020204,-42.0279592142787,
40.0995859581842));
#187288=CARTESIAN_POINT('Ctrl Pts',(46.7296675019384,-42.0208774479599,
40.0983275959623));
#187289=CARTESIAN_POINT('Ctrl Pts',(46.7325790801588,-42.0163525364107,
40.097523562407));
#187290=CARTESIAN_POINT('Ctrl Pts',(46.7352451892137,-42.0117164852004,
40.0964777059492));
#187291=CARTESIAN_POINT('Ctrl Pts',(46.7376689638752,-42.0070114066747,
40.0952149915961));
#187292=CARTESIAN_POINT('Ctrl Pts',(46.7409769299535,-42.0005899185698,
40.0934916398701));
#187293=CARTESIAN_POINT('Ctrl Pts',(46.743827608742,-41.9940383480778,40.091364392163));
#187294=CARTESIAN_POINT('Ctrl Pts',(46.7462229640888,-41.9874523371581,
40.0889118607713));
#187295=CARTESIAN_POINT('Ctrl Pts',(46.7474206417622,-41.9841593316983,
40.0876855950754));
#187296=CARTESIAN_POINT('Ctrl Pts',(46.7485046297347,-41.9808575622224,
40.0863782327526));
#187297=CARTESIAN_POINT('Ctrl Pts',(46.7494761782933,-41.9775578801518,
40.0850006373333));
#187298=CARTESIAN_POINT('Ctrl Pts',(46.7499619525726,-41.9759080391166,
40.0843118396237));
#187299=CARTESIAN_POINT('Ctrl Pts',(46.7504196286881,-41.9742587070256,
40.0836054919164));
#187300=CARTESIAN_POINT('Ctrl Pts',(46.7508494364812,-41.972611159284,40.0828829920417));
#187301=CARTESIAN_POINT('Ctrl Pts',(46.7509568884295,-41.9721992723486,
40.0827023670731));
#187302=CARTESIAN_POINT('Ctrl Pts',(46.7510625988575,-41.9717874966607,
40.0825207326932));
#187303=CARTESIAN_POINT('Ctrl Pts',(46.7511665718606,-41.9713758515958,
40.0823381109275));
#187304=CARTESIAN_POINT('Ctrl Pts',(46.7514784908699,-41.9701409164012,
40.0817902456303));
#187305=CARTESIAN_POINT('Ctrl Pts',(46.7517747718024,-41.9689071581769,
40.0812334935553));
#187306=CARTESIAN_POINT('Ctrl Pts',(46.7520555364232,-41.9676750878619,
40.0806684524227));
#187307=CARTESIAN_POINT('Ctrl Pts',(46.7539957941553,-41.9591607175417,
40.0767636676138));
#187308=CARTESIAN_POINT('Ctrl Pts',(46.7552464720207,-41.9507055072923,
40.0724404510892));
#187309=CARTESIAN_POINT('Ctrl Pts',(46.7559027543579,-41.9423805287177,
40.0677949937415));
#187310=CARTESIAN_POINT('Ctrl Pts',(46.7562289248781,-41.9382430372173,
40.065486214191));
#187311=CARTESIAN_POINT('Ctrl Pts',(46.7564078446195,-41.9341372814972,
40.0630972003218));
#187312=CARTESIAN_POINT('Ctrl Pts',(46.7564487173143,-41.9300700339484,
40.0606363359906));
#187313=CARTESIAN_POINT('Ctrl Pts',(46.7565388885838,-41.9210970783569,
40.0552073017123));
#187314=CARTESIAN_POINT('Ctrl Pts',(46.7559695796225,-41.9123126321654,
40.0494204304519));
#187315=CARTESIAN_POINT('Ctrl Pts',(46.7548061840817,-41.9038465062684,
40.0434049749851));
#187316=CARTESIAN_POINT('Ctrl Pts',(46.7543811810194,-41.9007537237148,
40.0412074532442));
#187317=CARTESIAN_POINT('Ctrl Pts',(46.7538836816023,-41.8976992635446,
40.0389814735788));
#187318=CARTESIAN_POINT('Ctrl Pts',(46.7533184435777,-41.8946854937102,
40.0367321210017));
#187319=CARTESIAN_POINT('Ctrl Pts',(46.7514198688647,-41.8845625597432,
40.0291767837139));
#187320=CARTESIAN_POINT('Ctrl Pts',(46.7487367327314,-41.8748360802677,
40.0213235332573));
#187321=CARTESIAN_POINT('Ctrl Pts',(46.7453971060007,-41.8655137786579,
40.0132649215853));
#187322=CARTESIAN_POINT('Ctrl Pts',(46.7417264606188,-41.8552674648896,
40.0044075527525));
#187323=CARTESIAN_POINT('Ctrl Pts',(46.7372626589216,-41.8455087367158,
39.995301625371));
#187324=CARTESIAN_POINT('Ctrl Pts',(46.7321227530968,-41.8362508575454,
39.9860353422346));
#187325=CARTESIAN_POINT('Ctrl Pts',(46.726586854296,-41.8262797250103,39.9760551582681));
#187326=CARTESIAN_POINT('Ctrl Pts',(46.7202662104757,-41.8168884800889,
39.965887973814));
#187327=CARTESIAN_POINT('Ctrl Pts',(46.7132528291638,-41.80811151121,39.9556174643237));
#187328=CARTESIAN_POINT('Ctrl Pts',(46.7063341521798,-41.7994530610458,
39.9454856413893));
#187329=CARTESIAN_POINT('Ctrl Pts',(46.6987402031259,-41.7913915075188,
39.9352519465107));
#187330=CARTESIAN_POINT('Ctrl Pts',(46.6905216402897,-41.7839914803027,
39.92499));
#187331=CARTESIAN_POINT('Ctrl Pts',(44.1339623850447,-39.4820551873931,
39.92499));
#187332=CARTESIAN_POINT('Ctrl Pts',(44.1260971752941,-39.4749733207244,
39.9348107241729));
#187333=CARTESIAN_POINT('Ctrl Pts',(44.1177016730286,-39.4685372764351,
39.9446038383183));
#187334=CARTESIAN_POINT('Ctrl Pts',(44.1088266671078,-39.4627751762741,
39.9543158069405));
#187335=CARTESIAN_POINT('Ctrl Pts',(44.100257068034,-39.457211361597,39.9636935671416));
#187336=CARTESIAN_POINT('Ctrl Pts',(44.0912392968991,-39.4522752837255,
39.9729968321017));
#187337=CARTESIAN_POINT('Ctrl Pts',(44.0817922708719,-39.4480294591785,
39.9821731151368));
#187338=CARTESIAN_POINT('Ctrl Pts',(44.0728618726509,-39.4440158252717,
39.9908475764388));
#187339=CARTESIAN_POINT('Ctrl Pts',(44.0635470605524,-39.4406186435271,
39.9994093733886));
#187340=CARTESIAN_POINT('Ctrl Pts',(44.0538529442782,-39.4379312493381,
40.0077966115884));
#187341=CARTESIAN_POINT('Ctrl Pts',(44.0449248258207,-39.4354562043743,
40.015521117264));
#187342=CARTESIAN_POINT('Ctrl Pts',(44.0356744386734,-39.4335831186675,
40.0230979941068));
#187343=CARTESIAN_POINT('Ctrl Pts',(44.0261054687939,-39.4324230329113,
40.0304554104797));
#187344=CARTESIAN_POINT('Ctrl Pts',(44.0232521951402,-39.432077118757,40.0326492435213));
#187345=CARTESIAN_POINT('Ctrl Pts',(44.020370621931,-39.4317948788024,40.0348233715076));
#187346=CARTESIAN_POINT('Ctrl Pts',(44.0174609456696,-39.4315800126157,
40.0369753512355));
#187347=CARTESIAN_POINT('Ctrl Pts',(44.0145809991274,-39.4313673418318,
40.0391053430352));
#187348=CARTESIAN_POINT('Ctrl Pts',(44.0116765294504,-39.4312206224783,
40.041211089324));
#187349=CARTESIAN_POINT('Ctrl Pts',(44.0087510493745,-39.4311433701095,
40.0432881154904));
#187350=CARTESIAN_POINT('Ctrl Pts',(44.0085476172113,-39.4311379981308,
40.043432547828));
#187351=CARTESIAN_POINT('Ctrl Pts',(44.0083440782824,-39.4311329512712,
40.0435768364421));
#187352=CARTESIAN_POINT('Ctrl Pts',(44.0081404327825,-39.4311282308202,
40.0437209807855));
#187353=CARTESIAN_POINT('Ctrl Pts',(43.9992118680544,-39.4309212689594,
40.050040796842));
#187354=CARTESIAN_POINT('Ctrl Pts',(43.9900881971805,-39.4313859080977,
40.0560490279345));
#187355=CARTESIAN_POINT('Ctrl Pts',(43.9808585737696,-39.4325966403784,
40.0616647108615));
#187356=CARTESIAN_POINT('Ctrl Pts',(43.9722549606529,-39.4337252532879,
40.0668995033487));
#187357=CARTESIAN_POINT('Ctrl Pts',(43.9635585482853,-39.4355025470896,
40.0717933267483));
#187358=CARTESIAN_POINT('Ctrl Pts',(43.9548613290778,-39.4380105519136,
40.0762460303074));
#187359=CARTESIAN_POINT('Ctrl Pts',(43.9516797737739,-39.4389280125248,
40.0778748868749));
#187360=CARTESIAN_POINT('Ctrl Pts',(43.9484983634053,-39.4399434521994,
40.0794443522248));
#187361=CARTESIAN_POINT('Ctrl Pts',(43.9453226165472,-39.4410615611723,
40.0809482021492));
#187362=CARTESIAN_POINT('Ctrl Pts',(43.9445589555201,-39.4413304290276,
40.0813098278169));
#187363=CARTESIAN_POINT('Ctrl Pts',(43.9437952833156,-39.4416057093429,
40.0816679525673));
#187364=CARTESIAN_POINT('Ctrl Pts',(43.943031734545,-39.4418874191261,40.0820224192581));
#187365=CARTESIAN_POINT('Ctrl Pts',(43.9422920466734,-39.4421603254786,
40.0823658088649));
#187366=CARTESIAN_POINT('Ctrl Pts',(43.9415524746579,-39.4424392657171,
40.0827057654617));
#187367=CARTESIAN_POINT('Ctrl Pts',(43.9408131433999,-39.4427242524725,
40.0830421470151));
#187368=CARTESIAN_POINT('Ctrl Pts',(43.9327129150435,-39.4458466117306,
40.0867275956805));
#187369=CARTESIAN_POINT('Ctrl Pts',(43.9246364083438,-39.4496972096651,
40.0899823432029));
#187370=CARTESIAN_POINT('Ctrl Pts',(43.9167721156746,-39.4542738890609,
40.0926299529354));
#187371=CARTESIAN_POINT('Ctrl Pts',(43.9135105590949,-39.4561719744227,
40.0937279956083));
#187372=CARTESIAN_POINT('Ctrl Pts',(43.9102855324952,-39.4581945203283,
40.0947220371802));
#187373=CARTESIAN_POINT('Ctrl Pts',(43.9071101492109,-39.4603395741451,
40.0956014538693));
#187374=CARTESIAN_POINT('Ctrl Pts',(43.9016942021215,-39.4639981869597,
40.097101390674));
#187375=CARTESIAN_POINT('Ctrl Pts',(43.8964251099356,-39.4680136963361,
40.0982667904316));
#187376=CARTESIAN_POINT('Ctrl Pts',(43.8913745966875,-39.472373749158,40.0990539325583));
#187377=CARTESIAN_POINT('Ctrl Pts',(43.8888493400634,-39.474553775569,40.0994475036216));
#187378=CARTESIAN_POINT('Ctrl Pts',(43.8863797569642,-39.476820955151,40.0997467259952));
#187379=CARTESIAN_POINT('Ctrl Pts',(43.8839748786093,-39.4791737454928,
40.0999473488896));
#187380=CARTESIAN_POINT('Ctrl Pts',(43.8815700002543,-39.4815265358346,
40.100147971784));
#187381=CARTESIAN_POINT('Ctrl Pts',(43.879229842074,-39.4839648939618,40.10025));
#187382=CARTESIAN_POINT('Ctrl Pts',(43.8769616275874,-39.4864862581817,
40.10025));
#187383=CARTESIAN_POINT('Origin',(38.9747476500513,-43.3086183250767,39.92499));
#187384=CARTESIAN_POINT('Ctrl Pts',(41.7839914803026,-46.6905216402898,
39.92499));
#187385=CARTESIAN_POINT('Ctrl Pts',(41.7910911765308,-46.6984066517723,
39.9348354642023));
#187386=CARTESIAN_POINT('Ctrl Pts',(41.7987919603593,-46.7057080773549,
39.9446440828467));
#187387=CARTESIAN_POINT('Ctrl Pts',(41.8070443420777,-46.7123936319706,
39.9543641760345));
#187388=CARTESIAN_POINT('Ctrl Pts',(41.81502857053,-46.7188619458711,39.9637684240729));
#187389=CARTESIAN_POINT('Ctrl Pts',(41.8235301761271,-46.7247545199419,
39.9730909636415));
#187390=CARTESIAN_POINT('Ctrl Pts',(41.8325358446889,-46.7300083326616,
39.9822808977162));
#187391=CARTESIAN_POINT('Ctrl Pts',(41.8410546526111,-46.7349781159832,
39.9909740094673));
#187392=CARTESIAN_POINT('Ctrl Pts',(41.8500252953129,-46.7393768060093,
39.9995492765025));
#187393=CARTESIAN_POINT('Ctrl Pts',(41.8594521748307,-46.7431119772979,
40.007946232872));
#187394=CARTESIAN_POINT('Ctrl Pts',(41.868135012636,-46.746552340189,40.0156804369717));
#187395=CARTESIAN_POINT('Ctrl Pts',(41.8772054497804,-46.7494299450235,
40.0232638017451));
#187396=CARTESIAN_POINT('Ctrl Pts',(41.8866715402936,-46.7516345991562,
40.0306257269996));
#187397=CARTESIAN_POINT('Ctrl Pts',(41.8894172933171,-46.7522740855146,
40.0327611416671));
#187398=CARTESIAN_POINT('Ctrl Pts',(41.8921963397434,-46.7528566833418,
40.034877742728));
#187399=CARTESIAN_POINT('Ctrl Pts',(41.8950088623279,-46.7533790039317,
40.03697331687));
#187400=CARTESIAN_POINT('Ctrl Pts',(41.8980578176395,-46.7539452330336,
40.039245053974));
#187401=CARTESIAN_POINT('Ctrl Pts',(41.9011416752732,-46.7544408966254,
40.041487875195));
#187402=CARTESIAN_POINT('Ctrl Pts',(41.9042597210856,-46.7548620578767,
40.04369857016));
#187403=CARTESIAN_POINT('Ctrl Pts',(41.9128172222843,-46.7560179382354,
40.0497658398386));
#187404=CARTESIAN_POINT('Ctrl Pts',(41.921627072481,-46.7565684843259,40.0555581699984));
#187405=CARTESIAN_POINT('Ctrl Pts',(41.9306033478349,-46.7564556264619,
40.0609828468885));
#187406=CARTESIAN_POINT('Ctrl Pts',(41.9388161524506,-46.7563523676436,
40.0659461317305));
#187407=CARTESIAN_POINT('Ctrl Pts',(41.9471607721489,-46.7556849461647,
40.0706039980708));
#187408=CARTESIAN_POINT('Ctrl Pts',(41.9555881906109,-46.7543795041529,
40.0748843180606));
#187409=CARTESIAN_POINT('Ctrl Pts',(41.9597277110299,-46.7537382753012,
40.0769867972572));
#187410=CARTESIAN_POINT('Ctrl Pts',(41.9638869554869,-46.7529426662693,
40.0789976708176));
#187411=CARTESIAN_POINT('Ctrl Pts',(41.9680580970364,-46.7519812517995,
40.08090504915));
#187412=CARTESIAN_POINT('Ctrl Pts',(41.968849530518,-46.7517988327682,40.0812669556105));
#187413=CARTESIAN_POINT('Ctrl Pts',(41.9696416823158,-46.7516099985531,
40.0816253922033));
#187414=CARTESIAN_POINT('Ctrl Pts',(41.9704344168203,-46.7514147143008,
40.081980198914));
#187415=CARTESIAN_POINT('Ctrl Pts',(41.9712023783716,-46.7512255326814,
40.0823239179149));
#187416=CARTESIAN_POINT('Ctrl Pts',(41.9719708867612,-46.7510302978707,
40.0826642303499));
#187417=CARTESIAN_POINT('Ctrl Pts',(41.9727398158587,-46.7508289807694,
40.08300099161));
#187418=CARTESIAN_POINT('Ctrl Pts',(41.9811194467227,-46.7486350684818,
40.0866709464313));
#187419=CARTESIAN_POINT('Ctrl Pts',(41.9895544525281,-46.7457169794821,
40.0899175831879));
#187420=CARTESIAN_POINT('Ctrl Pts',(41.9978556152123,-46.7420530111686,
40.0925642067063));
#187421=CARTESIAN_POINT('Ctrl Pts',(42.0013612477613,-46.7405056945977,
40.0936818922528));
#187422=CARTESIAN_POINT('Ctrl Pts',(42.0048429302643,-46.7388257854547,
40.0946930094791));
#187423=CARTESIAN_POINT('Ctrl Pts',(42.0082865614562,-46.737013581669,40.0955863397546));
#187424=CARTESIAN_POINT('Ctrl Pts',(42.0140855503365,-46.7339618757756,
40.0970906856166));
#187425=CARTESIAN_POINT('Ctrl Pts',(42.0197742252486,-46.7305342346687,
40.0982599215483));
#187426=CARTESIAN_POINT('Ctrl Pts',(42.0252784509104,-46.7267341265709,
40.0990497370453));
#187427=CARTESIAN_POINT('Ctrl Pts',(42.0266545073258,-46.7257840995464,
40.0992471909196));
#187428=CARTESIAN_POINT('Ctrl Pts',(42.0280188904106,-46.7248106099125,
40.0994209989363));
#187429=CARTESIAN_POINT('Ctrl Pts',(42.029370240857,-46.7238134778069,40.0995705982975));
#187430=CARTESIAN_POINT('Ctrl Pts',(42.0313972665264,-46.7223177796486,
40.0997949973393));
#187431=CARTESIAN_POINT('Ctrl Pts',(42.0333949481518,-46.7207688863878,
40.0999649129781));
#187432=CARTESIAN_POINT('Ctrl Pts',(42.0353598072045,-46.7191674503111,
40.1000786629733));
#187433=CARTESIAN_POINT('Ctrl Pts',(42.0373246662573,-46.7175660142344,
40.1001924129685));
#187434=CARTESIAN_POINT('Ctrl Pts',(42.0392567035862,-46.7159120469163,
40.10025));
#187435=CARTESIAN_POINT('Ctrl Pts',(42.0411527846894,-46.7142062431423,
40.10025));
#187436=CARTESIAN_POINT('Ctrl Pts',(39.4864862581816,-43.8769616275875,
40.10025));
#187437=CARTESIAN_POINT('Ctrl Pts',(39.4800703482066,-43.8827333680742,
40.10025));
#187438=CARTESIAN_POINT('Ctrl Pts',(39.4741864828742,-43.8889846873409,
40.0995786334239));
#187439=CARTESIAN_POINT('Ctrl Pts',(39.4688721660153,-43.8955692023392,
40.0983063763362));
#187440=CARTESIAN_POINT('Ctrl Pts',(39.4654396626057,-43.8998221234167,
40.0974846287989));
#187441=CARTESIAN_POINT('Ctrl Pts',(39.4622440309667,-43.9042134689405,
40.0964130309336));
#187442=CARTESIAN_POINT('Ctrl Pts',(39.4592874976153,-43.9086997575132,
40.0951176960923));
#187443=CARTESIAN_POINT('Ctrl Pts',(39.4553687820182,-43.914646076027,40.0934008039614));
#187444=CARTESIAN_POINT('Ctrl Pts',(39.4518755008533,-43.9207613318563,
40.0912909372156));
#187445=CARTESIAN_POINT('Ctrl Pts',(39.4488169076809,-43.9269559348854,
40.0888630467851));
#187446=CARTESIAN_POINT('Ctrl Pts',(39.4472876110947,-43.9300532363999,
40.0876491015698));
#187447=CARTESIAN_POINT('Ctrl Pts',(39.4458668372382,-43.9331705067652,
40.0863558569271));
#187448=CARTESIAN_POINT('Ctrl Pts',(39.4445546869049,-43.9362974878336,
40.084993634277));
#187449=CARTESIAN_POINT('Ctrl Pts',(39.4438986117382,-43.9378609783679,
40.084312522952));
#187450=CARTESIAN_POINT('Ctrl Pts',(39.443269680209,-43.9394269075361,40.0836141747073));
#187451=CARTESIAN_POINT('Ctrl Pts',(39.4426678279634,-43.9409940617755,
40.0828999161609));
#187452=CARTESIAN_POINT('Ctrl Pts',(39.442517364902,-43.9413858503353,40.0827213515242));
#187453=CARTESIAN_POINT('Ctrl Pts',(39.4423685940348,-43.9417777156945,
40.0825417925841));
#187454=CARTESIAN_POINT('Ctrl Pts',(39.4422215138293,-43.9421696393591,
40.082361260236));
#187455=CARTESIAN_POINT('Ctrl Pts',(39.4417802732128,-43.943345410353,40.0818196631917));
#187456=CARTESIAN_POINT('Ctrl Pts',(39.4413542498604,-43.9445217049429,
40.0812693052021));
#187457=CARTESIAN_POINT('Ctrl Pts',(39.4409433907177,-43.9456980341195,
40.0807107531874));
#187458=CARTESIAN_POINT('Ctrl Pts',(39.4380493519682,-43.9539839449479,
40.0767763849181));
#187459=CARTESIAN_POINT('Ctrl Pts',(39.4358558447894,-43.9622859173443,
40.0724140586137));
#187460=CARTESIAN_POINT('Ctrl Pts',(39.4342768603234,-43.9705207686462,
40.0677221223768));
#187461=CARTESIAN_POINT('Ctrl Pts',(39.4335110545637,-43.974514662629,40.0654465383721));
#187462=CARTESIAN_POINT('Ctrl Pts',(39.4328901532274,-43.9784932254699,
40.0630928000679));
#187463=CARTESIAN_POINT('Ctrl Pts',(39.4324063524315,-43.9824490059336,
40.0606689262479));
#187464=CARTESIAN_POINT('Ctrl Pts',(39.4316656872153,-43.9885050294412,
40.0569581447805));
#187465=CARTESIAN_POINT('Ctrl Pts',(39.4312456873368,-43.9945041897572,
40.0530843804605));
#187466=CARTESIAN_POINT('Ctrl Pts',(39.4311218425061,-44.0004074287823,
40.0490800251457));
#187467=CARTESIAN_POINT('Ctrl Pts',(39.4310643283261,-44.0031489235249,
40.0472203818218));
#187468=CARTESIAN_POINT('Ctrl Pts',(39.4310704471411,-44.0058696426791,
40.0453323608818));
#187469=CARTESIAN_POINT('Ctrl Pts',(39.431138952561,-44.0085654321301,40.0434201572162));
#187470=CARTESIAN_POINT('Ctrl Pts',(39.4311442032315,-44.0087720537695,
40.0432735943397));
#187471=CARTESIAN_POINT('Ctrl Pts',(39.4311497894112,-44.0089785427599,
40.0431268995707));
#187472=CARTESIAN_POINT('Ctrl Pts',(39.431155709954,-44.0091848981958,40.0429800745037));
#187473=CARTESIAN_POINT('Ctrl Pts',(39.4312388757299,-44.0120835699299,
40.0409176249753));
#187474=CARTESIAN_POINT('Ctrl Pts',(39.4313901062474,-44.0149559644984,
40.0388310783332));
#187475=CARTESIAN_POINT('Ctrl Pts',(39.4316052205105,-44.0177981990784,
40.036725739981));
#187476=CARTESIAN_POINT('Ctrl Pts',(39.4323765820013,-44.027989946807,40.0291763710723));
#187477=CARTESIAN_POINT('Ctrl Pts',(39.4339733733562,-44.0378728316078,
40.0213310894606));
#187478=CARTESIAN_POINT('Ctrl Pts',(39.4362681192145,-44.0474262866303,
40.0132837551337));
#187479=CARTESIAN_POINT('Ctrl Pts',(39.4387898143851,-44.0579245739704,
40.0044405431347));
#187480=CARTESIAN_POINT('Ctrl Pts',(39.4421543412257,-44.0680257165067,
39.9953528710629));
#187481=CARTESIAN_POINT('Ctrl Pts',(39.4462454222045,-44.0777053474387,
39.9861103629589));
#187482=CARTESIAN_POINT('Ctrl Pts',(39.4506627629405,-44.0881569195897,
39.9761307737593));
#187483=CARTESIAN_POINT('Ctrl Pts',(39.4559274600916,-44.0981181930531,
39.9659696936053));
#187484=CARTESIAN_POINT('Ctrl Pts',(39.4619494607974,-44.107547242149,39.9557128217551));
#187485=CARTESIAN_POINT('Ctrl Pts',(39.4679209431059,-44.1168971912129,
39.9455419945191));
#187486=CARTESIAN_POINT('Ctrl Pts',(39.4746380711556,-44.1257248429277,
39.9352756289356));
#187487=CARTESIAN_POINT('Ctrl Pts',(39.4820551873929,-44.1339623850448,
39.92499));
#187488=CARTESIAN_POINT('Origin',(0.0113255271402773,0.0101975504409131,
39.92499));
#187489=CARTESIAN_POINT('Ctrl Pts',(42.06380383897,-46.6938111422605,40.10025));
#187490=CARTESIAN_POINT('Ctrl Pts',(42.0701842568307,-46.6880613546455,
40.10025));
#187491=CARTESIAN_POINT('Ctrl Pts',(42.0760276657227,-46.6818296739369,
40.0995859581841));
#187492=CARTESIAN_POINT('Ctrl Pts',(42.0812997491649,-46.6752630175671,
40.0983275959619));
#187493=CARTESIAN_POINT('Ctrl Pts',(42.0846683595052,-46.6710672367544,
40.0975235624067));
#187494=CARTESIAN_POINT('Ctrl Pts',(42.0878044626438,-46.6667352666009,
40.096477705949));
#187495=CARTESIAN_POINT('Ctrl Pts',(42.0907067742416,-46.662309316429,40.0952149915961));
#187496=CARTESIAN_POINT('Ctrl Pts',(42.094667847219,-46.6562687825185,40.0934916398701));
#187497=CARTESIAN_POINT('Ctrl Pts',(42.0981877352864,-46.6500510792882,
40.091364392163));
#187498=CARTESIAN_POINT('Ctrl Pts',(42.1012583942265,-46.6437515300389,
40.0889118607713));
#187499=CARTESIAN_POINT('Ctrl Pts',(42.1027937236965,-46.6406017554142,
40.0876855950754));
#187500=CARTESIAN_POINT('Ctrl Pts',(42.1042169023589,-46.6374313809739,
40.0863782327526));
#187501=CARTESIAN_POINT('Ctrl Pts',(42.1055280393689,-46.6342513293848,
40.0850006373333));
#187502=CARTESIAN_POINT('Ctrl Pts',(42.1061836078739,-46.6326613035902,
40.0843118396237));
#187503=CARTESIAN_POINT('Ctrl Pts',(42.1068111789406,-46.6310688468941,
40.0836054919164));
#187504=CARTESIAN_POINT('Ctrl Pts',(42.1074108478353,-46.6294752517395,
40.0828829920417));
#187505=CARTESIAN_POINT('Ctrl Pts',(42.107560765059,-46.6290768529508,40.0827023670731));
#187506=CARTESIAN_POINT('Ctrl Pts',(42.1077089386741,-46.6286783827619,
40.0825207326932));
#187507=CARTESIAN_POINT('Ctrl Pts',(42.1078553707282,-46.62827986087,40.0823381109275));
#187508=CARTESIAN_POINT('Ctrl Pts',(42.1082946668907,-46.6270842951943,
40.0817902456303));
#187509=CARTESIAN_POINT('Ctrl Pts',(42.1087182876164,-46.6258882654171,
40.0812334935553));
#187510=CARTESIAN_POINT('Ctrl Pts',(42.109126300596,-46.6246922924066,40.0806684524226));
#187511=CARTESIAN_POINT('Ctrl Pts',(42.1119459234384,-46.6164273768569,
40.0767636676138));
#187512=CARTESIAN_POINT('Ctrl Pts',(42.1140735600937,-46.6081492165691,
40.0724404510891));
#187513=CARTESIAN_POINT('Ctrl Pts',(42.1155964444647,-46.5999384432823,
40.0677949937414));
#187514=CARTESIAN_POINT('Ctrl Pts',(42.116353313817,-46.5958577114966,40.0654862141909));
#187515=CARTESIAN_POINT('Ctrl Pts',(42.1169604217533,-46.5917931497416,
40.0630972003217));
#187516=CARTESIAN_POINT('Ctrl Pts',(42.1174262136791,-46.5877524553605,
40.0606363359906));
#187517=CARTESIAN_POINT('Ctrl Pts',(42.11845382024,-46.5788380800229,40.0552073017123));
#187518=CARTESIAN_POINT('Ctrl Pts',(42.1188058546738,-46.5700422469559,
40.0494204304519));
#187519=CARTESIAN_POINT('Ctrl Pts',(42.1185337834653,-46.5615008914344,
40.0434049749851));
#187520=CARTESIAN_POINT('Ctrl Pts',(42.1184343924218,-46.5583806265502,
40.0412074532442));
#187521=CARTESIAN_POINT('Ctrl Pts',(42.1182588963863,-46.5552908961828,
40.0389814735788));
#187522=CARTESIAN_POINT('Ctrl Pts',(42.1180117795242,-46.5522345526328,
40.0367321210017));
#187523=CARTESIAN_POINT('Ctrl Pts',(42.1171817401335,-46.5419686180608,
40.0291767837144));
#187524=CARTESIAN_POINT('Ctrl Pts',(42.1155299964534,-46.5320149571613,
40.0213235332582));
#187525=CARTESIAN_POINT('Ctrl Pts',(42.1131831104089,-46.5223946380456,
40.0132649215868));
#187526=CARTESIAN_POINT('Ctrl Pts',(42.110603604639,-46.5118207677355,40.0044075527545));
#187527=CARTESIAN_POINT('Ctrl Pts',(42.1071843209742,-46.5016489045644,
39.9953016253735));
#187528=CARTESIAN_POINT('Ctrl Pts',(42.1030402839743,-46.4919044745678,
39.9860353422377));
#187529=CARTESIAN_POINT('Ctrl Pts',(42.0985769785676,-46.4814093059457,
39.9760551582716));
#187530=CARTESIAN_POINT('Ctrl Pts',(42.0932726122956,-46.4714088200615,
39.9658879738179));
#187531=CARTESIAN_POINT('Ctrl Pts',(42.0872150940898,-46.4619468343658,
39.955617464328));
#187532=CARTESIAN_POINT('Ctrl Pts',(42.0812393728316,-46.4526126174232,
39.9454856413922));
#187533=CARTESIAN_POINT('Ctrl Pts',(42.0745296860263,-46.4438014421041,
39.9352519465123));
#187534=CARTESIAN_POINT('Ctrl Pts',(42.0671296588095,-46.4355828792671,
39.92499));
#187535=CARTESIAN_POINT('Ctrl Pts',(39.7651933658998,-43.8790236240221,
39.92499));
#187536=CARTESIAN_POINT('Ctrl Pts',(39.7581114992314,-43.8711584142718,
39.9348107241725));
#187537=CARTESIAN_POINT('Ctrl Pts',(39.7504347382251,-43.8638800583566,
39.9446038383176));
#187538=CARTESIAN_POINT('Ctrl Pts',(39.7422106539907,-43.857221832853,39.9543158069394));
#187539=CARTESIAN_POINT('Ctrl Pts',(39.7342695770756,-43.850792730313,39.9636935671402));
#187540=CARTESIAN_POINT('Ctrl Pts',(39.7258171668693,-43.8449410790338,
39.9729968321001));
#187541=CARTESIAN_POINT('Ctrl Pts',(39.7168657021547,-43.8397310304449,
39.982173115135));
#187542=CARTESIAN_POINT('Ctrl Pts',(39.7084037645741,-43.8348059028422,
39.9908475764368));
#187543=CARTESIAN_POINT('Ctrl Pts',(39.6994950821784,-43.8304536682204,
39.9994093733864));
#187544=CARTESIAN_POINT('Ctrl Pts',(39.6901349804726,-43.826767684781,40.0077966115861));
#187545=CARTESIAN_POINT('Ctrl Pts',(39.6815144838289,-43.8233729558702,
40.0155211172616));
#187546=CARTESIAN_POINT('Ctrl Pts',(39.6725105620411,-43.8205432023696,
40.0230979941044));
#187547=CARTESIAN_POINT('Ctrl Pts',(39.6631152739614,-43.818389241968,40.0304554104772));
#187548=CARTESIAN_POINT('Ctrl Pts',(39.6603137887132,-43.8177469744569,
40.0326492435197));
#187549=CARTESIAN_POINT('Ctrl Pts',(39.6574775031712,-43.8171650742227,
40.0348233715068));
#187550=CARTESIAN_POINT('Ctrl Pts',(39.654606226052,-43.8166472411071,40.0369753512356));
#187551=CARTESIAN_POINT('Ctrl Pts',(39.6517642863086,-43.8161346989696,
40.0391053430352));
#187552=CARTESIAN_POINT('Ctrl Pts',(39.6488910639689,-43.8156851836082,
40.041211089324));
#187553=CARTESIAN_POINT('Ctrl Pts',(39.6459896850503,-43.8153025584992,
40.0432881154904));
#187554=CARTESIAN_POINT('Ctrl Pts',(39.6457879288345,-43.8152759514975,
40.043432547828));
#187555=CARTESIAN_POINT('Ctrl Pts',(39.6455860324536,-43.8152496566736,
40.0435768364421));
#187556=CARTESIAN_POINT('Ctrl Pts',(39.6453839959665,-43.8152236753306,
40.0437209807855));
#187557=CARTESIAN_POINT('Ctrl Pts',(39.6365259762555,-43.8140845580783,
40.050040796842));
#187558=CARTESIAN_POINT('Ctrl Pts',(39.6274037177903,-43.813592968579,40.0560490279344));
#187559=CARTESIAN_POINT('Ctrl Pts',(39.6180980992375,-43.8138323099899,
40.0616647108614));
#187560=CARTESIAN_POINT('Ctrl Pts',(39.6094236454408,-43.8140554177821,
40.0668995033484));
#187561=CARTESIAN_POINT('Ctrl Pts',(39.6005890951404,-43.8149139527617,
40.071793326748));
#187562=CARTESIAN_POINT('Ctrl Pts',(39.5916773623197,-43.8164991115143,
40.076246030307));
#187563=CARTESIAN_POINT('Ctrl Pts',(39.5884173351606,-43.8170789830936,
40.0778748868747));
#187564=CARTESIAN_POINT('Ctrl Pts',(39.5851472105419,-43.8177563121466,
40.0794443522247));
#187565=CARTESIAN_POINT('Ctrl Pts',(39.5818719865444,-43.8185363400628,
40.0809482021492));
#187566=CARTESIAN_POINT('Ctrl Pts',(39.5810844045886,-43.8187239107182,
40.0813098278168));
#187567=CARTESIAN_POINT('Ctrl Pts',(39.580296141232,-43.8189178575371,40.0816679525672));
#187568=CARTESIAN_POINT('Ctrl Pts',(39.5795073285707,-43.8191182115051,
40.0820224192581));
#187569=CARTESIAN_POINT('Ctrl Pts',(39.5787431663051,-43.8193123044115,
40.0823658088648));
#187570=CARTESIAN_POINT('Ctrl Pts',(39.577978488548,-43.8195124102599,40.0827057654617));
#187571=CARTESIAN_POINT('Ctrl Pts',(39.5772134181964,-43.8197185546679,
40.0830421470151));
#187572=CARTESIAN_POINT('Ctrl Pts',(39.5688311883231,-43.8219771048931,
40.0867275956807));
#187573=CARTESIAN_POINT('Ctrl Pts',(39.560396428487,-43.8249623840155,40.0899823432032));
#187574=CARTESIAN_POINT('Ctrl Pts',(39.5520968239715,-43.8286919494555,
40.0926299529357));
#187575=CARTESIAN_POINT('Ctrl Pts',(39.5486547305943,-43.8302387114098,
40.0937279956085));
#187576=CARTESIAN_POINT('Ctrl Pts',(39.5452359574128,-43.8319130705227,
40.0947220371803));
#187577=CARTESIAN_POINT('Ctrl Pts',(39.5418537500316,-43.8337144555751,
40.0956014538692));
#187578=CARTESIAN_POINT('Ctrl Pts',(39.5360850428918,-43.8367869054995,
40.097101390674));
#187579=CARTESIAN_POINT('Ctrl Pts',(39.5304250803199,-43.8402296473864,
40.0982667904316));
#187580=CARTESIAN_POINT('Ctrl Pts',(39.5249464846904,-43.8440378929941,
40.0990539325582));
#187581=CARTESIAN_POINT('Ctrl Pts',(39.5222071868757,-43.845942015798,40.0994475036216));
#187582=CARTESIAN_POINT('Ctrl Pts',(39.5195141476135,-43.8479386338067,
40.0997467259952));
#187583=CARTESIAN_POINT('Ctrl Pts',(39.516876509875,-43.8500271570781,40.0999473488896));
#187584=CARTESIAN_POINT('Ctrl Pts',(39.5142388721366,-43.8521156803494,
40.100147971784));
#187585=CARTESIAN_POINT('Ctrl Pts',(39.5116566557598,-43.8542960677574,
40.10025));
#187586=CARTESIAN_POINT('Ctrl Pts',(39.5091373124622,-43.8565665267057,
40.10025));
#187587=CARTESIAN_POINT('Origin',(34.2342565846635,-47.1453396605409,39.92499));
#187588=CARTESIAN_POINT('Ctrl Pts',(36.6746059268177,-50.8023624960592,
39.92499));
#187589=CARTESIAN_POINT('Ctrl Pts',(36.6808425220337,-50.8109464329598,
39.9348354642014));
#187590=CARTESIAN_POINT('Ctrl Pts',(36.6877379133665,-50.8190128116683,
39.944644082845));
#187591=CARTESIAN_POINT('Ctrl Pts',(36.6952462569238,-50.8265243508952,
39.9543641760321));
#187592=CARTESIAN_POINT('Ctrl Pts',(36.7025106240248,-50.8337918098256,
39.96376842407));
#187593=CARTESIAN_POINT('Ctrl Pts',(36.7103497152241,-50.8405407635272,
39.9730909636382));
#187594=CARTESIAN_POINT('Ctrl Pts',(36.7187568768207,-50.8467071440062,
39.9822808977125));
#187595=CARTESIAN_POINT('Ctrl Pts',(36.726709534008,-50.8525401602356,39.9909740094633));
#187596=CARTESIAN_POINT('Ctrl Pts',(36.735171246281,-50.8578524412735,39.9995492764984));
#187597=CARTESIAN_POINT('Ctrl Pts',(36.7441560526511,-50.8625525281322,
40.0079462328676));
#187598=CARTESIAN_POINT('Ctrl Pts',(36.7524317091156,-50.8668816480481,
40.0156804369671));
#187599=CARTESIAN_POINT('Ctrl Pts',(36.7611516658444,-50.870691607918,40.0232638017403));
#187600=CARTESIAN_POINT('Ctrl Pts',(36.7703354510142,-50.8738736606193,
40.0306257269946));
#187601=CARTESIAN_POINT('Ctrl Pts',(36.772999317991,-50.8747966531494,40.0327611416638));
#187602=CARTESIAN_POINT('Ctrl Pts',(36.7757022424567,-50.8756665488978,
40.0348777427264));
#187603=CARTESIAN_POINT('Ctrl Pts',(36.7784447603818,-50.8764799968252,
40.0369733168701));
#187604=CARTESIAN_POINT('Ctrl Pts',(36.7814178261393,-50.8773618266782,
40.039245053974));
#187605=CARTESIAN_POINT('Ctrl Pts',(36.7844329791247,-50.8781771258723,
40.041487875195));
#187606=CARTESIAN_POINT('Ctrl Pts',(36.7874899206174,-50.8789219044953,
40.0436985701601));
#187607=CARTESIAN_POINT('Ctrl Pts',(36.7958797205316,-50.8809659552704,
40.0497658398386));
#187608=CARTESIAN_POINT('Ctrl Pts',(36.8045837617103,-50.8824343655144,
40.0555581699984));
#187609=CARTESIAN_POINT('Ctrl Pts',(36.8135226609478,-50.8832604021662,
40.0609828468885));
#187610=CARTESIAN_POINT('Ctrl Pts',(36.8217012684462,-50.8840161808561,
40.0659461317306));
#187611=CARTESIAN_POINT('Ctrl Pts',(36.8300699399865,-50.8842246658555,
40.070603998071));
#187612=CARTESIAN_POINT('Ctrl Pts',(36.838587648016,-50.8838072802927,40.0748843180608));
#187613=CARTESIAN_POINT('Ctrl Pts',(36.8427715183753,-50.8836022618678,
40.0769867972572));
#187614=CARTESIAN_POINT('Ctrl Pts',(36.8469911418452,-50.8832457706969,
40.0789976708176));
#187615=CARTESIAN_POINT('Ctrl Pts',(36.8512399286217,-50.8827256259725,
40.0809050491499));
#187616=CARTESIAN_POINT('Ctrl Pts',(36.8520460945289,-50.8826269335773,
40.0812669556104));
#187617=CARTESIAN_POINT('Ctrl Pts',(36.8528536453866,-50.8825219362259,
40.0816253922032));
#187618=CARTESIAN_POINT('Ctrl Pts',(36.8536624499713,-50.8824105850807,
40.0819801989139));
#187619=CARTESIAN_POINT('Ctrl Pts',(36.8544459794128,-50.8823027136588,
40.0823239179148));
#187620=CARTESIAN_POINT('Ctrl Pts',(36.8552306854278,-50.8821888793657,
40.0826642303498));
#187621=CARTESIAN_POINT('Ctrl Pts',(36.8560164456186,-50.8820690400775,
40.0830009916099));
#187622=CARTESIAN_POINT('Ctrl Pts',(36.8645794982679,-50.8807630562079,
40.0866709464313));
#187623=CARTESIAN_POINT('Ctrl Pts',(36.8732733195879,-50.8787426509996,
40.0899175831879));
#187624=CARTESIAN_POINT('Ctrl Pts',(36.8819119966118,-50.8759664620665,
40.0925642067064));
#187625=CARTESIAN_POINT('Ctrl Pts',(36.8855601635621,-50.8747940602409,
40.0936818922528));
#187626=CARTESIAN_POINT('Ctrl Pts',(36.8891983713651,-50.8734872887376,
40.0946930094791));
#187627=CARTESIAN_POINT('Ctrl Pts',(36.8928125648617,-50.8720449698704,
40.0955863397545));
#187628=CARTESIAN_POINT('Ctrl Pts',(36.8988987764016,-50.8696161409374,
40.0970906856166));
#187629=CARTESIAN_POINT('Ctrl Pts',(36.9049145742147,-50.8668019052537,
40.0982599215483));
#187630=CARTESIAN_POINT('Ctrl Pts',(36.9107858666119,-50.8635979627951,
40.0990497370453));
#187631=CARTESIAN_POINT('Ctrl Pts',(36.9122536897111,-50.8627969771804,
40.0992471909196));
#187632=CARTESIAN_POINT('Ctrl Pts',(36.9137123559381,-50.8619714372918,
40.0994209989363));
#187633=CARTESIAN_POINT('Ctrl Pts',(36.915160532232,-50.8611210221658,40.0995705982975));
#187634=CARTESIAN_POINT('Ctrl Pts',(36.9173327966728,-50.8598453994767,
40.0997949973393));
#187635=CARTESIAN_POINT('Ctrl Pts',(36.9194814382215,-50.8585138058057,
40.0999649129781));
#187636=CARTESIAN_POINT('Ctrl Pts',(36.921602929223,-50.8571265262608,40.1000786629733));
#187637=CARTESIAN_POINT('Ctrl Pts',(36.9237244202244,-50.855739246716,40.1001924129685));
#187638=CARTESIAN_POINT('Ctrl Pts',(36.9258187603139,-50.8542962928985,
40.10025));
#187639=CARTESIAN_POINT('Ctrl Pts',(36.9278827595336,-50.85279802814,40.10025));
#187640=CARTESIAN_POINT('Ctrl Pts',(34.6837837831345,-47.7640607692764,
40.10025));
#187641=CARTESIAN_POINT('Ctrl Pts',(34.6767997090229,-47.7691302463542,
40.10025));
#187642=CARTESIAN_POINT('Ctrl Pts',(34.6702946353246,-47.7747322888382,
40.0995786334241));
#187643=CARTESIAN_POINT('Ctrl Pts',(34.6643211616157,-47.7807252357992,
40.0983063763366));
#187644=CARTESIAN_POINT('Ctrl Pts',(34.6604629105137,-47.7845960646239,
40.0974846287992));
#187645=CARTESIAN_POINT('Ctrl Pts',(34.6568257642793,-47.7886293194336,
40.0964130309338));
#187646=CARTESIAN_POINT('Ctrl Pts',(34.6534164822763,-47.7927819897609,
40.0951176960924));
#187647=CARTESIAN_POINT('Ctrl Pts',(34.6488976742769,-47.7982861164003,
40.0934008039614));
#187648=CARTESIAN_POINT('Ctrl Pts',(34.6447843113774,-47.8040027249063,
40.0912909372156));
#187649=CARTESIAN_POINT('Ctrl Pts',(34.6410949611633,-47.8098436832078,
40.0888630467851));
#187650=CARTESIAN_POINT('Ctrl Pts',(34.6392502860562,-47.8127641623586,
40.0876491015699));
#187651=CARTESIAN_POINT('Ctrl Pts',(34.6375114518666,-47.8157158446827,
40.0863558569271));
#187652=CARTESIAN_POINT('Ctrl Pts',(34.6358796311044,-47.8186885387637,
40.0849936342771));
#187653=CARTESIAN_POINT('Ctrl Pts',(34.6350637207232,-47.8201748858042,
40.0843125229521));
#187654=CARTESIAN_POINT('Ctrl Pts',(34.6342745503772,-47.8216664954025,
40.0836141747074));
#187655=CARTESIAN_POINT('Ctrl Pts',(34.6335121829169,-47.8231621539166,
40.0828999161609));
#187656=CARTESIAN_POINT('Ctrl Pts',(34.6333215910518,-47.8235360685451,
40.0827213515243));
#187657=CARTESIAN_POINT('Ctrl Pts',(34.6331326740831,-47.8239102364346,
40.0825417925842));
#187658=CARTESIAN_POINT('Ctrl Pts',(34.63294543242,-47.8242846390326,40.0823612602361));
#187659=CARTESIAN_POINT('Ctrl Pts',(34.6323837074307,-47.8254078468264,
40.0818196631917));
#187660=CARTESIAN_POINT('Ctrl Pts',(34.6318370616129,-47.8265331659851,
40.0812693052022));
#187661=CARTESIAN_POINT('Ctrl Pts',(34.6313054933184,-47.8276601046326,
40.0807107531875));
#187662=CARTESIAN_POINT('Ctrl Pts',(34.6275611948903,-47.8355981149514,
40.0767763849182));
#187663=CARTESIAN_POINT('Ctrl Pts',(34.6245119115567,-47.8436253243398,
40.0724140586137));
#187664=CARTESIAN_POINT('Ctrl Pts',(34.622080800581,-47.851650015445,40.0677221223768));
#187665=CARTESIAN_POINT('Ctrl Pts',(34.6209017143849,-47.8555419819595,
40.0654465383721));
#187666=CARTESIAN_POINT('Ctrl Pts',(34.6198683413513,-47.8594338479542,
40.0630928000679));
#187667=CARTESIAN_POINT('Ctrl Pts',(34.618973699214,-47.8633173872849,40.0606689262479));
#187668=CARTESIAN_POINT('Ctrl Pts',(34.6176040646085,-47.8692628146652,
40.0569581447805));
#187669=CARTESIAN_POINT('Ctrl Pts',(34.6165592825246,-47.8751852090113,
40.0530843804605));
#187670=CARTESIAN_POINT('Ctrl Pts',(34.6158190596252,-47.8810431641656,
40.0490800251457));
#187671=CARTESIAN_POINT('Ctrl Pts',(34.6154752962814,-47.8837636288443,
40.0472203818218));
#187672=CARTESIAN_POINT('Ctrl Pts',(34.6151969889848,-47.8864700832047,
40.0453323608818));
#187673=CARTESIAN_POINT('Ctrl Pts',(34.6149833323962,-47.8891582656052,
40.0434201572162));
#187674=CARTESIAN_POINT('Ctrl Pts',(34.6149669564605,-47.8893643041942,
40.0432735943397));
#187675=CARTESIAN_POINT('Ctrl Pts',(34.6149509280617,-47.889570245931,40.0431268995707));
#187676=CARTESIAN_POINT('Ctrl Pts',(34.6149352461545,-47.8897760897956,
40.0429800745037));
#187677=CARTESIAN_POINT('Ctrl Pts',(34.6147149626377,-47.8926675754933,
40.0409176249753));
#187678=CARTESIAN_POINT('Ctrl Pts',(34.6145651177085,-47.8955400426774,
40.0388310783332));
#187679=CARTESIAN_POINT('Ctrl Pts',(34.6144819591403,-47.8983891927623,
40.036725739981));
#187680=CARTESIAN_POINT('Ctrl Pts',(34.614183767304,-47.9086057382627,40.0291763710716));
#187681=CARTESIAN_POINT('Ctrl Pts',(34.614738768508,-47.9186013937339,40.0213310894592));
#187682=CARTESIAN_POINT('Ctrl Pts',(34.6160223355362,-47.928342380189,40.0132837551316));
#187683=CARTESIAN_POINT('Ctrl Pts',(34.6174328467544,-47.9390467457341,
40.0044405431322));
#187684=CARTESIAN_POINT('Ctrl Pts',(34.6197230854587,-47.9494442419753,
39.9953528710599));
#187685=CARTESIAN_POINT('Ctrl Pts',(34.6227799581218,-47.9594984812844,
39.9861103629555));
#187686=CARTESIAN_POINT('Ctrl Pts',(34.6260806134275,-47.9703545364682,
39.976130773756));
#187687=CARTESIAN_POINT('Ctrl Pts',(34.6302752334096,-47.9808115517359,
39.9659696936021));
#187688=CARTESIAN_POINT('Ctrl Pts',(34.6352786409534,-47.9908184179935,
39.9557128217521));
#187689=CARTESIAN_POINT('Ctrl Pts',(34.6402400750495,-48.0007413369263,
39.945541994517));
#187690=CARTESIAN_POINT('Ctrl Pts',(34.6459976651004,-48.010222760913,39.9352756289345));
#187691=CARTESIAN_POINT('Ctrl Pts',(34.6525130919796,-48.0191904766737,
39.92499));
#187692=CARTESIAN_POINT('Origin',(0.0123294189942765,0.0089578472449418,
39.92499));
#187693=CARTESIAN_POINT('Ctrl Pts',(36.9525415975211,-50.8348823336487,
40.10025));
#187694=CARTESIAN_POINT('Ctrl Pts',(36.959488079248,-50.8298309792464,40.10025));
#187695=CARTESIAN_POINT('Ctrl Pts',(36.9659508653421,-50.8242442388892,
40.0995859581843));
#187696=CARTESIAN_POINT('Ctrl Pts',(36.9718804702581,-50.8182646381311,
40.0983275959624));
#187697=CARTESIAN_POINT('Ctrl Pts',(36.9756692055198,-50.8144439579064,
40.0975235624071));
#187698=CARTESIAN_POINT('Ctrl Pts',(36.9792409429411,-50.8104635307797,
40.0964777059492));
#187699=CARTESIAN_POINT('Ctrl Pts',(36.9825899931427,-50.8063652005965,
40.0952149915962));
#187700=CARTESIAN_POINT('Ctrl Pts',(36.9871607746749,-50.800771802234,40.0934916398702));
#187701=CARTESIAN_POINT('Ctrl Pts',(36.9913113073909,-50.7949560887231,
40.0913643921631));
#187702=CARTESIAN_POINT('Ctrl Pts',(36.9950236271423,-50.7890120203239,
40.0889118607714));
#187703=CARTESIAN_POINT('Ctrl Pts',(36.996879787018,-50.7860399861243,40.0876855950755));
#187704=CARTESIAN_POINT('Ctrl Pts',(36.998626563727,-50.7830357420055,40.0863782327527));
#187705=CARTESIAN_POINT('Ctrl Pts',(37.000262924097,-50.7800101622085,40.0850006373335));
#187706=CARTESIAN_POINT('Ctrl Pts',(37.0010811042821,-50.77849737231,40.0843118396238));
#187707=CARTESIAN_POINT('Ctrl Pts',(37.0018716945001,-50.7769792382974,
40.0836054919165));
#187708=CARTESIAN_POINT('Ctrl Pts',(37.0026346543984,-50.7754570554919,
40.0828829920418));
#187709=CARTESIAN_POINT('Ctrl Pts',(37.002825394373,-50.7750765097905,40.0827023670732));
#187710=CARTESIAN_POINT('Ctrl Pts',(37.003014407754,-50.7746957108232,40.0825207326934));
#187711=CARTESIAN_POINT('Ctrl Pts',(37.0032016945189,-50.7743146783935,
40.0823381109276));
#187712=CARTESIAN_POINT('Ctrl Pts',(37.0037635548139,-50.7731715811044,
40.0817902456304));
#187713=CARTESIAN_POINT('Ctrl Pts',(37.0043098740556,-50.7720263837271,
40.0812334935554));
#187714=CARTESIAN_POINT('Ctrl Pts',(37.0048406651183,-50.7708796113516,
40.0806684524228));
#187715=CARTESIAN_POINT('Ctrl Pts',(37.0085087606932,-50.7629547027167,
40.0767636676139));
#187716=CARTESIAN_POINT('Ctrl Pts',(37.0114900453058,-50.7549442896472,
40.0724404510892));
#187717=CARTESIAN_POINT('Ctrl Pts',(37.0138628466708,-50.7469376805987,
40.0677949937416));
#187718=CARTESIAN_POINT('Ctrl Pts',(37.0150421224361,-50.7429584178789,
40.065486214191));
#187719=CARTESIAN_POINT('Ctrl Pts',(37.0160707669657,-50.7389795822781,
40.0630972003218));
#187720=CARTESIAN_POINT('Ctrl Pts',(37.0169563748089,-50.7350097117577,
40.0606363359906));
#187721=CARTESIAN_POINT('Ctrl Pts',(37.0189101579885,-50.7262515844356,
40.0552073017124));
#187722=CARTESIAN_POINT('Ctrl Pts',(37.0201796788544,-50.7175407334808,
40.049420430452));
#187723=CARTESIAN_POINT('Ctrl Pts',(37.0208019128475,-50.7090177292133,
40.0434049749851));
#187724=CARTESIAN_POINT('Ctrl Pts',(37.0210292227719,-50.7059041682736,
40.0412074532442));
#187725=CARTESIAN_POINT('Ctrl Pts',(37.0211776528892,-50.7028130194416,
40.0389814735788));
#187726=CARTESIAN_POINT('Ctrl Pts',(37.0212513646537,-50.6997475881155,
40.0367321210016));
#187727=CARTESIAN_POINT('Ctrl Pts',(37.0214989546705,-50.6894511286651,
40.0291767837141));
#187728=CARTESIAN_POINT('Ctrl Pts',(37.0208967002929,-50.6793793407328,
40.0213235332578));
#187729=CARTESIAN_POINT('Ctrl Pts',(37.019568267909,-50.6695664063399,40.0132649215862));
#187730=CARTESIAN_POINT('Ctrl Pts',(37.0181081633559,-50.6587808290235,
40.0044075527537));
#187731=CARTESIAN_POINT('Ctrl Pts',(37.0157708601105,-50.648307275916,39.9953016253725));
#187732=CARTESIAN_POINT('Ctrl Pts',(37.0126680948718,-50.638183057107,39.9860353422364));
#187733=CARTESIAN_POINT('Ctrl Pts',(37.0093262837667,-50.6272788396614,
39.9760551582701));
#187734=CARTESIAN_POINT('Ctrl Pts',(37.0050963107894,-50.6167786802299,
39.9658879738162));
#187735=CARTESIAN_POINT('Ctrl Pts',(37.0000610231261,-50.6067353452124,
39.9556174643261));
#187736=CARTESIAN_POINT('Ctrl Pts',(36.9950937288471,-50.5968276291274,
39.9454856413909));
#187737=CARTESIAN_POINT('Ctrl Pts',(36.9893418170241,-50.5873633690984,
39.9352519465116));
#187738=CARTESIAN_POINT('Ctrl Pts',(36.9828414016746,-50.5784163149358,
39.92499));
#187739=CARTESIAN_POINT('Ctrl Pts',(34.9607485668365,-47.7952442955503,
39.92499));
#187740=CARTESIAN_POINT('Ctrl Pts',(34.9545276336626,-47.7866819156013,
39.9348107241734));
#187741=CARTESIAN_POINT('Ctrl Pts',(34.9476537221147,-47.7786409912499,
39.9446038383192));
#187742=CARTESIAN_POINT('Ctrl Pts',(34.9401706643534,-47.7711595893149,
39.9543158069418));
#187743=CARTESIAN_POINT('Ctrl Pts',(34.9329451136968,-47.7639356375043,
39.9636935671432));
#187744=CARTESIAN_POINT('Ctrl Pts',(34.9251506707932,-47.757232524733,39.9729968321037));
#187745=CARTESIAN_POINT('Ctrl Pts',(34.9167928415108,-47.7511153344846,
39.982173115139));
#187746=CARTESIAN_POINT('Ctrl Pts',(34.9088920753289,-47.7453326739146,
39.9908475764412));
#187747=CARTESIAN_POINT('Ctrl Pts',(34.9004871280237,-47.7400730704088,
39.9994093733912));
#187748=CARTESIAN_POINT('Ctrl Pts',(34.8915635921182,-47.735428882125,40.0077966115912));
#187749=CARTESIAN_POINT('Ctrl Pts',(34.8833451652528,-47.7311516626277,
40.015521117267));
#187750=CARTESIAN_POINT('Ctrl Pts',(34.8746863576748,-47.7273962447052,
40.02309799411));
#187751=CARTESIAN_POINT('Ctrl Pts',(34.8655676881364,-47.7242720088992,
40.030455410483));
#187752=CARTESIAN_POINT('Ctrl Pts',(34.8628486849558,-47.7233404248499,
40.0326492435235));
#187753=CARTESIAN_POINT('Ctrl Pts',(34.8600887620223,-47.7224652397578,
40.0348233715087));
#187754=CARTESIAN_POINT('Ctrl Pts',(34.857287342362,-47.721650113202,40.0369753512355));
#187755=CARTESIAN_POINT('Ctrl Pts',(34.8545145463038,-47.7208433152299,
40.0391053430351));
#187756=CARTESIAN_POINT('Ctrl Pts',(34.8517040509267,-47.7200959288448,
40.0412110893239));
#187757=CARTESIAN_POINT('Ctrl Pts',(34.84885856128,-47.7194121231166,40.0432881154903));
#187758=CARTESIAN_POINT('Ctrl Pts',(34.8486606914949,-47.7193645726035,
40.0434325478279));
#187759=CARTESIAN_POINT('Ctrl Pts',(34.848462649681,-47.719317317907,40.0435768364421));
#187760=CARTESIAN_POINT('Ctrl Pts',(34.8482644357608,-47.719270360329,40.0437209807855));
#187761=CARTESIAN_POINT('Ctrl Pts',(34.8395740113844,-47.7172115680922,
40.050040796842));
#187762=CARTESIAN_POINT('Ctrl Pts',(34.8305531107003,-47.7157691359127,
40.0560490279346));
#187763=CARTESIAN_POINT('Ctrl Pts',(34.8212734513095,-47.7150344641792,
40.0616647108616));
#187764=CARTESIAN_POINT('Ctrl Pts',(34.8126231959634,-47.7143496224385,
40.0668995033488));
#187765=CARTESIAN_POINT('Ctrl Pts',(34.8037473009116,-47.7142799923071,
40.0717933267485));
#187766=CARTESIAN_POINT('Ctrl Pts',(34.794718693287,-47.7149249376575,40.0762460303076));
#187767=CARTESIAN_POINT('Ctrl Pts',(34.7914159118131,-47.7151608670105,
40.077874886875));
#187768=CARTESIAN_POINT('Ctrl Pts',(34.7880929011146,-47.715492664483,40.0794443522248));
#187769=CARTESIAN_POINT('Ctrl Pts',(34.7847540840179,-47.7159260651933,
40.0809482021492));
#187770=CARTESIAN_POINT('Ctrl Pts',(34.7839512100461,-47.7160302835855,
40.0813098278168));
#187771=CARTESIAN_POINT('Ctrl Pts',(34.7831469919157,-47.7161407719861,
40.0816679525672));
#187772=CARTESIAN_POINT('Ctrl Pts',(34.7823415577603,-47.7162575750188,
40.082022419258));
#187773=CARTESIAN_POINT('Ctrl Pts',(34.7815612934223,-47.7163707279567,
40.0823658088648));
#187774=CARTESIAN_POINT('Ctrl Pts',(34.7807798878931,-47.7164898070134,
40.0827057654616));
#187775=CARTESIAN_POINT('Ctrl Pts',(34.7799974607188,-47.7166148505126,
40.0830421470151));
#187776=CARTESIAN_POINT('Ctrl Pts',(34.7714250667942,-47.7179848465559,
40.0867275956804));
#187777=CARTESIAN_POINT('Ctrl Pts',(34.7627244668166,-47.720072099523,40.0899823432026));
#187778=CARTESIAN_POINT('Ctrl Pts',(34.7540804826596,-47.7229136891072,
40.092629952935));
#187779=CARTESIAN_POINT('Ctrl Pts',(34.7504955647793,-47.7240921810067,
40.0937279956081));
#187780=CARTESIAN_POINT('Ctrl Pts',(34.7469205018093,-47.7254000086985,
40.0947220371801));
#187781=CARTESIAN_POINT('Ctrl Pts',(34.7433685265021,-47.7268379886353,
40.0956014538692));
#187782=CARTESIAN_POINT('Ctrl Pts',(34.7373102624745,-47.7292906132652,
40.097101390674));
#187783=CARTESIAN_POINT('Ctrl Pts',(34.7313214412509,-47.732122868262,40.0982667904316));
#187784=CARTESIAN_POINT('Ctrl Pts',(34.7254747878805,-47.73533758272,40.0990539325582));
#187785=CARTESIAN_POINT('Ctrl Pts',(34.7225514611953,-47.736944939949,40.0994475036216));
#187786=CARTESIAN_POINT('Ctrl Pts',(34.7196644712718,-47.7386491210197,
40.0997467259952));
#187787=CARTESIAN_POINT('Ctrl Pts',(34.7168229726608,-47.7404504949226,
40.0999473488896));
#187788=CARTESIAN_POINT('Ctrl Pts',(34.7139814740497,-47.7422518688254,
40.100147971784));
#187789=CARTESIAN_POINT('Ctrl Pts',(34.7111854907792,-47.7441503967332,
40.10025));
#187790=CARTESIAN_POINT('Ctrl Pts',(34.7084426211231,-47.7461450747865,
40.10025));
#187791=CARTESIAN_POINT('Origin',(29.1186878401555,-50.4655267888876,39.92499));
#187792=CARTESIAN_POINT('Ctrl Pts',(31.1634057161439,-54.3576020372439,
39.92499));
#187793=CARTESIAN_POINT('Ctrl Pts',(31.1687108809057,-54.3667908521538,
39.934835464201));
#187794=CARTESIAN_POINT('Ctrl Pts',(31.1747253323926,-54.3755338070552,
39.9446440828443));
#187795=CARTESIAN_POINT('Ctrl Pts',(31.1814073748059,-54.3837890328978,
39.954364176031));
#187796=CARTESIAN_POINT('Ctrl Pts',(31.1878722906298,-54.3917760130574,
39.9637684240687));
#187797=CARTESIAN_POINT('Ctrl Pts',(31.194962980708,-54.3993074034408,39.9730909636366));
#187798=CARTESIAN_POINT('Ctrl Pts',(31.202679524718,-54.4063187915244,39.9822808977107));
#187799=CARTESIAN_POINT('Ctrl Pts',(31.2099789001941,-54.4129511329151,
39.9909740094612));
#187800=CARTESIAN_POINT('Ctrl Pts',(31.2178389737483,-54.4191188025021,
39.9995492764961));
#187801=CARTESIAN_POINT('Ctrl Pts',(31.226283267552,-54.4247323097957,40.0079462328652));
#187802=CARTESIAN_POINT('Ctrl Pts',(31.234061072852,-54.4299027559923,40.0156804369644));
#187803=CARTESIAN_POINT('Ctrl Pts',(31.2423350114947,-54.43460332818,40.0232638017373));
#187804=CARTESIAN_POINT('Ctrl Pts',(31.251135871849,-54.4387279162144,40.0306257269915));
#187805=CARTESIAN_POINT('Ctrl Pts',(31.2536886668942,-54.4399243024168,
40.0327611416618));
#187806=CARTESIAN_POINT('Ctrl Pts',(31.2562858555923,-54.4410719653266,
40.0348777427254));
#187807=CARTESIAN_POINT('Ctrl Pts',(31.2589283212566,-54.4421676282858,
40.03697331687));
#187808=CARTESIAN_POINT('Ctrl Pts',(31.2617929239294,-54.4433553973773,
40.039245053974));
#187809=CARTESIAN_POINT('Ctrl Pts',(31.2647063376194,-54.4444813995853,
40.041487875195));
#187810=CARTESIAN_POINT('Ctrl Pts',(31.2676686823018,-54.4455416356296,
40.04369857016));
#187811=CARTESIAN_POINT('Ctrl Pts',(31.2757988605279,-54.4484514617727,
40.0497658398386));
#187812=CARTESIAN_POINT('Ctrl Pts',(31.2843017293921,-54.4508216479603,
40.0555581699984));
#187813=CARTESIAN_POINT('Ctrl Pts',(31.2931053160624,-54.4525775288975,
40.0609828468885));
#187814=CARTESIAN_POINT('Ctrl Pts',(31.3011601199077,-54.4541840646261,
40.0659461317304));
#187815=CARTESIAN_POINT('Ctrl Pts',(31.3094611543726,-54.4552661718985,
40.0706039980705));
#187816=CARTESIAN_POINT('Ctrl Pts',(31.3179758301772,-54.4557414157485,
40.0748843180601));
#187817=CARTESIAN_POINT('Ctrl Pts',(31.3221582111182,-54.4559748539752,
40.0769867972569));
#187818=CARTESIAN_POINT('Ctrl Pts',(31.3263919825241,-54.4560613864571,
40.0789976708174));
#187819=CARTESIAN_POINT('Ctrl Pts',(31.3306718639313,-54.4559882102924,
40.08090504915));
#187820=CARTESIAN_POINT('Ctrl Pts',(31.3314839297417,-54.4559743258279,
40.0812669556105));
#187821=CARTESIAN_POINT('Ctrl Pts',(31.332298031963,-54.4559543157131,40.0816253922032));
#187822=CARTESIAN_POINT('Ctrl Pts',(31.3331140451957,-54.4559281176615,
40.0819801989139));
#187823=CARTESIAN_POINT('Ctrl Pts',(31.3339045580149,-54.4559027382989,
40.0823239179149));
#187824=CARTESIAN_POINT('Ctrl Pts',(31.334696864252,-54.4558715517159,40.0826642303498));
#187825=CARTESIAN_POINT('Ctrl Pts',(31.3354908465828,-54.4558345032251,
40.0830009916099));
#187826=CARTESIAN_POINT('Ctrl Pts',(31.3441435024208,-54.4554307564062,
40.0866709464313));
#187827=CARTESIAN_POINT('Ctrl Pts',(31.3530008879296,-54.4543301709715,
40.0899175831879));
#187828=CARTESIAN_POINT('Ctrl Pts',(31.3618824321397,-54.4524721779258,
40.0925642067064));
#187829=CARTESIAN_POINT('Ctrl Pts',(31.3656331634109,-54.4516875359251,
40.0936818922529));
#187830=CARTESIAN_POINT('Ctrl Pts',(31.369388035548,-54.4507682193235,40.0946930094791));
#187831=CARTESIAN_POINT('Ctrl Pts',(31.3731331934892,-54.4497115877221,
40.0955863397546));
#187832=CARTESIAN_POINT('Ctrl Pts',(31.3794399458813,-54.4479322465076,
40.0970906856166));
#187833=CARTESIAN_POINT('Ctrl Pts',(31.3857169562559,-54.4457622496021,
40.0982599215483));
#187834=CARTESIAN_POINT('Ctrl Pts',(31.3918909882807,-54.4431895758475,
40.0990497370454));
#187835=CARTESIAN_POINT('Ctrl Pts',(31.393434496287,-54.4425464074089,40.0992471909196));
#187836=CARTESIAN_POINT('Ctrl Pts',(31.3949714642036,-54.4418778620532,
40.0994209989363));
#187837=CARTESIAN_POINT('Ctrl Pts',(31.3965005998225,-54.4411834812328,
40.0995705982975));
#187838=CARTESIAN_POINT('Ctrl Pts',(31.3987943032508,-54.4401419100021,
40.0997949973393));
#187839=CARTESIAN_POINT('Ctrl Pts',(31.4010703637564,-54.4390422051396,
40.0999649129781));
#187840=CARTESIAN_POINT('Ctrl Pts',(31.4033252432071,-54.4378842814514,
40.1000786629733));
#187841=CARTESIAN_POINT('Ctrl Pts',(31.4055801226577,-54.4367263577632,
40.1001924129685));
#187842=CARTESIAN_POINT('Ctrl Pts',(31.4078138194781,-54.4355102267487,
40.10025));
#187843=CARTESIAN_POINT('Ctrl Pts',(31.4100231232069,-54.4342359163079,
40.10025));
#187844=CARTESIAN_POINT('Ctrl Pts',(29.501078514911,-51.1278468659048,40.10025));
#187845=CARTESIAN_POINT('Ctrl Pts',(29.4936027956392,-51.1321585373227,
40.10025));
#187846=CARTESIAN_POINT('Ctrl Pts',(29.4865477845229,-51.137049925875,40.099578633424));
#187847=CARTESIAN_POINT('Ctrl Pts',(29.4799806005914,-51.1423856448187,
40.0983063763363));
#187848=CARTESIAN_POINT('Ctrl Pts',(29.4757388736044,-51.1458319717793,
40.097484628799));
#187849=CARTESIAN_POINT('Ctrl Pts',(29.4717000621108,-51.1494629466902,
40.0964130309336));
#187850=CARTESIAN_POINT('Ctrl Pts',(29.4678753842638,-51.153236501246,40.0951176960923));
#187851=CARTESIAN_POINT('Ctrl Pts',(29.4628059928682,-51.1582381316478,
40.0934008039613));
#187852=CARTESIAN_POINT('Ctrl Pts',(29.4581176150989,-51.1634934604716,
40.0912909372156));
#187853=CARTESIAN_POINT('Ctrl Pts',(29.453837929136,-51.168916779284,40.0888630467851));
#187854=CARTESIAN_POINT('Ctrl Pts',(29.4516980861545,-51.1716284386902,
40.0876491015698));
#187855=CARTESIAN_POINT('Ctrl Pts',(29.4496602426632,-51.174382193724,40.0863558569271));
#187856=CARTESIAN_POINT('Ctrl Pts',(29.4477266300417,-51.1771680313592,
40.084993634277));
#187857=CARTESIAN_POINT('Ctrl Pts',(29.446759823731,-51.1785609501768,40.084312522952));
#187858=CARTESIAN_POINT('Ctrl Pts',(29.4458190608836,-51.179961897818,40.0836141747074));
#187859=CARTESIAN_POINT('Ctrl Pts',(29.4449045308659,-51.1813696738592,
40.0828999161609));
#187860=CARTESIAN_POINT('Ctrl Pts',(29.4446758983615,-51.1817216178695,
40.0827213515243));
#187861=CARTESIAN_POINT('Ctrl Pts',(29.4444489051053,-51.1820739888278,
40.0825417925841));
#187862=CARTESIAN_POINT('Ctrl Pts',(29.4442235534434,-51.1824267683258,
40.082361260236));
#187863=CARTESIAN_POINT('Ctrl Pts',(29.4435474984577,-51.1834851068199,
40.0818196631917));
#187864=CARTESIAN_POINT('Ctrl Pts',(29.4428862193406,-51.1845471213152,
40.0812693052021));
#187865=CARTESIAN_POINT('Ctrl Pts',(29.4422397658678,-51.185612322458,40.0807107531874));
#187866=CARTESIAN_POINT('Ctrl Pts',(29.4376862310784,-51.1931154617649,
40.0767763849182));
#187867=CARTESIAN_POINT('Ctrl Pts',(29.4338145801762,-51.2007799603592,
40.0724140586139));
#187868=CARTESIAN_POINT('Ctrl Pts',(29.4305579784515,-51.2085065710724,
40.0677221223771));
#187869=CARTESIAN_POINT('Ctrl Pts',(29.428978530134,-51.2122539689191,40.0654465383722));
#187870=CARTESIAN_POINT('Ctrl Pts',(29.4275440072543,-51.2160164979697,
40.063092800068));
#187871=CARTESIAN_POINT('Ctrl Pts',(29.4262483256618,-51.2197852472979,
40.0606689262479));
#187872=CARTESIAN_POINT('Ctrl Pts',(29.4242647276705,-51.2255549392044,
40.0569581447805));
#187873=CARTESIAN_POINT('Ctrl Pts',(29.4226066102323,-51.231335680589,40.0530843804605));
#187874=CARTESIAN_POINT('Ctrl Pts',(29.4212581193013,-51.2370841708899,
40.0490800251457));
#187875=CARTESIAN_POINT('Ctrl Pts',(29.4206318731367,-51.2397537995244,
40.0472203818218));
#187876=CARTESIAN_POINT('Ctrl Pts',(29.4200721889214,-51.2424163366105,
40.0453323608818));
#187877=CARTESIAN_POINT('Ctrl Pts',(29.4195787111907,-51.2450674596717,
40.0434201572162));
#187878=CARTESIAN_POINT('Ctrl Pts',(29.419540888067,-51.2452706578084,40.0432735943397));
#187879=CARTESIAN_POINT('Ctrl Pts',(29.4195034207002,-51.2454737959509,
40.0431268995707));
#187880=CARTESIAN_POINT('Ctrl Pts',(29.4194663081573,-51.2456768729756,
40.0429800745037));
#187881=CARTESIAN_POINT('Ctrl Pts',(29.4189449888201,-51.2485294929146,
40.0409176249753));
#187882=CARTESIAN_POINT('Ctrl Pts',(29.4184957101765,-51.2513705613628,
40.0388310783332));
#187883=CARTESIAN_POINT('Ctrl Pts',(29.4181151898796,-51.2541954110681,
40.036725739981));
#187884=CARTESIAN_POINT('Ctrl Pts',(29.4167507117685,-51.2643248197279,
40.0291763710723));
#187885=CARTESIAN_POINT('Ctrl Pts',(29.4162578421121,-51.2743237313746,
40.0213310894606));
#187886=CARTESIAN_POINT('Ctrl Pts',(29.4165161672808,-51.2841455249748,
40.0132837551338));
#187887=CARTESIAN_POINT('Ctrl Pts',(29.4168000406901,-51.2949386894547,
40.0044405431351));
#187888=CARTESIAN_POINT('Ctrl Pts',(29.4179908989229,-51.3055186222551,
39.9953528710635));
#187889=CARTESIAN_POINT('Ctrl Pts',(29.419980071533,-51.3158373135905,39.9861103629598));
#187890=CARTESIAN_POINT('Ctrl Pts',(29.4221278787377,-51.3269789105944,
39.976130773761));
#187891=CARTESIAN_POINT('Ctrl Pts',(29.4252064644159,-51.3378170984186,
39.9659696936077));
#187892=CARTESIAN_POINT('Ctrl Pts',(29.4291364604171,-51.3482921445171,
39.9557128217582));
#187893=CARTESIAN_POINT('Ctrl Pts',(29.4330334877913,-51.3586793157456,
39.9455419945212));
#187894=CARTESIAN_POINT('Ctrl Pts',(29.4377684584833,-51.3687106315419,
39.9352756289366));
#187895=CARTESIAN_POINT('Ctrl Pts',(29.443310811626,-51.3783102687785,39.92499));
#187896=CARTESIAN_POINT('Origin',(0.0131982271536777,0.00762000000000484,
39.92499));
#187897=CARTESIAN_POINT('Ctrl Pts',(31.4364195775134,-54.4189959163064,
40.10025));
#187898=CARTESIAN_POINT('Ctrl Pts',(31.4438560160002,-54.4146983388117,
40.10025));
#187899=CARTESIAN_POINT('Ctrl Pts',(31.4508673716606,-54.4098177483011,
40.0995859581842));
#187900=CARTESIAN_POINT('Ctrl Pts',(31.4573895320591,-54.4044907169108,
40.098327595962));
#187901=CARTESIAN_POINT('Ctrl Pts',(31.4615568820646,-54.4010869974472,
40.0975235624068));
#187902=CARTESIAN_POINT('Ctrl Pts',(31.4655251210647,-54.397501723741,40.096477705949));
#187903=CARTESIAN_POINT('Ctrl Pts',(31.4692842169746,-54.3937759157108,
40.095214991596));
#187904=CARTESIAN_POINT('Ctrl Pts',(31.4744146286225,-54.3886909353393,
40.09349163987));
#187905=CARTESIAN_POINT('Ctrl Pts',(31.4791503318821,-54.3833409297221,
40.091364392163));
#187906=CARTESIAN_POINT('Ctrl Pts',(31.4834636394928,-54.3778174666303,
40.0889118607712));
#187907=CARTESIAN_POINT('Ctrl Pts',(31.4856202932981,-54.3750557350844,
40.0876855950753));
#187908=CARTESIAN_POINT('Ctrl Pts',(31.4876715300026,-54.3722505364142,
40.0863782327526));
#187909=CARTESIAN_POINT('Ctrl Pts',(31.4896151854259,-54.3694125772948,
40.0850006373333));
#187910=CARTESIAN_POINT('Ctrl Pts',(31.4905870131376,-54.3679935977351,
40.0843118396237));
#187911=CARTESIAN_POINT('Ctrl Pts',(31.4915319606351,-54.3665664194,40.0836054919164));
#187912=CARTESIAN_POINT('Ctrl Pts',(31.4924498523887,-54.3651323262969,
40.0828829920417));
#187913=CARTESIAN_POINT('Ctrl Pts',(31.4926793253271,-54.3647738030211,
40.082702367073));
#187914=CARTESIAN_POINT('Ctrl Pts',(31.4929071076039,-54.3644148473886,
40.0825207326932));
#187915=CARTESIAN_POINT('Ctrl Pts',(31.4931331971267,-54.3640554790922,
40.0823381109275));
#187916=CARTESIAN_POINT('Ctrl Pts',(31.4938114656951,-54.3629773742029,
40.0817902456303));
#187917=CARTESIAN_POINT('Ctrl Pts',(31.4944744978649,-54.3618955562473,
40.0812334935552));
#187918=CARTESIAN_POINT('Ctrl Pts',(31.4951222515527,-54.360810548785,40.0806684524226));
#187919=CARTESIAN_POINT('Ctrl Pts',(31.4995986314374,-54.3533124740225,
40.0767636676138));
#187920=CARTESIAN_POINT('Ctrl Pts',(31.5034009004292,-54.3456575719331,
40.0724404510892));
#187921=CARTESIAN_POINT('Ctrl Pts',(31.5065976218799,-54.337942849207,40.0677949937415));
#187922=CARTESIAN_POINT('Ctrl Pts',(31.5081863836662,-54.3341086531882,
40.065486214191));
#187923=CARTESIAN_POINT('Ctrl Pts',(31.5096252947445,-54.330259136697,40.0630972003218));
#187924=CARTESIAN_POINT('Ctrl Pts',(31.5109210156001,-54.3264035847696,
40.0606363359906));
#187925=CARTESIAN_POINT('Ctrl Pts',(31.5137795693411,-54.3178976613386,
40.0552073017123));
#187926=CARTESIAN_POINT('Ctrl Pts',(31.515952667503,-54.309367230402,40.0494204304519));
#187927=CARTESIAN_POINT('Ctrl Pts',(31.5174623893716,-54.3009559572067,
40.0434049749851));
#187928=CARTESIAN_POINT('Ctrl Pts',(31.5180139098087,-54.2978832130367,
40.0412074532442));
#187929=CARTESIAN_POINT('Ctrl Pts',(31.5184846398474,-54.2948245130134,
40.0389814735788));
#187930=CARTESIAN_POINT('Ctrl Pts',(31.5188783726369,-54.2917835794183,
40.0367321210017));
#187931=CARTESIAN_POINT('Ctrl Pts',(31.520200879413,-54.2815694052536,40.029176783714));
#187932=CARTESIAN_POINT('Ctrl Pts',(31.5206547127627,-54.2714898389044,
40.0213235332575));
#187933=CARTESIAN_POINT('Ctrl Pts',(31.5203592886225,-54.2615918017969,
40.0132649215857));
#187934=CARTESIAN_POINT('Ctrl Pts',(31.5200345824972,-54.2507126865161,
40.004407552753));
#187935=CARTESIAN_POINT('Ctrl Pts',(31.5188048676547,-54.2400521939116,
39.9953016253716));
#187936=CARTESIAN_POINT('Ctrl Pts',(31.5167773687224,-54.2296591093501,
39.9860353422353));
#187937=CARTESIAN_POINT('Ctrl Pts',(31.5145936655009,-54.218465311969,39.9760551582688));
#187938=CARTESIAN_POINT('Ctrl Pts',(31.5114844302874,-54.2075805209344,
39.9658879738147));
#187939=CARTESIAN_POINT('Ctrl Pts',(31.5075265408321,-54.1970658734754,
39.9556174643242));
#187940=CARTESIAN_POINT('Ctrl Pts',(31.5036220962481,-54.1866932092591,
39.9454856413897));
#187941=CARTESIAN_POINT('Ctrl Pts',(31.498890978557,-54.1766795569339,39.935251946511));
#187942=CARTESIAN_POINT('Ctrl Pts',(31.4933613949858,-54.1671020372439,
39.92499));
#187943=CARTESIAN_POINT('Ctrl Pts',(29.7732664904679,-51.1878102687786,
39.92499));
#187944=CARTESIAN_POINT('Ctrl Pts',(29.7679746486359,-51.1786445298599,
39.9348107241715));
#187945=CARTESIAN_POINT('Ctrl Pts',(29.7619788985616,-51.1699291351242,
39.9446038383154));
#187946=CARTESIAN_POINT('Ctrl Pts',(29.7553188532225,-51.1617065245649,
39.9543158069362));
#187947=CARTESIAN_POINT('Ctrl Pts',(29.748887993471,-51.1537668706126,39.9636935671364));
#187948=CARTESIAN_POINT('Ctrl Pts',(29.7418369154195,-51.1462857370565,
39.9729968320956));
#187949=CARTESIAN_POINT('Ctrl Pts',(29.7341642916979,-51.1393284263657,
39.9821731151299));
#187950=CARTESIAN_POINT('Ctrl Pts',(29.7269112593639,-51.132751588868,39.9908475764313));
#187951=CARTESIAN_POINT('Ctrl Pts',(29.7191021335126,-51.1266422417952,
39.9994093733805));
#187952=CARTESIAN_POINT('Ctrl Pts',(29.7107129315363,-51.1210907313657,
40.0077966115799));
#187953=CARTESIAN_POINT('Ctrl Pts',(29.7029866172554,-51.1159778833935,
40.0155211172552));
#187954=CARTESIAN_POINT('Ctrl Pts',(29.694767791597,-51.1113379461933,40.0230979940978));
#187955=CARTESIAN_POINT('Ctrl Pts',(29.6860256466534,-51.1072776647637,
40.0304554104705));
#187956=CARTESIAN_POINT('Ctrl Pts',(29.683418915501,-51.1060669708027,40.0326492435152));
#187957=CARTESIAN_POINT('Ctrl Pts',(29.6807655934619,-51.1049080895608,
40.0348233715046));
#187958=CARTESIAN_POINT('Ctrl Pts',(29.6780647241927,-51.1038046002594,
40.0369753512356));
#187959=CARTESIAN_POINT('Ctrl Pts',(29.6753914511536,-51.1027123859001,
40.0391053430352));
#187960=CARTESIAN_POINT('Ctrl Pts',(29.6726744751146,-51.101675317013,40.041211089324));
#187961=CARTESIAN_POINT('Ctrl Pts',(29.6699160505199,-51.1006978225841,
40.0432881154904));
#187962=CARTESIAN_POINT('Ctrl Pts',(29.6697242350682,-51.1006298495331,
40.0434325478279));
#187963=CARTESIAN_POINT('Ctrl Pts',(29.6695322176089,-51.1005621526963,
40.0435768364421));
#187964=CARTESIAN_POINT('Ctrl Pts',(29.6693399979287,-51.1004947333604,
40.0437209807855));
#187965=CARTESIAN_POINT('Ctrl Pts',(29.6609123829953,-51.0975388226977,
40.0500407968418));
#187966=CARTESIAN_POINT('Ctrl Pts',(29.6520916749685,-51.095161351427,40.0560490279341));
#187967=CARTESIAN_POINT('Ctrl Pts',(29.6429396446305,-51.0934607157664,
40.061664710861));
#187968=CARTESIAN_POINT('Ctrl Pts',(29.6344083617435,-51.0918754277622,
40.0668995033479));
#187969=CARTESIAN_POINT('Ctrl Pts',(29.6255883681047,-51.0908783954021,
40.0717933267473));
#187970=CARTESIAN_POINT('Ctrl Pts',(29.6165418049916,-51.0905760611938,
40.0762460303063));
#187971=CARTESIAN_POINT('Ctrl Pts',(29.6132324551666,-51.090465463429,40.0778748868741));
#187972=CARTESIAN_POINT('Ctrl Pts',(29.6098929659876,-51.0904480940785,
40.0794443522244));
#187973=CARTESIAN_POINT('Ctrl Pts',(29.6065271365691,-51.0905301191541,
40.0809482021491));
#187974=CARTESIAN_POINT('Ctrl Pts',(29.6057177670366,-51.0905498434446,
40.0813098278168));
#187975=CARTESIAN_POINT('Ctrl Pts',(29.6049064053145,-51.0905756628929,
40.0816679525671));
#187976=CARTESIAN_POINT('Ctrl Pts',(29.6040931741702,-51.0906076352718,
40.082022419258));
#187977=CARTESIAN_POINT('Ctrl Pts',(29.6033053564991,-51.0906386085138,
40.0823658088647));
#187978=CARTESIAN_POINT('Ctrl Pts',(29.6025157844404,-51.0906753561239,
40.0827057654616));
#187979=CARTESIAN_POINT('Ctrl Pts',(29.6017245728792,-51.0907179287116,
40.083042147015));
#187980=CARTESIAN_POINT('Ctrl Pts',(29.5930559358432,-51.0911843606098,
40.0867275956808));
#187981=CARTESIAN_POINT('Ctrl Pts',(29.5841848213163,-51.0923507190418,
40.0899823432035));
#187982=CARTESIAN_POINT('Ctrl Pts',(29.5752911628152,-51.094273199721,40.0926299529361));
#187983=CARTESIAN_POINT('Ctrl Pts',(29.5716026975442,-51.0950705097614,
40.0937279956087));
#187984=CARTESIAN_POINT('Ctrl Pts',(29.5679105139256,-51.0959974771976,
40.0947220371803));
#187985=CARTESIAN_POINT('Ctrl Pts',(29.5642276868789,-51.0970562972091,
40.0956014538692));
#187986=CARTESIAN_POINT('Ctrl Pts',(29.5579462415721,-51.0988622250758,
40.097101390674));
#187987=CARTESIAN_POINT('Ctrl Pts',(29.5516941764754,-51.1010529624041,
40.0982667904316));
#187988=CARTESIAN_POINT('Ctrl Pts',(29.5455435225216,-51.1036389246275,
40.0990539325582));
#187989=CARTESIAN_POINT('Ctrl Pts',(29.5424681955447,-51.1049319057392,
40.0994475036216));
#187990=CARTESIAN_POINT('Ctrl Pts',(29.5394188854256,-51.1063249785076,
40.0997467259952));
#187991=CARTESIAN_POINT('Ctrl Pts',(29.5364046579954,-51.1078194668127,
40.0999473488896));
#187992=CARTESIAN_POINT('Ctrl Pts',(29.5333904305653,-51.1093139551177,
40.100147971784));
#187993=CARTESIAN_POINT('Ctrl Pts',(29.5304113137792,-51.1109098228567,
40.10025));
#187994=CARTESIAN_POINT('Ctrl Pts',(29.5274749692184,-51.1126068659048,
40.10025));
#187995=CARTESIAN_POINT('Origin',(23.6840886581935,-53.2328030451448,39.92499));
#187996=CARTESIAN_POINT('Ctrl Pts',(25.3107727110821,-57.317288315449,39.92499));
#187997=CARTESIAN_POINT('Ctrl Pts',(25.3150883208945,-57.3269813337896,
39.9348354642016));
#187998=CARTESIAN_POINT('Ctrl Pts',(25.3201559369468,-57.3363050752407,
39.9446440828455));
#187999=CARTESIAN_POINT('Ctrl Pts',(25.3259384683616,-57.3452135417177,
39.9543641760326));
#188000=CARTESIAN_POINT('Ctrl Pts',(25.3315331019382,-57.3538325360806,
39.9637684240707));
#188001=CARTESIAN_POINT('Ctrl Pts',(25.3377977038115,-57.3620638476571,
39.9730909636389));
#188002=CARTESIAN_POINT('Ctrl Pts',(25.3447390861647,-57.3698434251105,
39.9822808977133));
#188003=CARTESIAN_POINT('Ctrl Pts',(25.3513052064451,-57.3772024263426,
39.9909740094641));
#188004=CARTESIAN_POINT('Ctrl Pts',(25.3584775246705,-57.3841579102003,
39.9995492764992));
#188005=CARTESIAN_POINT('Ctrl Pts',(25.3662887884588,-57.3906233351686,
40.0079462328685));
#188006=CARTESIAN_POINT('Ctrl Pts',(25.3734835273328,-57.3965784591557,
40.015680436968));
#188007=CARTESIAN_POINT('Ctrl Pts',(25.3812207968871,-57.4021181432088,
40.0232638017412));
#188008=CARTESIAN_POINT('Ctrl Pts',(25.3895423083593,-57.4071400767268,
40.0306257269956));
#188009=CARTESIAN_POINT('Ctrl Pts',(25.3919560625135,-57.4085967487426,
40.0327611416645));
#188010=CARTESIAN_POINT('Ctrl Pts',(25.3944190600984,-57.4100096047774,
40.0348777427267));
#188011=CARTESIAN_POINT('Ctrl Pts',(25.3969325220924,-57.4113754784546,
40.0369733168701));
#188012=CARTESIAN_POINT('Ctrl Pts',(25.3996572764942,-57.4128561733381,
40.039245053974));
#188013=CARTESIAN_POINT('Ctrl Pts',(25.4024370309187,-57.414280541844,40.041487875195));
#188014=CARTESIAN_POINT('Ctrl Pts',(25.4052723227226,-57.4156446191417,
40.04369857016));
#188015=CARTESIAN_POINT('Ctrl Pts',(25.4130538033266,-57.4193883399888,
40.0497658398386));
#188016=CARTESIAN_POINT('Ctrl Pts',(25.4212623406656,-57.4226343338643,
40.0555581699984));
#188017=CARTESIAN_POINT('Ctrl Pts',(25.4298341608309,-57.4253008212879,
40.0609828468885));
#188018=CARTESIAN_POINT('Ctrl Pts',(25.4376769109071,-57.4277405125134,
40.0659461317303));
#188019=CARTESIAN_POINT('Ctrl Pts',(25.4458193604262,-57.4296843862652,
40.0706039980704));
#188020=CARTESIAN_POINT('Ctrl Pts',(25.4542377154365,-57.4310470526567,
40.07488431806));
#188021=CARTESIAN_POINT('Ctrl Pts',(25.4583727839181,-57.4317163899369,
40.0769867972567));
#188022=CARTESIAN_POINT('Ctrl Pts',(25.4625743171739,-57.4322449980037,
40.0789976708173));
#188023=CARTESIAN_POINT('Ctrl Pts',(25.4668384019351,-57.4326195921322,
40.0809050491499));
#188024=CARTESIAN_POINT('Ctrl Pts',(25.4676474704857,-57.4326906677195,
40.0812669556104));
#188025=CARTESIAN_POINT('Ctrl Pts',(25.4684592045965,-57.4327558640763,
40.0816253922032));
#188026=CARTESIAN_POINT('Ctrl Pts',(25.4692734860654,-57.4328151061496,
40.0819801989139));
#188027=CARTESIAN_POINT('Ctrl Pts',(25.4700623212384,-57.432872496908,40.0823239179149));
#188028=CARTESIAN_POINT('Ctrl Pts',(25.4708535470246,-57.4329242997218,
40.0826642303498));
#188029=CARTESIAN_POINT('Ctrl Pts',(25.471647052459,-57.4329704479394,40.0830009916099));
#188030=CARTESIAN_POINT('Ctrl Pts',(25.4802945111775,-57.4334733617057,
40.0866709464313));
#188031=CARTESIAN_POINT('Ctrl Pts',(25.489218417506,-57.4333046542889,40.089917583188));
#188032=CARTESIAN_POINT('Ctrl Pts',(25.4982455208455,-57.4323852136912,
40.0925642067065));
#188033=CARTESIAN_POINT('Ctrl Pts',(25.5020577226409,-57.4319969282174,
40.0936818922529));
#188034=CARTESIAN_POINT('Ctrl Pts',(25.505888119947,-57.4314751387427,40.0946930094791));
#188035=CARTESIAN_POINT('Ctrl Pts',(25.5097232095986,-57.4308157710841,
40.0955863397545));
#188036=CARTESIAN_POINT('Ctrl Pts',(25.5161814047441,-57.4297054124226,
40.0970906856166));
#188037=CARTESIAN_POINT('Ctrl Pts',(25.5226508554408,-57.4282034292356,
40.0982599215483));
#188038=CARTESIAN_POINT('Ctrl Pts',(25.5290599831064,-57.426290210937,40.0990497370453));
#188039=CARTESIAN_POINT('Ctrl Pts',(25.5306622650228,-57.4258119063624,
40.0992471909196));
#188040=CARTESIAN_POINT('Ctrl Pts',(25.532260695287,-57.4253076802625,40.0994209989363));
#188041=CARTESIAN_POINT('Ctrl Pts',(25.5338540367011,-57.4247769415292,
40.0995705982975));
#188042=CARTESIAN_POINT('Ctrl Pts',(25.5362440488221,-57.4239808334292,
40.0997949973393));
#188043=CARTESIAN_POINT('Ctrl Pts',(25.5386225912894,-57.423125065972,40.0999649129781));
#188044=CARTESIAN_POINT('Ctrl Pts',(25.5409861542582,-57.4222091845947,
40.1000786629733));
#188045=CARTESIAN_POINT('Ctrl Pts',(25.543349717227,-57.4212933032174,40.1001924129685));
#188046=CARTESIAN_POINT('Ctrl Pts',(25.5456982979279,-57.4203173191901,
40.10025));
#188047=CARTESIAN_POINT('Ctrl Pts',(25.5480287005717,-57.419280924679,40.10025));
#188048=CARTESIAN_POINT('Ctrl Pts',(23.9951532569806,-53.9314655730805,
40.10025));
#188049=CARTESIAN_POINT('Ctrl Pts',(23.9872677980943,-53.9349721992637,
40.10025));
#188050=CARTESIAN_POINT('Ctrl Pts',(23.9797401457389,-53.939099342807,40.0995786334241));
#188051=CARTESIAN_POINT('Ctrl Pts',(23.972651203027,-53.9437193744793,40.0983063763366));
#188052=CARTESIAN_POINT('Ctrl Pts',(23.9680724734026,-53.9467034408969,
40.0974846287992));
#188053=CARTESIAN_POINT('Ctrl Pts',(23.9636762467129,-53.9498923541889,
40.0964130309338));
#188054=CARTESIAN_POINT('Ctrl Pts',(23.9594780769922,-53.9532454491205,
40.0951176960924));
#188055=CARTESIAN_POINT('Ctrl Pts',(23.9539136435133,-53.9576897843753,
40.0934008039614));
#188056=CARTESIAN_POINT('Ctrl Pts',(23.948701617722,-53.9624262550345,40.0912909372156));
#188057=CARTESIAN_POINT('Ctrl Pts',(23.9438784851453,-53.967372515342,40.0888630467851));
#188058=CARTESIAN_POINT('Ctrl Pts',(23.9414669188569,-53.9698456454958,
40.0876491015699));
#188059=CARTESIAN_POINT('Ctrl Pts',(23.9391523931036,-53.9723713025228,
40.0863558569271));
#188060=CARTESIAN_POINT('Ctrl Pts',(23.9369381736874,-53.9749397614922,
40.0849936342771));
#188061=CARTESIAN_POINT('Ctrl Pts',(23.9358310639794,-53.9762239909768,
40.0843125229521));
#188062=CARTESIAN_POINT('Ctrl Pts',(23.9347490158252,-53.9775189275856,
40.0836141747074));
#188063=CARTESIAN_POINT('Ctrl Pts',(23.9336923430325,-53.978823397265,40.0828999161609));
#188064=CARTESIAN_POINT('Ctrl Pts',(23.9334281748343,-53.9791495146848,
40.0827213515243));
#188065=CARTESIAN_POINT('Ctrl Pts',(23.9331655922761,-53.9794762280618,
40.0825417925842));
#188066=CARTESIAN_POINT('Ctrl Pts',(23.9329045996154,-53.979803519334,40.082361260236));
#188067=CARTESIAN_POINT('Ctrl Pts',(23.9321216216332,-53.9807853931503,
40.0818196631917));
#188068=CARTESIAN_POINT('Ctrl Pts',(23.9313529543291,-53.9817724673292,
40.0812693052021));
#188069=CARTESIAN_POINT('Ctrl Pts',(23.9305986983576,-53.9827642604005,
40.0807107531874));
#188070=CARTESIAN_POINT('Ctrl Pts',(23.9252858166868,-53.9897503227312,
40.0767763849182));
#188071=CARTESIAN_POINT('Ctrl Pts',(23.9206342168336,-53.9969681366812,
40.0724140586139));
#188072=CARTESIAN_POINT('Ctrl Pts',(23.9165878043697,-54.0043120126387,
40.0677221223771));
#188073=CARTESIAN_POINT('Ctrl Pts',(23.9146252986972,-54.0078737845424,
40.0654465383723));
#188074=CARTESIAN_POINT('Ctrl Pts',(23.9128053429043,-54.0114657535931,
40.063092800068));
#188075=CARTESIAN_POINT('Ctrl Pts',(23.9111228176154,-54.0150784217125,
40.0606689262479));
#188076=CARTESIAN_POINT('Ctrl Pts',(23.9085469889529,-54.0206091641932,
40.0569581447806));
#188077=CARTESIAN_POINT('Ctrl Pts',(23.906293702842,-54.0261849176039,40.0530843804606));
#188078=CARTESIAN_POINT('Ctrl Pts',(23.9043517182282,-54.0317609613887,
40.0490800251458));
#188079=CARTESIAN_POINT('Ctrl Pts',(23.903449850527,-54.034350504969,40.0472203818218));
#188080=CARTESIAN_POINT('Ctrl Pts',(23.9026149214104,-54.0369399534675,
40.0453323608818));
#188081=CARTESIAN_POINT('Ctrl Pts',(23.9018470291827,-54.0395249709303,
40.0434201572162));
#188082=CARTESIAN_POINT('Ctrl Pts',(23.9017881732692,-54.0397231023333,
40.0432735943397));
#188083=CARTESIAN_POINT('Ctrl Pts',(23.9017296774346,-54.0399212112576,
40.0431268995707));
#188084=CARTESIAN_POINT('Ctrl Pts',(23.9016715408688,-54.040119296488,40.0429800745037));
#188085=CARTESIAN_POINT('Ctrl Pts',(23.9008548973949,-54.0429017967673,
40.0409176249753));
#188086=CARTESIAN_POINT('Ctrl Pts',(23.9001111074278,-54.045680339139,40.0388310783332));
#188087=CARTESIAN_POINT('Ctrl Pts',(23.8994373944623,-54.0484499388202,
40.036725739981));
#188088=CARTESIAN_POINT('Ctrl Pts',(23.8970215795839,-54.0583812307199,
40.029176371072));
#188089=CARTESIAN_POINT('Ctrl Pts',(23.8954862390503,-54.068273848375,40.02133108946));
#188090=CARTESIAN_POINT('Ctrl Pts',(23.8947164920951,-54.0780688394955,
40.0132837551328));
#188091=CARTESIAN_POINT('Ctrl Pts',(23.8938706175193,-54.0888325507427,
40.0044405431337));
#188092=CARTESIAN_POINT('Ctrl Pts',(23.8939490479891,-54.0994790041457,
39.9953528710617));
#188093=CARTESIAN_POINT('Ctrl Pts',(23.8948487267555,-54.1099490937668,
39.9861103629577));
#188094=CARTESIAN_POINT('Ctrl Pts',(23.8958201540346,-54.1212541629234,
39.9761307737585));
#188095=CARTESIAN_POINT('Ctrl Pts',(23.8977489757806,-54.132354777851,39.9659696936048));
#188096=CARTESIAN_POINT('Ctrl Pts',(23.9005625023815,-54.1431832369939,
39.955712821755));
#188097=CARTESIAN_POINT('Ctrl Pts',(23.9033524263857,-54.153920856493,39.945541994519));
#188098=CARTESIAN_POINT('Ctrl Pts',(23.9070129003878,-54.1643921589007,
39.9352756289355));
#188099=CARTESIAN_POINT('Ctrl Pts',(23.9115214566113,-54.174518541976,39.92499));
#188100=CARTESIAN_POINT('Origin',(0.0139224327744766,0.00619866644048029,
39.92499));
#188101=CARTESIAN_POINT('Ctrl Pts',(25.5758735661207,-57.406883591798,40.10025));
#188102=CARTESIAN_POINT('Ctrl Pts',(25.5837184861912,-57.4033868763695,
40.10025));
#188103=CARTESIAN_POINT('Ctrl Pts',(25.591201593538,-57.3992659084767,40.0995859581841));
#188104=CARTESIAN_POINT('Ctrl Pts',(25.5982448512649,-57.394649810525,40.0983275959618));
#188105=CARTESIAN_POINT('Ctrl Pts',(25.6027451576555,-57.391700343685,40.0975235624066));
#188106=CARTESIAN_POINT('Ctrl Pts',(25.6070664213775,-57.3885495044081,
40.0964777059489));
#188107=CARTESIAN_POINT('Ctrl Pts',(25.611194377554,-57.3852370392633,40.0952149915961));
#188108=CARTESIAN_POINT('Ctrl Pts',(25.6168282094542,-57.3807161889917,
40.0934916398701));
#188109=CARTESIAN_POINT('Ctrl Pts',(25.6220971979014,-57.3758905070493,
40.0913643921631));
#188110=CARTESIAN_POINT('Ctrl Pts',(25.6269642358707,-57.3708481654824,
40.0889118607713));
#188111=CARTESIAN_POINT('Ctrl Pts',(25.6293977548553,-57.3683269946989,
40.0876855950754));
#188112=CARTESIAN_POINT('Ctrl Pts',(25.6317309777765,-57.3657515758211,
40.0863782327527));
#188113=CARTESIAN_POINT('Ctrl Pts',(25.6339606331577,-57.3631323306532,
40.0850006373334));
#188114=CARTESIAN_POINT('Ctrl Pts',(25.6350754608483,-57.3618227080692,
40.0843118396237));
#188115=CARTESIAN_POINT('Ctrl Pts',(25.6361644125826,-57.3605021218762,
40.0836054919164));
#188116=CARTESIAN_POINT('Ctrl Pts',(25.6372271795775,-57.3591718306995,
40.0828829920417));
#188117=CARTESIAN_POINT('Ctrl Pts',(25.6374928713262,-57.3588392579054,
40.0827023670731));
#188118=CARTESIAN_POINT('Ctrl Pts',(25.6377569268685,-57.3585060784008,
40.0825207326933));
#188119=CARTESIAN_POINT('Ctrl Pts',(25.638019342065,-57.3581723115519,40.0823381109275));
#188120=CARTESIAN_POINT('Ctrl Pts',(25.6388065876546,-57.3571710110051,
40.0817902456303));
#188121=CARTESIAN_POINT('Ctrl Pts',(25.6395790684331,-57.3561644250953,
40.0812334935553));
#188122=CARTESIAN_POINT('Ctrl Pts',(25.6403366878211,-57.355153070115,40.0806684524227));
#188123=CARTESIAN_POINT('Ctrl Pts',(25.6455723078611,-57.3481639797005,
40.0767636676137));
#188124=CARTESIAN_POINT('Ctrl Pts',(25.6501539027776,-57.3409484573,40.0724404510888));
#188125=CARTESIAN_POINT('Ctrl Pts',(25.6541395203649,-57.3336101450126,
40.0677949937409));
#188126=CARTESIAN_POINT('Ctrl Pts',(25.6561203613654,-57.3299630239491,
40.0654862141906));
#188127=CARTESIAN_POINT('Ctrl Pts',(25.6579537739812,-57.3262850026762,
40.0630972003216));
#188128=CARTESIAN_POINT('Ctrl Pts',(25.6596454116602,-57.3225860115759,
40.0606363359906));
#188129=CARTESIAN_POINT('Ctrl Pts',(25.6633774170497,-57.3144254847132,
40.0552073017123));
#188130=CARTESIAN_POINT('Ctrl Pts',(25.6664302835893,-57.3061689349812,
40.0494204304519));
#188131=CARTESIAN_POINT('Ctrl Pts',(25.6688109525047,-57.2979615485274,
40.0434049749851));
#188132=CARTESIAN_POINT('Ctrl Pts',(25.6696806408813,-57.2949632867552,
40.0412074532442));
#188133=CARTESIAN_POINT('Ctrl Pts',(25.6704685134247,-57.2919705472983,
40.0389814735788));
#188134=CARTESIAN_POINT('Ctrl Pts',(25.6711779534203,-57.288987428539,40.0367321210017));
#188135=CARTESIAN_POINT('Ctrl Pts',(25.673560887295,-57.2789674482903,40.029176783714));
#188136=CARTESIAN_POINT('Ctrl Pts',(25.6750658360791,-57.268990537363,40.0213235332575));
#188137=CARTESIAN_POINT('Ctrl Pts',(25.6758066569115,-57.2591158425071,
40.0132649215858));
#188138=CARTESIAN_POINT('Ctrl Pts',(25.6766209067623,-57.248262383126,40.0044075527531));
#188139=CARTESIAN_POINT('Ctrl Pts',(25.676512253336,-57.2375317496128,39.9953016253718));
#188140=CARTESIAN_POINT('Ctrl Pts',(25.6755822344129,-57.2269836681084,
39.9860353422355));
#188141=CARTESIAN_POINT('Ctrl Pts',(25.6745805641845,-57.2156229323787,
39.9760551582691));
#188142=CARTESIAN_POINT('Ctrl Pts',(25.6726261321667,-57.2044727657896,
39.9658879738151));
#188143=CARTESIAN_POINT('Ctrl Pts',(25.6697890043847,-57.1936020065669,
39.9556174643248));
#188144=CARTESIAN_POINT('Ctrl Pts',(25.6669901874071,-57.1828780392979,
39.94548564139));
#188145=CARTESIAN_POINT('Ctrl Pts',(25.6633316989628,-57.1724247063458,
39.9352519465111));
#188146=CARTESIAN_POINT('Ctrl Pts',(25.658833530444,-57.1623216544372,39.92499));
#188147=CARTESIAN_POINT('Ctrl Pts',(24.2595822759732,-54.0195518809642,
39.92499));
#188148=CARTESIAN_POINT('Ctrl Pts',(24.2552775040085,-54.0098832048283,
39.9348107241709));
#188149=CARTESIAN_POINT('Ctrl Pts',(24.2502256060993,-54.000588827396,39.9446038383143));
#188150=CARTESIAN_POINT('Ctrl Pts',(24.2444615420317,-53.9917150968536,
39.9543158069345));
#188151=CARTESIAN_POINT('Ctrl Pts',(24.2388958310295,-53.9831467292694,
39.9636935671344));
#188152=CARTESIAN_POINT('Ctrl Pts',(24.2326653709158,-53.9749695397927,
39.9729968320933));
#188153=CARTESIAN_POINT('Ctrl Pts',(24.2257620156251,-53.9672483344113,
39.9821731151272));
#188154=CARTESIAN_POINT('Ctrl Pts',(24.2192361828782,-53.9599493771937,
39.9908475764284));
#188155=CARTESIAN_POINT('Ctrl Pts',(24.2121084368968,-53.9530572218387,
39.9994093733774));
#188156=CARTESIAN_POINT('Ctrl Pts',(24.2043454827012,-53.9466592127736,
40.0077966115766));
#188157=CARTESIAN_POINT('Ctrl Pts',(24.1971959321202,-53.9407667537592,
40.0155211172517));
#188158=CARTESIAN_POINT('Ctrl Pts',(24.1895071355543,-53.9352931334045,
40.0230979940941));
#188159=CARTESIAN_POINT('Ctrl Pts',(24.1812372959741,-53.9303412916448,
40.0304554104666));
#188160=CARTESIAN_POINT('Ctrl Pts',(24.1787713967456,-53.9288647523895,
40.0326492435127));
#188161=CARTESIAN_POINT('Ctrl Pts',(24.1762537459562,-53.9274348719442,
40.0348233715034));
#188162=CARTESIAN_POINT('Ctrl Pts',(24.1736830183708,-53.9260551099576,
40.0369753512355));
#188163=CARTESIAN_POINT('Ctrl Pts',(24.1711385572897,-53.9246894457402,
40.0391053430352));
#188164=CARTESIAN_POINT('Ctrl Pts',(24.1685448683467,-53.923374056695,40.041211089324));
#188165=CARTESIAN_POINT('Ctrl Pts',(24.1659037306811,-53.9221135831988,
40.0432881154904));
#188166=CARTESIAN_POINT('Ctrl Pts',(24.1657200711331,-53.922025932337,40.043432547828));
#188167=CARTESIAN_POINT('Ctrl Pts',(24.1655361818118,-53.9219385350606,
40.0435768364421));
#188168=CARTESIAN_POINT('Ctrl Pts',(24.1653520623708,-53.9218513926271,
40.0437209807855));
#188169=CARTESIAN_POINT('Ctrl Pts',(24.1572795915928,-53.9180307491142,
40.0500407968419));
#188170=CARTESIAN_POINT('Ctrl Pts',(24.1487557177458,-53.9147442868248,
40.0560490279343));
#188171=CARTESIAN_POINT('Ctrl Pts',(24.1398315880196,-53.9120963197573,
40.0616647108613));
#188172=CARTESIAN_POINT('Ctrl Pts',(24.1315127481117,-53.9096279542368,
40.0668995033482));
#188173=CARTESIAN_POINT('Ctrl Pts',(24.1228452895811,-53.9077144433431,
40.0717933267478));
#188174=CARTESIAN_POINT('Ctrl Pts',(24.1138798870173,-53.9064681420132,
40.0762460303068));
#188175=CARTESIAN_POINT('Ctrl Pts',(24.1106002267716,-53.906012228863,40.0778748868745));
#188176=CARTESIAN_POINT('Ctrl Pts',(24.1072808472556,-53.9056458829916,
40.0794443522246));
#188177=CARTESIAN_POINT('Ctrl Pts',(24.103924882248,-53.9053756337486,40.0809482021492));
#188178=CARTESIAN_POINT('Ctrl Pts',(24.1031178847767,-53.9053106478339,
40.0813098278168));
#188179=CARTESIAN_POINT('Ctrl Pts',(24.1023082689118,-53.9052515154466,
40.0816679525672));
#188180=CARTESIAN_POINT('Ctrl Pts',(24.1014961507091,-53.9051983068757,
40.0820224192581));
#188181=CARTESIAN_POINT('Ctrl Pts',(24.1007094112003,-53.9051467610726,
40.0823658088648));
#188182=CARTESIAN_POINT('Ctrl Pts',(24.0999203233287,-53.9051007746215,
40.0827057654617));
#188183=CARTESIAN_POINT('Ctrl Pts',(24.0991289960601,-53.9050604098635,
40.0830421470151));
#188184=CARTESIAN_POINT('Ctrl Pts',(24.0904590913157,-53.9046181672909,
40.0867275956807));
#188185=CARTESIAN_POINT('Ctrl Pts',(24.0815146560285,-53.9048508523204,
40.0899823432031));
#188186=CARTESIAN_POINT('Ctrl Pts',(24.0724687639687,-53.9058331609932,
40.0926299529357));
#188187=CARTESIAN_POINT('Ctrl Pts',(24.0687171629025,-53.9062405536792,
40.0937279956085));
#188188=CARTESIAN_POINT('Ctrl Pts',(24.0649483109699,-53.9067765048111,
40.0947220371803));
#188189=CARTESIAN_POINT('Ctrl Pts',(24.0611749820059,-53.9074445642442,
40.0956014538692));
#188190=CARTESIAN_POINT('Ctrl Pts',(24.0547391762491,-53.9085840092241,
40.097101390674));
#188191=CARTESIAN_POINT('Ctrl Pts',(24.0482923662128,-53.9101092267073,
40.0982667904316));
#188192=CARTESIAN_POINT('Ctrl Pts',(24.0419050995277,-53.9120381043533,
40.0990539325582));
#188193=CARTESIAN_POINT('Ctrl Pts',(24.0387114661851,-53.9130025431763,
40.0994475036216));
#188194=CARTESIAN_POINT('Ctrl Pts',(24.0355332447502,-53.9140692448455,
40.0997467259952));
#188195=CARTESIAN_POINT('Ctrl Pts',(24.0323793130074,-53.915240473626,40.0999473488896));
#188196=CARTESIAN_POINT('Ctrl Pts',(24.0292253812646,-53.9164117024065,
40.100147971784));
#188197=CARTESIAN_POINT('Ctrl Pts',(24.0260957707896,-53.9176874253154,
40.10025));
#188198=CARTESIAN_POINT('Ctrl Pts',(24.0229981225296,-53.9190682401995,
40.10025));
#188199=CARTESIAN_POINT('Origin',(17.9900016446781,-55.4168495715592,39.92499));
#188200=CARTESIAN_POINT('Ctrl Pts',(19.180829583578,-59.6489943884565,39.92499));
#188201=CARTESIAN_POINT('Ctrl Pts',(19.1841083557168,-59.65908541149,39.9348354642015));
#188202=CARTESIAN_POINT('Ctrl Pts',(19.1881736144723,-59.6688877866282,
39.9446440828453));
#188203=CARTESIAN_POINT('Ctrl Pts',(19.192993280264,-59.6783518907163,39.9543641760323));
#188204=CARTESIAN_POINT('Ctrl Pts',(19.1976563356167,-59.6875084677765,
39.9637684240702));
#188205=CARTESIAN_POINT('Ctrl Pts',(19.2030262129956,-59.6963495165736,
39.9730909636384));
#188206=CARTESIAN_POINT('Ctrl Pts',(19.2091163824538,-59.704812048718,39.9822808977126));
#188207=CARTESIAN_POINT('Ctrl Pts',(19.2148773077502,-59.7128170830339,
39.9909740094633));
#188208=CARTESIAN_POINT('Ctrl Pts',(19.2212832892268,-59.7204841754253,
39.9995492764982));
#188209=CARTESIAN_POINT('Ctrl Pts',(19.2283759411582,-59.727730681519,40.0079462328674));
#188210=CARTESIAN_POINT('Ctrl Pts',(19.2349087865407,-59.7344052377118,
40.0156804369667));
#188211=CARTESIAN_POINT('Ctrl Pts',(19.2420246158616,-59.7407233396923,
40.0232638017398));
#188212=CARTESIAN_POINT('Ctrl Pts',(19.2497756062298,-59.7465875973392,
40.030625726994));
#188213=CARTESIAN_POINT('Ctrl Pts',(19.2520238738993,-59.7482885955661,
40.0327611416634));
#188214=CARTESIAN_POINT('Ctrl Pts',(19.2543256952561,-59.7499511651806,
40.0348777427262));
#188215=CARTESIAN_POINT('Ctrl Pts',(19.2566826155664,-59.751572284779,40.03697331687));
#188216=CARTESIAN_POINT('Ctrl Pts',(19.2592376687177,-59.7533296826513,
40.039245053974));
#188217=CARTESIAN_POINT('Ctrl Pts',(19.2618533083056,-59.7550368117758,
40.041487875195));
#188218=CARTESIAN_POINT('Ctrl Pts',(19.2645304831806,-59.7566897852104,
40.0436985701601));
#188219=CARTESIAN_POINT('Ctrl Pts',(19.2718780106326,-59.7612263837725,
40.0497658398386));
#188220=CARTESIAN_POINT('Ctrl Pts',(19.2797022819936,-59.7653126215476,
40.0555581699984));
#188221=CARTESIAN_POINT('Ctrl Pts',(19.2879484209985,-59.7688605008634,
40.0609828468886));
#188222=CARTESIAN_POINT('Ctrl Pts',(19.2954931904948,-59.7721066178186,
40.0659461317306));
#188223=CARTESIAN_POINT('Ctrl Pts',(19.3033878446878,-59.7748909605621,
40.0706039980708));
#188224=CARTESIAN_POINT('Ctrl Pts',(19.3116176456451,-59.777126119837,40.0748843180606));
#188225=CARTESIAN_POINT('Ctrl Pts',(19.3156600969912,-59.7782240227714,
40.0769867972572));
#188226=CARTESIAN_POINT('Ctrl Pts',(19.3197833592189,-59.7791889148824,
40.0789976708176));
#188227=CARTESIAN_POINT('Ctrl Pts',(19.3239849291286,-59.7800071751723,
40.08090504915));
#188228=CARTESIAN_POINT('Ctrl Pts',(19.3247821360952,-59.7801624320923,
40.0812669556105));
#188229=CARTESIAN_POINT('Ctrl Pts',(19.3255826085666,-59.7803121206159,
40.0816253922033));
#188230=CARTESIAN_POINT('Ctrl Pts',(19.3263862368335,-59.7804561537455,
40.0819801989139));
#188231=CARTESIAN_POINT('Ctrl Pts',(19.3271647517172,-59.7805956858397,
40.0823239179149));
#188232=CARTESIAN_POINT('Ctrl Pts',(19.3279462282172,-59.7807299104878,
40.0826642303498));
#188233=CARTESIAN_POINT('Ctrl Pts',(19.3287305629435,-59.7808587498043,
40.0830009916099));
#188234=CARTESIAN_POINT('Ctrl Pts',(19.3372780811747,-59.7822628141273,
40.0866709464312));
#188235=CARTESIAN_POINT('Ctrl Pts',(19.3461707361371,-59.7830278331223,
40.0899175831877));
#188236=CARTESIAN_POINT('Ctrl Pts',(19.3552444957723,-59.7830570185563,
40.0925642067061));
#188237=CARTESIAN_POINT('Ctrl Pts',(19.3590764008117,-59.7830693437464,
40.0936818922527));
#188238=CARTESIAN_POINT('Ctrl Pts',(19.3629403566531,-59.7829507982331,
40.094693009479));
#188239=CARTESIAN_POINT('Ctrl Pts',(19.3668233599709,-59.7826959186872,
40.0955863397546));
#188240=CARTESIAN_POINT('Ctrl Pts',(19.3733622405322,-59.7822667079007,
40.0970906856167));
#188241=CARTESIAN_POINT('Ctrl Pts',(19.3799532508955,-59.7814491944743,
40.0982599215483));
#188242=CARTESIAN_POINT('Ctrl Pts',(19.3865272544576,-59.7802163932509,
40.0990497370454));
#188243=CARTESIAN_POINT('Ctrl Pts',(19.3881707553481,-59.7799081929451,
40.0992471909196));
#188244=CARTESIAN_POINT('Ctrl Pts',(19.3898131352235,-59.7795738105078,
40.0994209989363));
#188245=CARTESIAN_POINT('Ctrl Pts',(19.3914532254508,-59.7792125287463,
40.0995705982975));
#188246=CARTESIAN_POINT('Ctrl Pts',(19.3939133607917,-59.778670606104,40.0997949973393));
#188247=CARTESIAN_POINT('Ctrl Pts',(19.3963683254117,-59.7780681520195,
40.0999649129781));
#188248=CARTESIAN_POINT('Ctrl Pts',(19.3988146762082,-59.7774043475413,
40.1000786629733));
#188249=CARTESIAN_POINT('Ctrl Pts',(19.4012610270047,-59.7767405430631,
40.1001924129685));
#188250=CARTESIAN_POINT('Ctrl Pts',(19.4036987600453,-59.7760153991102,
40.10025));
#188251=CARTESIAN_POINT('Ctrl Pts',(19.4061247292252,-59.7752282754837,
40.10025));
#188252=CARTESIAN_POINT('Ctrl Pts',(18.2263320786581,-56.1441998575528,
40.10025));
#188253=CARTESIAN_POINT('Ctrl Pts',(18.2181232748944,-56.1468630191713,
40.10025));
#188254=CARTESIAN_POINT('Ctrl Pts',(18.2102054558341,-56.1501806998577,
40.0995786334241));
#188255=CARTESIAN_POINT('Ctrl Pts',(18.2026724222811,-56.1540344262252,
40.0983063763366));
#188256=CARTESIAN_POINT('Ctrl Pts',(18.1978068555398,-56.1565235380435,
40.0974846287993));
#188257=CARTESIAN_POINT('Ctrl Pts',(18.1931013796339,-56.1592354513147,
40.0964130309338));
#188258=CARTESIAN_POINT('Ctrl Pts',(18.1885757140657,-56.162131349412,40.0951176960924));
#188259=CARTESIAN_POINT('Ctrl Pts',(18.1825772036012,-56.1659696964527,
40.0934008039614));
#188260=CARTESIAN_POINT('Ctrl Pts',(18.1768986338332,-56.1701354151836,
40.0912909372157));
#188261=CARTESIAN_POINT('Ctrl Pts',(18.1715848978926,-56.1745504247233,
40.0888630467852));
#188262=CARTESIAN_POINT('Ctrl Pts',(18.1689280299222,-56.1767579294931,
40.0876491015699));
#188263=CARTESIAN_POINT('Ctrl Pts',(18.1663621803353,-56.1790278168865,
40.0863558569272));
#188264=CARTESIAN_POINT('Ctrl Pts',(18.1638916135758,-56.1813507566159,
40.0849936342771));
#188265=CARTESIAN_POINT('Ctrl Pts',(18.1626563301961,-56.1825122264807,
40.0843125229521));
#188266=CARTESIAN_POINT('Ctrl Pts',(18.1614448518812,-56.1836869644604,
40.0836141747074));
#188267=CARTESIAN_POINT('Ctrl Pts',(18.1602576134416,-56.1848738357352,
40.082899916161));
#188268=CARTESIAN_POINT('Ctrl Pts',(18.1599608038317,-56.1851705535539,
40.0827213515244));
#188269=CARTESIAN_POINT('Ctrl Pts',(18.159665508881,-56.1854680298096,40.0825417925842));
#188270=CARTESIAN_POINT('Ctrl Pts',(18.1593717347116,-56.1857662469842,
40.0823612602361));
#188271=CARTESIAN_POINT('Ctrl Pts',(18.1584904122037,-56.1866608985078,
40.0818196631918));
#188272=CARTESIAN_POINT('Ctrl Pts',(18.1576227783924,-56.1875622177789,
40.0812693052022));
#188273=CARTESIAN_POINT('Ctrl Pts',(18.1567689837085,-56.1884697364865,
40.0807107531875));
#188274=CARTESIAN_POINT('Ctrl Pts',(18.1507549641993,-56.1948621810804,
40.0767763849182));
#188275=CARTESIAN_POINT('Ctrl Pts',(18.1453743792963,-56.2015542305062,
40.0724140586136));
#188276=CARTESIAN_POINT('Ctrl Pts',(18.1405824894349,-56.2084349106665,
40.0677221223766));
#188277=CARTESIAN_POINT('Ctrl Pts',(18.1382584280304,-56.2117720331087,
40.0654465383719));
#188278=CARTESIAN_POINT('Ctrl Pts',(18.1360729791409,-56.2151540877946,
40.0630928000678));
#188279=CARTESIAN_POINT('Ctrl Pts',(18.134022044255,-56.2185710935569,40.0606689262479));
#188280=CARTESIAN_POINT('Ctrl Pts',(18.1308822062392,-56.2238022906399,
40.0569581447806));
#188281=CARTESIAN_POINT('Ctrl Pts',(18.1280584389298,-56.2291119669555,
40.0530843804606));
#188282=CARTESIAN_POINT('Ctrl Pts',(18.125544237423,-56.2344544719217,40.0490800251458));
#188283=CARTESIAN_POINT('Ctrl Pts',(18.1243766292364,-56.2369355588664,
40.0472203818218));
#188284=CARTESIAN_POINT('Ctrl Pts',(18.1232756028766,-56.2394235482376,
40.0453323608818));
#188285=CARTESIAN_POINT('Ctrl Pts',(18.12224170934,-56.2419141381097,40.0434201572162));
#188286=CARTESIAN_POINT('Ctrl Pts',(18.1221624654742,-56.24210503201,40.0432735943397));
#188287=CARTESIAN_POINT('Ctrl Pts',(18.1220835820645,-56.2422959411932,
40.0431268995707));
#188288=CARTESIAN_POINT('Ctrl Pts',(18.1220050584321,-56.2424868643661,
40.0429800745037));
#188289=CARTESIAN_POINT('Ctrl Pts',(18.1209020381385,-56.2451687593303,
40.0409176249753));
#188290=CARTESIAN_POINT('Ctrl Pts',(18.1198718859664,-56.247854333334,40.0388310783332));
#188291=CARTESIAN_POINT('Ctrl Pts',(18.1189123616725,-56.2505383386774,
40.036725739981));
#188292=CARTESIAN_POINT('Ctrl Pts',(18.1154716782,-56.2601627045047,40.0291763710716));
#188293=CARTESIAN_POINT('Ctrl Pts',(18.1129106883011,-56.2698406425792,
40.021331089459));
#188294=CARTESIAN_POINT('Ctrl Pts',(18.1111213027307,-56.2795015152478,
40.0132837551313));
#188295=CARTESIAN_POINT('Ctrl Pts',(18.1091549477485,-56.2901178437901,
40.0044405431314));
#188296=CARTESIAN_POINT('Ctrl Pts',(18.1081200911546,-56.300714173025,39.9953528710584));
#188297=CARTESIAN_POINT('Ctrl Pts',(18.1079204190084,-56.3112209484395,
39.9861103629534));
#188298=CARTESIAN_POINT('Ctrl Pts',(18.1077048232014,-56.3225656290471,
39.9761307737524));
#188299=CARTESIAN_POINT('Ctrl Pts',(18.108462748441,-56.3338070504196,39.9659696935968));
#188300=CARTESIAN_POINT('Ctrl Pts',(18.1101289800559,-56.3448702837441,
39.9557128217451));
#188301=CARTESIAN_POINT('Ctrl Pts',(18.1117812336992,-56.3558407079052,
39.9455419945123));
#188302=CARTESIAN_POINT('Ctrl Pts',(18.1143271060921,-56.3666372711414,
39.9352756289322));
#188303=CARTESIAN_POINT('Ctrl Pts',(18.1177524687105,-56.3771794532808,
39.92499));
#188304=CARTESIAN_POINT('Origin',(0.014494101308342,0.00470941899427951,
39.92499));
#188305=CARTESIAN_POINT('Ctrl Pts',(19.4351129318419,-59.7658094374952,
40.10025));
#188306=CARTESIAN_POINT('Ctrl Pts',(19.4432803829091,-59.7631518948793,
40.10025));
#188307=CARTESIAN_POINT('Ctrl Pts',(19.4511532554515,-59.7598356997914,
40.0995859581842));
#188308=CARTESIAN_POINT('Ctrl Pts',(19.4586404431003,-59.7559811102142,
40.0983275959621));
#188309=CARTESIAN_POINT('Ctrl Pts',(19.4634243995784,-59.7535182109732,
40.0975235624068));
#188310=CARTESIAN_POINT('Ctrl Pts',(19.4680513433538,-59.7508363273795,
40.096477705949));
#188311=CARTESIAN_POINT('Ctrl Pts',(19.4725029330461,-59.7479734971806,
40.0952149915961));
#188312=CARTESIAN_POINT('Ctrl Pts',(19.4785784597572,-59.7440663083907,
40.0934916398701));
#188313=CARTESIAN_POINT('Ctrl Pts',(19.4843230052521,-59.7398178213043,
40.091364392163));
#188314=CARTESIAN_POINT('Ctrl Pts',(19.4896904492933,-59.7353118462116,
40.0889118607713));
#188315=CARTESIAN_POINT('Ctrl Pts',(19.4923741713139,-59.7330588586653,
40.0876855950754));
#188316=CARTESIAN_POINT('Ctrl Pts',(19.4949638171735,-59.730741436408,40.0863782327527));
#188317=CARTESIAN_POINT('Ctrl Pts',(19.4974550439415,-59.7283696021898,
40.0850006373334));
#188318=CARTESIAN_POINT('Ctrl Pts',(19.4987006573255,-59.7271836850807,
40.0843118396238));
#188319=CARTESIAN_POINT('Ctrl Pts',(19.4999216825137,-59.7259841596484,
40.0836054919165));
#188320=CARTESIAN_POINT('Ctrl Pts',(19.5011176808521,-59.7247722453468,
40.0828829920418));
#188321=CARTESIAN_POINT('Ctrl Pts',(19.5014166804367,-59.7244692667714,
40.0827023670731));
#188322=CARTESIAN_POINT('Ctrl Pts',(19.5017141161967,-59.724165513779,40.0825207326933));
#188323=CARTESIAN_POINT('Ctrl Pts',(19.5020099819911,-59.723861005197,40.0823381109275));
#188324=CARTESIAN_POINT('Ctrl Pts',(19.5028975793744,-59.7229474794511,
40.0817902456303));
#188325=CARTESIAN_POINT('Ctrl Pts',(19.5037710453008,-59.7220271539529,
40.0812334935553));
#188326=CARTESIAN_POINT('Ctrl Pts',(19.5046302297524,-59.7211005320714,
40.0806684524227));
#188327=CARTESIAN_POINT('Ctrl Pts',(19.5105677273986,-59.7146969999425,
40.0767636676137));
#188328=CARTESIAN_POINT('Ctrl Pts',(19.515878451327,-59.7079999120046,40.0724404510888));
#188329=CARTESIAN_POINT('Ctrl Pts',(19.5206092977905,-59.7011184102413,
40.0677949937409));
#188330=CARTESIAN_POINT('Ctrl Pts',(19.5229605154969,-59.6976983227544,
40.0654862141905));
#188331=CARTESIAN_POINT('Ctrl Pts',(19.5251683423981,-59.6942320938701,
40.0630972003216));
#188332=CARTESIAN_POINT('Ctrl Pts',(19.5272373629643,-59.6907301905171,
40.0606363359906));
#188333=CARTESIAN_POINT('Ctrl Pts',(19.5318019313701,-59.6830044686627,
40.0552073017123));
#188334=CARTESIAN_POINT('Ctrl Pts',(19.5357011184427,-59.6751122606219,
40.0494204304519));
#188335=CARTESIAN_POINT('Ctrl Pts',(19.5389266512982,-59.6671986827532,
40.0434049749851));
#188336=CARTESIAN_POINT('Ctrl Pts',(19.5401049791265,-59.6643077529623,
40.0412074532442));
#188337=CARTESIAN_POINT('Ctrl Pts',(19.541201362078,-59.6614137631514,40.0389814735788));
#188338=CARTESIAN_POINT('Ctrl Pts',(19.5422187365067,-59.6585211429014,
40.0367321210016));
#188339=CARTESIAN_POINT('Ctrl Pts',(19.5456359895575,-59.6488051375696,
40.0291767837145));
#188340=CARTESIAN_POINT('Ctrl Pts',(19.5481755652419,-59.6390401911886,
40.0213235332585));
#188341=CARTESIAN_POINT('Ctrl Pts',(19.5499445144588,-59.6292970278081,
40.0132649215873));
#188342=CARTESIAN_POINT('Ctrl Pts',(19.551888799194,-59.6185881370994,40.0044075527552));
#188343=CARTESIAN_POINT('Ctrl Pts',(19.5529023976137,-59.6079049297443,
39.9953016253744));
#188344=CARTESIAN_POINT('Ctrl Pts',(19.5530800481818,-59.5973174182857,
39.9860353422388));
#188345=CARTESIAN_POINT('Ctrl Pts',(19.5532713854553,-59.5859142148059,
39.9760551582729));
#188346=CARTESIAN_POINT('Ctrl Pts',(19.5524931697996,-59.5746208362211,
39.9658879738195));
#188347=CARTESIAN_POINT('Ctrl Pts',(19.5508078878569,-59.5635130675483,
39.9556174643298));
#188348=CARTESIAN_POINT('Ctrl Pts',(19.5491453629103,-59.5525552912546,
39.9454856413934));
#188349=CARTESIAN_POINT('Ctrl Pts',(19.5465995868778,-59.5417768065773,
39.9352519465128));
#188350=CARTESIAN_POINT('Ctrl Pts',(19.5431821162865,-59.5312589135996,
39.92499));
#188351=CARTESIAN_POINT('Ctrl Pts',(18.4801050014189,-56.2594439784239,
39.92499));
#188352=CARTESIAN_POINT('Ctrl Pts',(18.4768344633035,-56.2493782971082,
39.9348107241721));
#188353=CARTESIAN_POINT('Ctrl Pts',(18.472781767209,-56.2396067681217,39.9446038383168));
#188354=CARTESIAN_POINT('Ctrl Pts',(18.4679768367038,-56.2301791400435,
39.9543158069382));
#188355=CARTESIAN_POINT('Ctrl Pts',(18.4633372535446,-56.2210759356547,
39.9636935671387));
#188356=CARTESIAN_POINT('Ctrl Pts',(18.4579956735925,-56.2122922812559,
39.9729968320983));
#188357=CARTESIAN_POINT('Ctrl Pts',(18.4519372213368,-56.203891776325,39.9821731151329));
#188358=CARTESIAN_POINT('Ctrl Pts',(18.4462100865654,-56.19595066829,39.9908475764345));
#188359=CARTESIAN_POINT('Ctrl Pts',(18.4398418135294,-56.188351216549,39.9994093733838));
#188360=CARTESIAN_POINT('Ctrl Pts',(18.4327901596639,-56.1811768067744,
40.0077966115833));
#188361=CARTESIAN_POINT('Ctrl Pts',(18.4262957047542,-56.1745692957318,
40.0155211172585));
#188362=CARTESIAN_POINT('Ctrl Pts',(18.4192211773439,-56.1683219623526,
40.0230979941011));
#188363=CARTESIAN_POINT('Ctrl Pts',(18.4115142492191,-56.1625328136775,
40.0304554104737));
#188364=CARTESIAN_POINT('Ctrl Pts',(18.4092161988262,-56.1608066064038,
40.0326492435173));
#188365=CARTESIAN_POINT('Ctrl Pts',(18.4068618031993,-56.159121392827,40.0348233715057));
#188366=CARTESIAN_POINT('Ctrl Pts',(18.4044493827314,-56.1574804751187,
40.0369753512355));
#188367=CARTESIAN_POINT('Ctrl Pts',(18.4020616112563,-56.1558563235461,
40.0391053430352));
#188368=CARTESIAN_POINT('Ctrl Pts',(18.3996196264082,-56.1542770260203,
40.041211089324));
#188369=CARTESIAN_POINT('Ctrl Pts',(18.3971247125286,-56.1527473834684,
40.0432881154904));
#188370=CARTESIAN_POINT('Ctrl Pts',(18.3969512210967,-56.1526410151168,
40.043432547828));
#188371=CARTESIAN_POINT('Ctrl Pts',(18.3967774746434,-56.1525348749437,
40.0435768364421));
#188372=CARTESIAN_POINT('Ctrl Pts',(18.3966034726925,-56.1524289641633,
40.0437209807855));
#188373=CARTESIAN_POINT('Ctrl Pts',(18.3889745897491,-56.1477854475702,
40.050040796842));
#188374=CARTESIAN_POINT('Ctrl Pts',(18.3808409394275,-56.1436260014307,
40.0560490279344));
#188375=CARTESIAN_POINT('Ctrl Pts',(18.3722424849459,-56.1400597146375,
40.0616647108614));
#188376=CARTESIAN_POINT('Ctrl Pts',(18.3642272309678,-56.1367353155297,
40.0668995033486));
#188377=CARTESIAN_POINT('Ctrl Pts',(18.3558072700349,-56.1339262909283,
40.0717933267482));
#188378=CARTESIAN_POINT('Ctrl Pts',(18.3470212548469,-56.1317496772149,
40.0762460303073));
#188379=CARTESIAN_POINT('Ctrl Pts',(18.3438072168245,-56.1309534437592,
40.0778748868748));
#188380=CARTESIAN_POINT('Ctrl Pts',(18.3405443147881,-56.1302421351291,
40.0794443522247));
#188381=CARTESIAN_POINT('Ctrl Pts',(18.3372349828464,-56.1296225724748,
40.0809482021492));
#188382=CARTESIAN_POINT('Ctrl Pts',(18.3364391990694,-56.1294735883542,
40.0813098278168));
#188383=CARTESIAN_POINT('Ctrl Pts',(18.3356401993826,-56.1293301519981,
40.0816679525672));
#188384=CARTESIAN_POINT('Ctrl Pts',(18.3348380918585,-56.1291923454416,
40.082022419258));
#188385=CARTESIAN_POINT('Ctrl Pts',(18.3340610501946,-56.1290588453399,
40.0823658088648));
#188386=CARTESIAN_POINT('Ctrl Pts',(18.333281091922,-56.1289306286648,40.0827057654616));
#188387=CARTESIAN_POINT('Ctrl Pts',(18.3324983188931,-56.1288077688058,
40.0830421470151));
#188388=CARTESIAN_POINT('Ctrl Pts',(18.3239221357307,-56.1274616970648,
40.0867275956806));
#188389=CARTESIAN_POINT('Ctrl Pts',(18.3150023767873,-56.126758159346,40.0899823432031));
#188390=CARTESIAN_POINT('Ctrl Pts',(18.3059033598548,-56.1267895336331,
40.0926299529356));
#188391=CARTESIAN_POINT('Ctrl Pts',(18.3021297263203,-56.1268025454852,
40.0937279956084));
#188392=CARTESIAN_POINT('Ctrl Pts',(18.2983254984047,-56.1269416083199,
40.0947220371802));
#188393=CARTESIAN_POINT('Ctrl Pts',(18.2945030089056,-56.1272115877755,
40.0956014538692));
#188394=CARTESIAN_POINT('Ctrl Pts',(18.2879833547333,-56.1276720658709,
40.097101390674));
#188395=CARTESIAN_POINT('Ctrl Pts',(18.2814124323572,-56.1285150529071,
40.0982667904316));
#188396=CARTESIAN_POINT('Ctrl Pts',(18.2748585331712,-56.1297657127887,
40.0990539325582));
#188397=CARTESIAN_POINT('Ctrl Pts',(18.2715815835782,-56.1303910427295,
40.0994475036216));
#188398=CARTESIAN_POINT('Ctrl Pts',(18.2683092720866,-56.1311196862928,
40.0997467259952));
#188399=CARTESIAN_POINT('Ctrl Pts',(18.2650501911673,-56.1319548233211,
40.0999473488896));
#188400=CARTESIAN_POINT('Ctrl Pts',(18.261791110248,-56.1327899603494,40.100147971784));
#188401=CARTESIAN_POINT('Ctrl Pts',(18.2585452947514,-56.1337315613409,
40.10025));
#188402=CARTESIAN_POINT('Ctrl Pts',(18.2553202812748,-56.1347810195642,
40.10025));
#188403=CARTESIAN_POINT('Origin',(12.0988124084938,-56.9937374973463,39.92499));
#188404=CARTESIAN_POINT('Ctrl Pts',(12.8407372733096,-61.3271735965894,
39.92499));
#188405=CARTESIAN_POINT('Ctrl Pts',(12.8429432848611,-61.3375520649562,
39.9348354642019));
#188406=CARTESIAN_POINT('Ctrl Pts',(12.8459616464943,-61.3477256769086,
39.944644082846));
#188407=CARTESIAN_POINT('Ctrl Pts',(12.8497656413962,-61.3576417279031,
39.9543641760335));
#188408=CARTESIAN_POINT('Ctrl Pts',(12.853446029115,-61.3672355662866,39.9637684240717));
#188409=CARTESIAN_POINT('Ctrl Pts',(12.8578623484995,-61.3765894879239,
39.9730909636401));
#188410=CARTESIAN_POINT('Ctrl Pts',(12.8630345798921,-61.3856422574865,
39.9822808977146));
#188411=CARTESIAN_POINT('Ctrl Pts',(12.8679271923017,-61.3942056200553,
39.9909740094656));
#188412=CARTESIAN_POINT('Ctrl Pts',(12.8734966517565,-61.4025003187121,
39.9995492765008));
#188413=CARTESIAN_POINT('Ctrl Pts',(12.8797929832529,-61.4104485116943,
40.0079462328702));
#188414=CARTESIAN_POINT('Ctrl Pts',(12.8855923599233,-61.4177693722588,
40.0156804369697));
#188415=CARTESIAN_POINT('Ctrl Pts',(12.8920087864963,-61.4247966697195,
40.023263801743));
#188416=CARTESIAN_POINT('Ctrl Pts',(12.8991043342887,-61.4314390014616,
40.0306257269974));
#188417=CARTESIAN_POINT('Ctrl Pts',(12.901162482981,-61.4333656894057,40.0327611416657));
#188418=CARTESIAN_POINT('Ctrl Pts',(12.9032779088716,-61.4352597571381,
40.0348777427274));
#188419=CARTESIAN_POINT('Ctrl Pts',(12.9054524645843,-61.4371183613309,
40.0369733168701));
#188420=CARTESIAN_POINT('Ctrl Pts',(12.9078098227881,-61.4391332077732,
40.039245053974));
#188421=CARTESIAN_POINT('Ctrl Pts',(12.9102326900447,-61.4411043938523,
40.041487875195));
#188422=CARTESIAN_POINT('Ctrl Pts',(12.9127224163027,-61.4430281531012,
40.0436985701601));
#188423=CARTESIAN_POINT('Ctrl Pts',(12.9195554895544,-61.448307925455,40.0497658398386));
#188424=CARTESIAN_POINT('Ctrl Pts',(12.926909770583,-61.4531896374536,40.0555581699984));
#188425=CARTESIAN_POINT('Ctrl Pts',(12.9347398820029,-61.4575800373534,
40.0609828468886));
#188426=CARTESIAN_POINT('Ctrl Pts',(12.9419040088455,-61.4615970149013,
40.0659461317305));
#188427=CARTESIAN_POINT('Ctrl Pts',(12.9494643722285,-61.4651913207947,
40.0706039980707));
#188428=CARTESIAN_POINT('Ctrl Pts',(12.9574154517107,-61.4682744840803,
40.0748843180604));
#188429=CARTESIAN_POINT('Ctrl Pts',(12.961320995979,-61.4697889238146,40.076986797257));
#188430=CARTESIAN_POINT('Ctrl Pts',(12.9653208118553,-61.47117952841,40.0789976708175));
#188431=CARTESIAN_POINT('Ctrl Pts',(12.9694138336349,-61.4724324898304,
40.08090504915));
#188432=CARTESIAN_POINT('Ctrl Pts',(12.970190444651,-61.4726702270559,40.0812669556105));
#188433=CARTESIAN_POINT('Ctrl Pts',(12.9709708853391,-61.4729027677274,
40.0816253922033));
#188434=CARTESIAN_POINT('Ctrl Pts',(12.9717550556846,-61.4731300138562,
40.0819801989139));
#188435=CARTESIAN_POINT('Ctrl Pts',(12.9725147207069,-61.4733501585435,
40.0823239179149));
#188436=CARTESIAN_POINT('Ctrl Pts',(12.9732778859006,-61.4735653344326,
40.0826642303498));
#188437=CARTESIAN_POINT('Ctrl Pts',(12.9740444565835,-61.4737754532574,
40.0830009916099));
#188438=CARTESIAN_POINT('Ctrl Pts',(12.9823983859298,-61.4760652849147,
40.0866709464313));
#188439=CARTESIAN_POINT('Ctrl Pts',(12.9911623597382,-61.4777556486132,
40.0899175831878));
#188440=CARTESIAN_POINT('Ctrl Pts',(13.0001833616604,-61.478733140317,40.0925642067063));
#188441=CARTESIAN_POINT('Ctrl Pts',(13.0039929867896,-61.4791459411335,
40.0936818922528));
#188442=CARTESIAN_POINT('Ctrl Pts',(13.0078481668567,-61.4794319383911,
40.0946930094791));
#188443=CARTESIAN_POINT('Ctrl Pts',(13.011736540843,-61.4795843394718,40.0955863397546));
#188444=CARTESIAN_POINT('Ctrl Pts',(13.0182844654763,-61.4798409790834,
40.0970906856166));
#188445=CARTESIAN_POINT('Ctrl Pts',(13.0249248230174,-61.4797168922658,
40.0982599215483));
#188446=CARTESIAN_POINT('Ctrl Pts',(13.0315916763176,-61.4791780149467,
40.0990497370454));
#188447=CARTESIAN_POINT('Ctrl Pts',(13.0332583896426,-61.4790432956169,
40.0992471909196));
#188448=CARTESIAN_POINT('Ctrl Pts',(13.0349267248715,-61.4788824204061,
40.0994209989363));
#188449=CARTESIAN_POINT('Ctrl Pts',(13.0365955947403,-61.4786945538949,
40.0995705982975));
#188450=CARTESIAN_POINT('Ctrl Pts',(13.0390988995433,-61.4784127541282,
40.0997949973393));
#188451=CARTESIAN_POINT('Ctrl Pts',(13.04160338921,-61.4780702140292,40.0999649129781));
#188452=CARTESIAN_POINT('Ctrl Pts',(13.0441057251028,-61.4776657592307,
40.1000786629733));
#188453=CARTESIAN_POINT('Ctrl Pts',(13.0466080609957,-61.4772613044321,
40.1001924129685));
#188454=CARTESIAN_POINT('Ctrl Pts',(13.0491082380627,-61.4767949453822,
40.10025));
#188455=CARTESIAN_POINT('Ctrl Pts',(13.0516031943527,-61.4762657165316,
40.10025));
#188456=CARTESIAN_POINT('Ctrl Pts',(12.2578193919766,-57.7418065394566,
40.10025));
#188457=CARTESIAN_POINT('Ctrl Pts',(12.2493771807071,-57.7435970583545,
40.10025));
#188458=CARTESIAN_POINT('Ctrl Pts',(12.2411559442239,-57.7460689269803,
40.099578633424));
#188459=CARTESIAN_POINT('Ctrl Pts',(12.2332613533216,-57.7491141258107,
40.0983063763365));
#188460=CARTESIAN_POINT('Ctrl Pts',(12.228162257631,-57.7510810117995,40.0974846287991));
#188461=CARTESIAN_POINT('Ctrl Pts',(12.223199086688,-57.7532862127606,40.0964130309337));
#188462=CARTESIAN_POINT('Ctrl Pts',(12.2183955094117,-57.7556931859579,
40.0951176960924));
#188463=CARTESIAN_POINT('Ctrl Pts',(12.2120286428976,-57.7588834910511,
40.0934008039614));
#188464=CARTESIAN_POINT('Ctrl Pts',(12.2059457447516,-57.7624328173675,
40.0912909372156));
#188465=CARTESIAN_POINT('Ctrl Pts',(12.2001996238499,-57.7662682043709,
40.0888630467851));
#188466=CARTESIAN_POINT('Ctrl Pts',(12.1973265633991,-57.7681858978726,
40.0876491015699));
#188467=CARTESIAN_POINT('Ctrl Pts',(12.1945375019637,-57.770175146271,40.0863558569271));
#188468=CARTESIAN_POINT('Ctrl Pts',(12.1918376559072,-57.7722271161468,
40.0849936342771));
#188469=CARTESIAN_POINT('Ctrl Pts',(12.190487732879,-57.7732531010847,40.0843125229521));
#188470=CARTESIAN_POINT('Ctrl Pts',(12.1891600976133,-57.7742947697603,
40.0836141747074));
#188471=CARTESIAN_POINT('Ctrl Pts',(12.1878553011596,-57.7753510390204,
40.082899916161));
#188472=CARTESIAN_POINT('Ctrl Pts',(12.1875291020462,-57.7756151063355,
40.0827213515243));
#188473=CARTESIAN_POINT('Ctrl Pts',(12.1872043300163,-57.7758800862577,
40.0825417925842));
#188474=CARTESIAN_POINT('Ctrl Pts',(12.1868809929896,-57.7761459620049,
40.0823612602361));
#188475=CARTESIAN_POINT('Ctrl Pts',(12.1859109819096,-57.7769435892465,
40.0818196631917));
#188476=CARTESIAN_POINT('Ctrl Pts',(12.1849538875689,-57.7777492785674,
40.0812693052022));
#188477=CARTESIAN_POINT('Ctrl Pts',(12.1840099085256,-57.7785625799462,
40.0807107531875));
#188478=CARTESIAN_POINT('Ctrl Pts',(12.1773606420347,-57.7842913698425,
40.0767763849181));
#188479=CARTESIAN_POINT('Ctrl Pts',(12.1713100228962,-57.7903843352499,
40.0724140586136));
#188480=CARTESIAN_POINT('Ctrl Pts',(12.1658251565855,-57.7967264334409,
40.0677221223767));
#188481=CARTESIAN_POINT('Ctrl Pts',(12.1631650023518,-57.7998023442101,
40.065446538372));
#188482=CARTESIAN_POINT('Ctrl Pts',(12.1606380046011,-57.8029374300326,
40.0630928000679));
#188483=CARTESIAN_POINT('Ctrl Pts',(12.1582411305897,-57.8061213360079,
40.0606689262479));
#188484=CARTESIAN_POINT('Ctrl Pts',(12.1545716839429,-57.8109956736032,
40.0569581447806));
#188485=CARTESIAN_POINT('Ctrl Pts',(12.1512083732206,-57.815981098899,40.0530843804605));
#188486=CARTESIAN_POINT('Ctrl Pts',(12.1481495009385,-57.8210315314441,
40.0490800251457));
#188487=CARTESIAN_POINT('Ctrl Pts',(12.1467289448262,-57.8233769784455,
40.0472203818218));
#188488=CARTESIAN_POINT('Ctrl Pts',(12.1453738842984,-57.8257362497572,
40.0453323608818));
#188489=CARTESIAN_POINT('Ctrl Pts',(12.1440853170069,-57.8281051246148,
40.0434201572162));
#188490=CARTESIAN_POINT('Ctrl Pts',(12.1439865534012,-57.8282866895388,
40.0432735943397));
#188491=CARTESIAN_POINT('Ctrl Pts',(12.1438881466795,-57.8284683073399,
40.0431268995708));
#188492=CARTESIAN_POINT('Ctrl Pts',(12.143790096302,-57.8286499766611,40.0429800745037));
#188493=CARTESIAN_POINT('Ctrl Pts',(12.1424127841096,-57.8312018829079,
40.0409176249753));
#188494=CARTESIAN_POINT('Ctrl Pts',(12.1411075562953,-57.8337650648327,
40.0388310783332));
#188495=CARTESIAN_POINT('Ctrl Pts',(12.1398727334219,-57.836334069314,40.036725739981));
#188496=CARTESIAN_POINT('Ctrl Pts',(12.1354448782036,-57.8455460625025,
40.0291763710714));
#188497=CARTESIAN_POINT('Ctrl Pts',(12.1318862976808,-57.8549032874812,
40.0213310894588));
#188498=CARTESIAN_POINT('Ctrl Pts',(12.1290968783779,-57.8643241951548,
40.0132837551309));
#188499=CARTESIAN_POINT('Ctrl Pts',(12.126031586786,-57.874676826274,40.004440543131));
#188500=CARTESIAN_POINT('Ctrl Pts',(12.1238947812336,-57.8851069357391,
39.9953528710581));
#188501=CARTESIAN_POINT('Ctrl Pts',(12.1225979458244,-57.895535282516,39.986110362953));
#188502=CARTESIAN_POINT('Ctrl Pts',(12.1211976890437,-57.9067952798775,
39.9761307737522));
#188503=CARTESIAN_POINT('Ctrl Pts',(12.1207764137885,-57.9180543443278,
39.9659696935969));
#188504=CARTESIAN_POINT('Ctrl Pts',(12.1212770948341,-57.9292311407324,
39.9557128217455));
#188505=CARTESIAN_POINT('Ctrl Pts',(12.12177357568,-57.9403141752966,39.9455419945126));
#188506=CARTESIAN_POINT('Ctrl Pts',(12.1231769533539,-57.9513177099587,
39.9352756289323));
#188507=CARTESIAN_POINT('Ctrl Pts',(12.125481593379,-57.9621601888121,39.92499));
#188508=CARTESIAN_POINT('Origin',(0.0149069694351876,0.0031685741680681,
39.92499));
#188509=CARTESIAN_POINT('Ctrl Pts',(13.0814171332231,-61.4699285681955,
40.10025));
#188510=CARTESIAN_POINT('Ctrl Pts',(13.0898176309848,-61.4681393149849,
40.10025));
#188511=CARTESIAN_POINT('Ctrl Pts',(13.0979940118843,-61.465664225629,40.0995859581841));
#188512=CARTESIAN_POINT('Ctrl Pts',(13.1058430982611,-61.4626133761158,
40.0983275959619));
#188513=CARTESIAN_POINT('Ctrl Pts',(13.1108582907976,-61.4606640285135,
40.0975235624067));
#188514=CARTESIAN_POINT('Ctrl Pts',(13.1157402208612,-61.4584804838814,
40.0964777059489));
#188515=CARTESIAN_POINT('Ctrl Pts',(13.1204666715205,-61.4560986543956,
40.0952149915961));
#188516=CARTESIAN_POINT('Ctrl Pts',(13.1269173283004,-61.4528479350654,
40.0934916398701));
#188517=CARTESIAN_POINT('Ctrl Pts',(13.1330744924004,-61.4492231901485,
40.0913643921631));
#188518=CARTESIAN_POINT('Ctrl Pts',(13.1388835356735,-61.4453029499362,
40.0889118607713));
#188519=CARTESIAN_POINT('Ctrl Pts',(13.1417880573101,-61.44334282983,40.0876855950754));
#188520=CARTESIAN_POINT('Ctrl Pts',(13.144605753406,-61.4413087943564,40.0863782327527));
#188521=CARTESIAN_POINT('Ctrl Pts',(13.147331257159,-61.4392103573999,40.0850006373334));
#188522=CARTESIAN_POINT('Ctrl Pts',(13.1486940090356,-61.4381611389217,
40.0843118396237));
#188523=CARTESIAN_POINT('Ctrl Pts',(13.1500337298701,-61.4370958165017,
40.0836054919165));
#188524=CARTESIAN_POINT('Ctrl Pts',(13.1513498559441,-61.4360155570619,
40.0828829920418));
#188525=CARTESIAN_POINT('Ctrl Pts',(13.1516788874626,-61.4357454922019,
40.0827023670731));
#188526=CARTESIAN_POINT('Ctrl Pts',(13.1520064446718,-61.4354744937031,
40.0825207326933));
#188527=CARTESIAN_POINT('Ctrl Pts',(13.1523325194966,-61.4352025796478,
40.0823381109275));
#188528=CARTESIAN_POINT('Ctrl Pts',(13.1533107439709,-61.434386837482,40.0817902456303));
#188529=CARTESIAN_POINT('Ctrl Pts',(13.1542756251696,-61.4335628556742,
40.0812334935553));
#188530=CARTESIAN_POINT('Ctrl Pts',(13.1552269612802,-61.4327311191547,
40.0806684524227));
#188531=CARTESIAN_POINT('Ctrl Pts',(13.161801284066,-61.4269833037494,40.0767636676136));
#188532=CARTESIAN_POINT('Ctrl Pts',(13.1677829516036,-61.420878024971,40.0724404510887));
#188533=CARTESIAN_POINT('Ctrl Pts',(13.1732071947995,-61.4145287289051,
40.0677949937408));
#188534=CARTESIAN_POINT('Ctrl Pts',(13.1759030287785,-61.411373146189,40.0654862141905));
#188535=CARTESIAN_POINT('Ctrl Pts',(13.1784610805514,-61.4081566864224,
40.0630972003215));
#188536=CARTESIAN_POINT('Ctrl Pts',(13.1808848153825,-61.4048902384027,
40.0606363359906));
#188537=CARTESIAN_POINT('Ctrl Pts',(13.1862319364381,-61.3976839661818,
40.0552073017124));
#188538=CARTESIAN_POINT('Ctrl Pts',(13.1909347237342,-61.3902425685152,
40.0494204304519));
#188539=CARTESIAN_POINT('Ctrl Pts',(13.1949697809168,-61.3827095020466,
40.0434049749851));
#188540=CARTESIAN_POINT('Ctrl Pts',(13.1964438381903,-61.3799575778687,
40.0412074532442));
#188541=CARTESIAN_POINT('Ctrl Pts',(13.197836719349,-61.3771940448619,40.0389814735788));
#188542=CARTESIAN_POINT('Ctrl Pts',(13.1991508816437,-61.3744236152738,
40.0367321210017));
#188543=CARTESIAN_POINT('Ctrl Pts',(13.2035650137315,-61.3651180354449,
40.0291767837139));
#188544=CARTESIAN_POINT('Ctrl Pts',(13.207111392194,-61.3556720404047,40.0213235332572));
#188545=CARTESIAN_POINT('Ctrl Pts',(13.2098890888176,-61.346167156635,40.0132649215853));
#188546=CARTESIAN_POINT('Ctrl Pts',(13.2129421064467,-61.3357201634447,
40.0044075527525));
#188547=CARTESIAN_POINT('Ctrl Pts',(13.2150668515158,-61.3252014297016,
39.9953016253709));
#188548=CARTESIAN_POINT('Ctrl Pts',(13.2163502251979,-61.3146904872786,
39.9860353422345));
#188549=CARTESIAN_POINT('Ctrl Pts',(13.2177324736417,-61.3033697519309,
39.9760551582678));
#188550=CARTESIAN_POINT('Ctrl Pts',(13.2181390006411,-61.2920568939682,
39.9658879738135));
#188551=CARTESIAN_POINT('Ctrl Pts',(13.2176240288384,-61.280833814882,39.9556174643229));
#188552=CARTESIAN_POINT('Ctrl Pts',(13.217116010894,-61.2697622852581,39.9454856413888));
#188553=CARTESIAN_POINT('Ctrl Pts',(13.2157108393287,-61.2587767401938,
39.9352519465106));
#188554=CARTESIAN_POINT('Ctrl Pts',(13.2134115091892,-61.2479592423878,
39.92499));
#188555=CARTESIAN_POINT('Ctrl Pts',(12.4981558292586,-57.8829458346106,
39.92499));
#188556=CARTESIAN_POINT('Ctrl Pts',(12.4959553576927,-57.8725934298269,
39.9348107241722));
#188557=CARTESIAN_POINT('Ctrl Pts',(12.4929462656002,-57.8624518082037,
39.944603838317));
#188558=CARTESIAN_POINT('Ctrl Pts',(12.4891531124823,-57.8525735736565,
39.9543158069385));
#188559=CARTESIAN_POINT('Ctrl Pts',(12.4854904894106,-57.8430352690759,
39.9636935671392));
#188560=CARTESIAN_POINT('Ctrl Pts',(12.4810963130884,-57.8337413853111,
39.9729968320989));
#188561=CARTESIAN_POINT('Ctrl Pts',(12.4759491415391,-57.8247536185209,
39.9821731151335));
#188562=CARTESIAN_POINT('Ctrl Pts',(12.4710834524306,-57.8162573641099,
39.9908475764353));
#188563=CARTESIAN_POINT('Ctrl Pts',(12.4655444244727,-57.8080338771665,
39.9994093733848));
#188564=CARTESIAN_POINT('Ctrl Pts',(12.4592813303333,-57.8001616710171,
40.0077966115844));
#188565=CARTESIAN_POINT('Ctrl Pts',(12.4535131257022,-57.7929115012196,
40.0155211172599));
#188566=CARTESIAN_POINT('Ctrl Pts',(12.4471303774507,-57.7859589019078,
40.0230979941026));
#188567=CARTESIAN_POINT('Ctrl Pts',(12.4400707994989,-57.7793958734413,
40.0304554104753));
#188568=CARTESIAN_POINT('Ctrl Pts',(12.4379657758606,-57.7774389108361,
40.0326492435184));
#188569=CARTESIAN_POINT('Ctrl Pts',(12.4358004306453,-57.7755168276793,
40.0348233715062));
#188570=CARTESIAN_POINT('Ctrl Pts',(12.433572748276,-57.7736327324861,40.0369753512356));
#188571=CARTESIAN_POINT('Ctrl Pts',(12.4313678273309,-57.7717678881028,
40.0391053430352));
#188572=CARTESIAN_POINT('Ctrl Pts',(12.4291043014747,-57.7699419852106,
40.041211089324));
#188573=CARTESIAN_POINT('Ctrl Pts',(12.4267829461797,-57.7681599326868,
40.0432881154904));
#188574=CARTESIAN_POINT('Ctrl Pts',(12.4266215236723,-57.7680360122395,
40.043432547828));
#188575=CARTESIAN_POINT('Ctrl Pts',(12.4264598236895,-57.7679122920635,
40.0435768364421));
#188576=CARTESIAN_POINT('Ctrl Pts',(12.4262978456307,-57.7677887733169,
40.0437209807855));
#188577=CARTESIAN_POINT('Ctrl Pts',(12.4191961341598,-57.762373258983,40.0500407968421));
#188578=CARTESIAN_POINT('Ctrl Pts',(12.4115418213385,-57.7573864007557,
40.0560490279346));
#188579=CARTESIAN_POINT('Ctrl Pts',(12.4033632485683,-57.7529408672212,
40.0616647108617));
#188580=CARTESIAN_POINT('Ctrl Pts',(12.39573939732,-57.7487968573386,40.0668995033489));
#188581=CARTESIAN_POINT('Ctrl Pts',(12.3876591848388,-57.7451230952906,
40.0717933267486));
#188582=CARTESIAN_POINT('Ctrl Pts',(12.3791488184477,-57.742040016629,40.0762460303077));
#188583=CARTESIAN_POINT('Ctrl Pts',(12.3760356163216,-57.7409121865683,
40.0778748868751));
#188584=CARTESIAN_POINT('Ctrl Pts',(12.3728649408022,-57.7398637084257,
40.0794443522249));
#188585=CARTESIAN_POINT('Ctrl Pts',(12.3696384996596,-57.7389016204182,
40.0809482021492));
#188586=CARTESIAN_POINT('Ctrl Pts',(12.3688626483506,-57.7386702703929,
40.0813098278168));
#188587=CARTESIAN_POINT('Ctrl Pts',(12.3680830188495,-57.7384441015868,
40.0816679525672));
#188588=CARTESIAN_POINT('Ctrl Pts',(12.367299710062,-57.7382232068821,40.082022419258));
#188589=CARTESIAN_POINT('Ctrl Pts',(12.3665408796741,-57.738009215137,40.0823658088648));
#188590=CARTESIAN_POINT('Ctrl Pts',(12.3657785963866,-57.7378001730065,
40.0827057654617));
#188591=CARTESIAN_POINT('Ctrl Pts',(12.3650129538224,-57.7375961641249,
40.0830421470151));
#188592=CARTESIAN_POINT('Ctrl Pts',(12.3566244546994,-57.7353610110591,
40.0867275956806));
#188593=CARTESIAN_POINT('Ctrl Pts',(12.3478270988457,-57.7337289586985,
40.0899823432029));
#188594=CARTESIAN_POINT('Ctrl Pts',(12.3387746477742,-57.7328090548568,
40.0926299529354));
#188595=CARTESIAN_POINT('Ctrl Pts',(12.3350203264899,-57.7324275433142,
40.0937279956083));
#188596=CARTESIAN_POINT('Ctrl Pts',(12.3312224025082,-57.7321681942502,
40.0947220371802));
#188597=CARTESIAN_POINT('Ctrl Pts',(12.3273926324687,-57.7320371357769,
40.0956014538693));
#188598=CARTESIAN_POINT('Ctrl Pts',(12.3208605605765,-57.7318136018935,
40.097101390674));
#188599=CARTESIAN_POINT('Ctrl Pts',(12.3142375182613,-57.7319651225402,
40.0982667904316));
#188600=CARTESIAN_POINT('Ctrl Pts',(12.3075887924653,-57.7325238621659,
40.0990539325582));
#188601=CARTESIAN_POINT('Ctrl Pts',(12.3042644295673,-57.7328032319787,
40.0994475036216));
#188602=CARTESIAN_POINT('Ctrl Pts',(12.3009338801485,-57.7331858342648,
40.0997467259952));
#188603=CARTESIAN_POINT('Ctrl Pts',(12.2976053572253,-57.7336757296049,
40.0999473488896));
#188604=CARTESIAN_POINT('Ctrl Pts',(12.294276834302,-57.734165624945,40.100147971784));
#188605=CARTESIAN_POINT('Ctrl Pts',(12.2909503756177,-57.7347627876418,
40.10025));
#188606=CARTESIAN_POINT('Ctrl Pts',(12.2876333308469,-57.7354693911205,
40.10025));
#188607=CARTESIAN_POINT('Origin',(6.07506605172281,-57.9461901084062,39.92499));
#188608=CARTESIAN_POINT('Ctrl Pts',(6.35995915837782,-62.3334394572619,
39.92499));
#188609=CARTESIAN_POINT('Ctrl Pts',(6.36106823981771,-62.3439916622904,
39.934835464202));
#188610=CARTESIAN_POINT('Ctrl Pts',(6.3630066345268,-62.3544250468352,39.9446440828461));
#188611=CARTESIAN_POINT('Ctrl Pts',(6.36575328117442,-62.3646844024062,
39.9543641760336));
#188612=CARTESIAN_POINT('Ctrl Pts',(6.36841067816121,-62.3746103900116,
39.9637684240718));
#188613=CARTESIAN_POINT('Ctrl Pts',(6.37182505343178,-62.384374700966,39.9730909636402));
#188614=CARTESIAN_POINT('Ctrl Pts',(6.37602267870886,-62.3939185239089,
39.9822808977147));
#188615=CARTESIAN_POINT('Ctrl Pts',(6.3799933737461,-62.4029463927381,39.9909740094656));
#188616=CARTESIAN_POINT('Ctrl Pts',(6.38466529101533,-62.4117778192058,
39.9995492765008));
#188617=CARTESIAN_POINT('Ctrl Pts',(6.39009631815078,-62.4203406170107,
40.0079462328701));
#188618=CARTESIAN_POINT('Ctrl Pts',(6.39509868692439,-62.4282275730663,
40.0156804369695));
#188619=CARTESIAN_POINT('Ctrl Pts',(6.4007454110367,-62.4358870734656,40.0232638017428));
#188620=CARTESIAN_POINT('Ctrl Pts',(6.40710777594629,-62.4432347045261,
40.0306257269972));
#188621=CARTESIAN_POINT('Ctrl Pts',(6.40895325615476,-62.4453659729922,
40.0327611416655));
#188622=CARTESIAN_POINT('Ctrl Pts',(6.41085910953167,-62.447470787041,40.0348777427273));
#188623=CARTESIAN_POINT('Ctrl Pts',(6.41282747576063,-62.4495465125725,
40.0369733168701));
#188624=CARTESIAN_POINT('Ctrl Pts',(6.41496131130727,-62.4517967325056,
40.039245053974));
#188625=CARTESIAN_POINT('Ctrl Pts',(6.41716486079182,-62.4540103788122,
40.041487875195));
#188626=CARTESIAN_POINT('Ctrl Pts',(6.41943986047092,-62.4561838467662,
40.04369857016));
#188627=CARTESIAN_POINT('Ctrl Pts',(6.4256836149418,-62.4621489466211,40.0497658398386));
#188628=CARTESIAN_POINT('Ctrl Pts',(6.43248733059615,-62.4677726477849,
40.0555581699984));
#188629=CARTESIAN_POINT('Ctrl Pts',(6.43981562609174,-62.4729574661286,
40.0609828468885));
#188630=CARTESIAN_POINT('Ctrl Pts',(6.4465206186082,-62.477701293423,40.0659461317308));
#188631=CARTESIAN_POINT('Ctrl Pts',(6.45366385825844,-62.482066182499,40.0706039980712));
#188632=CARTESIAN_POINT('Ctrl Pts',(6.46124910257559,-62.4859635700134,
40.0748843180612));
#188633=CARTESIAN_POINT('Ctrl Pts',(6.46497494980514,-62.4878779540286,
40.0769867972575));
#188634=CARTESIAN_POINT('Ctrl Pts',(6.46880749650979,-62.4896790353533,
40.0789976708177));
#188635=CARTESIAN_POINT('Ctrl Pts',(6.47274712615552,-62.4913529701965,
40.08090504915));
#188636=CARTESIAN_POINT('Ctrl Pts',(6.4734946325084,-62.4916705830287,40.0812669556104));
#188637=CARTESIAN_POINT('Ctrl Pts',(6.47424649074167,-62.4919834280838,
40.0816253922032));
#188638=CARTESIAN_POINT('Ctrl Pts',(6.47500261163139,-62.4922913974557,
40.0819801989139));
#188639=CARTESIAN_POINT('Ctrl Pts',(6.47573510374331,-62.4925897427847,
40.0823239179149));
#188640=CARTESIAN_POINT('Ctrl Pts',(6.47647159623326,-62.4928835124027,
40.0826642303498));
#188641=CARTESIAN_POINT('Ctrl Pts',(6.47721200416385,-62.4931726086301,
40.0830009916099));
#188642=CARTESIAN_POINT('Ctrl Pts',(6.4852808172263,-62.4963231197465,40.086670946431));
#188643=CARTESIAN_POINT('Ctrl Pts',(6.49382008994887,-62.49892030817,40.0899175831874));
#188644=CARTESIAN_POINT('Ctrl Pts',(6.5026894981724,-62.5008353965401,40.0925642067058));
#188645=CARTESIAN_POINT('Ctrl Pts',(6.50643510434215,-62.5016441502511,
40.0936818922525));
#188646=CARTESIAN_POINT('Ctrl Pts',(6.51023927047611,-62.5023315568339,
40.0946930094789));
#188647=CARTESIAN_POINT('Ctrl Pts',(6.5140904132927,-62.502889568803,40.0955863397546));
#188648=CARTESIAN_POINT('Ctrl Pts',(6.52057564156552,-62.5038292470155,
40.0970906856166));
#188649=CARTESIAN_POINT('Ctrl Pts',(6.52719259313763,-62.5043999463277,
40.0982599215483));
#188650=CARTESIAN_POINT('Ctrl Pts',(6.53387925273587,-62.5045608969643,
40.0990497370454));
#188651=CARTESIAN_POINT('Ctrl Pts',(6.53555091763542,-62.5046011346235,
40.0992471909196));
#188652=CARTESIAN_POINT('Ctrl Pts',(6.53722692958795,-62.5046155292216,
40.0994209989363));
#188653=CARTESIAN_POINT('Ctrl Pts',(6.53890629461062,-62.5046031362657,
40.0995705982975));
#188654=CARTESIAN_POINT('Ctrl Pts',(6.54142534214462,-62.5045845468319,
40.0997949973393));
#188655=CARTESIAN_POINT('Ctrl Pts',(6.54395191714495,-62.5045056736597,
40.0999649129781));
#188656=CARTESIAN_POINT('Ctrl Pts',(6.54648282201853,-62.5043649998325,
40.1000786629733));
#188657=CARTESIAN_POINT('Ctrl Pts',(6.54901372689211,-62.5042243260053,
40.1001924129685));
#188658=CARTESIAN_POINT('Ctrl Pts',(6.5515489555224,-62.5040218613861,40.10025));
#188659=CARTESIAN_POINT('Ctrl Pts',(6.55408556365926,-62.5037563256535,
40.10025));
#188660=CARTESIAN_POINT('Ctrl Pts',(6.15500747092297,-58.7067819056643,
40.10025));
#188661=CARTESIAN_POINT('Ctrl Pts',(6.14642434678156,-58.7076801645418,
40.10025));
#188662=CARTESIAN_POINT('Ctrl Pts',(6.13798976646346,-58.7092791387968,
40.0995786334241));
#188663=CARTESIAN_POINT('Ctrl Pts',(6.1298201130023,-58.7114824462541,40.0983063763366));
#188664=CARTESIAN_POINT('Ctrl Pts',(6.12454335512134,-58.7129055567991,
40.0974846287992));
#188665=CARTESIAN_POINT('Ctrl Pts',(6.11937686668017,-58.714579884807,40.0964130309338));
#188666=CARTESIAN_POINT('Ctrl Pts',(6.11434800669312,-58.7164715618025,
40.0951176960923));
#188667=CARTESIAN_POINT('Ctrl Pts',(6.10768254085112,-58.7189788712981,
40.0934008039614));
#188668=CARTESIAN_POINT('Ctrl Pts',(6.10126195983219,-58.7218729180381,
40.0912909372156));
#188669=CARTESIAN_POINT('Ctrl Pts',(6.09514640967252,-58.7250866612026,
40.0888630467851));
#188670=CARTESIAN_POINT('Ctrl Pts',(6.09208863459269,-58.7266935327848,
40.0876491015699));
#188671=CARTESIAN_POINT('Ctrl Pts',(6.08910691884952,-58.7283803475666,
40.0863558569271));
#188672=CARTESIAN_POINT('Ctrl Pts',(6.08620737357445,-58.7301388657774,
40.0849936342771));
#188673=CARTESIAN_POINT('Ctrl Pts',(6.08475760093692,-58.7310181248827,
40.0843125229521));
#188674=CARTESIAN_POINT('Ctrl Pts',(6.08332835457024,-58.7319153115143,
40.0836141747074));
#188675=CARTESIAN_POINT('Ctrl Pts',(6.08192029572551,-58.7328294060527,
40.0828999161609));
#188676=CARTESIAN_POINT('Ctrl Pts',(6.08156828101433,-58.7330579296873,
40.0827213515243));
#188677=CARTESIAN_POINT('Ctrl Pts',(6.08121759017549,-58.7332875101006,
40.0825417925841));
#188678=CARTESIAN_POINT('Ctrl Pts',(6.08086823283962,-58.7335181314301,
40.082361260236));
#188679=CARTESIAN_POINT('Ctrl Pts',(6.079820160832,-58.7342099954187,40.0818196631917));
#188680=CARTESIAN_POINT('Ctrl Pts',(6.07878409208759,-58.7349112274885,
40.0812693052021));
#188681=CARTESIAN_POINT('Ctrl Pts',(6.077760271117,-58.7356214008386,40.0807107531875));
#188682=CARTESIAN_POINT('Ctrl Pts',(6.07054860839961,-58.7406237702161,
40.0767763849182));
#188683=CARTESIAN_POINT('Ctrl Pts',(6.0638942468752,-58.746050895801,40.0724140586138));
#188684=CARTESIAN_POINT('Ctrl Pts',(6.05777649745833,-58.7517849266677,
40.067722122377));
#188685=CARTESIAN_POINT('Ctrl Pts',(6.05480939560192,-58.7545659254419,
40.0654465383722));
#188686=CARTESIAN_POINT('Ctrl Pts',(6.05196853530582,-58.7574196937447,
40.063092800068));
#188687=CARTESIAN_POINT('Ctrl Pts',(6.04925198282213,-58.7603356163931,
40.0606689262479));
#188688=CARTESIAN_POINT('Ctrl Pts',(6.04509313076973,-58.7647996902381,
40.0569581447805));
#188689=CARTESIAN_POINT('Ctrl Pts',(6.04122712577058,-58.7694062431511,
40.0530843804605));
#188690=CARTESIAN_POINT('Ctrl Pts',(6.03765709635815,-58.7741092696793,
40.0490800251457));
#188691=CARTESIAN_POINT('Ctrl Pts',(6.03599915623013,-58.7762933795292,
40.0472203818218));
#188692=CARTESIAN_POINT('Ctrl Pts',(6.03440490786102,-58.7784980841112,
40.0453323608818));
#188693=CARTESIAN_POINT('Ctrl Pts',(6.03287578462736,-58.7807192900657,
40.0434201572162));
#188694=CARTESIAN_POINT('Ctrl Pts',(6.03275858335655,-58.7808895367501,
40.0432735943397));
#188695=CARTESIAN_POINT('Ctrl Pts',(6.03264173148759,-58.7810598733265,
40.0431268995707));
#188696=CARTESIAN_POINT('Ctrl Pts',(6.03252522862529,-58.7812302983888,
40.0429800745037));
#188697=CARTESIAN_POINT('Ctrl Pts',(6.03088871465485,-58.7836242566993,
40.0409176249753));
#188698=CARTESIAN_POINT('Ctrl Pts',(6.02932271154744,-58.7860369637877,
40.0388310783332));
#188699=CARTESIAN_POINT('Ctrl Pts',(6.02782611907238,-58.7884628208563,
40.036725739981));
#188700=CARTESIAN_POINT('Ctrl Pts',(6.02245960461748,-58.7971615128793,
40.0291763710726));
#188701=CARTESIAN_POINT('Ctrl Pts',(6.01794242202427,-58.8060955050456,
40.0213310894612));
#188702=CARTESIAN_POINT('Ctrl Pts',(6.01418353045086,-58.8151732302866,
40.0132837551347));
#188703=CARTESIAN_POINT('Ctrl Pts',(6.01005288622599,-58.8251487383876,
40.0044405431366));
#188704=CARTESIAN_POINT('Ctrl Pts',(6.00683754300419,-58.8352983536189,
39.9953528710656));
#188705=CARTESIAN_POINT('Ctrl Pts',(6.00445775273193,-58.8455340166064,
39.9861103629626));
#188706=CARTESIAN_POINT('Ctrl Pts',(6.00188817648396,-58.8565859638311,
39.9761307737652));
#188707=CARTESIAN_POINT('Ctrl Pts',(6.00029231631344,-58.8677393146896,
39.9659696936133));
#188708=CARTESIAN_POINT('Ctrl Pts',(5.99962196122237,-58.8789072188508,
39.9557128217654));
#188709=CARTESIAN_POINT('Ctrl Pts',(5.99895722972124,-58.889981435779,39.945541994526));
#188710=CARTESIAN_POINT('Ctrl Pts',(5.99920273697621,-58.9010713848459,
39.935275628939));
#188711=CARTESIAN_POINT('Ctrl Pts',(6.00036140429027,-58.912095367953,39.92499));
#188712=CARTESIAN_POINT('Origin',(0.0151565136854175,0.00159301378020458,
39.92499));
#188713=CARTESIAN_POINT('Ctrl Pts',(6.58439859103009,-62.5005702980931,
40.10025));
#188714=CARTESIAN_POINT('Ctrl Pts',(6.59294009787482,-62.4996689377205,
40.10025));
#188715=CARTESIAN_POINT('Ctrl Pts',(6.60133040499131,-62.4980620716935,
40.0995859581841));
#188716=CARTESIAN_POINT('Ctrl Pts',(6.60945539386312,-62.4958483879901,
40.0983275959618));
#188717=CARTESIAN_POINT('Ctrl Pts',(6.6146468749591,-62.4944339494868,40.0975235624066));
#188718=CARTESIAN_POINT('Ctrl Pts',(6.61973030386369,-62.4927726671881,
40.0964777059489));
#188719=CARTESIAN_POINT('Ctrl Pts',(6.62467983150736,-62.4908979342377,
40.0952149915961));
#188720=CARTESIAN_POINT('Ctrl Pts',(6.63143494361066,-62.4883392999283,
40.0934916398701));
#188721=CARTESIAN_POINT('Ctrl Pts',(6.63793726713738,-62.4853780106448,
40.0913643921631));
#188722=CARTESIAN_POINT('Ctrl Pts',(6.64412426454869,-62.4820864562849,
40.0889118607713));
#188723=CARTESIAN_POINT('Ctrl Pts',(6.64721776325435,-62.480440679105,40.0876855950754));
#188724=CARTESIAN_POINT('Ctrl Pts',(6.6502326383185,-62.4787123157334,40.0863782327526));
#188725=CARTESIAN_POINT('Ctrl Pts',(6.65316255786718,-62.476910266953,40.0850006373334));
#188726=CARTESIAN_POINT('Ctrl Pts',(6.65462751764151,-62.4760092425629,
40.0843118396237));
#188727=CARTESIAN_POINT('Ctrl Pts',(6.65607125586061,-62.4750897950506,
40.0836054919164));
#188728=CARTESIAN_POINT('Ctrl Pts',(6.6574930899174,-62.474153026021,40.0828829920417));
#188729=CARTESIAN_POINT('Ctrl Pts',(6.6578485484316,-62.4739188337636,40.0827023670731));
#188730=CARTESIAN_POINT('Ctrl Pts',(6.65820263830482,-62.4736835588747,
40.0825207326932));
#188731=CARTESIAN_POINT('Ctrl Pts',(6.65855534961594,-62.4734472184934,
40.0823381109275));
#188732=CARTESIAN_POINT('Ctrl Pts',(6.65961348354927,-62.4727381973495,
40.0817902456303));
#188733=CARTESIAN_POINT('Ctrl Pts',(6.66065920857986,-62.4720195869492,
40.0812334935553));
#188734=CARTESIAN_POINT('Ctrl Pts',(6.66169227331197,-62.471291848471,40.0806684524227));
#188735=CARTESIAN_POINT('Ctrl Pts',(6.66883139158116,-62.4662627240578,
40.0767636676136));
#188736=CARTESIAN_POINT('Ctrl Pts',(6.67541846632667,-62.4608161451508,
40.0724404510887));
#188737=CARTESIAN_POINT('Ctrl Pts',(6.6814766771114,-62.4550686189988,40.0677949937407));
#188738=CARTESIAN_POINT('Ctrl Pts',(6.68448759124181,-62.452212114278,40.0654862141904));
#188739=CARTESIAN_POINT('Ctrl Pts',(6.68736784133602,-62.4492806638353,
40.0630972003215));
#188740=CARTESIAN_POINT('Ctrl Pts',(6.69011973548588,-62.4462854590369,
40.0606363359906));
#188741=CARTESIAN_POINT('Ctrl Pts',(6.69619082501401,-62.4396775898761,
40.0552073017123));
#188742=CARTESIAN_POINT('Ctrl Pts',(6.70164568781197,-62.4327685320937,
40.0494204304519));
#188743=CARTESIAN_POINT('Ctrl Pts',(6.70644606039073,-62.4256985108779,
40.0434049749851));
#188744=CARTESIAN_POINT('Ctrl Pts',(6.70819969702964,-62.42311574297,40.0412074532442));
#188745=CARTESIAN_POINT('Ctrl Pts',(6.70987381569794,-62.4205129446132,
40.0389814735788));
#188746=CARTESIAN_POINT('Ctrl Pts',(6.71147036762154,-62.4178950590935,
40.0367321210017));
#188747=CARTESIAN_POINT('Ctrl Pts',(6.71683301659107,-62.4091018586486,
40.0291767837141));
#188748=CARTESIAN_POINT('Ctrl Pts',(6.72134734296672,-62.4000783072487,
40.0213235332576));
#188749=CARTESIAN_POINT('Ctrl Pts',(6.7251033539715,-62.3909158405868,40.0132649215857));
#188750=CARTESIAN_POINT('Ctrl Pts',(6.7292316549945,-62.3808452043598,40.0044075527531));
#188751=CARTESIAN_POINT('Ctrl Pts',(6.73244426756144,-62.3706061896782,
39.9953016253718));
#188752=CARTESIAN_POINT('Ctrl Pts',(6.73481930344724,-62.3602869763768,
39.9860353422356));
#188753=CARTESIAN_POINT('Ctrl Pts',(6.7373773188584,-62.3491727415083,39.9760551582693));
#188754=CARTESIAN_POINT('Ctrl Pts',(6.73896413451842,-62.3379643502084,
39.9658879738155));
#188755=CARTESIAN_POINT('Ctrl Pts',(6.7396251149954,-62.326748923113,39.9556174643255));
#188756=CARTESIAN_POINT('Ctrl Pts',(6.74027717000425,-62.3156849421506,
39.9454856413905));
#188757=CARTESIAN_POINT('Ctrl Pts',(6.74002799825967,-62.3046126966258,
39.9352519465113));
#188758=CARTESIAN_POINT('Ctrl Pts',(6.73887200051313,-62.2936141127569,
39.92499));
#188759=CARTESIAN_POINT('Ctrl Pts',(6.37927424642559,-58.8722700234481,
39.92499));
#188760=CARTESIAN_POINT('Ctrl Pts',(6.37816795023629,-58.8617443183088,
39.9348107241731));
#188761=CARTESIAN_POINT('Ctrl Pts',(6.37623543038822,-58.8513437177768,
39.9446038383187));
#188762=CARTESIAN_POINT('Ctrl Pts',(6.37349561323655,-58.8411231047648,
39.9543158069411));
#188763=CARTESIAN_POINT('Ctrl Pts',(6.37085007871699,-58.8312542036531,
39.9636935671423));
#188764=CARTESIAN_POINT('Ctrl Pts',(6.36745144953993,-58.8215519162572,
39.9729968321024));
#188765=CARTESIAN_POINT('Ctrl Pts',(6.36327195218524,-58.8120753594613,
39.9821731151375));
#188766=CARTESIAN_POINT('Ctrl Pts',(6.35932101824761,-58.8031170454156,
39.9908475764394));
#188767=CARTESIAN_POINT('Ctrl Pts',(6.354671922117,-58.7943596215135,39.9994093733891));
#188768=CARTESIAN_POINT('Ctrl Pts',(6.34926600747357,-58.7858758685273,
40.0077966115888));
#188769=CARTESIAN_POINT('Ctrl Pts',(6.34428725077805,-58.7780624743528,
40.0155211172641));
#188770=CARTESIAN_POINT('Ctrl Pts',(6.33866621241084,-58.7704807832414,
40.0230979941068));
#188771=CARTESIAN_POINT('Ctrl Pts',(6.33233133084537,-58.7632157808971,
40.0304554104795));
#188772=CARTESIAN_POINT('Ctrl Pts',(6.33044239704174,-58.7610495038531,
40.0326492435212));
#188773=CARTESIAN_POINT('Ctrl Pts',(6.3284898262139,-58.7589116098624,40.0348233715076));
#188774=CARTESIAN_POINT('Ctrl Pts',(6.32647128889818,-58.7568049797264,
40.0369753512356));
#188775=CARTESIAN_POINT('Ctrl Pts',(6.32447337605832,-58.7547198741578,
40.0391053430352));
#188776=CARTESIAN_POINT('Ctrl Pts',(6.32241310885704,-58.7526673708734,
40.041211089324));
#188777=CARTESIAN_POINT('Ctrl Pts',(6.32029074540098,-58.7506524329181,
40.0432881154904));
#188778=CARTESIAN_POINT('Ctrl Pts',(6.32014316039693,-58.7505123180733,
40.043432547828));
#188779=CARTESIAN_POINT('Ctrl Pts',(6.31999527850335,-58.7503723733987,
40.0435768364421));
#188780=CARTESIAN_POINT('Ctrl Pts',(6.31984709900205,-58.7502325999832,
40.0437209807855));
#188781=CARTESIAN_POINT('Ctrl Pts',(6.31335036684093,-58.7441044214168,
40.050040796842));
#188782=CARTESIAN_POINT('Ctrl Pts',(6.30625925377334,-58.7383447881642,
40.0560490279344));
#188783=CARTESIAN_POINT('Ctrl Pts',(6.29859016886937,-58.7330687140843,
40.0616647108614));
#188784=CARTESIAN_POINT('Ctrl Pts',(6.29144124886088,-58.7281504960662,
40.0668995033485));
#188785=CARTESIAN_POINT('Ctrl Pts',(6.28378931333054,-58.7236522470777,
40.0717933267481));
#188786=CARTESIAN_POINT('Ctrl Pts',(6.27564783709185,-58.719696482323,40.0762460303072));
#188787=CARTESIAN_POINT('Ctrl Pts',(6.27266957975555,-58.718249412399,40.0778748868748));
#188788=CARTESIAN_POINT('Ctrl Pts',(6.26962586933712,-58.7168752520897,
40.0794443522247));
#188789=CARTESIAN_POINT('Ctrl Pts',(6.26651766855732,-58.7155811795664,
40.0809482021492));
#188790=CARTESIAN_POINT('Ctrl Pts',(6.26577025010559,-58.7152699983557,
40.0813098278168));
#188791=CARTESIAN_POINT('Ctrl Pts',(6.26501853257419,-58.7149635750523,
40.0816679525672));
#188792=CARTESIAN_POINT('Ctrl Pts',(6.26426260461821,-58.7146620123681,
40.082022419258));
#188793=CARTESIAN_POINT('Ctrl Pts',(6.26353029941086,-58.7143698735178,
40.0823658088648));
#188794=CARTESIAN_POINT('Ctrl Pts',(6.26279404284355,-58.7140822962414,
40.0827057654616));
#188795=CARTESIAN_POINT('Ctrl Pts',(6.26205391928439,-58.7137993735012,
40.0830421470151));
#188796=CARTESIAN_POINT('Ctrl Pts',(6.25394501035227,-58.7106996279152,
40.0867275956806));
#188797=CARTESIAN_POINT('Ctrl Pts',(6.24536644325941,-58.7081569420199,
40.0899823432031));
#188798=CARTESIAN_POINT('Ctrl Pts',(6.23645973859677,-58.7062958387084,
40.0926299529356));
#188799=CARTESIAN_POINT('Ctrl Pts',(6.23276586269276,-58.7055239836916,
40.0937279956084));
#188800=CARTESIAN_POINT('Ctrl Pts',(6.22901585349531,-58.7048690642115,
40.0947220371802));
#188801=CARTESIAN_POINT('Ctrl Pts',(6.22522076267779,-58.7043384037134,
40.0956014538692));
#188802=CARTESIAN_POINT('Ctrl Pts',(6.21874783981215,-58.7034333069351,
40.097101390674));
#188803=CARTESIAN_POINT('Ctrl Pts',(6.21214524099542,-58.7028917011005,
40.0982667904316));
#188804=CARTESIAN_POINT('Ctrl Pts',(6.20547453342054,-58.7027523988018,
40.0990539325582));
#188805=CARTESIAN_POINT('Ctrl Pts',(6.2021391796331,-58.7026827476525,40.0994475036216));
#188806=CARTESIAN_POINT('Ctrl Pts',(6.19878688248348,-58.7027151167906,
40.0997467259952));
#188807=CARTESIAN_POINT('Ctrl Pts',(6.19542538555006,-58.7028544030467,
40.0999473488896));
#188808=CARTESIAN_POINT('Ctrl Pts',(6.19206388861663,-58.7029936893028,
40.100147971784));
#188809=CARTESIAN_POINT('Ctrl Pts',(6.18869323212197,-58.7032398710655,
40.10025));
#188810=CARTESIAN_POINT('Ctrl Pts',(6.1853204982938,-58.7035958781039,40.10025));
#188811=CARTESIAN_POINT('Origin',(-0.0152400000001978,-58.2637721346185,
39.92499));
#188812=CARTESIAN_POINT('Ctrl Pts',(-0.190500000000213,-62.6567671111299,
39.92499));
#188813=CARTESIAN_POINT('Ctrl Pts',(-0.190500000000213,-62.6673774406538,
39.9348354642013));
#188814=CARTESIAN_POINT('Ctrl Pts',(-0.189662809673347,-62.6779562874462,
39.9446440828448));
#188815=CARTESIAN_POINT('Ctrl Pts',(-0.188003604115532,-62.6884465439468,
39.9543641760318));
#188816=CARTESIAN_POINT('Ctrl Pts',(-0.186398312858405,-62.6985959295766,
39.9637684240697));
#188817=CARTESIAN_POINT('Ctrl Pts',(-0.18402329031191,-62.7086636500137,
39.9730909636378));
#188818=CARTESIAN_POINT('Ctrl Pts',(-0.18084626121144,-62.7185939622152,
39.9822808977121));
#188819=CARTESIAN_POINT('Ctrl Pts',(-0.177840987312561,-62.7279874260843,
39.9909740094629));
#188820=CARTESIAN_POINT('Ctrl Pts',(-0.174117798732319,-62.7372588214061,
39.9995492764979));
#188821=CARTESIAN_POINT('Ctrl Pts',(-0.169611579427885,-62.7463424082288,
40.0079462328672));
#188822=CARTESIAN_POINT('Ctrl Pts',(-0.165461025550434,-62.7547090486342,
40.0156804369666));
#188823=CARTESIAN_POINT('Ctrl Pts',(-0.160645870590088,-62.7629168328826,
40.0232638017397));
#188824=CARTESIAN_POINT('Ctrl Pts',(-0.155086395964948,-62.7708892610779,
40.0306257269941));
#188825=CARTESIAN_POINT('Ctrl Pts',(-0.153473803707011,-62.7732017594436,
40.0327611416635));
#188826=CARTESIAN_POINT('Ctrl Pts',(-0.15179840377153,-62.7754942590266,
40.0348777427262));
#188827=CARTESIAN_POINT('Ctrl Pts',(-0.150057792857863,-62.7777643638146,
40.0369733168701));
#188828=CARTESIAN_POINT('Ctrl Pts',(-0.148170858717248,-62.7802253033581,
40.039245053974));
#188829=CARTESIAN_POINT('Ctrl Pts',(-0.146210769553979,-62.7826571567199,
40.041487875195));
#188830=CARTESIAN_POINT('Ctrl Pts',(-0.144175421826364,-62.7850565204095,
40.0436985701601));
#188831=CARTESIAN_POINT('Ctrl Pts',(-0.138589394016836,-62.791641592883,
40.0497658398386));
#188832=CARTESIAN_POINT('Ctrl Pts',(-0.13241078666925,-62.7979456687653,
40.0555581699984));
#188833=CARTESIAN_POINT('Ctrl Pts',(-0.125664597436941,-62.8038680995981,
40.0609828468886));
#188834=CARTESIAN_POINT('Ctrl Pts',(-0.119492200548591,-62.8092868022738,
40.0659461317304));
#188835=CARTESIAN_POINT('Ctrl Pts',(-0.11284434746055,-62.8143744518938,
40.0706039980706));
#188836=CARTESIAN_POINT('Ctrl Pts',(-0.105708043833672,-62.8190433630433,
40.0748843180602));
#188837=CARTESIAN_POINT('Ctrl Pts',(-0.102202714803807,-62.8213367169483,
40.0769867972569));
#188838=CARTESIAN_POINT('Ctrl Pts',(-0.0985794274535627,-62.8235285419788,
40.0789976708174));
#188839=CARTESIAN_POINT('Ctrl Pts',(-0.0948363533474329,-62.8256051102648,
40.08090504915));
#188840=CARTESIAN_POINT('Ctrl Pts',(-0.0941261414938337,-62.825999118871,
40.0812669556105));
#188841=CARTESIAN_POINT('Ctrl Pts',(-0.0934111032314831,-62.8263888407139,
40.0816253922032));
#188842=CARTESIAN_POINT('Ctrl Pts',(-0.0926913160162872,-62.826774159152,
40.0819801989139));
#188843=CARTESIAN_POINT('Ctrl Pts',(-0.0919940221515661,-62.8271474363889,
40.0823239179149));
#188844=CARTESIAN_POINT('Ctrl Pts',(-0.0912922715312453,-62.8275165811343,
40.0826642303498));
#188845=CARTESIAN_POINT('Ctrl Pts',(-0.0905861384171559,-62.8278814873655,
40.0830009916099));
#188846=CARTESIAN_POINT('Ctrl Pts',(-0.0828908452419125,-62.8318581602825,
40.0866709464313));
#188847=CARTESIAN_POINT('Ctrl Pts',(-0.0746698316629355,-62.8353337180914,
40.0899175831879));
#188848=CARTESIAN_POINT('Ctrl Pts',(-0.0660491922293915,-62.8381654210188,
40.0925642067063));
#188849=CARTESIAN_POINT('Ctrl Pts',(-0.0624086426652736,-62.839361266749,
40.0936818922528));
#188850=CARTESIAN_POINT('Ctrl Pts',(-0.0586971697057687,-62.8404425512865,
40.0946930094791));
#188851=CARTESIAN_POINT('Ctrl Pts',(-0.0549254519866895,-62.8414000604479,
40.0955863397546));
#188852=CARTESIAN_POINT('Ctrl Pts',(-0.0485739735924287,-62.8430124819501,
40.0970906856166));
#188853=CARTESIAN_POINT('Ctrl Pts',(-0.0420529246954846,-62.8442717146911,
40.0982599215483));
#188854=CARTESIAN_POINT('Ctrl Pts',(-0.0354197192409226,-62.8451307298764,
40.0990497370454));
#188855=CARTESIAN_POINT('Ctrl Pts',(-0.033761417877282,-62.8453454836727,
40.0992471909196));
#188856=CARTESIAN_POINT('Ctrl Pts',(-0.0320960919388051,-62.8455349903695,
40.0994209989363));
#188857=CARTESIAN_POINT('Ctrl Pts',(-0.0304246312368034,-62.8456982067485,
40.0995705982975));
#188858=CARTESIAN_POINT('Ctrl Pts',(-0.027917440183801,-62.845943031317,
40.0997949973393));
#188859=CARTESIAN_POINT('Ctrl Pts',(-0.0253964615341821,-62.8461286892223,
40.0999649129781));
#188860=CARTESIAN_POINT('Ctrl Pts',(-0.0228647168033253,-62.846253337618,
40.1000786629733));
#188861=CARTESIAN_POINT('Ctrl Pts',(-0.0203329720724685,-62.8463779860137,
40.1001924129685));
#188862=CARTESIAN_POINT('Ctrl Pts',(-0.0177904683743677,-62.8464416340693,
40.10025));
#188863=CARTESIAN_POINT('Ctrl Pts',(-0.0152400000002138,-62.8464427007196,
40.10025));
#188864=CARTESIAN_POINT('Ctrl Pts',(-0.0152400000002007,-59.0285534841296,
40.10025));
#188865=CARTESIAN_POINT('Ctrl Pts',(-0.0238699985093192,-59.0285496414744,
40.10025));
#188866=CARTESIAN_POINT('Ctrl Pts',(-0.0324255116353325,-59.0292582026621,
40.0995786334241));
#188867=CARTESIAN_POINT('Ctrl Pts',(-0.0407807192224094,-59.0305954788489,
40.0983063763367));
#188868=CARTESIAN_POINT('Ctrl Pts',(-0.046177326030172,-59.0314592220531,
40.0974846287994));
#188869=CARTESIAN_POINT('Ctrl Pts',(-0.0514905268410185,-59.0325843328198,
40.0964130309339));
#188870=CARTESIAN_POINT('Ctrl Pts',(-0.0566895722964741,-59.0339399880044,
40.0951176960924));
#188871=CARTESIAN_POINT('Ctrl Pts',(-0.063580609227685,-59.0357368312948,
40.0934008039614));
#188872=CARTESIAN_POINT('Ctrl Pts',(-0.0702685278903685,-59.0379438906768,
40.0912909372157));
#188873=CARTESIAN_POINT('Ctrl Pts',(-0.0766865040606948,-59.0405007795597,
40.0888630467852));
#188874=CARTESIAN_POINT('Ctrl Pts',(-0.079895492145858,-59.0417792240012,
40.0876491015699));
#188875=CARTESIAN_POINT('Ctrl Pts',(-0.0830371938951596,-59.0431451240706,
40.0863558569272));
#188876=CARTESIAN_POINT('Ctrl Pts',(-0.086104670364025,-59.0445909239228,
40.0849936342771));
#188877=CARTESIAN_POINT('Ctrl Pts',(-0.0876384085984576,-59.0453138238489,
40.0843125229521));
#188878=CARTESIAN_POINT('Ctrl Pts',(-0.0891536069438513,-59.0460566986719,
40.0836141747075));
#188879=CARTESIAN_POINT('Ctrl Pts',(-0.0906495011922853,-59.0468186034776,
40.082899916161));
#188880=CARTESIAN_POINT('Ctrl Pts',(-0.0910234747543938,-59.047009079679,
40.0827213515244));
#188881=CARTESIAN_POINT('Ctrl Pts',(-0.0913962421599235,-59.0472007452523,
40.0825417925842));
#188882=CARTESIAN_POINT('Ctrl Pts',(-0.0917677921729251,-59.0473935854286,
40.0823612602361));
#188883=CARTESIAN_POINT('Ctrl Pts',(-0.09288244221193,-59.0479721059574,
40.0818196631918));
#188884=CARTESIAN_POINT('Ctrl Pts',(-0.0939861339740177,-59.0485611979309,
40.0812693052022));
#188885=CARTESIAN_POINT('Ctrl Pts',(-0.0950785796751375,-59.0491604624443,
40.0807107531875));
#188886=CARTESIAN_POINT('Ctrl Pts',(-0.102773626133571,-59.0533816042977,
40.0767763849181));
#188887=CARTESIAN_POINT('Ctrl Pts',(-0.109958823466872,-59.0580834293368,
40.0724140586136));
#188888=CARTESIAN_POINT('Ctrl Pts',(-0.116642428647321,-59.0631465696374,
40.0677221223766));
#188889=CARTESIAN_POINT('Ctrl Pts',(-0.119883969937292,-59.0656021872118,
40.0654465383719));
#188890=CARTESIAN_POINT('Ctrl Pts',(-0.123007567718441,-59.068143371512,
40.0630928000678));
#188891=CARTESIAN_POINT('Ctrl Pts',(-0.126014035556628,-59.0707593633743,
40.0606689262479));
#188892=CARTESIAN_POINT('Ctrl Pts',(-0.130616727761249,-59.0747642641417,
40.0569581447806));
#188893=CARTESIAN_POINT('Ctrl Pts',(-0.13494307027746,-59.0789414743144,
40.0530843804606));
#188894=CARTESIAN_POINT('Ctrl Pts',(-0.138985142830921,-59.0832455674828,
40.0490800251458));
#188895=CARTESIAN_POINT('Ctrl Pts',(-0.140862302235661,-59.0852444106167,
40.0472203818218));
#188896=CARTESIAN_POINT('Ctrl Pts',(-0.142678271527312,-59.0872703932642,
40.0453323608818));
#188897=CARTESIAN_POINT('Ctrl Pts',(-0.144431197308936,-59.0893195943183,
40.0434201572162));
#188898=CARTESIAN_POINT('Ctrl Pts',(-0.144565552163221,-59.0894766575049,
40.0432735943397));
#188899=CARTESIAN_POINT('Ctrl Pts',(-0.144699568925986,-59.0896338466134,
40.0431268995707));
#188900=CARTESIAN_POINT('Ctrl Pts',(-0.144833247843275,-59.0897911602042,
40.0429800745037));
#188901=CARTESIAN_POINT('Ctrl Pts',(-0.146711033602282,-59.0920009418701,
40.0409176249753));
#188902=CARTESIAN_POINT('Ctrl Pts',(-0.148520654545084,-59.0942367399983,
40.0388310783332));
#188903=CARTESIAN_POINT('Ctrl Pts',(-0.150262619641468,-59.0964928714566,
40.036725739981));
#188904=CARTESIAN_POINT('Ctrl Pts',(-0.15650899667944,-59.1045829576269,
40.0291763710713));
#188905=CARTESIAN_POINT('Ctrl Pts',(-0.161935290146647,-59.1129958342961,
40.0213310894585));
#188906=CARTESIAN_POINT('Ctrl Pts',(-0.166622470788754,-59.1216309196503,
40.0132837551304));
#188907=CARTESIAN_POINT('Ctrl Pts',(-0.171773211445404,-59.1311200109833,
40.0044405431303));
#188908=CARTESIAN_POINT('Ctrl Pts',(-0.176031864364012,-59.1408779306769,
39.9953528710572));
#188909=CARTESIAN_POINT('Ctrl Pts',(-0.179468536018904,-59.1508087658139,
39.9861103629519));
#188910=CARTESIAN_POINT('Ctrl Pts',(-0.18317927891942,-59.1615315754626,
39.976130773751));
#188911=CARTESIAN_POINT('Ctrl Pts',(-0.185932239426363,-59.1724570142908,
39.9659696935954));
#188912=CARTESIAN_POINT('Ctrl Pts',(-0.187766286101261,-59.1834936683209,
39.9557128217438));
#188913=CARTESIAN_POINT('Ctrl Pts',(-0.189584947008437,-59.1944377361602,
39.9455419945115));
#188914=CARTESIAN_POINT('Ctrl Pts',(-0.190500000000201,-59.205492595814,
39.9352756289317));
#188915=CARTESIAN_POINT('Ctrl Pts',(-0.190500000000201,-59.2165773020941,
39.92499));
#188916=CARTESIAN_POINT('Origin',(0.0152400000000056,5.56890342380664E-15,
39.92499));
#188917=CARTESIAN_POINT('Ctrl Pts',(0.0152399999997863,-62.8464427007196,
40.10025));
#188918=CARTESIAN_POINT('Ctrl Pts',(0.0238289333903676,-62.8464391086779,
40.10025));
#188919=CARTESIAN_POINT('Ctrl Pts',(0.0323412407625178,-62.8457180711405,
40.0995859581842));
#188920=CARTESIAN_POINT('Ctrl Pts',(0.0406531130503384,-62.844365806829,
40.0983275959621));
#188921=CARTESIAN_POINT('Ctrl Pts',(0.0459640037534202,-62.8435017743089,
40.0975235624068));
#188922=CARTESIAN_POINT('Ctrl Pts',(0.0511932363889303,-62.8423809556998,
40.096477705949));
#188923=CARTESIAN_POINT('Ctrl Pts',(0.0563116129572096,-62.841033859251,
40.0952149915961));
#188924=CARTESIAN_POINT('Ctrl Pts',(0.0632971699619951,-62.8391953428955,
40.0934916398701));
#188925=CARTESIAN_POINT('Ctrl Pts',(0.0700734120981451,-62.8369299537504,
40.091364392163));
#188926=CARTESIAN_POINT('Ctrl Pts',(0.0765705776092501,-62.8343031482014,
40.0889118607713));
#188927=CARTESIAN_POINT('Ctrl Pts',(0.0798191603648026,-62.8329897454269,
40.0876855950754));
#188928=CARTESIAN_POINT('Ctrl Pts',(0.0829981827950912,-62.8315859904681,
40.0863782327526));
#188929=CARTESIAN_POINT('Ctrl Pts',(0.0861004173276405,-62.8301000734874,
40.0850006373334));
#188930=CARTESIAN_POINT('Ctrl Pts',(0.0876515345939151,-62.8293571149971,
40.0843118396237));
#188931=CARTESIAN_POINT('Ctrl Pts',(0.0891834722994834,-62.8285936160519,
40.0836054919164));
#188932=CARTESIAN_POINT('Ctrl Pts',(0.0906954364276482,-62.82781060087,
40.0828829920418));
#188933=CARTESIAN_POINT('Ctrl Pts',(0.0910734274596893,-62.8276148470746,
40.0827023670731));
#188934=CARTESIAN_POINT('Ctrl Pts',(0.091450170514115,-62.8274178735164,
40.0825207326933));
#188935=CARTESIAN_POINT('Ctrl Pts',(0.091825653932623,-62.8272196962038,
40.0823381109275));
#188936=CARTESIAN_POINT('Ctrl Pts',(0.092952104188147,-62.8266251642659,
40.0817902456303));
#188937=CARTESIAN_POINT('Ctrl Pts',(0.0940672158684322,-62.826019798519,
40.0812334935553));
#188938=CARTESIAN_POINT('Ctrl Pts',(0.0951706907486232,-62.8254040313373,
40.0806684524227));
#188939=CARTESIAN_POINT('Ctrl Pts',(0.102796386827374,-62.8211486980556,
40.0767636676137));
#188940=CARTESIAN_POINT('Ctrl Pts',(0.109916699411343,-62.8164204928784,
40.0724404510888));
#188941=CARTESIAN_POINT('Ctrl Pts',(0.116542502759708,-62.8113377077395,
40.0677949937409));
#188942=CARTESIAN_POINT('Ctrl Pts',(0.119835508836344,-62.8088115774775,
40.0654862141906));
#188943=CARTESIAN_POINT('Ctrl Pts',(0.123006400629162,-62.8061972539432,
40.0630972003216));
#188944=CARTESIAN_POINT('Ctrl Pts',(0.126056303769755,-62.8035061084565,
40.0606363359906));
#188945=CARTESIAN_POINT('Ctrl Pts',(0.13278484564307,-62.7975690395532,
40.0552073017123));
#188946=CARTESIAN_POINT('Ctrl Pts',(0.138932019324476,-62.7912680187378,
40.0494204304519));
#188947=CARTESIAN_POINT('Ctrl Pts',(0.144445113412955,-62.7847385034067,
40.0434049749851));
#188948=CARTESIAN_POINT('Ctrl Pts',(0.146459116207252,-62.7823531891148,
40.0412074532442));
#188949=CARTESIAN_POINT('Ctrl Pts',(0.148396130390766,-62.7799396422114,
40.0389814735788));
#188950=CARTESIAN_POINT('Ctrl Pts',(0.150257579786274,-62.7775029828616,
40.0367321210016));
#188951=CARTESIAN_POINT('Ctrl Pts',(0.156509991333158,-62.7693185019449,
40.0291767837143));
#188952=CARTESIAN_POINT('Ctrl Pts',(0.161942805717456,-62.7608162581028,
40.0213235332582));
#188953=CARTESIAN_POINT('Ctrl Pts',(0.166635979460758,-62.7520965944505,
40.0132649215867));
#188954=CARTESIAN_POINT('Ctrl Pts',(0.171794333347662,-62.7425126511844,
40.0044075527545));
#188955=CARTESIAN_POINT('Ctrl Pts',(0.176059615356826,-62.7326655363514,
39.9953016253735));
#188956=CARTESIAN_POINT('Ctrl Pts',(0.179500292056051,-62.7226511116317,
39.9860353422376));
#188957=CARTESIAN_POINT('Ctrl Pts',(0.183206048282415,-62.7118651471246,
39.9760551582716));
#188958=CARTESIAN_POINT('Ctrl Pts',(0.185955767118563,-62.7008840239675,
39.9658879738179));
#188959=CARTESIAN_POINT('Ctrl Pts',(0.1877854580346,-62.6897991274289,39.955617464328));
#188960=CARTESIAN_POINT('Ctrl Pts',(0.18959044194574,-62.6788639144192,
39.9454856413922));
#188961=CARTESIAN_POINT('Ctrl Pts',(0.190499999999787,-62.6678262782739,
39.9352519465123));
#188962=CARTESIAN_POINT('Ctrl Pts',(0.190499999999787,-62.6567671111299,
39.92499));
#188963=CARTESIAN_POINT('Ctrl Pts',(0.190499999999799,-59.2165773020941,
39.92499));
#188964=CARTESIAN_POINT('Ctrl Pts',(0.190499999999799,-59.2059936184294,
39.9348107241721));
#188965=CARTESIAN_POINT('Ctrl Pts',(0.189665225488479,-59.1954479901466,
39.9446038383166));
#188966=CARTESIAN_POINT('Ctrl Pts',(0.18800876231396,-59.1849969778467,
39.954315806938));
#188967=CARTESIAN_POINT('Ctrl Pts',(0.186409301376905,-59.1749056059505,
39.9636935671386));
#188968=CARTESIAN_POINT('Ctrl Pts',(0.184043455438109,-59.1649012152157,
39.9729968320982));
#188969=CARTESIAN_POINT('Ctrl Pts',(0.180877423726644,-59.1550396955543,
39.9821731151328));
#188970=CARTESIAN_POINT('Ctrl Pts',(0.177884532219545,-59.1457174710375,
39.9908475764344));
#188971=CARTESIAN_POINT('Ctrl Pts',(0.174176304387074,-59.136522058346,
39.9994093733838));
#188972=CARTESIAN_POINT('Ctrl Pts',(0.169686797572568,-59.1275197082963,
40.0077966115833));
#188973=CARTESIAN_POINT('Ctrl Pts',(0.16555203711349,-59.1192286949263,
40.0155211172587));
#188974=CARTESIAN_POINT('Ctrl Pts',(0.160754293903832,-59.1111009786095,
40.0230979941014));
#188975=CARTESIAN_POINT('Ctrl Pts',(0.155213515013513,-59.1032135992732,
40.0304554104741));
#188976=CARTESIAN_POINT('Ctrl Pts',(0.153561366596104,-59.1008617419719,
40.0326492435176));
#188977=CARTESIAN_POINT('Ctrl Pts',(0.151842962927694,-59.0985314603582,
40.0348233715058));
#188978=CARTESIAN_POINT('Ctrl Pts',(0.150055686179939,-59.096225375957,
40.0369753512356));
#188979=CARTESIAN_POINT('Ctrl Pts',(0.148286670996504,-59.0939428540559,
40.0391053430352));
#188980=CARTESIAN_POINT('Ctrl Pts',(0.146452235168709,-59.0916862380348,
40.041211089324));
#188981=CARTESIAN_POINT('Ctrl Pts',(0.144552116609772,-59.0894604907299,
40.0432881154904));
#188982=CARTESIAN_POINT('Ctrl Pts',(0.144419986081224,-59.0893057166152,
40.043432547828));
#188983=CARTESIAN_POINT('Ctrl Pts',(0.144287542501902,-59.0891510807051,
40.0435768364421));
#188984=CARTESIAN_POINT('Ctrl Pts',(0.144154785043746,-59.0889965840074,
40.0437209807855));
#188985=CARTESIAN_POINT('Ctrl Pts',(0.138334211749301,-59.0822228828153,
40.050040796842));
#188986=CARTESIAN_POINT('Ctrl Pts',(0.131883990153885,-59.0757535782845,
40.0560490279345));
#188987=CARTESIAN_POINT('Ctrl Pts',(0.124808417215064,-59.0697047694307,
40.0616647108615));
#188988=CARTESIAN_POINT('Ctrl Pts',(0.118212753509824,-59.0640662283031,
40.0668995033486));
#188989=CARTESIAN_POINT('Ctrl Pts',(0.111072931137127,-59.0587927761312,
40.0717933267482));
#188990=CARTESIAN_POINT('Ctrl Pts',(0.103389544768,-59.0540076654697,40.0762460303072));
#188991=CARTESIAN_POINT('Ctrl Pts',(0.100578862632434,-59.0522572100837,
40.0778748868748));
#188992=CARTESIAN_POINT('Ctrl Pts',(0.0976954648435965,-59.0505724231957,
40.0794443522248));
#188993=CARTESIAN_POINT('Ctrl Pts',(0.094739558525147,-59.048960544286,
40.0809482021492));
#188994=CARTESIAN_POINT('Ctrl Pts',(0.0940287618036509,-59.0485729412563,
40.0813098278168));
#188995=CARTESIAN_POINT('Ctrl Pts',(0.0933131922165579,-59.0481896206935,
40.0816679525672));
#188996=CARTESIAN_POINT('Ctrl Pts',(0.0925929271969717,-59.0478106940136,
40.082022419258));
#188997=CARTESIAN_POINT('Ctrl Pts',(0.0918951704592475,-59.0474436087926,
40.0823658088648));
#188998=CARTESIAN_POINT('Ctrl Pts',(0.091193007193228,-59.0470806471271,
40.0827057654616));
#188999=CARTESIAN_POINT('Ctrl Pts',(0.0904865115876297,-59.0467219102889,
40.0830421470151));
#189000=CARTESIAN_POINT('Ctrl Pts',(0.0827460357497242,-59.0427915336441,
40.0867275956806));
#189001=CARTESIAN_POINT('Ctrl Pts',(0.0744802459942153,-59.039366072413,
40.0899823432031));
#189002=CARTESIAN_POINT('Ctrl Pts',(0.0658168714608038,-59.036584160269,
40.0926299529356));
#189003=CARTESIAN_POINT('Ctrl Pts',(0.0622239118142435,-59.035430418383,
40.0937279956084));
#189004=CARTESIAN_POINT('Ctrl Pts',(0.0585629032863412,-59.0343871039217,
40.0947220371802));
#189005=CARTESIAN_POINT('Ctrl Pts',(0.0548440714997746,-59.0334626554262,
40.0956014538692));
#189006=CARTESIAN_POINT('Ctrl Pts',(0.0485012163582068,-59.0318859121827,
40.097101390674));
#189007=CARTESIAN_POINT('Ctrl Pts',(0.0419914004942192,-59.0306571138137,
40.0982667904316));
#189008=CARTESIAN_POINT('Ctrl Pts',(0.0353717968086245,-59.0298212958157,
40.0990539325582));
#189009=CARTESIAN_POINT('Ctrl Pts',(0.0320619949658271,-59.0294033868167,
40.0994475036216));
#189010=CARTESIAN_POINT('Ctrl Pts',(0.0287246785544799,-59.0290851681639,
40.0997467259952));
#189011=CARTESIAN_POINT('Ctrl Pts',(0.0253670368746702,-59.0288723192866,
40.0999473488896));
#189012=CARTESIAN_POINT('Ctrl Pts',(0.0220093951948606,-59.0286594704093,
40.100147971784));
#189013=CARTESIAN_POINT('Ctrl Pts',(0.0186314705078069,-59.0285519740191,
40.10025));
#189014=CARTESIAN_POINT('Ctrl Pts',(0.0152399999997995,-59.0285534841296,
40.10025));
#189015=CARTESIAN_POINT('Origin',(-6.10537907909402,-57.9430040808458,39.92499));
#189016=CARTESIAN_POINT('Ctrl Pts',(-6.73887200051354,-62.2936141127569,
39.92499));
#189017=CARTESIAN_POINT('Ctrl Pts',(-6.73998108195343,-62.3041663177855,
39.9348354642016));
#189018=CARTESIAN_POINT('Ctrl Pts',(-6.74025426844112,-62.3147747227668,
39.9446440828455));
#189019=CARTESIAN_POINT('Ctrl Pts',(-6.7397006825762,-62.3253809467521,
39.9543641760327));
#189020=CARTESIAN_POINT('Ctrl Pts',(-6.7391650849555,-62.3356425316138,
39.9637684240707));
#189021=CARTESIAN_POINT('Ctrl Pts',(-6.73785543637686,-62.3459033574821,
39.973090963639));
#189022=CARTESIAN_POINT('Ctrl Pts',(-6.73573381164832,-62.3561113603641,
39.9822808977133));
#189023=CARTESIAN_POINT('Ctrl Pts',(-6.73372688529723,-62.3657675025179,
39.9909740094642));
#189024=CARTESIAN_POINT('Ctrl Pts',(-6.73099321743882,-62.375377287347,
39.9995492764993));
#189025=CARTESIAN_POINT('Ctrl Pts',(-6.72746117704663,-62.3848821415098,
40.0079462328686));
#189026=CARTESIAN_POINT('Ctrl Pts',(-6.72420791240176,-62.3936367996024,
40.0156804369681));
#189027=CARTESIAN_POINT('Ctrl Pts',(-6.72027708243827,-62.4023029414984,
40.0232638017413));
#189028=CARTESIAN_POINT('Ctrl Pts',(-6.7155814088644,-62.4108128192372,
40.0306257269957));
#189029=CARTESIAN_POINT('Ctrl Pts',(-6.71421937245637,-62.4132812112848,
40.0327611416645));
#189030=CARTESIAN_POINT('Ctrl Pts',(-6.71279278199583,-62.4157362792952,
40.0348777427268));
#189031=CARTESIAN_POINT('Ctrl Pts',(-6.7112989968962,-62.418175891595,40.03697331687));
#189032=CARTESIAN_POINT('Ctrl Pts',(-6.70967963780691,-62.4208205881801,
40.039245053974));
#189033=CARTESIAN_POINT('Ctrl Pts',(-6.70798448411196,-62.4234440047029,
40.041487875195));
#189034=CARTESIAN_POINT('Ctrl Pts',(-6.70621108803145,-62.4260429761973,
40.0436985701601));
#189035=CARTESIAN_POINT('Ctrl Pts',(-6.7013439885729,-62.4331758738575,
40.0497658398386));
#189036=CARTESIAN_POINT('Ctrl Pts',(-6.69585818364715,-62.4400912556837,
40.0555581699984));
#189037=CARTESIAN_POINT('Ctrl Pts',(-6.68976801333909,-62.4466864116141,
40.0609828468885));
#189038=CARTESIAN_POINT('Ctrl Pts',(-6.68419583815052,-62.4527206212308,
40.0659461317302));
#189039=CARTESIAN_POINT('Ctrl Pts',(-6.67811620689394,-62.458475290041,
40.0706039980702));
#189040=CARTESIAN_POINT('Ctrl Pts',(-6.67150703079287,-62.463864571258,
40.0748843180598));
#189041=CARTESIAN_POINT('Ctrl Pts',(-6.6682606250814,-62.4665117685873,
40.0769867972566));
#189042=CARTESIAN_POINT('Ctrl Pts',(-6.66488629458032,-62.4690703232298,
40.0789976708173));
#189043=CARTESIAN_POINT('Ctrl Pts',(-6.66138078591733,-62.4715267736418,
40.08090504915));
#189044=CARTESIAN_POINT('Ctrl Pts',(-6.6607156497927,-62.4719928611813,
40.0812669556105));
#189045=CARTESIAN_POINT('Ctrl Pts',(-6.66004526561012,-62.472455189938,
40.0816253922033));
#189046=CARTESIAN_POINT('Ctrl Pts',(-6.65936969820881,-62.4729136358129,
40.0819801989139));
#189047=CARTESIAN_POINT('Ctrl Pts',(-6.65871524228878,-62.4733577552541,
40.0823239179149));
#189048=CARTESIAN_POINT('Ctrl Pts',(-6.65805592206474,-62.4737982306999,
40.0826642303498));
#189049=CARTESIAN_POINT('Ctrl Pts',(-6.65739180030931,-62.4742349489459,
40.0830009916099));
#189050=CARTESIAN_POINT('Ctrl Pts',(-6.65015433826397,-62.4789942144027,
40.0866709464314));
#189051=CARTESIAN_POINT('Ctrl Pts',(-6.64234165497406,-62.4833100626583,
40.0899175831881));
#189052=CARTESIAN_POINT('Ctrl Pts',(-6.63406423386048,-62.4870273554132,
40.0925642067066));
#189053=CARTESIAN_POINT('Ctrl Pts',(-6.63056862752451,-62.4885971912266,
40.093681892253));
#189054=CARTESIAN_POINT('Ctrl Pts',(-6.62699051141353,-62.4900605069391,
40.0946930094792));
#189055=CARTESIAN_POINT('Ctrl Pts',(-6.62333954252022,-62.491407022622,
40.0955863397546));
#189056=CARTESIAN_POINT('Ctrl Pts',(-6.61719140213093,-62.4936745213866,
40.0970906856166));
#189057=CARTESIAN_POINT('Ctrl Pts',(-6.61083770188548,-62.4956084911391,
40.0982599215483));
#189058=CARTESIAN_POINT('Ctrl Pts',(-6.60433062536177,-62.4971561593225,
40.0990497370453));
#189059=CARTESIAN_POINT('Ctrl Pts',(-6.60270385623084,-62.4975430763684,
40.0992471909196));
#189060=CARTESIAN_POINT('Ctrl Pts',(-6.60106746196587,-62.4979056188888,
40.0994209989363));
#189061=CARTESIAN_POINT('Ctrl Pts',(-6.59942221845775,-62.4982426563699,
40.0995705982975));
#189062=CARTESIAN_POINT('Ctrl Pts',(-6.59695435319557,-62.4987482125917,
40.0997949973393));
#189063=CARTESIAN_POINT('Ctrl Pts',(-6.59446659126629,-62.4991963674676,
40.0999649129781));
#189064=CARTESIAN_POINT('Ctrl Pts',(-6.5919617450032,-62.4995849724124,
40.1000786629733));
#189065=CARTESIAN_POINT('Ctrl Pts',(-6.58945689874012,-62.4999735773571,
40.1001924129685));
#189066=CARTESIAN_POINT('Ctrl Pts',(-6.58693497617671,-62.5003026407462,
40.10025));
#189067=CARTESIAN_POINT('Ctrl Pts',(-6.5843985910305,-62.5005702980931,
40.10025));
#189068=CARTESIAN_POINT('Ctrl Pts',(-6.18532049829418,-58.7035958781039,
40.10025));
#189069=CARTESIAN_POINT('Ctrl Pts',(-6.19390281910169,-58.702689976017,
40.10025));
#189070=CARTESIAN_POINT('Ctrl Pts',(-6.20248552904374,-58.7025003609928,
40.0995786334241));
#189071=CARTESIAN_POINT('Ctrl Pts',(-6.21093474935423,-58.7029569544313,
40.0983063763367));
#189072=CARTESIAN_POINT('Ctrl Pts',(-6.21639207873495,-58.7032518669434,
40.0974846287993));
#189073=CARTESIAN_POINT('Ctrl Pts',(-6.2217937793752,-58.7038154335198,
40.0964130309338));
#189074=CARTESIAN_POINT('Ctrl Pts',(-6.22710604846875,-58.7046202140516,
40.0951176960924));
#189075=CARTESIAN_POINT('Ctrl Pts',(-6.23414715684653,-58.7056869045457,
40.0934008039614));
#189076=CARTESIAN_POINT('Ctrl Pts',(-6.24102913891656,-58.7071827955652,
40.0912909372156));
#189077=CARTESIAN_POINT('Ctrl Pts',(-6.2476792244076,-58.7090548163569,
40.0888630467851));
#189078=CARTESIAN_POINT('Ctrl Pts',(-6.25100426715312,-58.7099908267528,
40.0876491015699));
#189079=CARTESIAN_POINT('Ctrl Pts',(-6.25427153376677,-58.7110208470228,
40.0863558569271));
#189080=CARTESIAN_POINT('Ctrl Pts',(-6.25747333351534,-58.7121380880307,
40.0849936342771));
#189081=CARTESIAN_POINT('Ctrl Pts',(-6.25907423338962,-58.7126967085347,
40.0843125229521));
#189082=CARTESIAN_POINT('Ctrl Pts',(-6.2606587828836,-58.7132771324571,
40.0836141747074));
#189083=CARTESIAN_POINT('Ctrl Pts',(-6.26222612320532,-58.7138784999415,
40.0828999161609));
#189084=CARTESIAN_POINT('Ctrl Pts',(-6.26261795828575,-58.7140288418126,
40.0827213515243));
#189085=CARTESIAN_POINT('Ctrl Pts',(-6.26300871814027,-58.7141804926178,
40.0825417925842));
#189086=CARTESIAN_POINT('Ctrl Pts',(-6.26339839005071,-58.7143334388435,
40.082361260236));
#189087=CARTESIAN_POINT('Ctrl Pts',(-6.26456740578202,-58.7147922775207,
40.0818196631917));
#189088=CARTESIAN_POINT('Ctrl Pts',(-6.26572662828387,-58.715262775183,
40.0812693052021));
#189089=CARTESIAN_POINT('Ctrl Pts',(-6.26687572965181,-58.7157445651924,
40.0807107531875));
#189090=CARTESIAN_POINT('Ctrl Pts',(-6.27496985131161,-58.7191382318078,
40.0767763849182));
#189091=CARTESIAN_POINT('Ctrl Pts',(-6.28260716192787,-58.7230632421218,
40.0724140586137));
#189092=CARTESIAN_POINT('Ctrl Pts',(-6.28978339589464,-58.7274000190313,
40.0677221223768));
#189093=CARTESIAN_POINT('Ctrl Pts',(-6.29326386161383,-58.7295033511461,
40.0654465383721));
#189094=CARTESIAN_POINT('Ctrl Pts',(-6.29663597408943,-58.731704109697,
40.0630928000679));
#189095=CARTESIAN_POINT('Ctrl Pts',(-6.29989941779165,-58.7339915094193,
40.0606689262479));
#189096=CARTESIAN_POINT('Ctrl Pts',(-6.30489552208954,-58.7374933585782,
40.0569581447805));
#189097=CARTESIAN_POINT('Ctrl Pts',(-6.30963480180889,-58.7411954596217,
40.0530843804605));
#189098=CARTESIAN_POINT('Ctrl Pts',(-6.31410463171063,-58.745053462885,
40.0490800251457));
#189099=CARTESIAN_POINT('Ctrl Pts',(-6.31618044384084,-58.7468451395592,
40.0472203818218));
#189100=CARTESIAN_POINT('Ctrl Pts',(-6.31819823791544,-58.7486702031823,
40.0453323608818));
#189101=CARTESIAN_POINT('Ctrl Pts',(-6.32015576082334,-58.7505249478605,
40.0434201572162));
#189102=CARTESIAN_POINT('Ctrl Pts',(-6.3203057972412,-58.750667106732,40.0432735943397));
#189103=CARTESIAN_POINT('Ctrl Pts',(-6.32045551058208,-58.7508094261759,
40.0431268995707));
#189104=CARTESIAN_POINT('Ctrl Pts',(-6.32060490094018,-58.7509519047346,
40.0429800745037));
#189105=CARTESIAN_POINT('Ctrl Pts',(-6.32270338507402,-58.7529532989256,
40.0409176249753));
#189106=CARTESIAN_POINT('Ctrl Pts',(-6.32473679726646,-58.7549876922215,
40.0388310783332));
#189107=CARTESIAN_POINT('Ctrl Pts',(-6.32670504965004,-58.757049379421,
40.036725739981));
#189108=CARTESIAN_POINT('Ctrl Pts',(-6.33376285265555,-58.7644422230594,
40.0291763710718));
#189109=CARTESIAN_POINT('Ctrl Pts',(-6.34003880538882,-58.772241810992,
40.0213310894596));
#189110=CARTESIAN_POINT('Ctrl Pts',(-6.34560292136685,-58.7803396486548,
40.0132837551322));
#189111=CARTESIAN_POINT('Ctrl Pts',(-6.35171732586152,-58.7892383587461,
40.0044405431331));
#189112=CARTESIAN_POINT('Ctrl Pts',(-6.35697262978372,-58.7984976730883,
39.995352871061));
#189113=CARTESIAN_POINT('Ctrl Pts',(-6.36142852992733,-58.8080148760634,
39.9861103629568));
#189114=CARTESIAN_POINT('Ctrl Pts',(-6.36623978380391,-58.818291066784,
39.9761307737578));
#189115=CARTESIAN_POINT('Ctrl Pts',(-6.37011968263616,-58.8288688921818,
39.9659696936042));
#189116=CARTESIAN_POINT('Ctrl Pts',(-6.37309732669698,-58.8396533761837,
39.9557128217545));
#189117=CARTESIAN_POINT('Ctrl Pts',(-6.37604999138425,-58.8503473894481,
39.9455419945187));
#189118=CARTESIAN_POINT('Ctrl Pts',(-6.37811557911233,-58.8612460403448,
39.9352756289354));
#189119=CARTESIAN_POINT('Ctrl Pts',(-6.37927424642597,-58.872270023448,
39.92499));
#189120=CARTESIAN_POINT('Origin',(0.0151565136854187,-0.0015930137801935,
39.92499));
#189121=CARTESIAN_POINT('Ctrl Pts',(-6.55408556365967,-62.5037563256534,
40.10025));
#189122=CARTESIAN_POINT('Ctrl Pts',(-6.54554330587437,-62.5046505412977,
40.10025));
#189123=CARTESIAN_POINT('Ctrl Pts',(-6.537002260867,-62.5048232320878,40.0995859581842));
#189124=CARTESIAN_POINT('Ctrl Pts',(-6.52859457177493,-62.5043472028589,
40.0983275959621));
#189125=CARTESIAN_POINT('Ctrl Pts',(-6.52322245869524,-62.5040430428431,
40.0975235624068));
#189126=CARTESIAN_POINT('Ctrl Pts',(-6.51790471489642,-62.5034749678471,
40.0964777059491));
#189127=CARTESIAN_POINT('Ctrl Pts',(-6.51267356740883,-62.5026702669707,
40.0952149915961));
#189128=CARTESIAN_POINT('Ctrl Pts',(-6.50553410072686,-62.5015720117389,
40.0934916398701));
#189129=CARTESIAN_POINT('Ctrl Pts',(-6.49855818190806,-62.5000273428098,
40.0913643921631));
#189130=CARTESIAN_POINT('Ctrl Pts',(-6.49182203260206,-62.4980940659029,
40.0889118607713));
#189131=CARTESIAN_POINT('Ctrl Pts',(-6.48845395794906,-62.4971274274495,
40.0876855950754));
#189132=CARTESIAN_POINT('Ctrl Pts',(-6.48514561818761,-62.4960636607365,
40.0863782327526));
#189133=CARTESIAN_POINT('Ctrl Pts',(-6.48190505740188,-62.494910155573,
40.0850006373334));
#189134=CARTESIAN_POINT('Ctrl Pts',(-6.48028477700901,-62.4943334029912,
40.0843118396237));
#189135=CARTESIAN_POINT('Ctrl Pts',(-6.47868142404705,-62.4937342176673,
40.0836054919164));
#189136=CARTESIAN_POINT('Ctrl Pts',(-6.47709589524289,-62.4931135352113,
40.0828829920417));
#189137=CARTESIAN_POINT('Ctrl Pts',(-6.47669951304185,-62.4929583645973,
40.0827023670731));
#189138=CARTESIAN_POINT('Ctrl Pts',(-6.47630424448195,-62.4928018504535,
40.0825207326933));
#189139=CARTESIAN_POINT('Ctrl Pts',(-6.47591010283095,-62.4926440074817,
40.0823381109275));
#189140=CARTESIAN_POINT('Ctrl Pts',(-6.47472767787796,-62.4921704785661,
40.0817902456303));
#189141=CARTESIAN_POINT('Ctrl Pts',(-6.47355539694489,-62.4916849899864,
40.0812334935553));
#189142=CARTESIAN_POINT('Ctrl Pts',(-6.47239360181831,-62.4911879405752,
40.0806684524227));
#189143=CARTESIAN_POINT('Ctrl Pts',(-6.46436487665219,-62.487753020747,
40.0767636676138));
#189144=CARTESIAN_POINT('Ctrl Pts',(-6.45678933786461,-62.483794992505,
40.0724404510891));
#189145=CARTESIAN_POINT('Ctrl Pts',(-6.44966853564077,-62.479432636437,
40.0677949937413));
#189146=CARTESIAN_POINT('Ctrl Pts',(-6.44612951648143,-62.4772645574455,
40.0654862141908));
#189147=CARTESIAN_POINT('Ctrl Pts',(-6.44270272394389,-62.4749960038953,
40.0630972003217));
#189148=CARTESIAN_POINT('Ctrl Pts',(-6.43938822718945,-62.4726384024734,
40.0606363359906));
#189149=CARTESIAN_POINT('Ctrl Pts',(-6.43207595228375,-62.4674371815967,
40.0552073017123));
#189150=CARTESIAN_POINT('Ctrl Pts',(-6.42530381744011,-62.461813233051,
40.0494204304519));
#189151=CARTESIAN_POINT('Ctrl Pts',(-6.41913840445446,-62.455895762341,
40.0434049749851));
#189152=CARTESIAN_POINT('Ctrl Pts',(-6.41688610134085,-62.4537340356674,
40.0412074532442));
#189153=CARTESIAN_POINT('Ctrl Pts',(-6.41470741397488,-62.4515361835425,
40.0389814735788));
#189154=CARTESIAN_POINT('Ctrl Pts',(-6.41260146153659,-62.4493074469123,
40.0367321210017));
#189155=CARTESIAN_POINT('Ctrl Pts',(-6.40552779014119,-62.4418213564088,
40.029176783714));
#189156=CARTESIAN_POINT('Ctrl Pts',(-6.39923601079914,-62.4339335724864,
40.0213235332575));
#189157=CARTESIAN_POINT('Ctrl Pts',(-6.39365709371068,-62.4257522463028,
40.0132649215856));
#189158=CARTESIAN_POINT('Ctrl Pts',(-6.3875252029643,-62.4167599996853,
40.004407552753));
#189159=CARTESIAN_POINT('Ctrl Pts',(-6.38225398283504,-62.4074126717511,
39.9953016253716));
#189160=CARTESIAN_POINT('Ctrl Pts',(-6.37778536209628,-62.3978127557455,
39.9860353422353));
#189161=CARTESIAN_POINT('Ctrl Pts',(-6.37297246609546,-62.3874732348838,
39.9760551582689));
#189162=CARTESIAN_POINT('Ctrl Pts',(-6.36908997057829,-62.3768396913524,
39.9658879738149));
#189163=CARTESIAN_POINT('Ctrl Pts',(-6.36611161569997,-62.3660067738162,
39.9556174643246));
#189164=CARTESIAN_POINT('Ctrl Pts',(-6.36317347866863,-62.355320137243,
39.9454856413899));
#189165=CARTESIAN_POINT('Ctrl Pts',(-6.3611151561247,-62.3444380411301,
39.9352519465111));
#189166=CARTESIAN_POINT('Ctrl Pts',(-6.35995915837823,-62.3334394572619,
39.92499));
#189167=CARTESIAN_POINT('Ctrl Pts',(-6.00036140429066,-58.912095367953,
39.92499));
#189168=CARTESIAN_POINT('Ctrl Pts',(-5.99925510810146,-58.9015696628146,
39.9348107241723));
#189169=CARTESIAN_POINT('Ctrl Pts',(-5.99898299131207,-58.8909945468898,
39.9446038383171));
#189170=CARTESIAN_POINT('Ctrl Pts',(-5.99953795195275,-58.8804276387785,
39.9543158069386));
#189171=CARTESIAN_POINT('Ctrl Pts',(-6.00007381527891,-58.8702243592796,
39.9636935671393));
#189172=CARTESIAN_POINT('Ctrl Pts',(-6.00138095727672,-58.8600274754035,
39.972996832099));
#189173=CARTESIAN_POINT('Ctrl Pts',(-6.00349883563959,-58.8498890377491,
39.9821731151337));
#189174=CARTESIAN_POINT('Ctrl Pts',(-6.00550089397094,-58.8403050390036,
39.9908475764353));
#189175=CARTESIAN_POINT('Ctrl Pts',(-6.00822762538565,-58.8307723843882,
39.9994093733847));
#189176=CARTESIAN_POINT('Ctrl Pts',(-6.01175153639566,-58.8213500689059,
40.0077966115843));
#189177=CARTESIAN_POINT('Ctrl Pts',(-6.01499699931784,-58.8126722744178,
40.0155211172596));
#189178=CARTESIAN_POINT('Ctrl Pts',(-6.01891888229176,-58.8040875818567,
40.0230979941022));
#189179=CARTESIAN_POINT('Ctrl Pts',(-6.02360485257435,-58.795664241307,
40.0304554104749));
#189180=CARTESIAN_POINT('Ctrl Pts',(-6.0250021143202,-58.7931525711912,
40.0326492435181));
#189181=CARTESIAN_POINT('Ctrl Pts',(-6.0264675236373,-58.7906554330095,
40.0348233715061));
#189182=CARTESIAN_POINT('Ctrl Pts',(-6.02800395803724,-58.7881751602884,
40.0369753512356));
#189183=CARTESIAN_POINT('Ctrl Pts',(-6.02952469386371,-58.7857202298425,
40.0391053430352));
#189184=CARTESIAN_POINT('Ctrl Pts',(-6.03111319985524,-58.783284225042,
40.041211089324));
#189185=CARTESIAN_POINT('Ctrl Pts',(-6.03277025542049,-58.7808720541407,
40.0432881154904));
#189186=CARTESIAN_POINT('Ctrl Pts',(-6.03288548382381,-58.7807043164937,
40.043432547828));
#189187=CARTESIAN_POINT('Ctrl Pts',(-6.0330010380093,-58.7805366835715,
40.0435768364421));
#189188=CARTESIAN_POINT('Ctrl Pts',(-6.03311691890582,-58.7803691562898,
40.0437209807855));
#189189=CARTESIAN_POINT('Ctrl Pts',(-6.03819756191453,-58.7730241465597,
40.050040796842));
#189190=CARTESIAN_POINT('Ctrl Pts',(-6.04393622206017,-58.7659160498048,
40.0560490279345));
#189191=CARTESIAN_POINT('Ctrl Pts',(-6.05034076157606,-58.7591607781928,
40.0616647108616));
#189192=CARTESIAN_POINT('Ctrl Pts',(-6.05631090550637,-58.752863690992,
40.0668995033488));
#189193=CARTESIAN_POINT('Ctrl Pts',(-6.06286038933353,-58.7468728126822,
40.0717933267484));
#189194=CARTESIAN_POINT('Ctrl Pts',(-6.07000150504434,-58.7413107827877,
40.0762460303076));
#189195=CARTESIAN_POINT('Ctrl Pts',(-6.0726138175574,-58.7392761202951,
40.077874886875));
#189196=CARTESIAN_POINT('Ctrl Pts',(-6.07530531160696,-58.7372991657063,
40.0794443522248));
#189197=CARTESIAN_POINT('Ctrl Pts',(-6.07807653793574,-58.735387140493,
40.0809482021492));
#189198=CARTESIAN_POINT('Ctrl Pts',(-6.07874292528937,-58.7349273623043,
40.0813098278168));
#189199=CARTESIAN_POINT('Ctrl Pts',(-6.07941450700203,-58.7344713442223,
40.0816679525672));
#189200=CARTESIAN_POINT('Ctrl Pts',(-6.08009121771094,-58.7340192051468,
40.082022419258));
#189201=CARTESIAN_POINT('Ctrl Pts',(-6.08074678121021,-58.7335811954175,
40.0823658088648));
#189202=CARTESIAN_POINT('Ctrl Pts',(-6.08140715812726,-58.7331468260468,
40.0827057654617));
#189203=CARTESIAN_POINT('Ctrl Pts',(-6.0820722852656,-58.7327162055066,
40.0830421470151));
#189204=CARTESIAN_POINT('Ctrl Pts',(-6.0893595217361,-58.7279982598321,
40.0867275956805));
#189205=CARTESIAN_POINT('Ctrl Pts',(-6.09722197243183,-58.7237275533352,
40.0899823432029));
#189206=CARTESIAN_POINT('Ctrl Pts',(-6.10554709909155,-58.7200553115704,
40.0926299529354));
#189207=CARTESIAN_POINT('Ctrl Pts',(-6.10899977726302,-58.7185323234526,
40.0937279956083));
#189208=CARTESIAN_POINT('Ctrl Pts',(-6.11253167434596,-58.7171120447816,
40.0947220371802));
#189209=CARTESIAN_POINT('Ctrl Pts',(-6.11613350280244,-58.7158039367398,
40.0956014538692));
#189210=CARTESIAN_POINT('Ctrl Pts',(-6.12227679657168,-58.7135728221602,
40.097101390674));
#189211=CARTESIAN_POINT('Ctrl Pts',(-6.12862250657806,-58.7116702942288,
40.0982667904316));
#189212=CARTESIAN_POINT('Ctrl Pts',(-6.13511848061117,-58.7101471179287,
40.0990539325582));
#189213=CARTESIAN_POINT('Ctrl Pts',(-6.13836646762773,-58.7093855297787,
40.0994475036216));
#189214=CARTESIAN_POINT('Ctrl Pts',(-6.14165223896381,-58.708720209805,
40.0997467259952));
#189215=CARTESIAN_POINT('Ctrl Pts',(-6.14496923836512,-58.7081575578111,
40.0999473488896));
#189216=CARTESIAN_POINT('Ctrl Pts',(-6.14828623776643,-58.7075949058171,
40.100147971784));
#189217=CARTESIAN_POINT('Ctrl Pts',(-6.15163442139611,-58.7071349090267,
40.10025));
#189218=CARTESIAN_POINT('Ctrl Pts',(-6.15500747092336,-58.7067819056643,
40.10025));
#189219=CARTESIAN_POINT('Origin',(-12.1286263473646,-56.9874003490101,39.92499));
#189220=CARTESIAN_POINT('Ctrl Pts',(-13.2134115091896,-61.2479592423877,
39.92499));
#189221=CARTESIAN_POINT('Ctrl Pts',(-13.215617520741,-61.2583377107544,
39.9348354642017));
#189222=CARTESIAN_POINT('Ctrl Pts',(-13.216998090955,-61.2688594460194,
39.9446440828456));
#189223=CARTESIAN_POINT('Ctrl Pts',(-13.2175561899856,-61.2794654334797,
39.9543641760328));
#189224=CARTESIAN_POINT('Ctrl Pts',(-13.218096154121,-61.289726789502,39.9637684240708));
#189225=CARTESIAN_POINT('Ctrl Pts',(-13.2178662282942,-61.300068301046,
39.9730909636391));
#189226=CARTESIAN_POINT('Ctrl Pts',(-13.2168232529022,-61.3104421535926,
39.9822808977134));
#189227=CARTESIAN_POINT('Ctrl Pts',(-13.2158366624041,-61.3202551793167,
39.9909740094642));
#189228=CARTESIAN_POINT('Ctrl Pts',(-13.2141224659048,-61.3300980668392,
39.9995492764992));
#189229=CARTESIAN_POINT('Ctrl Pts',(-13.2116033021987,-61.3399200511708,
40.0079462328684));
#189230=CARTESIAN_POINT('Ctrl Pts',(-13.2092829702348,-61.3489668090842,
40.0156804369678));
#189231=CARTESIAN_POINT('Ctrl Pts',(-13.2062795322641,-61.3579963605636,
40.0232638017409));
#189232=CARTESIAN_POINT('Ctrl Pts',(-13.202499106524,-61.3669504518443,
40.0306257269953));
#189233=CARTESIAN_POINT('Ctrl Pts',(-13.2014025487214,-61.3695476933549,
40.0327611416642));
#189234=CARTESIAN_POINT('Ctrl Pts',(-13.2002403977589,-61.3721384315545,
40.0348777427266));
#189235=CARTESIAN_POINT('Ctrl Pts',(-13.1990098046949,-61.374720822464,
40.03697331687));
#189236=CARTESIAN_POINT('Ctrl Pts',(-13.197675762694,-61.3775203002416,
40.039245053974));
#189237=CARTESIAN_POINT('Ctrl Pts',(-13.196264116926,-61.3803065372249,
40.041487875195));
#189238=CARTESIAN_POINT('Ctrl Pts',(-13.1947721021912,-61.3830766416486,
40.0436985701601));
#189239=CARTESIAN_POINT('Ctrl Pts',(-13.1906772560438,-61.3906792149761,
40.0497658398386));
#189240=CARTESIAN_POINT('Ctrl Pts',(-13.1859443571666,-61.3981301363758,
40.0555581699984));
#189241=CARTESIAN_POINT('Ctrl Pts',(-13.1805769309631,-61.4053257594952,
40.0609828468885));
#189242=CARTESIAN_POINT('Ctrl Pts',(-13.1756660273915,-61.4119093639898,
40.0659461317303));
#189243=CARTESIAN_POINT('Ctrl Pts',(-13.1702212276784,-61.4182680026346,
40.0706039980703));
#189244=CARTESIAN_POINT('Ctrl Pts',(-13.1642115906192,-61.4243186078266,
40.0748843180598));
#189245=CARTESIAN_POINT('Ctrl Pts',(-13.1612596765267,-61.4272906453321,
40.0769867972567));
#189246=CARTESIAN_POINT('Ctrl Pts',(-13.1581712727462,-61.4301878975264,
40.0789976708173));
#189247=CARTESIAN_POINT('Ctrl Pts',(-13.1549417366132,-61.4329973166795,
40.08090504915));
#189248=CARTESIAN_POINT('Ctrl Pts',(-13.1543289635881,-61.4335303765997,
40.0812669556105));
#189249=CARTESIAN_POINT('Ctrl Pts',(-13.1537105783546,-61.4340602468994,
40.0816253922032));
#189250=CARTESIAN_POINT('Ctrl Pts',(-13.153086632425,-61.4345867973821,
40.0819801989139));
#189251=CARTESIAN_POINT('Ctrl Pts',(-13.1524821848057,-61.4350968931622,
40.0823239179149));
#189252=CARTESIAN_POINT('Ctrl Pts',(-13.1518725186283,-61.4356038733672,
40.0826642303498));
#189253=CARTESIAN_POINT('Ctrl Pts',(-13.1512576844885,-61.4361076188515,
40.0830009916099));
#189254=CARTESIAN_POINT('Ctrl Pts',(-13.1445573487221,-61.4415973333396,
40.0866709464313));
#189255=CARTESIAN_POINT('Ctrl Pts',(-13.1372385931148,-61.446706186705,
40.0899175831879));
#189256=CARTESIAN_POINT('Ctrl Pts',(-13.1293950794796,-61.45126834185,40.0925642067064));
#189257=CARTESIAN_POINT('Ctrl Pts',(-13.1260827149658,-61.4531949682972,
40.0936818922529));
#189258=CARTESIAN_POINT('Ctrl Pts',(-13.1226771582918,-61.4550242827917,
40.0946930094791));
#189259=CARTESIAN_POINT('Ctrl Pts',(-13.119186939003,-61.4567450522888,
40.0955863397546));
#189260=CARTESIAN_POINT('Ctrl Pts',(-13.1133094969314,-61.4596427851248,
40.0970906856166));
#189261=CARTESIAN_POINT('Ctrl Pts',(-13.1071927578069,-61.4622303029112,
40.0982599215483));
#189262=CARTESIAN_POINT('Ctrl Pts',(-13.100883103106,-61.4644496675157,
40.0990497370454));
#189263=CARTESIAN_POINT('Ctrl Pts',(-13.0993056894308,-61.4650045086668,
40.0992471909196));
#189264=CARTESIAN_POINT('Ctrl Pts',(-13.0977161555174,-61.4655361149191,
40.0994209989363));
#189265=CARTESIAN_POINT('Ctrl Pts',(-13.0961151548353,-61.4660432808493,
40.0995705982975));
#189266=CARTESIAN_POINT('Ctrl Pts',(-13.0937136538122,-61.4668040297446,
40.0997949973393));
#189267=CARTESIAN_POINT('Ctrl Pts',(-13.0912863650436,-61.4675097715127,
40.0999649129781));
#189268=CARTESIAN_POINT('Ctrl Pts',(-13.0888358608681,-61.4681580753695,
40.1000786629733));
#189269=CARTESIAN_POINT('Ctrl Pts',(-13.0863853566926,-61.4688063792264,
40.1001924129685));
#189270=CARTESIAN_POINT('Ctrl Pts',(-13.0839116459753,-61.4693972526618,
40.10025));
#189271=CARTESIAN_POINT('Ctrl Pts',(-13.0814171332235,-61.4699285681954,
40.10025));
#189272=CARTESIAN_POINT('Ctrl Pts',(-12.2876333308473,-57.7354693911204,
40.10025));
#189273=CARTESIAN_POINT('Ctrl Pts',(-12.2960739442508,-57.7336713548546,
40.10025));
#189274=CARTESIAN_POINT('Ctrl Pts',(-12.3045898170431,-57.7325856410804,
40.099578633424));
#189275=CARTESIAN_POINT('Ctrl Pts',(-12.3130404786515,-57.7321565492375,
40.0983063763365));
#189276=CARTESIAN_POINT('Ctrl Pts',(-12.3184987389622,-57.7318793999343,
40.0974846287991));
#189277=CARTESIAN_POINT('Ctrl Pts',(-12.323929757269,-57.7318752477671,
40.0964130309337));
#189278=CARTESIAN_POINT('Ctrl Pts',(-12.3292970476685,-57.7321203363021,
40.0951176960924));
#189279=CARTESIAN_POINT('Ctrl Pts',(-12.336411083636,-57.7324451871157,
40.0934008039614));
#189280=CARTESIAN_POINT('Ctrl Pts',(-12.3434117286777,-57.7332135204776,
40.0912909372156));
#189281=CARTESIAN_POINT('Ctrl Pts',(-12.3502210637611,-57.7343801629266,
40.0888630467851));
#189282=CARTESIAN_POINT('Ctrl Pts',(-12.3536257313028,-57.734963484151,
40.0876491015699));
#189283=CARTESIAN_POINT('Ctrl Pts',(-12.3569827659241,-57.735646339504,
40.0863558569271));
#189284=CARTESIAN_POINT('Ctrl Pts',(-12.3602838093643,-57.7364227809414,
40.0849936342771));
#189285=CARTESIAN_POINT('Ctrl Pts',(-12.3619343310843,-57.7368110016601,
40.0843125229521));
#189286=CARTESIAN_POINT('Ctrl Pts',(-12.363570871071,-57.7372226154359,
40.0836141747074));
#189287=CARTESIAN_POINT('Ctrl Pts',(-12.3651924853575,-57.7376568568911,
40.0828999161609));
#189288=CARTESIAN_POINT('Ctrl Pts',(-12.3655978889291,-57.7377654172549,
40.0827213515243));
#189289=CARTESIAN_POINT('Ctrl Pts',(-12.3660023599859,-57.737875391774,
40.0825417925842));
#189290=CARTESIAN_POINT('Ctrl Pts',(-12.3664058844668,-57.7379867683383,
40.0823612602361));
#189291=CARTESIAN_POINT('Ctrl Pts',(-12.3676164579094,-57.7383208980313,
40.0818196631917));
#189292=CARTESIAN_POINT('Ctrl Pts',(-12.3688185104667,-57.7386676465115,
40.0812693052021));
#189293=CARTESIAN_POINT('Ctrl Pts',(-12.3700116777064,-57.7390266834246,
40.0807107531875));
#189294=CARTESIAN_POINT('Ctrl Pts',(-12.3784161936772,-57.7415556930807,
40.0767763849181));
#189295=CARTESIAN_POINT('Ctrl Pts',(-12.3864219416033,-57.7446608854354,
40.0724140586136));
#189296=CARTESIAN_POINT('Ctrl Pts',(-12.3940121800356,-57.7482237843187,
40.0677221223766));
#189297=CARTESIAN_POINT('Ctrl Pts',(-12.3976934374729,-57.749951786427,
40.0654465383719));
#189298=CARTESIAN_POINT('Ctrl Pts',(-12.4012771190728,-57.7517880072572,
40.0630928000678));
#189299=CARTESIAN_POINT('Ctrl Pts',(-12.4047617836667,-57.7537217536092,
40.0606689262479));
#189300=CARTESIAN_POINT('Ctrl Pts',(-12.4100965616936,-57.7566821841674,
40.0569581447805));
#189301=CARTESIAN_POINT('Ctrl Pts',(-12.4151968540757,-57.759868615088,
40.0530843804605));
#189302=CARTESIAN_POINT('Ctrl Pts',(-12.420045468934,-57.763238259355,40.0490800251457));
#189303=CARTESIAN_POINT('Ctrl Pts',(-12.4222971907576,-57.7648031395849,
40.0472203818218));
#189304=CARTESIAN_POINT('Ctrl Pts',(-12.424494702241,-57.7664072884047,
40.0453323608818));
#189305=CARTESIAN_POINT('Ctrl Pts',(-12.4266353752445,-57.7680472557362,
40.0434201572162));
#189306=CARTESIAN_POINT('Ctrl Pts',(-12.4267994493956,-57.7681729527703,
40.0432735943397));
#189307=CARTESIAN_POINT('Ctrl Pts',(-12.4269632190239,-57.7682988432679,
40.0431268995707));
#189308=CARTESIAN_POINT('Ctrl Pts',(-12.4271266840708,-57.7684249257696,
40.0429800745037));
#189309=CARTESIAN_POINT('Ctrl Pts',(-12.4294228751481,-57.7701960047921,
40.0409176249753));
#189310=CARTESIAN_POINT('Ctrl Pts',(-12.4316578001007,-57.772006704017,
40.0388310783332));
#189311=CARTESIAN_POINT('Ctrl Pts',(-12.4338307751865,-57.7738513586813,
40.036725739981));
#189312=CARTESIAN_POINT('Ctrl Pts',(-12.4416226773931,-57.7804659622463,
40.0291763710721));
#189313=CARTESIAN_POINT('Ctrl Pts',(-12.448679528741,-57.7875668075251,
40.0213310894602));
#189314=CARTESIAN_POINT('Ctrl Pts',(-12.455059618436,-57.7950386758929,
40.0132837551332));
#189315=CARTESIAN_POINT('Ctrl Pts',(-12.4620706960738,-57.8032495086132,
40.0044405431344));
#189316=CARTESIAN_POINT('Ctrl Pts',(-12.4682650727902,-57.8119087706193,
39.9953528710627));
#189317=CARTESIAN_POINT('Ctrl Pts',(-12.4736913816481,-57.8209080689657,
39.986110362959));
#189318=CARTESIAN_POINT('Ctrl Pts',(-12.4795504333966,-57.8306250526638,
39.9761307737604));
#189319=CARTESIAN_POINT('Ctrl Pts',(-12.4845147615706,-57.8407393717642,
39.9659696936073));
#189320=CARTESIAN_POINT('Ctrl Pts',(-12.4886033793256,-57.851153528676,
39.9557128217581));
#189321=CARTESIAN_POINT('Ctrl Pts',(-12.4926576977801,-57.8614803215156,
39.9455419945211));
#189322=CARTESIAN_POINT('Ctrl Pts',(-12.4958511892329,-57.8721033557526,
39.9352756289366));
#189323=CARTESIAN_POINT('Ctrl Pts',(-12.4981558292589,-57.8829458346105,
39.92499));
#189324=CARTESIAN_POINT('Origin',(0.0149069694351899,-0.0031685741680572,
39.92499));
#189325=CARTESIAN_POINT('Ctrl Pts',(-13.0516031943531,-61.4762657165315,
40.10025));
#189326=CARTESIAN_POINT('Ctrl Pts',(-13.0432012029365,-61.4780479426482,
40.10025));
#189327=CARTESIAN_POINT('Ctrl Pts',(-13.0347249977698,-61.4791124697294,
40.0995859581841));
#189328=CARTESIAN_POINT('Ctrl Pts',(-13.0263136082741,-61.4795178910588,
40.0983275959619));
#189329=CARTESIAN_POINT('Ctrl Pts',(-13.0209391308134,-61.479776935988,
40.0975235624067));
#189330=CARTESIAN_POINT('Ctrl Pts',(-13.0155911381655,-61.4797678285536,
40.096477705949));
#189331=CARTESIAN_POINT('Ctrl Pts',(-13.0103045333056,-61.4795143397208,
40.0952149915961));
#189332=CARTESIAN_POINT('Ctrl Pts',(-13.0030893784375,-61.4791683783269,
40.0934916398701));
#189333=CARTESIAN_POINT('Ctrl Pts',(-12.9959902125625,-61.4783613533298,
40.0913643921631));
#189334=CARTESIAN_POINT('Ctrl Pts',(-12.989088882123,-61.4771427864514,
40.0889118607713));
#189335=CARTESIAN_POINT('Ctrl Pts',(-12.9856382169033,-61.4765335030122,
40.0876855950754));
#189336=CARTESIAN_POINT('Ctrl Pts',(-12.9822368066734,-61.4758213793959,
40.0863782327526));
#189337=CARTESIAN_POINT('Ctrl Pts',(-12.9788934238966,-61.4750129240933,
40.0850006373334));
#189338=CARTESIAN_POINT('Ctrl Pts',(-12.9772217325082,-61.4746086964421,
40.0843118396237));
#189339=CARTESIAN_POINT('Ctrl Pts',(-12.9755645309605,-61.4741803895393,
40.0836054919164));
#189340=CARTESIAN_POINT('Ctrl Pts',(-12.9739228088657,-61.4737288401361,
40.0828829920418));
#189341=CARTESIAN_POINT('Ctrl Pts',(-12.973512378342,-61.4736159527853,
40.0827023670731));
#189342=CARTESIAN_POINT('Ctrl Pts',(-12.9731029149217,-61.4735016128574,
40.0825207326933));
#189343=CARTESIAN_POINT('Ctrl Pts',(-12.9726944333366,-61.473385833587,
40.0823381109275));
#189344=CARTESIAN_POINT('Ctrl Pts',(-12.9714689885814,-61.4730384957757,
40.0817902456303));
#189345=CARTESIAN_POINT('Ctrl Pts',(-12.9702523821507,-61.4726782034777,
40.0812334935553));
#189346=CARTESIAN_POINT('Ctrl Pts',(-12.9690449956483,-61.4723053176143,
40.0806684524227));
#189347=CARTESIAN_POINT('Ctrl Pts',(-12.9607012057876,-61.46972844494,40.0767636676138));
#189348=CARTESIAN_POINT('Ctrl Pts',(-12.9527534399845,-61.4665839586187,
40.0724404510891));
#189349=CARTESIAN_POINT('Ctrl Pts',(-12.9452156558843,-61.4629898265075,
40.0677949937414));
#189350=CARTESIAN_POINT('Ctrl Pts',(-12.9414693978769,-61.4612035527137,
40.0654862141909));
#189351=CARTESIAN_POINT('Ctrl Pts',(-12.937824249251,-61.459305623895,40.0630972003217));
#189352=CARTESIAN_POINT('Ctrl Pts',(-12.9342814732029,-61.4573073969127,
40.0606363359906));
#189353=CARTESIAN_POINT('Ctrl Pts',(-12.9264655800789,-61.4528990097271,
40.0552073017123));
#189354=CARTESIAN_POINT('Ctrl Pts',(-12.9191426809995,-61.4480137506082,
40.0494204304519));
#189355=CARTESIAN_POINT('Ctrl Pts',(-12.9123924986716,-61.4427731575667,
40.0434049749851));
#189356=CARTESIAN_POINT('Ctrl Pts',(-12.9099265719429,-61.4408587028413,
40.0412074532442));
#189357=CARTESIAN_POINT('Ctrl Pts',(-12.9075300815492,-61.4389006256226,
40.0389814735788));
#189358=CARTESIAN_POINT('Ctrl Pts',(-12.9052026993237,-61.4369042302169,
40.0367321210016));
#189359=CARTESIAN_POINT('Ctrl Pts',(-12.8973852687043,-61.4301985493013,
40.0291767837142));
#189360=CARTESIAN_POINT('Ctrl Pts',(-12.8903034584561,-61.4230116455107,
40.0213235332579));
#189361=CARTESIAN_POINT('Ctrl Pts',(-12.8838999218058,-61.4154582931182,
40.0132649215863));
#189362=CARTESIAN_POINT('Ctrl Pts',(-12.8768616764785,-61.4071562640854,
40.0044075527539));
#189363=CARTESIAN_POINT('Ctrl Pts',(-12.8706422708201,-61.3984111343316,
39.9953016253727));
#189364=CARTESIAN_POINT('Ctrl Pts',(-12.8651946651858,-61.3893309057294,
39.9860353422367));
#189365=CARTESIAN_POINT('Ctrl Pts',(-12.8593273605064,-61.379551110468,
39.9760551582706));
#189366=CARTESIAN_POINT('Ctrl Pts',(-12.8543546257415,-61.3693816498911,
39.9658879738169));
#189367=CARTESIAN_POINT('Ctrl Pts',(-12.85026023838,-61.3589193990694,39.955617464327));
#189368=CARTESIAN_POINT('Ctrl Pts',(-12.8462211390718,-61.3485984239575,
39.9454856413915));
#189369=CARTESIAN_POINT('Ctrl Pts',(-12.84303660345,-61.3379910943973,39.9352519465118));
#189370=CARTESIAN_POINT('Ctrl Pts',(-12.84073727331,-61.3271735965893,39.92499));
#189371=CARTESIAN_POINT('Ctrl Pts',(-12.1254815933794,-57.962160188812,
39.92499));
#189372=CARTESIAN_POINT('Ctrl Pts',(-12.1232811218133,-57.9518077840272,
39.9348107241733));
#189373=CARTESIAN_POINT('Ctrl Pts',(-12.1219050950916,-57.9413190436427,
39.944603838319));
#189374=CARTESIAN_POINT('Ctrl Pts',(-12.1213524729335,-57.9307520129756,
39.9543158069416));
#189375=CARTESIAN_POINT('Ctrl Pts',(-12.1208188676181,-57.9205486151387,
39.9636935671429));
#189376=CARTESIAN_POINT('Ctrl Pts',(-12.1210529843538,-57.9102709573144,
39.9729968321032));
#189377=CARTESIAN_POINT('Ctrl Pts',(-12.1220995054498,-57.899966680511,
39.9821731151384));
#189378=CARTESIAN_POINT('Ctrl Pts',(-12.1230887956356,-57.8902259118322,
39.9908475764405));
#189379=CARTESIAN_POINT('Ctrl Pts',(-12.1248041559929,-57.8804604570511,
39.9994093733903));
#189380=CARTESIAN_POINT('Ctrl Pts',(-12.1273238624924,-57.8707214089959,
40.0077966115901));
#189381=CARTESIAN_POINT('Ctrl Pts',(-12.1296444699072,-57.8617519091218,
40.0155211172656));
#189382=CARTESIAN_POINT('Ctrl Pts',(-12.1326475236753,-57.852804296004,
40.0230979941085));
#189383=CARTESIAN_POINT('Ctrl Pts',(-12.1364273448798,-57.8439372821223,
40.0304554104812));
#189384=CARTESIAN_POINT('Ctrl Pts',(-12.1375544112612,-57.8412933175777,
40.0326492435223));
#189385=CARTESIAN_POINT('Ctrl Pts',(-12.138750770895,-57.8386566819989,
40.0348233715081));
#189386=CARTESIAN_POINT('Ctrl Pts',(-12.1400195294492,-57.8360293953471,
40.0369753512356));
#189387=CARTESIAN_POINT('Ctrl Pts',(-12.1412753244188,-57.833428953088,
40.0391053430352));
#189388=CARTESIAN_POINT('Ctrl Pts',(-12.14260049657,-57.8308402488865,40.041211089324));
#189389=CARTESIAN_POINT('Ctrl Pts',(-12.143996334094,-57.8282680826381,
40.0432881154904));
#189390=CARTESIAN_POINT('Ctrl Pts',(-12.1440933979056,-57.8280892192275,
40.0434325478279));
#189391=CARTESIAN_POINT('Ctrl Pts',(-12.1441907966614,-57.8279104259145,
40.0435768364421));
#189392=CARTESIAN_POINT('Ctrl Pts',(-12.144288531381,-57.8277317035128,
40.0437209807855));
#189393=CARTESIAN_POINT('Ctrl Pts',(-12.1485735795159,-57.8198958587084,
40.0500407968421));
#189394=CARTESIAN_POINT('Ctrl Pts',(-12.1535378042503,-57.812226847525,
40.0560490279346));
#189395=CARTESIAN_POINT('Ctrl Pts',(-12.1592011408681,-57.804839125324,
40.0616647108617));
#189396=CARTESIAN_POINT('Ctrl Pts',(-12.1644803548773,-57.7979524842552,
40.066899503349));
#189397=CARTESIAN_POINT('Ctrl Pts',(-12.1703677426436,-57.7913098171238,
40.0717933267487));
#189398=CARTESIAN_POINT('Ctrl Pts',(-12.176888348138,-57.7850318067596,
40.0762460303079));
#189399=CARTESIAN_POINT('Ctrl Pts',(-12.179273669986,-57.7827352293487,
40.0778748868752));
#189400=CARTESIAN_POINT('Ctrl Pts',(-12.1817437717242,-57.7804877669872,
40.0794443522249));
#189401=CARTESIAN_POINT('Ctrl Pts',(-12.1842999559277,-57.7782965440188,
40.0809482021492));
#189402=CARTESIAN_POINT('Ctrl Pts',(-12.1849146328342,-57.7777696280971,
40.0813098278168));
#189403=CARTESIAN_POINT('Ctrl Pts',(-12.1855348686826,-57.7772459087254,
40.0816679525672));
#189404=CARTESIAN_POINT('Ctrl Pts',(-12.1861606108967,-57.7767255109847,
40.082022419258));
#189405=CARTESIAN_POINT('Ctrl Pts',(-12.1867667986667,-57.7762213756733,
40.0823658088648));
#189406=CARTESIAN_POINT('Ctrl Pts',(-12.1873781540071,-57.7757203576392,
40.0827057654616));
#189407=CARTESIAN_POINT('Ctrl Pts',(-12.187994625406,-57.7752225713657,
40.0830421470151));
#189408=CARTESIAN_POINT('Ctrl Pts',(-12.1947487820215,-57.7697687474616,
40.0867275956805));
#189409=CARTESIAN_POINT('Ctrl Pts',(-12.2021217510025,-57.764699586453,
40.0899823432029));
#189410=CARTESIAN_POINT('Ctrl Pts',(-12.2100174179588,-57.7601772489165,
40.0926299529354));
#189411=CARTESIAN_POINT('Ctrl Pts',(-12.2132919863905,-57.7583017007436,
40.0937279956083));
#189412=CARTESIAN_POINT('Ctrl Pts',(-12.2166560758248,-57.7565200187332,
40.0947220371802));
#189413=CARTESIAN_POINT('Ctrl Pts',(-12.2201014385647,-57.7548425830506,
40.0956014538692));
#189414=CARTESIAN_POINT('Ctrl Pts',(-12.2259778637495,-57.751981541693,
40.097101390674));
#189415=CARTESIAN_POINT('Ctrl Pts',(-12.2320899429716,-57.7494261286934,
40.0982667904316));
#189416=CARTESIAN_POINT('Ctrl Pts',(-12.2383911161013,-57.7472322823295,
40.0990539325582));
#189417=CARTESIAN_POINT('Ctrl Pts',(-12.2415417026662,-57.7461353591476,
40.0994475036216));
#189418=CARTESIAN_POINT('Ctrl Pts',(-12.2447399293287,-57.7451302272379,
40.0997467259952));
#189419=CARTESIAN_POINT('Ctrl Pts',(-12.2479799447119,-57.7442239366603,
40.0999473488896));
#189420=CARTESIAN_POINT('Ctrl Pts',(-12.2512199600952,-57.7433176460828,
40.100147971784));
#189421=CARTESIAN_POINT('Ctrl Pts',(-12.254501719267,-57.7425101887132,
40.10025));
#189422=CARTESIAN_POINT('Ctrl Pts',(-12.257819391977,-57.7418065394565,
40.10025));
#189423=CARTESIAN_POINT('Origin',(-18.0189898472952,-55.4074307335706,39.92499));
#189424=CARTESIAN_POINT('Ctrl Pts',(-19.5431821162869,-59.5312589135995,
39.92499));
#189425=CARTESIAN_POINT('Ctrl Pts',(-19.5464608884256,-59.5413499366329,
39.934835464202));
#189426=CARTESIAN_POINT('Ctrl Pts',(-19.5489337165496,-59.5516697238483,
39.9446440828461));
#189427=CARTESIAN_POINT('Ctrl Pts',(-19.550597385826,-59.5621592733656,
39.9543641760334));
#189428=CARTESIAN_POINT('Ctrl Pts',(-19.5522069957574,-59.5723079749847,
39.9637684240715));
#189429=CARTESIAN_POINT('Ctrl Pts',(-19.5530593117978,-59.5826168684398,
39.9730909636398));
#189430=CARTESIAN_POINT('Ctrl Pts',(-19.553106412799,-59.5930429125518,
39.9822808977141));
#189431=CARTESIAN_POINT('Ctrl Pts',(-19.5531509674458,-59.6029053082829,
39.9909740094649));
#189432=CARTESIAN_POINT('Ctrl Pts',(-19.5524750234012,-59.6128734577637,
39.9995492764999));
#189433=CARTESIAN_POINT('Ctrl Pts',(-19.5509963368659,-59.6229049605484,
40.0079462328691));
#189434=CARTESIAN_POINT('Ctrl Pts',(-19.5496343596255,-59.6321447001099,
40.0156804369684));
#189435=CARTESIAN_POINT('Ctrl Pts',(-19.5475912199423,-59.6414387315172,
40.0232638017415));
#189436=CARTESIAN_POINT('Ctrl Pts',(-19.5447674611716,-59.6507389334421,
40.0306257269958));
#189437=CARTESIAN_POINT('Ctrl Pts',(-19.5439483960912,-59.6534365684937,
40.0327611416646));
#189438=CARTESIAN_POINT('Ctrl Pts',(-19.5430634173961,-59.6561345922125,
40.0348777427268));
#189439=CARTESIAN_POINT('Ctrl Pts',(-19.542109499003,-59.658831468516,40.0369733168701));
#189440=CARTESIAN_POINT('Ctrl Pts',(-19.5410753901339,-59.6617550558218,
40.039245053974));
#189441=CARTESIAN_POINT('Ctrl Pts',(-19.5399627185792,-59.6646735866702,
40.041487875195));
#189442=CARTESIAN_POINT('Ctrl Pts',(-19.5387684320157,-59.6675844741794,
40.0436985701601));
#189443=CARTESIAN_POINT('Ctrl Pts',(-19.5354907031708,-59.6755734277898,
40.0497658398386));
#189444=CARTESIAN_POINT('Ctrl Pts',(-19.5315625649727,-59.6834782549089,
40.0555581699984));
#189445=CARTESIAN_POINT('Ctrl Pts',(-19.5269766895185,-59.6911955084648,
40.0609828468886));
#189446=CARTESIAN_POINT('Ctrl Pts',(-19.5227808624509,-59.698256376489,
40.0659461317305));
#189447=CARTESIAN_POINT('Ctrl Pts',(-19.518030548646,-59.7051493183932,
40.0706039980707));
#189448=CARTESIAN_POINT('Ctrl Pts',(-19.5126862934697,-59.7117949558637,
40.0748843180604));
#189449=CARTESIAN_POINT('Ctrl Pts',(-19.510061212785,-59.7150592712802,
40.076986797257));
#189450=CARTESIAN_POINT('Ctrl Pts',(-19.5072925729233,-59.7182634781247,
40.0789976708175));
#189451=CARTESIAN_POINT('Ctrl Pts',(-19.5043743927941,-59.7213950854345,
40.08090504915));
#189452=CARTESIAN_POINT('Ctrl Pts',(-19.5038206965381,-59.7219892774193,
40.0812669556105));
#189453=CARTESIAN_POINT('Ctrl Pts',(-19.5032610854118,-59.7225808838922,
40.0816253922033));
#189454=CARTESIAN_POINT('Ctrl Pts',(-19.5026955970361,-59.7231697699855,
40.0819801989139));
#189455=CARTESIAN_POINT('Ctrl Pts',(-19.5021477801721,-59.7237402533883,
40.0823239179149));
#189456=CARTESIAN_POINT('Ctrl Pts',(-19.5015944476715,-59.7243081837713,
40.0826642303498));
#189457=CARTESIAN_POINT('Ctrl Pts',(-19.5010356373988,-59.7248734373529,
40.0830009916099));
#189458=CARTESIAN_POINT('Ctrl Pts',(-19.4949458381922,-59.7310334544116,
40.0866709464312));
#189459=CARTESIAN_POINT('Ctrl Pts',(-19.4882011960853,-59.7368793392203,
40.0899175831878));
#189460=CARTESIAN_POINT('Ctrl Pts',(-19.4808775251051,-59.7422363728289,
40.0925642067062));
#189461=CARTESIAN_POINT('Ctrl Pts',(-19.4777846933724,-59.7444986813873,
40.0936818922528));
#189462=CARTESIAN_POINT('Ctrl Pts',(-19.474589008127,-59.7466739523114,
40.0946930094791));
#189463=CARTESIAN_POINT('Ctrl Pts',(-19.4712977780157,-59.748750122512,
40.0955863397546));
#189464=CARTESIAN_POINT('Ctrl Pts',(-19.465755428747,-59.752246341252,40.0970906856166));
#189465=CARTESIAN_POINT('Ctrl Pts',(-19.4599426670173,-59.7554590576861,
40.0982599215483));
#189466=CARTESIAN_POINT('Ctrl Pts',(-19.4538995640365,-59.7583258028883,
40.0990497370454));
#189467=CARTESIAN_POINT('Ctrl Pts',(-19.4523887882913,-59.7590424891888,
40.0992471909196));
#189468=CARTESIAN_POINT('Ctrl Pts',(-19.4508635299956,-59.7597373347838,
40.0994209989363));
#189469=CARTESIAN_POINT('Ctrl Pts',(-19.4493243130381,-59.760409072547,
40.0995705982975));
#189470=CARTESIAN_POINT('Ctrl Pts',(-19.4470154876019,-59.7614166791918,
40.0997949973393));
#189471=CARTESIAN_POINT('Ctrl Pts',(-19.4446752658776,-59.7623722755976,
40.0999649129781));
#189472=CARTESIAN_POINT('Ctrl Pts',(-19.4423059520263,-59.7632731754138,
40.1000786629733));
#189473=CARTESIAN_POINT('Ctrl Pts',(-19.439936638175,-59.7641740752301,
40.1001924129685));
#189474=CARTESIAN_POINT('Ctrl Pts',(-19.4375382417961,-59.765020284979,
40.10025));
#189475=CARTESIAN_POINT('Ctrl Pts',(-19.4351129318423,-59.765809437495,
40.10025));
#189476=CARTESIAN_POINT('Ctrl Pts',(-18.2553202812751,-56.1347810195641,
40.10025));
#189477=CARTESIAN_POINT('Ctrl Pts',(-18.263526710147,-56.1321105487811,
40.10025));
#189478=CARTESIAN_POINT('Ctrl Pts',(-18.2718824441042,-56.1301406315644,
40.0995786334241));
#189479=CARTESIAN_POINT('Ctrl Pts',(-18.2802419597926,-56.1288305556599,
40.0983063763368));
#189480=CARTESIAN_POINT('Ctrl Pts',(-18.285641349192,-56.1279843810471,
40.0974846287994));
#189481=CARTESIAN_POINT('Ctrl Pts',(-18.2910421817931,-56.1274125556282,
40.0964130309339));
#189482=CARTESIAN_POINT('Ctrl Pts',(-18.2964056883426,-56.1270952669252,
40.0951176960924));
#189483=CARTESIAN_POINT('Ctrl Pts',(-18.3035147090331,-56.1266747189247,
40.0934008039614));
#189484=CARTESIAN_POINT('Ctrl Pts',(-18.3105573165143,-56.126707076608,
40.0912909372157));
#189485=CARTESIAN_POINT('Ctrl Pts',(-18.3174512966901,-56.1271555587354,
40.0888630467852));
#189486=CARTESIAN_POINT('Ctrl Pts',(-18.320898286778,-56.1273797997991,
40.0876491015699));
#189487=CARTESIAN_POINT('Ctrl Pts',(-18.324308309033,-56.1277080087289,
40.0863558569272));
#189488=CARTESIAN_POINT('Ctrl Pts',(-18.3276724292421,-56.1281351437409,
40.0849936342772));
#189489=CARTESIAN_POINT('Ctrl Pts',(-18.3293544893467,-56.1283487112469,
40.0843125229521));
#189490=CARTESIAN_POINT('Ctrl Pts',(-18.3310250895515,-56.1285870051495,
40.0836141747075));
#189491=CARTESIAN_POINT('Ctrl Pts',(-18.3326832110572,-56.1288493629352,
40.082899916161));
#189492=CARTESIAN_POINT('Ctrl Pts',(-18.3330977414337,-56.1289149523816,
40.0827213515244));
#189493=CARTESIAN_POINT('Ctrl Pts',(-18.3335114922231,-56.1289820457108,
40.0825417925842));
#189494=CARTESIAN_POINT('Ctrl Pts',(-18.3339244481758,-56.1290506323488,
40.0823612602361));
#189495=CARTESIAN_POINT('Ctrl Pts',(-18.3351633160338,-56.1292563922627,
40.0818196631918));
#189496=CARTESIAN_POINT('Ctrl Pts',(-18.3363950287072,-56.1294755925118,
40.0812693052022));
#189497=CARTESIAN_POINT('Ctrl Pts',(-18.3376191892287,-56.1297079426452,
40.0807107531875));
#189498=CARTESIAN_POINT('Ctrl Pts',(-18.3462420178744,-56.1313445869828,
40.0767763849182));
#189499=CARTESIAN_POINT('Ctrl Pts',(-18.3545284904607,-56.1335959402408,
40.0724140586137));
#189500=CARTESIAN_POINT('Ctrl Pts',(-18.3624495731176,-56.136345925232,
40.0677221223768));
#189501=CARTESIAN_POINT('Ctrl Pts',(-18.3662912896465,-56.1376796649811,
40.065446538372));
#189502=CARTESIAN_POINT('Ctrl Pts',(-18.3700472768053,-56.1391312300711,
40.0630928000679));
#189503=CARTESIAN_POINT('Ctrl Pts',(-18.3737149835765,-56.1406901365233,
40.0606689262479));
#189504=CARTESIAN_POINT('Ctrl Pts',(-18.3793299863881,-56.1430767133841,
40.0569581447806));
#189505=CARTESIAN_POINT('Ctrl Pts',(-18.3847354115624,-56.1457125629778,
40.0530843804605));
#189506=CARTESIAN_POINT('Ctrl Pts',(-18.3899096889381,-56.1485569297209,
40.0490800251457));
#189507=CARTESIAN_POINT('Ctrl Pts',(-18.3923126501195,-56.1498778683512,
40.0472203818218));
#189508=CARTESIAN_POINT('Ctrl Pts',(-18.3946658026161,-56.1512435269776,
40.0453323608818));
#189509=CARTESIAN_POINT('Ctrl Pts',(-18.3969661720539,-56.1526507491369,
40.0434201572162));
#189510=CARTESIAN_POINT('Ctrl Pts',(-18.3971424863074,-56.1527586071707,
40.0432735943397));
#189511=CARTESIAN_POINT('Ctrl Pts',(-18.3973185179288,-56.1528666894394,
40.0431268995707));
#189512=CARTESIAN_POINT('Ctrl Pts',(-18.3974942667072,-56.1529749944978,
40.0429800745037));
#189513=CARTESIAN_POINT('Ctrl Pts',(-18.3999630071782,-56.1544963540395,
40.0409176249753));
#189514=CARTESIAN_POINT('Ctrl Pts',(-18.4023749585854,-56.1560635207937,
40.0388310783332));
#189515=CARTESIAN_POINT('Ctrl Pts',(-18.4047288488037,-56.1576709325003,
40.036725739981));
#189516=CARTESIAN_POINT('Ctrl Pts',(-18.413169480501,-56.1634348250117,
40.0291763710717));
#189517=CARTESIAN_POINT('Ctrl Pts',(-18.4209299141243,-56.1697591292906,
40.0213310894593));
#189518=CARTESIAN_POINT('Ctrl Pts',(-18.428056075939,-56.1765231650109,
40.0132837551317));
#189519=CARTESIAN_POINT('Ctrl Pts',(-18.4358870118869,-56.1839561607598,
40.0044405431321));
#189520=CARTESIAN_POINT('Ctrl Pts',(-18.4429525945105,-56.1919204977443,
39.9953528710596));
#189521=CARTESIAN_POINT('Ctrl Pts',(-18.4492898603077,-56.2003032932675,
39.986110362955));
#189522=CARTESIAN_POINT('Ctrl Pts',(-18.456132516932,-56.2093546086381,
39.9761307737549));
#189523=CARTESIAN_POINT('Ctrl Pts',(-18.4621268842299,-56.2188946068466,
39.9659696936003));
#189524=CARTESIAN_POINT('Ctrl Pts',(-18.4672816799275,-56.2288243369879,
39.9557128217496));
#189525=CARTESIAN_POINT('Ctrl Pts',(-18.4723932321854,-56.2386707668957,
39.9455419945154));
#189526=CARTESIAN_POINT('Ctrl Pts',(-18.4766796388004,-56.2489017962828,
39.9352756289337));
#189527=CARTESIAN_POINT('Ctrl Pts',(-18.4801050014193,-56.2594439784238,
39.92499));
#189528=CARTESIAN_POINT('Origin',(0.0144941013083455,-0.00470941899426891,
39.92499));
#189529=CARTESIAN_POINT('Ctrl Pts',(-19.4061247292256,-59.7752282754836,
40.10025));
#189530=CARTESIAN_POINT('Ctrl Pts',(-19.3979550581547,-59.7778789856301,
40.10025));
#189531=CARTESIAN_POINT('Ctrl Pts',(-19.3896365599073,-59.7798236858209,
40.0995859581842));
#189532=CARTESIAN_POINT('Ctrl Pts',(-19.3813136269524,-59.7811061158278,
40.0983275959622));
#189533=CARTESIAN_POINT('Ctrl Pts',(-19.3759956690093,-59.7819255275518,
40.0975235624069));
#189534=CARTESIAN_POINT('Ctrl Pts',(-19.3706760212382,-59.782475487462,
40.0964777059491));
#189535=CARTESIAN_POINT('Ctrl Pts',(-19.3653918801542,-59.7827759879494,
40.0952149915962));
#189536=CARTESIAN_POINT('Ctrl Pts',(-19.3581800878465,-59.7831861108189,
40.0934916398702));
#189537=CARTESIAN_POINT('Ctrl Pts',(-19.3510354548622,-59.7831255716886,
40.0913643921631));
#189538=CARTESIAN_POINT('Ctrl Pts',(-19.3440445557098,-59.7826350657123,
40.0889118607714));
#189539=CARTESIAN_POINT('Ctrl Pts',(-19.3405491061336,-59.7823898127242,
40.0876855950755));
#189540=CARTESIAN_POINT('Ctrl Pts',(-19.3370918919976,-59.7820371343798,
40.0863782327527));
#189541=CARTESIAN_POINT('Ctrl Pts',(-19.3336823180311,-59.7815825865438,
40.0850006373335));
#189542=CARTESIAN_POINT('Ctrl Pts',(-19.3319775310479,-59.7813553126258,
40.0843118396238));
#189543=CARTESIAN_POINT('Ctrl Pts',(-19.3302846375612,-59.7811025767642,
40.0836054919165));
#189544=CARTESIAN_POINT('Ctrl Pts',(-19.3286047092266,-59.7808251076836,
40.0828829920418));
#189545=CARTESIAN_POINT('Ctrl Pts',(-19.328184727143,-59.7807557404134,
40.0827023670732));
#189546=CARTESIAN_POINT('Ctrl Pts',(-19.3277655550292,-59.7806848274337,
40.0825207326934));
#189547=CARTESIAN_POINT('Ctrl Pts',(-19.3273472089197,-59.7806123803666,
40.0823381109276));
#189548=CARTESIAN_POINT('Ctrl Pts',(-19.3260921705914,-59.7803950391652,
40.0817902456304));
#189549=CARTESIAN_POINT('Ctrl Pts',(-19.3248445680579,-59.7801638905867,
40.0812334935554));
#189550=CARTESIAN_POINT('Ctrl Pts',(-19.3236048185588,-59.7799192536868,
40.0806684524228));
#189551=CARTESIAN_POINT('Ctrl Pts',(-19.3150373803109,-59.7782286609225,
40.0767636676137));
#189552=CARTESIAN_POINT('Ctrl Pts',(-19.306804464877,-59.775932168172,40.0724404510887));
#189553=CARTESIAN_POINT('Ctrl Pts',(-19.2989322844401,-59.7731456380807,
40.0677949937407));
#189554=CARTESIAN_POINT('Ctrl Pts',(-19.2950198323719,-59.7717607402743,
40.0654862141904));
#189555=CARTESIAN_POINT('Ctrl Pts',(-19.2911962646691,-59.7702542302927,
40.0630972003216));
#189556=CARTESIAN_POINT('Ctrl Pts',(-19.2874640247236,-59.768637270743,
40.0606363359906));
#189557=CARTESIAN_POINT('Ctrl Pts',(-19.2792301459419,-59.765070016461,
40.0552073017124));
#189558=CARTESIAN_POINT('Ctrl Pts',(-19.2714367138416,-59.7609769706901,
40.0494204304519));
#189559=CARTESIAN_POINT('Ctrl Pts',(-19.2641757185814,-59.7564706723512,
40.0434049749851));
#189560=CARTESIAN_POINT('Ctrl Pts',(-19.2615231854469,-59.7548244647406,
40.0412074532442));
#189561=CARTESIAN_POINT('Ctrl Pts',(-19.2589351484757,-59.7531276155318,
40.0389814735788));
#189562=CARTESIAN_POINT('Ctrl Pts',(-19.2564118357498,-59.7513854342765,
40.0367321210017));
#189563=CARTESIAN_POINT('Ctrl Pts',(-19.2479362953114,-59.7455336317915,
40.0291767837137));
#189564=CARTESIAN_POINT('Ctrl Pts',(-19.2401420439511,-59.7391263493538,
40.0213235332567));
#189565=CARTESIAN_POINT('Ctrl Pts',(-19.2329840462261,-59.7322837268608,
40.0132649215845));
#189566=CARTESIAN_POINT('Ctrl Pts',(-19.2251165588057,-59.7247628741792,
40.0044075527515));
#189567=CARTESIAN_POINT('Ctrl Pts',(-19.2180171087277,-59.7167157560764,
39.9953016253696));
#189568=CARTESIAN_POINT('Ctrl Pts',(-19.2116502033049,-59.7082546997612,
39.986035342233));
#189569=CARTESIAN_POINT('Ctrl Pts',(-19.2047927733642,-59.6991417795822,
39.976055158266));
#189570=CARTESIAN_POINT('Ctrl Pts',(-19.1987842816741,-59.6895478206965,
39.9658879738114));
#189571=CARTESIAN_POINT('Ctrl Pts',(-19.1936187207943,-59.6795708631975,
39.9556174643205));
#189572=CARTESIAN_POINT('Ctrl Pts',(-19.1885229124283,-59.6697286283129,
39.9454856413872));
#189573=CARTESIAN_POINT('Ctrl Pts',(-19.1842470541687,-59.6595122814308,
39.9352519465097));
#189574=CARTESIAN_POINT('Ctrl Pts',(-19.1808295835784,-59.6489943884563,
39.92499));
#189575=CARTESIAN_POINT('Ctrl Pts',(-18.1177524687109,-56.3771794532806,
39.92499));
#189576=CARTESIAN_POINT('Ctrl Pts',(-18.1144819305953,-56.3671137719645,
39.9348107241725));
#189577=CARTESIAN_POINT('Ctrl Pts',(-18.112017069978,-56.3568263239568,
39.9446038383174));
#189578=CARTESIAN_POINT('Ctrl Pts',(-18.1103629196651,-56.3463749453352,
39.9543158069392));
#189579=CARTESIAN_POINT('Ctrl Pts',(-18.1087656919994,-56.3362832197235,
39.9636935671399));
#189580=CARTESIAN_POINT('Ctrl Pts',(-18.1079242184407,-56.3260373921222,
39.9729968320996));
#189581=CARTESIAN_POINT('Ctrl Pts',(-18.107887916365,-56.315680171984,39.9821731151343));
#189582=CARTESIAN_POINT('Ctrl Pts',(-18.1078535995344,-56.305889355273,
39.9908475764359));
#189583=CARTESIAN_POINT('Ctrl Pts',(-18.1085387949865,-56.2959980926935,
39.9994093733852));
#189584=CARTESIAN_POINT('Ctrl Pts',(-18.1100266905428,-56.2860490151148,
40.0077966115846));
#189585=CARTESIAN_POINT('Ctrl Pts',(-18.1113970173888,-56.2768860815733,
40.0155211172598));
#189586=CARTESIAN_POINT('Ctrl Pts',(-18.1134483398646,-56.2676735798215,
40.0230979941022));
#189587=CARTESIAN_POINT('Ctrl Pts',(-18.1162805994775,-56.2584600414683,
40.0304554104747));
#189588=CARTESIAN_POINT('Ctrl Pts',(-18.1171251221212,-56.2557127503185,
40.032649243518));
#189589=CARTESIAN_POINT('Ctrl Pts',(-18.1180393245073,-56.2529655048685,
40.034823371506));
#189590=CARTESIAN_POINT('Ctrl Pts',(-18.1190265064342,-56.2502199893831,
40.0369753512356));
#189591=CARTESIAN_POINT('Ctrl Pts',(-18.1200036017944,-56.2475025263005,
40.0391053430352));
#189592=CARTESIAN_POINT('Ctrl Pts',(-18.1210509212418,-56.2447894850829,
40.041211089324));
#189593=CARTESIAN_POINT('Ctrl Pts',(-18.1221702476366,-56.242085504679,
40.0432881154904));
#189594=CARTESIAN_POINT('Ctrl Pts',(-18.1222480834051,-56.2418974751698,
40.043432547828));
#189595=CARTESIAN_POINT('Ctrl Pts',(-18.12232625961,-56.241709480363,40.0435768364421));
#189596=CARTESIAN_POINT('Ctrl Pts',(-18.1224047773506,-56.2415215209613,
40.0437209807855));
#189597=CARTESIAN_POINT('Ctrl Pts',(-18.1258472827276,-56.2332806922381,
40.050040796842));
#189598=CARTESIAN_POINT('Ctrl Pts',(-18.1299826829657,-56.2251347899177,
40.0560490279345));
#189599=CARTESIAN_POINT('Ctrl Pts',(-18.1348427679841,-56.2171955585584,
40.0616647108615));
#189600=CARTESIAN_POINT('Ctrl Pts',(-18.1393732118983,-56.2097948151026,
40.0668995033485));
#189601=CARTESIAN_POINT('Ctrl Pts',(-18.1445340001509,-56.2025731376012,
40.0717933267481));
#189602=CARTESIAN_POINT('Ctrl Pts',(-18.15036265431,-56.1956479299631,40.0762460303071));
#189603=CARTESIAN_POINT('Ctrl Pts',(-18.1524948514082,-56.193114599416,
40.0778748868747));
#189604=CARTESIAN_POINT('Ctrl Pts',(-18.1547164978841,-56.1906212529492,
40.0794443522247));
#189605=CARTESIAN_POINT('Ctrl Pts',(-18.1570296338739,-56.1881748397224,
40.0809482021492));
#189606=CARTESIAN_POINT('Ctrl Pts',(-18.1575858658044,-56.1875865590688,
40.0813098278168));
#189607=CARTESIAN_POINT('Ctrl Pts',(-18.1581479603548,-56.1870008763867,
40.0816679525672));
#189608=CARTESIAN_POINT('Ctrl Pts',(-18.1587158783115,-56.1864179215671,
40.082022419258));
#189609=CARTESIAN_POINT('Ctrl Pts',(-18.159266048832,-56.1858531840857,
40.0823658088648));
#189610=CARTESIAN_POINT('Ctrl Pts',(-18.1598216844587,-56.1852910066465,
40.0827057654616));
#189611=CARTESIAN_POINT('Ctrl Pts',(-18.1603827459286,-56.1847315084904,
40.0830421470151));
#189612=CARTESIAN_POINT('Ctrl Pts',(-18.166529822736,-56.1786015595924,
40.0867275956806));
#189613=CARTESIAN_POINT('Ctrl Pts',(-18.1733325302114,-56.1727894828607,
40.0899823432031));
#189614=CARTESIAN_POINT('Ctrl Pts',(-18.1807122308852,-56.1674665972289,
40.0926299529356));
#189615=CARTESIAN_POINT('Ctrl Pts',(-18.1837728127199,-56.1652590378992,
40.0937279956085));
#189616=CARTESIAN_POINT('Ctrl Pts',(-18.1869322368375,-56.1631354730306,
40.0947220371803));
#189617=CARTESIAN_POINT('Ctrl Pts',(-18.1901833857455,-56.1611070880438,
40.0956014538692));
#189618=CARTESIAN_POINT('Ctrl Pts',(-18.1957285590018,-56.157647466076,
40.097101390674));
#189619=CARTESIAN_POINT('Ctrl Pts',(-18.2015400422205,-56.1544671656477,
40.0982667904316));
#189620=CARTESIAN_POINT('Ctrl Pts',(-18.2075773774753,-56.1516266854593,
40.0990539325582));
#189621=CARTESIAN_POINT('Ctrl Pts',(-18.2105960451028,-56.1502064453651,
40.0994475036216));
#189622=CARTESIAN_POINT('Ctrl Pts',(-18.2136716866511,-56.1488725139551,
40.0997467259952));
#189623=CARTESIAN_POINT('Ctrl Pts',(-18.2167992197297,-56.1476325143033,
40.0999473488896));
#189624=CARTESIAN_POINT('Ctrl Pts',(-18.2199267528084,-56.1463925146515,
40.100147971784));
#189625=CARTESIAN_POINT('Ctrl Pts',(-18.2231061318822,-56.1452464433751,
40.10025));
#189626=CARTESIAN_POINT('Ctrl Pts',(-18.2263320786585,-56.1441998575527,
40.10025));
#189627=CARTESIAN_POINT('Origin',(-23.7119335237428,-53.2204057122637,39.92499));
#189628=CARTESIAN_POINT('Ctrl Pts',(-25.6588335304443,-57.162321654437,
39.92499));
#189629=CARTESIAN_POINT('Ctrl Pts',(-25.6631491402569,-57.1720146727778,
39.9348354642018));
#189630=CARTESIAN_POINT('Ctrl Pts',(-25.6666871334687,-57.1820194461957,
39.9446440828459));
#189631=CARTESIAN_POINT('Ctrl Pts',(-25.6694381454821,-57.1922776320705,
39.9543641760333));
#189632=CARTESIAN_POINT('Ctrl Pts',(-25.6720997659863,-57.2022024879878,
39.9637684240715));
#189633=CARTESIAN_POINT('Ctrl Pts',(-25.6740249857412,-57.2123658169602,
39.97309096364));
#189634=CARTESIAN_POINT('Ctrl Pts',(-25.6751616470871,-57.2227298227164,
39.9822808977145));
#189635=CARTESIAN_POINT('Ctrl Pts',(-25.6762368587287,-57.2325335339832,
39.9909740094656));
#189636=CARTESIAN_POINT('Ctrl Pts',(-25.676606572923,-57.2425177322905,
39.9995492765009));
#189637=CARTESIAN_POINT('Ctrl Pts',(-25.6761845643574,-57.2526488462847,
40.0079462328703));
#189638=CARTESIAN_POINT('Ctrl Pts',(-25.6757958639481,-57.2619803349743,
40.01568043697));
#189639=CARTESIAN_POINT('Ctrl Pts',(-25.6747354076183,-57.2714370189567,
40.0232638017433));
#189640=CARTESIAN_POINT('Ctrl Pts',(-25.6728992535086,-57.2809814365677,
40.0306257269979));
#189641=CARTESIAN_POINT('Ctrl Pts',(-25.672366654999,-57.2837499093055,
40.032761141666));
#189642=CARTESIAN_POINT('Ctrl Pts',(-25.6717685445831,-57.2865256584302,
40.0348777427275));
#189643=CARTESIAN_POINT('Ctrl Pts',(-25.6711017521907,-57.2893074725859,
40.0369733168701));
#189644=CARTESIAN_POINT('Ctrl Pts',(-25.6703789063664,-57.2923231379855,
40.039245053974));
#189645=CARTESIAN_POINT('Ctrl Pts',(-25.6695773996876,-57.2953419866642,
40.041487875195));
#189646=CARTESIAN_POINT('Ctrl Pts',(-25.6686939261489,-57.2983617649663,
40.0436985701601));
#189647=CARTESIAN_POINT('Ctrl Pts',(-25.6662692260896,-57.3066495702122,
40.0497658398386));
#189648=CARTESIAN_POINT('Ctrl Pts',(-25.6631888860747,-57.3149216961105,
40.0555581699984));
#189649=CARTESIAN_POINT('Ctrl Pts',(-25.6594348051809,-57.3230760282579,
40.0609828468886));
#189650=CARTESIAN_POINT('Ctrl Pts',(-25.656000024977,-57.3305367994636,
40.0659461317303));
#189651=CARTESIAN_POINT('Ctrl Pts',(-25.651996242513,-57.3378885241126,
40.0706039980704));
#189652=CARTESIAN_POINT('Ctrl Pts',(-25.6473759219982,-57.3450563828663,
40.07488431806));
#189653=CARTESIAN_POINT('Ctrl Pts',(-25.645106435654,-57.3485772116716,
40.0769867972568));
#189654=CARTESIAN_POINT('Ctrl Pts',(-25.6426878935085,-57.352053267206,
40.0789976708174));
#189655=CARTESIAN_POINT('Ctrl Pts',(-25.6401130415749,-57.355472752128,
40.08090504915));
#189656=CARTESIAN_POINT('Ctrl Pts',(-25.6396244884999,-57.3561215660857,
40.0812669556105));
#189657=CARTESIAN_POINT('Ctrl Pts',(-25.6391297826974,-57.3567684269676,
40.0816253922032));
#189658=CARTESIAN_POINT('Ctrl Pts',(-25.6386289474846,-57.3574131967121,
40.0819801989139));
#189659=CARTESIAN_POINT('Ctrl Pts',(-25.6381437633721,-57.3580378174021,
40.0823239179149));
#189660=CARTESIAN_POINT('Ctrl Pts',(-25.637652826975,-57.358660475599,40.0826642303498));
#189661=CARTESIAN_POINT('Ctrl Pts',(-25.6371561630117,-57.3592810442414,
40.0830009916099));
#189662=CARTESIAN_POINT('Ctrl Pts',(-25.6317436214791,-57.3660438734349,
40.0866709464313));
#189663=CARTESIAN_POINT('Ctrl Pts',(-25.6256469885827,-57.3725627409497,
40.0899175831879));
#189664=CARTESIAN_POINT('Ctrl Pts',(-25.6189233999291,-57.3786559602408,
40.0925642067064));
#189665=CARTESIAN_POINT('Ctrl Pts',(-25.6160839866894,-57.3812291645843,
40.0936818922529));
#189666=CARTESIAN_POINT('Ctrl Pts',(-25.6131331854691,-57.3837265592144,
40.0946930094791));
#189667=CARTESIAN_POINT('Ctrl Pts',(-25.6100770039414,-57.3861353831631,
40.0955863397546));
#189668=CARTESIAN_POINT('Ctrl Pts',(-25.6049304706141,-57.3901917825029,
40.0970906856166));
#189669=CARTESIAN_POINT('Ctrl Pts',(-25.5994853721131,-57.3939944983913,
40.0982599215483));
#189670=CARTESIAN_POINT('Ctrl Pts',(-25.5937750303535,-57.3974772155317,
40.0990497370454));
#189671=CARTESIAN_POINT('Ctrl Pts',(-25.5923474449136,-57.3983478948168,
40.0992471909196));
#189672=CARTESIAN_POINT('Ctrl Pts',(-25.5909031732847,-57.3991983668806,
40.0994209989363));
#189673=CARTESIAN_POINT('Ctrl Pts',(-25.5894426040348,-57.4000273167772,
40.0995705982975));
#189674=CARTESIAN_POINT('Ctrl Pts',(-25.58725175016,-57.4012707416221,40.0997949973393));
#189675=CARTESIAN_POINT('Ctrl Pts',(-25.585024235439,-57.4024657229512,
40.0999649129781));
#189676=CARTESIAN_POINT('Ctrl Pts',(-25.5827620706102,-57.4036093482798,
40.1000786629733));
#189677=CARTESIAN_POINT('Ctrl Pts',(-25.5804999057814,-57.4047529736084,
40.1001924129685));
#189678=CARTESIAN_POINT('Ctrl Pts',(-25.578203101074,-57.4058452484211,
40.10025));
#189679=CARTESIAN_POINT('Ctrl Pts',(-25.5758735661218,-57.4068835917994,
40.10025));
#189680=CARTESIAN_POINT('Ctrl Pts',(-24.0229981225299,-53.9190682401994,
40.10025));
#189681=CARTESIAN_POINT('Ctrl Pts',(-24.0308804555189,-53.9155545931357,
40.10025));
#189682=CARTESIAN_POINT('Ctrl Pts',(-24.0389845034721,-53.9127220553015,
40.0995786334241));
#189683=CARTESIAN_POINT('Ctrl Pts',(-24.0471612846382,-53.9105453488013,
40.0983063763366));
#189684=CARTESIAN_POINT('Ctrl Pts',(-24.0524426462853,-53.9091394197452,
40.0974846287992));
#189685=CARTESIAN_POINT('Ctrl Pts',(-24.0577541205276,-53.9080061861137,
40.0964130309338));
#189686=CARTESIAN_POINT('Ctrl Pts',(-24.0630550795263,-53.9071299964541,
40.0951176960924));
#189687=CARTESIAN_POINT('Ctrl Pts',(-24.0700811970213,-53.9059686572514,
40.0934008039614));
#189688=CARTESIAN_POINT('Ctrl Pts',(-24.0770886066608,-53.9052646847385,
40.0912909372156));
#189689=CARTESIAN_POINT('Ctrl Pts',(-24.0839917000394,-53.9049900928804,
40.0888630467851));
#189690=CARTESIAN_POINT('Ctrl Pts',(-24.0874432467287,-53.9048527969513,
40.0876491015699));
#189691=CARTESIAN_POINT('Ctrl Pts',(-24.0908688957001,-53.9048227635322,
40.0863558569271));
#189692=CARTESIAN_POINT('Ctrl Pts',(-24.0942592346731,-53.9048959123382,
40.0849936342771));
#189693=CARTESIAN_POINT('Ctrl Pts',(-24.0959544041596,-53.9049324867412,
40.0843125229521));
#189694=CARTESIAN_POINT('Ctrl Pts',(-24.0976407611372,-53.9049948499727,
40.0836141747074));
#189695=CARTESIAN_POINT('Ctrl Pts',(-24.099317223136,-53.9050824496421,
40.0828999161609));
#189696=CARTESIAN_POINT('Ctrl Pts',(-24.0997363386357,-53.9051043495594,
40.0827213515243));
#189697=CARTESIAN_POINT('Ctrl Pts',(-24.1001548360176,-53.9051278266101,
40.0825417925842));
#189698=CARTESIAN_POINT('Ctrl Pts',(-24.1005726990102,-53.9051528718722,
40.082361260236));
#189699=CARTESIAN_POINT('Ctrl Pts',(-24.1018262879881,-53.9052280076584,
40.0818196631917));
#189700=CARTESIAN_POINT('Ctrl Pts',(-24.1030741658758,-53.9053172580726,
40.0812693052021));
#189701=CARTESIAN_POINT('Ctrl Pts',(-24.1043159075202,-53.9054203757496,
40.0807107531875));
#189702=CARTESIAN_POINT('Ctrl Pts',(-24.1130625753257,-53.9061467233509,
40.0767763849182));
#189703=CARTESIAN_POINT('Ctrl Pts',(-24.1215389842443,-53.9075195712148,
40.0724140586139));
#189704=CARTESIAN_POINT('Ctrl Pts',(-24.1297041260866,-53.9094265129029,
40.067722122377));
#189705=CARTESIAN_POINT('Ctrl Pts',(-24.133664211057,-53.9103513775611,
40.0654465383722));
#189706=CARTESIAN_POINT('Ctrl Pts',(-24.1375513523935,-53.9114023832599,
40.063092800068));
#189707=CARTESIAN_POINT('Ctrl Pts',(-24.1413619171793,-53.912569370107,
40.0606689262479));
#189708=CARTESIAN_POINT('Ctrl Pts',(-24.1471956256297,-53.9143559454349,
40.0569581447806));
#189709=CARTESIAN_POINT('Ctrl Pts',(-24.1528469606267,-53.9164123347819,
40.0530843804605));
#189710=CARTESIAN_POINT('Ctrl Pts',(-24.1582902100542,-53.9187002605238,
40.0490800251458));
#189711=CARTESIAN_POINT('Ctrl Pts',(-24.1608180832479,-53.9197627850744,
40.0472203818218));
#189712=CARTESIAN_POINT('Ctrl Pts',(-24.1633010951265,-53.9208749910657,
40.0453323608818));
#189713=CARTESIAN_POINT('Ctrl Pts',(-24.1657359576696,-53.9220340502326,
40.0434201572162));
#189714=CARTESIAN_POINT('Ctrl Pts',(-24.1659225802897,-53.9221228875508,
40.0432735943397));
#189715=CARTESIAN_POINT('Ctrl Pts',(-24.1661089452649,-53.9222119774186,
40.0431268995707));
#189716=CARTESIAN_POINT('Ctrl Pts',(-24.1662950522344,-53.9223013184209,
40.0429800745037));
#189717=CARTESIAN_POINT('Ctrl Pts',(-24.1689092940617,-53.9235562901481,
40.0409176249753));
#189718=CARTESIAN_POINT('Ctrl Pts',(-24.1714718460793,-53.9248627542249,
40.0388310783332));
#189719=CARTESIAN_POINT('Ctrl Pts',(-24.1739808617162,-53.9262153118347,
40.036725739981));
#189720=CARTESIAN_POINT('Ctrl Pts',(-24.1829777455758,-53.9310653428791,
40.0291763710723));
#189721=CARTESIAN_POINT('Ctrl Pts',(-24.1913567365385,-53.936543815756,
40.0213310894606));
#189722=CARTESIAN_POINT('Ctrl Pts',(-24.199150894752,-53.9425259106368,
40.0132837551337));
#189723=CARTESIAN_POINT('Ctrl Pts',(-24.2077158916356,-53.9490996319559,
40.0044405431351));
#189724=CARTESIAN_POINT('Ctrl Pts',(-24.2155752681635,-53.9562817849744,
39.9953528710637));
#189725=CARTESIAN_POINT('Ctrl Pts',(-24.222754058489,-53.9639562340105,
39.9861103629602));
#189726=CARTESIAN_POINT('Ctrl Pts',(-24.2305053504095,-53.9722427129451,
39.9761307737619));
#189727=CARTESIAN_POINT('Ctrl Pts',(-24.2374640812876,-53.9811038680413,
39.9659696936093));
#189728=CARTESIAN_POINT('Ctrl Pts',(-24.2436285779068,-53.9904403792073,
39.9557128217605));
#189729=CARTESIAN_POINT('Ctrl Pts',(-24.2497413607364,-53.9996985666423,
39.9455419945227));
#189730=CARTESIAN_POINT('Ctrl Pts',(-24.2550737197492,-54.0094254978869,
39.9352756289374));
#189731=CARTESIAN_POINT('Ctrl Pts',(-24.2595822759735,-54.019551880964,
39.92499));
#189732=CARTESIAN_POINT('Origin',(0.0139224327744811,-0.00619866644047012,
39.92499));
#189733=CARTESIAN_POINT('Ctrl Pts',(-25.5480287005721,-57.4192809246788,
40.10025));
#189734=CARTESIAN_POINT('Ctrl Pts',(-25.5401808584716,-57.4227710771205,
40.10025));
#189735=CARTESIAN_POINT('Ctrl Pts',(-25.5321112063496,-57.4255746438789,
40.0995859581841));
#189736=CARTESIAN_POINT('Ctrl Pts',(-25.5239679177294,-57.4277200319917,
40.0983275959618));
#189737=CARTESIAN_POINT('Ctrl Pts',(-25.5187647439654,-57.4290908328638,
40.0975235624066));
#189738=CARTESIAN_POINT('Ctrl Pts',(-25.5135317242463,-57.4301938346426,
40.0964777059489));
#189739=CARTESIAN_POINT('Ctrl Pts',(-25.5083079410949,-57.431045032104,
40.0952149915961));
#189740=CARTESIAN_POINT('Ctrl Pts',(-25.5011785252534,-57.4322067458447,
40.0934916398701));
#189741=CARTESIAN_POINT('Ctrl Pts',(-25.4940667032539,-57.4328933558606,
40.091364392163));
#189742=CARTESIAN_POINT('Ctrl Pts',(-25.4870628291426,-57.4331362848727,
40.0889118607713));
#189743=CARTESIAN_POINT('Ctrl Pts',(-25.483560892087,-57.4332577493787,
40.0876855950754));
#189744=CARTESIAN_POINT('Ctrl Pts',(-25.4800857520064,-57.433268380324,
40.0863782327527));
#189745=CARTESIAN_POINT('Ctrl Pts',(-25.4766473428561,-57.4331727200757,
40.0850006373334));
#189746=CARTESIAN_POINT('Ctrl Pts',(-25.4749281382809,-57.4331248899516,
40.0843118396238));
#189747=CARTESIAN_POINT('Ctrl Pts',(-25.4732181005507,-57.4330504941581,
40.0836054919165));
#189748=CARTESIAN_POINT('Ctrl Pts',(-25.4715183716227,-57.4329501454093,
40.0828829920418));
#189749=CARTESIAN_POINT('Ctrl Pts',(-25.4710934393907,-57.4329250582221,
40.0827023670731));
#189750=CARTESIAN_POINT('Ctrl Pts',(-25.4706691511208,-57.4328983491281,
40.0825207326933));
#189751=CARTESIAN_POINT('Ctrl Pts',(-25.4702455239745,-57.4328700280095,
40.0823381109276));
#189752=CARTESIAN_POINT('Ctrl Pts',(-25.4689746425358,-57.4327850646537,
40.0817902456304));
#189753=CARTESIAN_POINT('Ctrl Pts',(-25.4677097128937,-57.432685592307,
40.0812334935553));
#189754=CARTESIAN_POINT('Ctrl Pts',(-25.4664511833529,-57.4325718846636,
40.0806684524227));
#189755=CARTESIAN_POINT('Ctrl Pts',(-25.4577539633643,-57.4317860942975,
40.0767636676136));
#189756=CARTESIAN_POINT('Ctrl Pts',(-25.4493260998444,-57.430362755973,
40.0724404510885));
#189757=CARTESIAN_POINT('Ctrl Pts',(-25.4412057723272,-57.4284143577087,
40.0677949937404));
#189758=CARTESIAN_POINT('Ctrl Pts',(-25.4371699918414,-57.4274460091197,
40.0654862141902));
#189759=CARTESIAN_POINT('Ctrl Pts',(-25.4332098968694,-57.4263474236137,
40.0630972003214));
#189760=CARTESIAN_POINT('Ctrl Pts',(-25.4293290842281,-57.4251294472436,
40.0606363359906));
#189761=CARTESIAN_POINT('Ctrl Pts',(-25.4207674318877,-57.4224424094496,
40.0552073017123));
#189762=CARTESIAN_POINT('Ctrl Pts',(-25.4125888532393,-57.4191864212928,
40.0494204304519));
#189763=CARTESIAN_POINT('Ctrl Pts',(-25.4048965980306,-57.415463789604,
40.0434049749851));
#189764=CARTESIAN_POINT('Ctrl Pts',(-25.4020865201984,-57.4141038653032,
40.0412074532442));
#189765=CARTESIAN_POINT('Ctrl Pts',(-25.3993352917243,-57.4126868351394,
40.0389814735788));
#189766=CARTESIAN_POINT('Ctrl Pts',(-25.3966436944401,-57.411217955737,
40.0367321210016));
#189767=CARTESIAN_POINT('Ctrl Pts',(-25.3876029039784,-57.4062841452559,
40.029176783714));
#189768=CARTESIAN_POINT('Ctrl Pts',(-25.3791816069561,-57.400726683699,
40.0213235332575));
#189769=CARTESIAN_POINT('Ctrl Pts',(-25.3713475726781,-57.3946697603108,
40.0132649215857));
#189770=CARTESIAN_POINT('Ctrl Pts',(-25.3627370410041,-57.3880124840173,
40.0044075527531));
#189771=CARTESIAN_POINT('Ctrl Pts',(-25.3548353295677,-57.3807515434767,
39.9953016253717));
#189772=CARTESIAN_POINT('Ctrl Pts',(-25.347618881505,-57.3730023605534,
39.9860353422355));
#189773=CARTESIAN_POINT('Ctrl Pts',(-25.3398464577412,-57.3646561585189,
39.9760551582691));
#189774=CARTESIAN_POINT('Ctrl Pts',(-25.3328680394184,-57.3557428147474,
39.9658879738151));
#189775=CARTESIAN_POINT('Ctrl Pts',(-25.3266878999862,-57.3463604602068,
39.9556174643249));
#189776=CARTESIAN_POINT('Ctrl Pts',(-25.3205912133029,-57.337104799131,
39.9454856413901));
#189777=CARTESIAN_POINT('Ctrl Pts',(-25.3152708796015,-57.3273913673577,
39.9352519465112));
#189778=CARTESIAN_POINT('Ctrl Pts',(-25.3107727110825,-57.3172883154489,
39.92499));
#189779=CARTESIAN_POINT('Ctrl Pts',(-23.9115214566117,-54.1745185419759,
39.92499));
#189780=CARTESIAN_POINT('Ctrl Pts',(-23.9072166846462,-54.1648498658381,
39.9348107241728));
#189781=CARTESIAN_POINT('Ctrl Pts',(-23.903689995662,-54.1548764216391,
39.9446038383182));
#189782=CARTESIAN_POINT('Ctrl Pts',(-23.9009524404112,-54.1446552025529,
39.9543158069403));
#189783=CARTESIAN_POINT('Ctrl Pts',(-23.8983090899558,-54.134785716223,
39.9636935671413));
#189784=CARTESIAN_POINT('Ctrl Pts',(-23.8964012454632,-54.124683974275,
39.9729968321014));
#189785=CARTESIAN_POINT('Ctrl Pts',(-23.8952825179495,-54.1143872866722,
39.9821731151364));
#189786=CARTESIAN_POINT('Ctrl Pts',(-23.8942249700852,-54.1046536921647,
39.9908475764383));
#189787=CARTESIAN_POINT('Ctrl Pts',(-23.8938724934878,-54.0947449925285,
39.9994093733879));
#189788=CARTESIAN_POINT('Ctrl Pts',(-23.8943122764065,-54.0846948896014,
40.0077966115876));
#189789=CARTESIAN_POINT('Ctrl Pts',(-23.8947173090968,-54.0754389134087,
40.015521117263));
#189790=CARTESIAN_POINT('Ctrl Pts',(-23.8957944255627,-54.0660624571189,
40.0230979941058));
#189791=CARTESIAN_POINT('Ctrl Pts',(-23.8976480927561,-54.0566033397473,
40.0304554104785));
#189792=CARTESIAN_POINT('Ctrl Pts',(-23.8982008188942,-54.0537828218934,
40.0326492435205));
#189793=CARTESIAN_POINT('Ctrl Pts',(-23.8988228478386,-54.0509550659726,
40.0348233715073));
#189794=CARTESIAN_POINT('Ctrl Pts',(-23.8995176373646,-54.0481214021002,
40.0369753512356));
#189795=CARTESIAN_POINT('Ctrl Pts',(-23.9002053278541,-54.0453166912882,
40.0391053430352));
#189796=CARTESIAN_POINT('Ctrl Pts',(-23.9009633199468,-54.0425090377019,
40.041211089324));
#189797=CARTESIAN_POINT('Ctrl Pts',(-23.9017938716382,-54.0397028685176,
40.0432881154904));
#189798=CARTESIAN_POINT('Ctrl Pts',(-23.9018516265785,-54.0395077330005,
40.043432547828));
#189799=CARTESIAN_POINT('Ctrl Pts',(-23.9019097237178,-54.0393125964103,
40.0435768364421));
#189800=CARTESIAN_POINT('Ctrl Pts',(-23.9019681642225,-54.0391174593311,
40.0437209807855));
#189801=CARTESIAN_POINT('Ctrl Pts',(-23.9045304100324,-54.0305619349332,
40.050040796842));
#189802=CARTESIAN_POINT('Ctrl Pts',(-23.9077916774637,-54.0220283896862,
40.0560490279344));
#189803=CARTESIAN_POINT('Ctrl Pts',(-23.9117952627744,-54.0136246330487,
40.0616647108614));
#189804=CARTESIAN_POINT('Ctrl Pts',(-23.9155273001023,-54.0057908712996,
40.0668995033484));
#189805=CARTESIAN_POINT('Ctrl Pts',(-23.9199049461654,-53.9980693056379,
40.0717933267479));
#189806=CARTESIAN_POINT('Ctrl Pts',(-23.9249777890349,-53.9905727747497,
40.076246030307));
#189807=CARTESIAN_POINT('Ctrl Pts',(-23.9268335005852,-53.9878304467662,
40.0778748868746));
#189808=CARTESIAN_POINT('Ctrl Pts',(-23.9287823509748,-53.9851185338202,
40.0794443522247));
#189809=CARTESIAN_POINT('Ctrl Pts',(-23.9308270955486,-53.9824437337506,
40.0809482021492));
#189810=CARTESIAN_POINT('Ctrl Pts',(-23.9313187883097,-53.9818005336911,
40.0813098278168));
#189811=CARTESIAN_POINT('Ctrl Pts',(-23.9318165831366,-53.9811593045603,
40.0816679525672));
#189812=CARTESIAN_POINT('Ctrl Pts',(-23.9323204546079,-53.980520179637,
40.082022419258));
#189813=CARTESIAN_POINT('Ctrl Pts',(-23.9328085800956,-53.9799010273675,
40.0823658088648));
#189814=CARTESIAN_POINT('Ctrl Pts',(-23.9333024083484,-53.979283849857,
40.0827057654616));
#189815=CARTESIAN_POINT('Ctrl Pts',(-23.9338019127824,-53.978668769797,
40.0830421470151));
#189816=CARTESIAN_POINT('Ctrl Pts',(-23.9392745611216,-53.9719298569083,
40.0867275956806));
#189817=CARTESIAN_POINT('Ctrl Pts',(-23.9454324752044,-53.9654385427828,
40.089982343203));
#189818=CARTESIAN_POINT('Ctrl Pts',(-23.9522153560504,-53.9593734277047,
40.0926299529355));
#189819=CARTESIAN_POINT('Ctrl Pts',(-23.9550284189133,-53.9568580437,40.0937279956084));
#189820=CARTESIAN_POINT('Ctrl Pts',(-23.9579485624028,-53.954415862194,
40.0947220371802));
#189821=CARTESIAN_POINT('Ctrl Pts',(-23.9609698772114,-53.9520587513131,
40.0956014538692));
#189822=CARTESIAN_POINT('Ctrl Pts',(-23.9661230444607,-53.9480384530774,
40.097101390674));
#189823=CARTESIAN_POINT('Ctrl Pts',(-23.9715702598497,-53.9442681092574,
40.0982667904316));
#189824=CARTESIAN_POINT('Ctrl Pts',(-23.9772776109213,-53.9408121161403,
40.0990539325582));
#189825=CARTESIAN_POINT('Ctrl Pts',(-23.9801312864571,-53.9390841195818,
40.0994475036216));
#189826=CARTESIAN_POINT('Ctrl Pts',(-23.9830506455188,-53.937436003503,
40.0997467259952));
#189827=CARTESIAN_POINT('Ctrl Pts',(-23.986031430386,-53.9358758804725,
40.0999473488896));
#189828=CARTESIAN_POINT('Ctrl Pts',(-23.9890122152531,-53.934315757442,
40.100147971784));
#189829=CARTESIAN_POINT('Ctrl Pts',(-23.9920543802864,-53.9328436288552,
40.10025));
#189830=CARTESIAN_POINT('Ctrl Pts',(-23.995153256981,-53.9314655730803,
40.10025));
#189831=CARTESIAN_POINT('Origin',(-29.1450842944632,-50.4502867888874,39.92499));
#189832=CARTESIAN_POINT('Ctrl Pts',(-31.4933613949861,-54.1671020372437,
39.92499));
#189833=CARTESIAN_POINT('Ctrl Pts',(-31.4986665597482,-54.1762908521541,
39.9348354642018));
#189834=CARTESIAN_POINT('Ctrl Pts',(-31.5032309550537,-54.1858709973829,
39.9446440828459));
#189835=CARTESIAN_POINT('Ctrl Pts',(-31.5070391691409,-54.195785428784,
39.9543641760333));
#189836=CARTESIAN_POINT('Ctrl Pts',(-31.5107236389468,-54.2053777002011,
39.9637684240715));
#189837=CARTESIAN_POINT('Ctrl Pts',(-31.5137006693055,-54.2152841131315,
39.97309096364));
#189838=CARTESIAN_POINT('Ctrl Pts',(-31.5159144374966,-54.2254725303162,
39.9822808977146));
#189839=CARTESIAN_POINT('Ctrl Pts',(-31.5180085258894,-54.2351101456063,
39.9909740094657));
#189840=CARTESIAN_POINT('Ctrl Pts',(-31.5194198476566,-54.245001003774,
39.999549276501));
#189841=CARTESIAN_POINT('Ctrl Pts',(-31.5200591406751,-54.2551207303727,
40.0079462328705));
#189842=CARTESIAN_POINT('Ctrl Pts',(-31.5206479757801,-54.2644417304473,
40.0156804369702));
#189843=CARTESIAN_POINT('Ctrl Pts',(-31.5205818213852,-54.2739574575959,
40.0232638017436));
#189844=CARTESIAN_POINT('Ctrl Pts',(-31.5197533892255,-54.283641520256,
40.0306257269981));
#189845=CARTESIAN_POINT('Ctrl Pts',(-31.5195130925471,-54.2864504987141,
40.0327611416661));
#189846=CARTESIAN_POINT('Ctrl Pts',(-31.5192084034331,-54.2892735615571,
40.0348777427276));
#189847=CARTESIAN_POINT('Ctrl Pts',(-31.518836042558,-54.2921098354278,
40.0369733168701));
#189848=CARTESIAN_POINT('Ctrl Pts',(-31.5184323794287,-54.29518453866,40.039245053974));
#189849=CARTESIAN_POINT('Ctrl Pts',(-31.5179508191006,-54.2982706300313,
40.041487875195));
#189850=CARTESIAN_POINT('Ctrl Pts',(-31.5173878381078,-54.3013662138032,
40.0436985701601));
#189851=CARTESIAN_POINT('Ctrl Pts',(-31.5158427323552,-54.3098620677558,
40.0497658398386));
#189852=CARTESIAN_POINT('Ctrl Pts',(-31.5136439393734,-54.3184108612911,
40.0555581699984));
#189853=CARTESIAN_POINT('Ctrl Pts',(-31.5107627835359,-54.3269129314606,
40.0609828468886));
#189854=CARTESIAN_POINT('Ctrl Pts',(-31.508126682366,-54.3346918640779,
40.0659461317307));
#189855=CARTESIAN_POINT('Ctrl Pts',(-31.504913297521,-54.3424218244388,
40.0706039980711));
#189856=CARTESIAN_POINT('Ctrl Pts',(-31.5010675328654,-54.350033371916,
40.0748843180609));
#189857=CARTESIAN_POINT('Ctrl Pts',(-31.4991785058296,-54.3537721391722,
40.0769867972573));
#189858=CARTESIAN_POINT('Ctrl Pts',(-31.4971365594545,-54.3574819590039,
40.0789976708176));
#189859=CARTESIAN_POINT('Ctrl Pts',(-31.4949332463336,-54.361151856945,
40.08090504915));
#189860=CARTESIAN_POINT('Ctrl Pts',(-31.4945151891294,-54.361848184334,
40.0812669556105));
#189861=CARTESIAN_POINT('Ctrl Pts',(-31.494090808751,-54.3625432124816,
40.0816253922033));
#189862=CARTESIAN_POINT('Ctrl Pts',(-31.4936601139564,-54.3632368016452,
40.0819801989139));
#189863=CARTESIAN_POINT('Ctrl Pts',(-31.4932428783741,-54.3639087161473,
40.0823239179149));
#189864=CARTESIAN_POINT('Ctrl Pts',(-31.4928197168825,-54.3645792801847,
40.0826642303498));
#189865=CARTESIAN_POINT('Ctrl Pts',(-31.4923906407828,-54.3652483648079,
40.0830009916099));
#189866=CARTESIAN_POINT('Ctrl Pts',(-31.4877146578622,-54.372539911164,
40.0866709464311));
#189867=CARTESIAN_POINT('Ctrl Pts',(-31.4823328301626,-54.379660339308,
40.0899175831876));
#189868=CARTESIAN_POINT('Ctrl Pts',(-31.4762829888802,-54.3864229856956,
40.092564206706));
#189869=CARTESIAN_POINT('Ctrl Pts',(-31.4737281033389,-54.3892788932593,
40.0936818922527));
#189870=CARTESIAN_POINT('Ctrl Pts',(-31.471054515739,-54.3920710496175,
40.094693009479));
#189871=CARTESIAN_POINT('Ctrl Pts',(-31.4682668669588,-54.3947861357354,
40.0955863397546));
#189872=CARTESIAN_POINT('Ctrl Pts',(-31.4635725360689,-54.3993582729151,
40.0970906856166));
#189873=CARTESIAN_POINT('Ctrl Pts',(-31.4585547584353,-54.4037093249066,
40.0982599215483));
#189874=CARTESIAN_POINT('Ctrl Pts',(-31.4532397415957,-54.4077698566064,
40.0990497370454));
#189875=CARTESIAN_POINT('Ctrl Pts',(-31.4519109873858,-54.4087849895313,
40.0992471909196));
#189876=CARTESIAN_POINT('Ctrl Pts',(-31.4505635261659,-54.4097817701142,
40.0994209989363));
#189877=CARTESIAN_POINT('Ctrl Pts',(-31.449197606926,-54.4107588499957,
40.0995705982975));
#189878=CARTESIAN_POINT('Ctrl Pts',(-31.4471487280663,-54.412224469818,
40.0997949973393));
#189879=CARTESIAN_POINT('Ctrl Pts',(-31.445058325466,-54.4136457436053,
40.0999649129781));
#189880=CARTESIAN_POINT('Ctrl Pts',(-31.442928094411,-54.4150195646479,
40.1000786629733));
#189881=CARTESIAN_POINT('Ctrl Pts',(-31.4407978633561,-54.4163933856906,
40.1001924129685));
#189882=CARTESIAN_POINT('Ctrl Pts',(-31.438627814593,-54.4177197583743,
40.10025));
#189883=CARTESIAN_POINT('Ctrl Pts',(-31.4364195775146,-54.4189959163077,
40.10025));
#189884=CARTESIAN_POINT('Ctrl Pts',(-29.5274749692187,-51.1126068659045,
40.10025));
#189885=CARTESIAN_POINT('Ctrl Pts',(-29.5349468458348,-51.1082885388128,
40.10025));
#189886=CARTESIAN_POINT('Ctrl Pts',(-29.5427104181385,-51.1046244142385,
40.0995786334241));
#189887=CARTESIAN_POINT('Ctrl Pts',(-29.5506148782564,-51.1016049255944,
40.0983063763366));
#189888=CARTESIAN_POINT('Ctrl Pts',(-29.555720348448,-51.0996546457479,
40.0974846287992));
#189889=CARTESIAN_POINT('Ctrl Pts',(-29.5608842707087,-51.0979724198486,
40.0964130309338));
#189890=CARTESIAN_POINT('Ctrl Pts',(-29.5660646037406,-51.0965469289496,
40.0951176960924));
#189891=CARTESIAN_POINT('Ctrl Pts',(-29.5729308384267,-51.0946575224201,
40.0934008039614));
#189892=CARTESIAN_POINT('Ctrl Pts',(-29.579826275578,-51.0932249325812,
40.0912909372156));
#189893=CARTESIAN_POINT('Ctrl Pts',(-29.5866628504239,-51.0922302752233,
40.0888630467851));
#189894=CARTESIAN_POINT('Ctrl Pts',(-29.5900811378468,-51.0917329465443,
40.0876491015699));
#189895=CARTESIAN_POINT('Ctrl Pts',(-29.5934848814075,-51.0913449998288,
40.0863558569271));
#189896=CARTESIAN_POINT('Ctrl Pts',(-29.5968642938812,-51.0910633609952,
40.0849936342771));
#189897=CARTESIAN_POINT('Ctrl Pts',(-29.598554000118,-51.0909225415784,
40.0843125229521));
#189898=CARTESIAN_POINT('Ctrl Pts',(-29.6002376377884,-51.0908082908742,
40.0836141747074));
#189899=CARTESIAN_POINT('Ctrl Pts',(-29.6019140726117,-51.090720172667,
40.0828999161609));
#189900=CARTESIAN_POINT('Ctrl Pts',(-29.6023331813176,-51.0906981431152,
40.0827213515243));
#189901=CARTESIAN_POINT('Ctrl Pts',(-29.6027518401471,-51.0906777466679,
40.0825417925842));
#189902=CARTESIAN_POINT('Ctrl Pts',(-29.6031700319853,-51.0906589761529,
40.0823612602361));
#189903=CARTESIAN_POINT('Ctrl Pts',(-29.6044246074998,-51.090602664608,
40.0818196631917));
#189904=CARTESIAN_POINT('Ctrl Pts',(-29.6056749785905,-51.0905609873412,
40.0812693052022));
#189905=CARTESIAN_POINT('Ctrl Pts',(-29.6069206965766,-51.0905337427829,
40.0807107531875));
#189906=CARTESIAN_POINT('Ctrl Pts',(-29.6156953732195,-51.0903418356316,
40.0767763849181));
#189907=CARTESIAN_POINT('Ctrl Pts',(-29.6242688491609,-51.090821136893,
40.0724140586136));
#189908=CARTESIAN_POINT('Ctrl Pts',(-29.6325885911862,-51.091864142426,
40.0677221223767));
#189909=CARTESIAN_POINT('Ctrl Pts',(-29.636623657078,-51.0923699989824,
40.065446538372));
#189910=CARTESIAN_POINT('Ctrl Pts',(-29.6405993642579,-51.0930089302515,
40.0630928000679));
#189911=CARTESIAN_POINT('Ctrl Pts',(-29.6445110377126,-51.0937712117413,
40.0606689262479));
#189912=CARTESIAN_POINT('Ctrl Pts',(-29.6504995364713,-51.0949382114431,
40.0569581447805));
#189913=CARTESIAN_POINT('Ctrl Pts',(-29.6563348640822,-51.0963926103115,
40.0530843804606));
#189914=CARTESIAN_POINT('Ctrl Pts',(-29.6619874481817,-51.098099028059,
40.0490800251458));
#189915=CARTESIAN_POINT('Ctrl Pts',(-29.66461253748,-51.0988914972887,40.0472203818218));
#189916=CARTESIAN_POINT('Ctrl Pts',(-29.6671982043428,-51.0997380650832,
40.0453323608819));
#189917=CARTESIAN_POINT('Ctrl Pts',(-29.6697408831278,-51.1006362623628,
40.0434201572162));
#189918=CARTESIAN_POINT('Ctrl Pts',(-29.669935769438,-51.1007051056452,
40.0432735943397));
#189919=CARTESIAN_POINT('Ctrl Pts',(-29.6701304259133,-51.1007742270249,
40.0431268995707));
#189920=CARTESIAN_POINT('Ctrl Pts',(-29.670324852047,-51.1008436251323,
40.0429800745037));
#189921=CARTESIAN_POINT('Ctrl Pts',(-29.6730559530502,-51.1018184593123,
40.0409176249753));
#189922=CARTESIAN_POINT('Ctrl Pts',(-29.675741029822,-51.1028499068177,
40.0388310783332));
#189923=CARTESIAN_POINT('Ctrl Pts',(-29.6783776815771,-51.1039327914266,
40.036725739981));
#189924=CARTESIAN_POINT('Ctrl Pts',(-29.687832245858,-51.1078158230496,
40.0291763710718));
#189925=CARTESIAN_POINT('Ctrl Pts',(-29.6967379921829,-51.1123884412301,
40.0213310894596));
#189926=CARTESIAN_POINT('Ctrl Pts',(-29.7051147523676,-51.1175230541891,
40.0132837551322));
#189927=CARTESIAN_POINT('Ctrl Pts',(-29.7143199702903,-51.1231654780134,
40.004440543133));
#189928=CARTESIAN_POINT('Ctrl Pts',(-29.7228870317498,-51.129486757896,
39.9953528710608));
#189929=CARTESIAN_POINT('Ctrl Pts',(-29.7308286942753,-51.1363687775772,
39.9861103629565));
#189930=CARTESIAN_POINT('Ctrl Pts',(-29.7394036967174,-51.1437996316814,
39.9761307737571));
#189931=CARTESIAN_POINT('Ctrl Pts',(-29.7472505498652,-51.151884858999,
39.9659696936032));
#189932=CARTESIAN_POINT('Ctrl Pts',(-29.7543572078919,-51.1605258584228,
39.9557128217532));
#189933=CARTESIAN_POINT('Ctrl Pts',(-29.7614042483606,-51.169094368741,
39.9455419945178));
#189934=CARTESIAN_POINT('Ctrl Pts',(-29.7677241373264,-51.1782106315433,
39.9352756289349));
#189935=CARTESIAN_POINT('Ctrl Pts',(-29.7732664904682,-51.1878102687783,
39.92499));
#189936=CARTESIAN_POINT('Origin',(0.0131982271536832,-0.00761999999999517,
39.92499));
#189937=CARTESIAN_POINT('Ctrl Pts',(-31.4100231232064,-54.4342359163062,
40.10025));
#189938=CARTESIAN_POINT('Ctrl Pts',(-31.402583092678,-54.438527272202,40.10025));
#189939=CARTESIAN_POINT('Ctrl Pts',(-31.3948506994802,-54.4421589890635,
40.0995859581842));
#189940=CARTESIAN_POINT('Ctrl Pts',(-31.3869762747703,-54.4451438299611,
40.0983275959621));
#189941=CARTESIAN_POINT('Ctrl Pts',(-31.3819448922446,-54.4470510012005,
40.0975235624068));
#189942=CARTESIAN_POINT('Ctrl Pts',(-31.3768558346353,-54.4486949601299,
40.096477705949));
#189943=CARTESIAN_POINT('Ctrl Pts',(-31.3717496422765,-54.450087528668,
40.0952149915961));
#189944=CARTESIAN_POINT('Ctrl Pts',(-31.364780714273,-54.4519881053012,
40.0934916398701));
#189945=CARTESIAN_POINT('Ctrl Pts',(-31.3577796218684,-54.4534143418202,
40.091364392163));
#189946=CARTESIAN_POINT('Ctrl Pts',(-31.3508395087087,-54.4543880442395,
40.0889118607713));
#189947=CARTESIAN_POINT('Ctrl Pts',(-31.3473694521288,-54.4548748954491,
40.0876855950754));
#189948=CARTESIAN_POINT('Ctrl Pts',(-31.3439144604656,-54.4552487192093,
40.0863782327526));
#189949=CARTESIAN_POINT('Ctrl Pts',(-31.3404848880616,-54.4555129946224,
40.0850006373334));
#189950=CARTESIAN_POINT('Ctrl Pts',(-31.3387701018596,-54.455645132329,
40.0843118396237));
#189951=CARTESIAN_POINT('Ctrl Pts',(-31.337061655417,-54.4557498916995,
40.0836054919164));
#189952=CARTESIAN_POINT('Ctrl Pts',(-31.3353607484814,-54.4558277627245,
40.0828829920417));
#189953=CARTESIAN_POINT('Ctrl Pts',(-31.3349355217475,-54.4558472304807,
40.0827023670731));
#189954=CARTESIAN_POINT('Ctrl Pts',(-31.3345107659126,-54.4558650179027,
40.0825207326933));
#189955=CARTESIAN_POINT('Ctrl Pts',(-31.3340864990772,-54.4558811330248,
40.0823381109275));
#189956=CARTESIAN_POINT('Ctrl Pts',(-31.3328136985709,-54.455929478391,
40.0817902456303));
#189957=CARTESIAN_POINT('Ctrl Pts',(-31.3315453006542,-54.4559627721157,
40.0812334935553));
#189958=CARTESIAN_POINT('Ctrl Pts',(-31.3302817797847,-54.4559812395336,
40.0806684524227));
#189959=CARTESIAN_POINT('Ctrl Pts',(-31.321550066618,-54.4561088608495,
40.0767636676136));
#189960=CARTESIAN_POINT('Ctrl Pts',(-31.3130195924487,-54.4555742713437,
40.0724404510887));
#189961=CARTESIAN_POINT('Ctrl Pts',(-31.304740085859,-54.4544853519656,
40.0677949937408));
#189962=CARTESIAN_POINT('Ctrl Pts',(-31.3006251938109,-54.4539441620238,
40.0654862141905));
#189963=CARTESIAN_POINT('Ctrl Pts',(-31.2965719591987,-54.4532655373258,
40.0630972003215));
#189964=CARTESIAN_POINT('Ctrl Pts',(-31.2925850928566,-54.4524598885394,
40.0606363359906));
#189965=CARTESIAN_POINT('Ctrl Pts',(-31.2837894702122,-54.4506825069817,
40.0552073017123));
#189966=CARTESIAN_POINT('Ctrl Pts',(-31.2753153512349,-54.4482992497265,
40.0494204304519));
#189967=CARTESIAN_POINT('Ctrl Pts',(-31.2672761140353,-54.4454010706196,
40.0434049749851));
#189968=CARTESIAN_POINT('Ctrl Pts',(-31.2643392793061,-54.444342329244,
40.0412074532442));
#189969=CARTESIAN_POINT('Ctrl Pts',(-31.2614550023641,-54.4432206434042,
40.0389814735788));
#189970=CARTESIAN_POINT('Ctrl Pts',(-31.2586246102248,-54.4420411592046,
40.0367321210016));
#189971=CARTESIAN_POINT('Ctrl Pts',(-31.2491176225321,-54.4380793965875,
40.0291767837144));
#189972=CARTESIAN_POINT('Ctrl Pts',(-31.2401615453402,-54.4334326446233,
40.0213235332584));
#189973=CARTESIAN_POINT('Ctrl Pts',(-31.2317373058281,-54.4282277812596,
40.0132649215871));
#189974=CARTESIAN_POINT('Ctrl Pts',(-31.2224780686874,-54.4225070198663,
40.0044075527549));
#189975=CARTESIAN_POINT('Ctrl Pts',(-31.2138606686968,-54.4161118092716,
39.995301625374));
#189976=CARTESIAN_POINT('Ctrl Pts',(-31.2058737429093,-54.4091594014098,
39.9860353422383));
#189977=CARTESIAN_POINT('Ctrl Pts',(-31.1972714816235,-54.4016713602556,
39.9760551582724));
#189978=CARTESIAN_POINT('Ctrl Pts',(-31.1893995936796,-54.3935362880577,
39.9658879738188));
#189979=CARTESIAN_POINT('Ctrl Pts',(-31.182272586596,-54.3848513315151,
39.9556174643291));
#189980=CARTESIAN_POINT('Ctrl Pts',(-31.1752418181704,-54.3762836512082,
39.9454856413929));
#189981=CARTESIAN_POINT('Ctrl Pts',(-31.1689352997164,-54.3671795569354,
39.9352519465126));
#189982=CARTESIAN_POINT('Ctrl Pts',(-31.1634057161443,-54.3576020372437,
39.92499));
#189983=CARTESIAN_POINT('Ctrl Pts',(-29.4433108116264,-51.3783102687783,
39.92499));
#189984=CARTESIAN_POINT('Ctrl Pts',(-29.4380189697943,-51.3691445298596,
39.9348107241716));
#189985=CARTESIAN_POINT('Ctrl Pts',(-29.4334690915863,-51.3595943606125,
39.9446038383157));
#189986=CARTESIAN_POINT('Ctrl Pts',(-29.429678124626,-51.3497152868788,
39.9543158069366));
#189987=CARTESIAN_POINT('Ctrl Pts',(-29.4260176124818,-51.3401761719895,
39.9636935671369));
#189988=CARTESIAN_POINT('Ctrl Pts',(-29.4230642997988,-51.3303291924946,
39.9729968320963));
#189989=CARTESIAN_POINT('Ctrl Pts',(-29.4208754038594,-51.3202058500926,
39.9821731151306));
#189990=CARTESIAN_POINT('Ctrl Pts',(-29.4188062116769,-51.3106361210879,
39.9908475764321));
#189991=CARTESIAN_POINT('Ctrl Pts',(-29.4174199248369,-51.3008185461827,
39.9994093733814));
#189992=CARTESIAN_POINT('Ctrl Pts',(-29.4168067767638,-51.2907775289389,
40.0077966115808));
#189993=CARTESIAN_POINT('Ctrl Pts',(-29.4162420776747,-51.281529920508,
40.0155211172561));
#189994=CARTESIAN_POINT('Ctrl Pts',(-29.4163331870166,-51.2720922400983,
40.0230979940988));
#189995=CARTESIAN_POINT('Ctrl Pts',(-29.4171879526239,-51.2624911797787,
40.0304554104714));
#189996=CARTESIAN_POINT('Ctrl Pts',(-29.4174428264736,-51.2596283373998,
40.0326492435158));
#189997=CARTESIAN_POINT('Ctrl Pts',(-29.4177658668977,-51.2567510524891,
40.0348233715049));
#189998=CARTESIAN_POINT('Ctrl Pts',(-29.4181606517644,-51.2538602864393,
40.0369753512355));
#189999=CARTESIAN_POINT('Ctrl Pts',(-29.4185514029024,-51.2509990568965,
40.0391053430352));
#190000=CARTESIAN_POINT('Ctrl Pts',(-29.4190117629203,-51.2481275521817,
40.041211089324));
#190001=CARTESIAN_POINT('Ctrl Pts',(-29.4195444402101,-51.2452499391938,
40.0432881154904));
#190002=CARTESIAN_POINT('Ctrl Pts',(-29.4195814815471,-51.2450498356144,
40.043432547828));
#190003=CARTESIAN_POINT('Ctrl Pts',(-29.4196188630963,-51.2448496951982,
40.0435768364421));
#190004=CARTESIAN_POINT('Ctrl Pts',(-29.4196565860788,-51.2446495184042,
40.0437209807855));
#190005=CARTESIAN_POINT('Ctrl Pts',(-29.4213104998203,-51.235873034447,
40.050040796842));
#190006=CARTESIAN_POINT('Ctrl Pts',(-29.4236619033165,-51.2270453415808,
40.0560490279344));
#190007=CARTESIAN_POINT('Ctrl Pts',(-29.426765124801,-51.2182691329814,
40.0616647108614));
#190008=CARTESIAN_POINT('Ctrl Pts',(-29.4296578665607,-51.2100881812721,
40.0668995033484));
#190009=CARTESIAN_POINT('Ctrl Pts',(-29.4332044080279,-51.2019513265394,
40.071793326748));
#190010=CARTESIAN_POINT('Ctrl Pts',(-29.4374658604799,-51.1939656059622,
40.076246030307));
#190011=CARTESIAN_POINT('Ctrl Pts',(-29.4390247549183,-51.1910443260617,
40.0778748868747));
#190012=CARTESIAN_POINT('Ctrl Pts',(-29.4406794572087,-51.1881435589222,
40.0794443522247));
#190013=CARTESIAN_POINT('Ctrl Pts',(-29.4424334077169,-51.1852696776792,
40.0809482021492));
#190014=CARTESIAN_POINT('Ctrl Pts',(-29.4428551742199,-51.1845786052482,
40.0813098278169));
#190015=CARTESIAN_POINT('Ctrl Pts',(-29.443283215379,-51.1838888551094,
40.0816679525672));
#190016=CARTESIAN_POINT('Ctrl Pts',(-29.4437175198435,-51.1832005624687,
40.0820224192581));
#190017=CARTESIAN_POINT('Ctrl Pts',(-29.4441382522935,-51.1825337789731,
40.0823658088648));
#190018=CARTESIAN_POINT('Ctrl Pts',(-29.4445648626868,-51.1818683633171,
40.0827057654617));
#190019=CARTESIAN_POINT('Ctrl Pts',(-29.4449973374098,-51.1812044402992,
40.0830421470151));
#190020=CARTESIAN_POINT('Ctrl Pts',(-29.4497355978005,-51.1739303963594,
40.0867275956807));
#190021=CARTESIAN_POINT('Ctrl Pts',(-29.4551812510955,-51.1668309650357,
40.0899823432031));
#190022=CARTESIAN_POINT('Ctrl Pts',(-29.461292997452,-51.1600900711811,
40.0926299529356));
#190023=CARTESIAN_POINT('Ctrl Pts',(-29.4638277208377,-51.1572944215752,
40.0937279956085));
#190024=CARTESIAN_POINT('Ctrl Pts',(-29.4664765899956,-51.1545603804837,
40.0947220371803));
#190025=CARTESIAN_POINT('Ctrl Pts',(-29.4692349685474,-51.1519003687089,
40.0956014538693));
#190026=CARTESIAN_POINT('Ctrl Pts',(-29.4739396706108,-51.147363441434,
40.097101390674));
#190027=CARTESIAN_POINT('Ctrl Pts',(-29.4789629373384,-51.1430443628983,
40.0982667904316));
#190028=CARTESIAN_POINT('Ctrl Pts',(-29.4842777732941,-51.1390107214363,
40.0990539325583));
#190029=CARTESIAN_POINT('Ctrl Pts',(-29.486935191272,-51.1369939007053,
40.0994475036216));
#190030=CARTESIAN_POINT('Ctrl Pts',(-29.4896662827383,-51.1350496570623,
40.0997467259952));
#190031=CARTESIAN_POINT('Ctrl Pts',(-29.4924676612911,-51.1331865036875,
40.0999473488896));
#190032=CARTESIAN_POINT('Ctrl Pts',(-29.495269039844,-51.1313233503127,
40.100147971784));
#190033=CARTESIAN_POINT('Ctrl Pts',(-29.49814066024,-51.1295412933645,40.10025));
#190034=CARTESIAN_POINT('Ctrl Pts',(-29.5010785149114,-51.1278468659046,
40.10025));
#190035=CARTESIAN_POINT('Origin',(-34.2589154226524,-47.1274239660508,39.92499));
#190036=CARTESIAN_POINT('Ctrl Pts',(-36.9828414016749,-50.5784163149355,
39.92499));
#190037=CARTESIAN_POINT('Ctrl Pts',(-36.989077996891,-50.5870002518363,
39.9348354642021));
#190038=CARTESIAN_POINT('Ctrl Pts',(-36.99461878582,-50.5960508068,39.9446440828464));
#190039=CARTESIAN_POINT('Ctrl Pts',(-36.9994424783905,-50.6055128591422,
39.9543641760339));
#190040=CARTESIAN_POINT('Ctrl Pts',(-37.0041094296757,-50.6146674511261,
39.9637684240722));
#190041=CARTESIAN_POINT('Ctrl Pts',(-37.0081056536708,-50.6242084112815,
39.9730909636407));
#190042=CARTESIAN_POINT('Ctrl Pts',(-37.0113722741996,-50.6341096134638,
39.9822808977153));
#190043=CARTESIAN_POINT('Ctrl Pts',(-37.0144622960729,-50.6434755410473,
39.9909740094663));
#190044=CARTESIAN_POINT('Ctrl Pts',(-37.0168997626766,-50.6531646927637,
39.9995492765015));
#190045=CARTESIAN_POINT('Ctrl Pts',(-37.0185933530511,-50.6631621581244,
40.0079462328709));
#190046=CARTESIAN_POINT('Ctrl Pts',(-37.0201532722697,-50.6723705467568,
40.0156804369705));
#190047=CARTESIAN_POINT('Ctrl Pts',(-37.0210821446113,-50.6818410607736,
40.0232638017438));
#190048=CARTESIAN_POINT('Ctrl Pts',(-37.0212705108777,-50.6915586678658,
40.0306257269983));
#190049=CARTESIAN_POINT('Ctrl Pts',(-37.0213251487712,-50.6943773762885,
40.0327611416662));
#190050=CARTESIAN_POINT('Ctrl Pts',(-37.0213172191968,-50.6972168227827,
40.0348777427276));
#190051=CARTESIAN_POINT('Ctrl Pts',(-37.0212433695026,-50.7000764815584,
40.0369733168701));
#190052=CARTESIAN_POINT('Ctrl Pts',(-37.021163311686,-50.7031765355312,
40.0392450539741));
#190053=CARTESIAN_POINT('Ctrl Pts',(-37.0210069737843,-50.706296057732,
40.041487875195));
#190054=CARTESIAN_POINT('Ctrl Pts',(-37.0207706534748,-50.7094335311102,
40.0436985701601));
#190055=CARTESIAN_POINT('Ctrl Pts',(-37.0201220705311,-50.7180443514158,
40.0497658398386));
#190056=CARTESIAN_POINT('Ctrl Pts',(-37.0188289150183,-50.7267761502171,
40.0555581699984));
#190057=CARTESIAN_POINT('Ctrl Pts',(-37.0168522507833,-50.7355328079488,
40.0609828468885));
#190058=CARTESIAN_POINT('Ctrl Pts',(-37.015043710324,-50.743544674363,40.0659461317303));
#190059=CARTESIAN_POINT('Ctrl Pts',(-37.0126559296152,-50.7515681793715,
40.0706039980704));
#190060=CARTESIAN_POINT('Ctrl Pts',(-37.009626855822,-50.7595400218642,
40.07488431806));
#190061=CARTESIAN_POINT('Ctrl Pts',(-37.0081389846695,-50.7634557648558,
40.0769867972568));
#190062=CARTESIAN_POINT('Ctrl Pts',(-37.0064960060562,-50.7673587034236,
40.0789976708174));
#190063=CARTESIAN_POINT('Ctrl Pts',(-37.0046883717069,-50.7712388062148,
40.08090504915));
#190064=CARTESIAN_POINT('Ctrl Pts',(-37.0043453906958,-50.7719750179268,
40.0812669556105));
#190065=CARTESIAN_POINT('Ctrl Pts',(-37.0039959853417,-50.7727105984662,
40.0816253922032));
#190066=CARTESIAN_POINT('Ctrl Pts',(-37.0036401497476,-50.7734454079408,
40.0819801989139));
#190067=CARTESIAN_POINT('Ctrl Pts',(-37.0032954340158,-50.7741572546192,
40.0823239179149));
#190068=CARTESIAN_POINT('Ctrl Pts',(-37.0029446836755,-50.774868377657,
40.0826642303498));
#190069=CARTESIAN_POINT('Ctrl Pts',(-37.0025878964871,-50.77557864763,40.0830009916099));
#190070=CARTESIAN_POINT('Ctrl Pts',(-36.9986997032254,-50.7833190234415,
40.0866709464313));
#190071=CARTESIAN_POINT('Ctrl Pts',(-36.9940916451525,-50.7909629993145,
40.0899175831879));
#190072=CARTESIAN_POINT('Ctrl Pts',(-36.988781834568,-50.7983209798302,
40.0925642067064));
#190073=CARTESIAN_POINT('Ctrl Pts',(-36.986539468586,-50.8014283006926,
40.0936818922529));
#190074=CARTESIAN_POINT('Ctrl Pts',(-36.9841723869923,-50.804484627329,
40.0946930094791));
#190075=CARTESIAN_POINT('Ctrl Pts',(-36.9816838130236,-50.8074762285638,
40.0955863397546));
#190076=CARTESIAN_POINT('Ctrl Pts',(-36.9774931166428,-50.8125140102917,
40.0970906856166));
#190077=CARTESIAN_POINT('Ctrl Pts',(-36.9729576356984,-50.8173657273501,
40.0982599215483));
#190078=CARTESIAN_POINT('Ctrl Pts',(-36.9680961762159,-50.8219595855752,
40.0990497370454));
#190079=CARTESIAN_POINT('Ctrl Pts',(-36.9668808113453,-50.8231080501314,
40.0992471909196));
#190080=CARTESIAN_POINT('Ctrl Pts',(-36.9656449236015,-50.8242402182965,
40.0994209989363));
#190081=CARTESIAN_POINT('Ctrl Pts',(-36.9643886196686,-50.8253547230713,
40.0995705982975));
#190082=CARTESIAN_POINT('Ctrl Pts',(-36.9625041637694,-50.8270264802335,
40.0997949973393));
#190083=CARTESIAN_POINT('Ctrl Pts',(-36.9605737761781,-50.8286584747056,
40.0999649129781));
#190084=CARTESIAN_POINT('Ctrl Pts',(-36.9585988181541,-50.8302474395914,
40.1000786629733));
#190085=CARTESIAN_POINT('Ctrl Pts',(-36.9566238601301,-50.8318364044772,
40.1001924129685));
#190086=CARTESIAN_POINT('Ctrl Pts',(-36.9546043428195,-50.8333823430148,
40.10025));
#190087=CARTESIAN_POINT('Ctrl Pts',(-36.9525415975225,-50.8348823336498,
40.10025));
#190088=CARTESIAN_POINT('Ctrl Pts',(-34.7084426211234,-47.7461450747863,
40.10025));
#190089=CARTESIAN_POINT('Ctrl Pts',(-34.7154221779228,-47.7410693801618,
40.10025));
#190090=CARTESIAN_POINT('Ctrl Pts',(-34.722760215254,-47.7366138137629,
40.0995786334241));
#190091=CARTESIAN_POINT('Ctrl Pts',(-34.7303057514044,-47.7327846251246,
40.0983063763366));
#190092=CARTESIAN_POINT('Ctrl Pts',(-34.7351793935409,-47.7303113621616,
40.0974846287993));
#190093=CARTESIAN_POINT('Ctrl Pts',(-34.7401391868071,-47.7280985748135,
40.0964130309338));
#190094=CARTESIAN_POINT('Ctrl Pts',(-34.7451421370596,-47.7261394006517,
40.0951176960924));
#190095=CARTESIAN_POINT('Ctrl Pts',(-34.7517732610326,-47.7235426275287,
40.0934008039614));
#190096=CARTESIAN_POINT('Ctrl Pts',(-34.7584811778434,-47.7213971161179,
40.0912909372156));
#190097=CARTESIAN_POINT('Ctrl Pts',(-34.7651763312118,-47.7196932909344,
40.0888630467851));
#190098=CARTESIAN_POINT('Ctrl Pts',(-34.768523907896,-47.7188413783427,
40.0876491015699));
#190099=CARTESIAN_POINT('Ctrl Pts',(-34.7718684539193,-47.718099768756,
40.0863558569271));
#190100=CARTESIAN_POINT('Ctrl Pts',(-34.7751999143434,-47.7174664279768,
40.0849936342771));
#190101=CARTESIAN_POINT('Ctrl Pts',(-34.7768656445554,-47.7171497575872,
40.0843125229521));
#190102=CARTESIAN_POINT('Ctrl Pts',(-34.7785281166319,-47.7168601447019,
40.0836141747074));
#190103=CARTESIAN_POINT('Ctrl Pts',(-34.7801861569092,-47.7165972740596,
40.0828999161609));
#190104=CARTESIAN_POINT('Ctrl Pts',(-34.7806006669785,-47.716531556399,
40.0827213515243));
#190105=CARTESIAN_POINT('Ctrl Pts',(-34.7810149003418,-47.7164675099216,
40.0825417925842));
#190106=CARTESIAN_POINT('Ctrl Pts',(-34.7814288392283,-47.7164051292833,
40.0823612602361));
#190107=CARTESIAN_POINT('Ctrl Pts',(-34.7826706558876,-47.7162179873683,
40.0818196631917));
#190108=CARTESIAN_POINT('Ctrl Pts',(-34.783909820854,-47.7160458390453,
40.0812693052022));
#190109=CARTESIAN_POINT('Ctrl Pts',(-34.7851458668348,-47.7158885307487,
40.0807107531875));
#190110=CARTESIAN_POINT('Ctrl Pts',(-34.7938524151213,-47.7147804714198,
40.0767763849182));
#190111=CARTESIAN_POINT('Ctrl Pts',(-34.8024290252887,-47.7143609747537,
40.0724140586137));
#190112=CARTESIAN_POINT('Ctrl Pts',(-34.8108122146622,-47.7145286167445,
40.0677221223767));
#190113=CARTESIAN_POINT('Ctrl Pts',(-34.8148780524494,-47.7146099229289,
40.065446538372));
#190114=CARTESIAN_POINT('Ctrl Pts',(-34.818898766793,-47.7148297795038,
40.0630928000679));
#190115=CARTESIAN_POINT('Ctrl Pts',(-34.8228686918041,-47.7151790039208,
40.0606689262479));
#190116=CARTESIAN_POINT('Ctrl Pts',(-34.8289463696254,-47.7157136421036,
40.0569581447806));
#190117=CARTESIAN_POINT('Ctrl Pts',(-34.8349017567798,-47.716550115795,
40.0530843804606));
#190118=CARTESIAN_POINT('Ctrl Pts',(-34.8407017446569,-47.717656329678,
40.0490800251458));
#190119=CARTESIAN_POINT('Ctrl Pts',(-34.8433952890323,-47.7181700611281,
40.0472203818218));
#190120=CARTESIAN_POINT('Ctrl Pts',(-34.8460552817721,-47.718741715552,
40.0453323608819));
#190121=CARTESIAN_POINT('Ctrl Pts',(-34.8486779186779,-47.7193692101069,
40.0434201572162));
#190122=CARTESIAN_POINT('Ctrl Pts',(-34.848878933463,-47.7194173050921,
40.0432735943397));
#190123=CARTESIAN_POINT('Ctrl Pts',(-34.8490797487414,-47.7194657006755,
40.0431268995707));
#190124=CARTESIAN_POINT('Ctrl Pts',(-34.849280363866,-47.7195143955478,
40.0429800745037));
#190125=CARTESIAN_POINT('Ctrl Pts',(-34.8520984015308,-47.7201984116933,
40.0409176249753));
#190126=CARTESIAN_POINT('Ctrl Pts',(-34.8548765847938,-47.7209435418726,
40.0388310783332));
#190127=CARTESIAN_POINT('Ctrl Pts',(-34.8576119849588,-47.7217448891702,
40.036725739981));
#190128=CARTESIAN_POINT('Ctrl Pts',(-34.8674206434757,-47.7246183780645,
40.0291763710718));
#190129=CARTESIAN_POINT('Ctrl Pts',(-34.8767555719421,-47.7282350429866,
40.0213310894595));
#190130=CARTESIAN_POINT('Ctrl Pts',(-34.8856231565602,-47.7324659181293,
40.0132837551321));
#190131=CARTESIAN_POINT('Ctrl Pts',(-34.8953677412278,-47.7371152248822,
40.0044405431325));
#190132=CARTESIAN_POINT('Ctrl Pts',(-34.9045486251006,-47.7425063743635,
39.9953528710599));
#190133=CARTESIAN_POINT('Ctrl Pts',(-34.9131661493096,-47.7485205638414,
39.9861103629552));
#190134=CARTESIAN_POINT('Ctrl Pts',(-34.9224709127524,-47.7550143791224,
39.9761307737546));
#190135=CARTESIAN_POINT('Ctrl Pts',(-34.9311199164051,-47.7622350952187,
39.9659696935995));
#190136=CARTESIAN_POINT('Ctrl Pts',(-34.939090873807,-47.7700859103021,
39.9557128217484));
#190137=CARTESIAN_POINT('Ctrl Pts',(-34.9469949630654,-47.7778708651125,
39.9455419945145));
#190138=CARTESIAN_POINT('Ctrl Pts',(-34.9542331399583,-47.7862765797904,
39.9352756289333));
#190139=CARTESIAN_POINT('Ctrl Pts',(-34.9607485668368,-47.79524429555,39.92499));
#190140=CARTESIAN_POINT('Origin',(0.0123294189942831,-0.00895784724493279,
39.92499));
#190141=CARTESIAN_POINT('Ctrl Pts',(-36.9278827595329,-50.8527980281383,
40.10025));
#190142=CARTESIAN_POINT('Ctrl Pts',(-36.920932055107,-50.8578435704956,
40.10025));
#190143=CARTESIAN_POINT('Ctrl Pts',(-36.9136216385504,-50.8622636476107,
40.0995859581841));
#190144=CARTESIAN_POINT('Ctrl Pts',(-36.9061023515947,-50.8660552387517,
40.0983275959619));
#190145=CARTESIAN_POINT('Ctrl Pts',(-36.9012978851881,-50.8684778849908,
40.0975235624067));
#190146=CARTESIAN_POINT('Ctrl Pts',(-36.8964085464699,-50.8706447895123,
40.0964777059489));
#190147=CARTESIAN_POINT('Ctrl Pts',(-36.8914758894168,-50.8725634718545,
40.0952149915961));
#190148=CARTESIAN_POINT('Ctrl Pts',(-36.8847438022849,-50.8751820882649,
40.0934916398701));
#190149=CARTESIAN_POINT('Ctrl Pts',(-36.8779301449085,-50.8773323251413,
40.091364392163));
#190150=CARTESIAN_POINT('Ctrl Pts',(-36.8711298300324,-50.8790261328804,
40.0889118607712));
#190151=CARTESIAN_POINT('Ctrl Pts',(-36.8677296725944,-50.8798730367499,
40.0876855950754));
#190152=CARTESIAN_POINT('Ctrl Pts',(-36.8643326829601,-50.8806059576335,
40.0863782327526));
#190153=CARTESIAN_POINT('Ctrl Pts',(-36.8609495224154,-50.8812272732513,
40.0850006373333));
#190154=CARTESIAN_POINT('Ctrl Pts',(-36.8592579421431,-50.8815379310602,
40.0843118396237));
#190155=CARTESIAN_POINT('Ctrl Pts',(-36.8575698050848,-50.8818206978292,
40.0836054919164));
#190156=CARTESIAN_POINT('Ctrl Pts',(-36.855886355634,-50.8820759354567,
40.0828829920417));
#190157=CARTESIAN_POINT('Ctrl Pts',(-36.8554654932713,-50.8821397448636,
40.082702367073));
#190158=CARTESIAN_POINT('Ctrl Pts',(-36.8550449235852,-50.8822018339189,
40.0825207326932));
#190159=CARTESIAN_POINT('Ctrl Pts',(-36.8546246654168,-50.8822622087209,
40.0823381109275));
#190160=CARTESIAN_POINT('Ctrl Pts',(-36.8533638909117,-50.8824433331272,
40.0817902456303));
#190161=CARTESIAN_POINT('Ctrl Pts',(-36.8521059215534,-50.8826090281504,
40.0812334935553));
#190162=CARTESIAN_POINT('Ctrl Pts',(-36.8508512527542,-50.8827594682966,
40.0806684524226));
#190163=CARTESIAN_POINT('Ctrl Pts',(-36.8421807128861,-50.8837991030486,
40.0767636676137));
#190164=CARTESIAN_POINT('Ctrl Pts',(-36.8336410897277,-50.8841591194359,
40.072440451089));
#190165=CARTESIAN_POINT('Ctrl Pts',(-36.8252931160724,-50.8839416093726,
40.0677949937412));
#190166=CARTESIAN_POINT('Ctrl Pts',(-36.8211441960803,-50.8838335074682,
40.0654862141908));
#190167=CARTESIAN_POINT('Ctrl Pts',(-36.8170422299142,-50.8835822787326,
40.0630972003217));
#190168=CARTESIAN_POINT('Ctrl Pts',(-36.8129929908133,-50.8831977843865,
40.0606363359906));
#190169=CARTESIAN_POINT('Ctrl Pts',(-36.8040597645471,-50.8823495324294,
40.0552073017123));
#190170=CARTESIAN_POINT('Ctrl Pts',(-36.7953829494618,-50.8808651175411,
40.0494204304519));
#190171=CARTESIAN_POINT('Ctrl Pts',(-36.7870848098364,-50.878823144073,
40.0434049749851));
#190172=CARTESIAN_POINT('Ctrl Pts',(-36.7840533947862,-50.8780771854144,
40.0412074532442));
#190173=CARTESIAN_POINT('Ctrl Pts',(-36.7810676701179,-50.8772631333234,
40.0389814735788));
#190174=CARTESIAN_POINT('Ctrl Pts',(-36.7781294934921,-50.8763859670025,
40.0367321210016));
#190175=CARTESIAN_POINT('Ctrl Pts',(-36.7682604691151,-50.8734396581495,
40.0291767837149));
#190176=CARTESIAN_POINT('Ctrl Pts',(-36.7588677364097,-50.8697545265647,
40.0213235332593));
#190177=CARTESIAN_POINT('Ctrl Pts',(-36.7499455893946,-50.8654587487979,
40.0132649215884));
#190178=CARTESIAN_POINT('Ctrl Pts',(-36.7401390929271,-50.8607371801638,
40.0044075527568));
#190179=CARTESIAN_POINT('Ctrl Pts',(-36.7309004184199,-50.8552777667807,
39.9953016253764));
#190180=CARTESIAN_POINT('Ctrl Pts',(-36.7222305213381,-50.8491983060158,
39.9860353422412));
#190181=CARTESIAN_POINT('Ctrl Pts',(-36.7128926707054,-50.8426504662879,
39.9760551582758));
#190182=CARTESIAN_POINT('Ctrl Pts',(-36.7042135591923,-50.835382795217,
39.9658879738229));
#190183=CARTESIAN_POINT('Ctrl Pts',(-36.6962177694384,-50.8274903908739,
39.9556174643338));
#190184=CARTESIAN_POINT('Ctrl Pts',(-36.6883299498402,-50.8197045606343,
39.9454856413961));
#190185=CARTESIAN_POINT('Ctrl Pts',(-36.6811063421692,-50.8113095502238,
39.9352519465142));
#190186=CARTESIAN_POINT('Ctrl Pts',(-36.674605926818,-50.8023624960589,
39.92499));
#190187=CARTESIAN_POINT('Ctrl Pts',(-34.6525130919799,-48.0191904766735,
39.92499));
#190188=CARTESIAN_POINT('Ctrl Pts',(-34.6462921588072,-48.0106280967261,
39.9348107241715));
#190189=CARTESIAN_POINT('Ctrl Pts',(-34.6407689407928,-48.0016058360827,
39.9446038383155));
#190190=CARTESIAN_POINT('Ctrl Pts',(-34.6359660967504,-47.9921771448993,
39.9543158069363));
#190191=CARTESIAN_POINT('Ctrl Pts',(-34.6313285282544,-47.9830729139886,
39.9636935671366));
#190192=CARTESIAN_POINT('Ctrl Pts',(-34.6273621044928,-47.9735885825141,
39.972996832096));
#190193=CARTESIAN_POINT('Ctrl Pts',(-34.62412702213,-47.9637494987697,39.9821731151303));
#190194=CARTESIAN_POINT('Ctrl Pts',(-34.6210688561319,-47.9544484832207,
39.990847576432));
#190195=CARTESIAN_POINT('Ctrl Pts',(-34.6186639474984,-47.944829596451,
39.9994093733814));
#190196=CARTESIAN_POINT('Ctrl Pts',(-34.6170045862124,-47.934907676376,
40.007796611581));
#190197=CARTESIAN_POINT('Ctrl Pts',(-34.6154763423058,-47.9257697544393,
40.0155211172565));
#190198=CARTESIAN_POINT('Ctrl Pts',(-34.6145804463111,-47.9163742511105,
40.0230979940994));
#190199=CARTESIAN_POINT('Ctrl Pts',(-34.6144269453422,-47.9067364390682,
40.0304554104723));
#190200=CARTESIAN_POINT('Ctrl Pts',(-34.6143811744519,-47.903862638068,
40.0326492435164));
#190201=CARTESIAN_POINT('Ctrl Pts',(-34.6144016870566,-47.9009673483063,
40.0348233715052));
#190202=CARTESIAN_POINT('Ctrl Pts',(-34.6144921419176,-47.8980511519204,
40.0369753512356));
#190203=CARTESIAN_POINT('Ctrl Pts',(-34.6145816725529,-47.8951647518765,
40.0391053430352));
#190204=CARTESIAN_POINT('Ctrl Pts',(-34.6147393566953,-47.8922608568397,
40.041211089324));
#190205=CARTESIAN_POINT('Ctrl Pts',(-34.6149683234597,-47.8893433277783,
40.0432881154904));
#190206=CARTESIAN_POINT('Ctrl Pts',(-34.6149842453607,-47.8891404485132,
40.043432547828));
#190207=CARTESIAN_POINT('Ctrl Pts',(-34.6150005017597,-47.8889374970513,
40.0435768364421));
#190208=CARTESIAN_POINT('Ctrl Pts',(-34.6150170939191,-47.8887344737213,
40.0437209807855));
#190209=CARTESIAN_POINT('Ctrl Pts',(-34.6157445549671,-47.8798331871998,
40.0500407968419));
#190210=CARTESIAN_POINT('Ctrl Pts',(-34.6171603320595,-47.8708080647648,
40.0560490279343));
#190211=CARTESIAN_POINT('Ctrl Pts',(-34.6193291901737,-47.8617555581815,
40.0616647108613));
#190212=CARTESIAN_POINT('Ctrl Pts',(-34.6213509428811,-47.8533170487309,
40.0668995033483));
#190213=CARTESIAN_POINT('Ctrl Pts',(-34.6240275231021,-47.8448540540103,
40.0717933267478));
#190214=CARTESIAN_POINT('Ctrl Pts',(-34.6274308957715,-47.8364666369699,
40.0762460303069));
#190215=CARTESIAN_POINT('Ctrl Pts',(-34.6286758935244,-47.8333984113063,
40.0778748868745));
#190216=CARTESIAN_POINT('Ctrl Pts',(-34.6300183184512,-47.830340571385,
40.0794443522246));
#190217=CARTESIAN_POINT('Ctrl Pts',(-34.6314622582451,-47.8272990958128,
40.0809482021492));
#190218=CARTESIAN_POINT('Ctrl Pts',(-34.6318094775277,-47.8265677225445,
40.0813098278168));
#190219=CARTESIAN_POINT('Ctrl Pts',(-34.6321630753106,-47.8258370084446,
40.0816679525672));
#190220=CARTESIAN_POINT('Ctrl Pts',(-34.6325230544378,-47.8251070891647,
40.082022419258));
#190221=CARTESIAN_POINT('Ctrl Pts',(-34.6328717842173,-47.8243999798624,
40.0823658088648));
#190222=CARTESIAN_POINT('Ctrl Pts',(-34.6332265027182,-47.8236936164942,
40.0827057654616));
#190223=CARTESIAN_POINT('Ctrl Pts',(-34.6335872094466,-47.8229881245978,
40.0830421470151));
#190224=CARTESIAN_POINT('Ctrl Pts',(-34.6375391685163,-47.8152586455546,
40.0867275956806));
#190225=CARTESIAN_POINT('Ctrl Pts',(-34.6422128973066,-47.8076288798881,
40.0899823432031));
#190226=CARTESIAN_POINT('Ctrl Pts',(-34.6475865476014,-47.8002860619008,
40.0926299529356));
#190227=CARTESIAN_POINT('Ctrl Pts',(-34.6498151605499,-47.7972407764157,
40.0937279956084));
#190228=CARTESIAN_POINT('Ctrl Pts',(-34.6521637338117,-47.7942448304649,
40.0947220371802));
#190229=CARTESIAN_POINT('Ctrl Pts',(-34.654628954734,-47.7913110614418,
40.0956014538692));
#190230=CARTESIAN_POINT('Ctrl Pts',(-34.6588336459112,-47.7863072126524,
40.097101390674));
#190231=CARTESIAN_POINT('Ctrl Pts',(-34.6633779280161,-47.7814867201292,
40.0982667904316));
#190232=CARTESIAN_POINT('Ctrl Pts',(-34.6682420184009,-47.7769196237422,
40.0990539325582));
#190233=CARTESIAN_POINT('Ctrl Pts',(-34.6706740635933,-47.7746360755486,
40.0994475036216));
#190234=CARTESIAN_POINT('Ctrl Pts',(-34.6731869650545,-47.7724170058818,
40.0997467259952));
#190235=CARTESIAN_POINT('Ctrl Pts',(-34.6757782448035,-47.7702712352609,
40.0999473488896));
#190236=CARTESIAN_POINT('Ctrl Pts',(-34.6783695245525,-47.7681254646401,
40.100147971784));
#190237=CARTESIAN_POINT('Ctrl Pts',(-34.6810391382372,-47.7660530039192,
40.10025));
#190238=CARTESIAN_POINT('Ctrl Pts',(-34.6837837831348,-47.7640607692761,
40.10025));
#190239=CARTESIAN_POINT('Origin',(-38.9973987043321,-43.2882232241946,39.92499));
#190240=CARTESIAN_POINT('Ctrl Pts',(-42.0671296588098,-46.4355828792668,
39.92499));
#190241=CARTESIAN_POINT('Ctrl Pts',(-42.0742293550381,-46.4434678907494,
39.9348354642022));
#190242=CARTESIAN_POINT('Ctrl Pts',(-42.0806858315479,-46.4518896956744,
39.9446440828466));
#190243=CARTESIAN_POINT('Ctrl Pts',(-42.0864721532166,-46.4607957007324,
39.9543641760343));
#190244=CARTESIAN_POINT('Ctrl Pts',(-42.0920704538863,-46.4694123136578,
39.9637684240728));
#190245=CARTESIAN_POINT('Ctrl Pts',(-42.0970420880514,-46.4784832882822,
39.9730909636415));
#190246=CARTESIAN_POINT('Ctrl Pts',(-42.1013257711398,-46.4879887958193,
39.9822808977163));
#190247=CARTESIAN_POINT('Ctrl Pts',(-42.1053778715674,-46.4969804206339,
39.9909740094675));
#190248=CARTESIAN_POINT('Ctrl Pts',(-42.1088147776131,-46.5063617095252,
39.999549276503));
#190249=CARTESIAN_POINT('Ctrl Pts',(-42.1115441100131,-46.5161273793256,
40.0079462328726));
#190250=CARTESIAN_POINT('Ctrl Pts',(-42.1140580225438,-46.5251222674832,
40.0156804369724));
#190251=CARTESIAN_POINT('Ctrl Pts',(-42.115971744702,-46.5344438074352,
40.023263801746));
#190252=CARTESIAN_POINT('Ctrl Pts',(-42.1171748456141,-46.544088490823,
40.0306257270007));
#190253=CARTESIAN_POINT('Ctrl Pts',(-42.1175238194552,-46.5468860468499,
40.0327611416679));
#190254=CARTESIAN_POINT('Ctrl Pts',(-42.1178127362982,-46.5497107674243,
40.0348777427284));
#190255=CARTESIAN_POINT('Ctrl Pts',(-42.1180382068977,-46.552562480084,
40.0369733168701));
#190256=CARTESIAN_POINT('Ctrl Pts',(-42.118282631524,-46.5556539199572,
40.039245053974));
#190257=CARTESIAN_POINT('Ctrl Pts',(-42.1184532289194,-46.5587726948497,
40.041487875195));
#190258=CARTESIAN_POINT('Ctrl Pts',(-42.1185461584681,-46.5619176830192,
40.0436985701601));
#190259=CARTESIAN_POINT('Ctrl Pts',(-42.1188012043436,-46.5705491277287,
40.0497658398386));
#190260=CARTESIAN_POINT('Ctrl Pts',(-42.1184278543823,-46.579368264381,
40.0555581699984));
#190261=CARTESIAN_POINT('Ctrl Pts',(-42.1173773384969,-46.5882835699002,
40.0609828468886));
#190262=CARTESIAN_POINT('Ctrl Pts',(-42.1164161734956,-46.5964405904272,
40.0659461317305));
#190263=CARTESIAN_POINT('Ctrl Pts',(-42.1148801579478,-46.604669732884,
40.0706039980707));
#190264=CARTESIAN_POINT('Ctrl Pts',(-42.1127009621828,-46.6129145292184,
40.0748843180604));
#190265=CARTESIAN_POINT('Ctrl Pts',(-42.1116305483418,-46.616964346245,
40.076986797257));
#190266=CARTESIAN_POINT('Ctrl Pts',(-42.1104045383079,-46.6210176421364,
40.0789976708175));
#190267=CARTESIAN_POINT('Ctrl Pts',(-42.109012387551,-46.6250654385591,
40.08090504915));
#190268=CARTESIAN_POINT('Ctrl Pts',(-42.1087482405046,-46.6258334685042,
40.0812669556105));
#190269=CARTESIAN_POINT('Ctrl Pts',(-42.108477638333,-46.6266015422612,
40.0816253922033));
#190270=CARTESIAN_POINT('Ctrl Pts',(-42.1082005605487,-46.6273695213204,
40.0819801989139));
#190271=CARTESIAN_POINT('Ctrl Pts',(-42.1079321414451,-46.628113501034,
40.0823239179149));
#190272=CARTESIAN_POINT('Ctrl Pts',(-42.1076576451502,-46.6288573918595,
40.0826642303498));
#190273=CARTESIAN_POINT('Ctrl Pts',(-42.1073770559081,-46.6296010653158,
40.0830009916099));
#190274=CARTESIAN_POINT('Ctrl Pts',(-42.1043192521647,-46.6377054654049,
40.0866709464312));
#190275=CARTESIAN_POINT('Ctrl Pts',(-42.1005354505675,-46.645789240007,
40.0899175831877));
#190276=CARTESIAN_POINT('Ctrl Pts',(-42.0960238460772,-46.6536619390761,
40.0925642067062));
#190277=CARTESIAN_POINT('Ctrl Pts',(-42.0941185674852,-46.65698662878,40.0936818922527));
#190278=CARTESIAN_POINT('Ctrl Pts',(-42.0920839261385,-46.660273639941,
40.094693009479));
#190279=CARTESIAN_POINT('Ctrl Pts',(-42.0899216923181,-46.6635089796842,
40.0955863397546));
#190280=CARTESIAN_POINT('Ctrl Pts',(-42.0862805445927,-46.6689572109693,
40.0970906856166));
#190281=CARTESIAN_POINT('Ctrl Pts',(-42.0822770520158,-46.6742564366674,
40.0982599215483));
#190282=CARTESIAN_POINT('Ctrl Pts',(-42.0779224130575,-46.679333290145,
40.0990497370454));
#190283=CARTESIAN_POINT('Ctrl Pts',(-42.0768337533179,-46.6806025035144,
40.0992471909196));
#190284=CARTESIAN_POINT('Ctrl Pts',(-42.0757229796949,-46.6818576549905,
40.0994209989363));
#190285=CARTESIAN_POINT('Ctrl Pts',(-42.0745900553979,-46.6830973739111,
40.0995705982975));
#190286=CARTESIAN_POINT('Ctrl Pts',(-42.0728906689524,-46.6849569522919,
40.0997949973393));
#190287=CARTESIAN_POINT('Ctrl Pts',(-42.0711414461006,-46.686781786976,
40.0999649129781));
#190288=CARTESIAN_POINT('Ctrl Pts',(-42.0693433991611,-46.6885684866732,
40.1000786629733));
#190289=CARTESIAN_POINT('Ctrl Pts',(-42.0675453522215,-46.6903551863704,
40.1001924129685));
#190290=CARTESIAN_POINT('Ctrl Pts',(-42.0656984926178,-46.6921037531361,
40.10025));
#190291=CARTESIAN_POINT('Ctrl Pts',(-42.0638038389714,-46.6938111422615,
40.10025));
#190292=CARTESIAN_POINT('Ctrl Pts',(-39.5091373124624,-43.8565665267054,
40.10025));
#190293=CARTESIAN_POINT('Ctrl Pts',(-39.5155480799606,-43.8507890749204,
40.10025));
#190294=CARTESIAN_POINT('Ctrl Pts',(-39.5223801852472,-43.8455908828145,
40.099578633424));
#190295=CARTESIAN_POINT('Ctrl Pts',(-39.5294841269576,-43.8409939475737,
40.0983063763364));
#190296=CARTESIAN_POINT('Ctrl Pts',(-39.5340725443954,-43.8380247990812,
40.0974846287991));
#190297=CARTESIAN_POINT('Ctrl Pts',(-39.5387738681337,-43.8353056940457,
40.0964130309337));
#190298=CARTESIAN_POINT('Ctrl Pts',(-39.5435446222366,-43.8328343017435,
40.0951176960924));
#190299=CARTESIAN_POINT('Ctrl Pts',(-39.5498679835146,-43.8295586128167,
40.0934008039614));
#190300=CARTESIAN_POINT('Ctrl Pts',(-39.5563148866445,-43.826723686506,
40.0912909372156));
#190301=CARTESIAN_POINT('Ctrl Pts',(-39.5627952650342,-43.8243293609622,
40.0888630467851));
#190302=CARTESIAN_POINT('Ctrl Pts',(-39.566035454229,-43.8231321981903,
40.0876491015699));
#190303=CARTESIAN_POINT('Ctrl Pts',(-39.5692841591688,-43.8220450509624,
40.0863558569271));
#190304=CARTESIAN_POINT('Ctrl Pts',(-39.5725311673657,-43.8210669472517,
40.0849936342771));
#190305=CARTESIAN_POINT('Ctrl Pts',(-39.5741546714642,-43.8205778953963,
40.0843125229521));
#190306=CARTESIAN_POINT('Ctrl Pts',(-39.5757777635549,-43.8201160933894,
40.0836141747074));
#190307=CARTESIAN_POINT('Ctrl Pts',(-39.5773992434497,-43.8196813503777,
40.082899916161));
#190308=CARTESIAN_POINT('Ctrl Pts',(-39.5778046134234,-43.8195726646248,
40.0827213515243));
#190309=CARTESIAN_POINT('Ctrl Pts',(-39.5782098828931,-43.8194656698237,
40.0825417925842));
#190310=CARTESIAN_POINT('Ctrl Pts',(-39.5786150336268,-43.8193603625174,
40.0823612602361));
#190311=CARTESIAN_POINT('Ctrl Pts',(-39.5798304858278,-43.8190444405983,
40.0818196631917));
#190312=CARTESIAN_POINT('Ctrl Pts',(-39.5810448681191,-43.8187437073122,
40.0812693052022));
#190313=CARTESIAN_POINT('Ctrl Pts',(-39.5822576997163,-43.81845805878,40.0807107531875));
#190314=CARTESIAN_POINT('Ctrl Pts',(-39.5908007288818,-43.8164459874032,
40.076776384918));
#190315=CARTESIAN_POINT('Ctrl Pts',(-39.5992865061397,-43.8151322889028,
40.0724140586133));
#190316=CARTESIAN_POINT('Ctrl Pts',(-39.6076412948847,-43.8144227306309,
40.0677221223761));
#190317=CARTESIAN_POINT('Ctrl Pts',(-39.6116933583972,-43.8140785956357,
40.0654465383716));
#190318=CARTESIAN_POINT('Ctrl Pts',(-39.6157150281166,-43.8138769687218,
40.0630928000677));
#190319=CARTESIAN_POINT('Ctrl Pts',(-39.6196997093544,-43.8138093098902,
40.0606689262479));
#190320=CARTESIAN_POINT('Ctrl Pts',(-39.6257999779283,-43.8137057289462,
40.0569581447806));
#190321=CARTESIAN_POINT('Ctrl Pts',(-39.6318101761582,-43.8139151128798,
40.0530843804606));
#190322=CARTESIAN_POINT('Ctrl Pts',(-39.6376940219322,-43.8144090029876,
40.0490800251458));
#190323=CARTESIAN_POINT('Ctrl Pts',(-39.6404265103486,-43.8146383681088,
40.0472203818218));
#190324=CARTESIAN_POINT('Ctrl Pts',(-39.6431316855283,-43.8149288459965,
40.0453323608818));
#190325=CARTESIAN_POINT('Ctrl Pts',(-39.6458055463963,-43.8152787628651,
40.0434201572162));
#190326=CARTESIAN_POINT('Ctrl Pts',(-39.6460104872963,-43.8153055826144,
40.0432735943397));
#190327=CARTESIAN_POINT('Ctrl Pts',(-39.6462152612035,-43.8153327221692,
40.0431268995707));
#190328=CARTESIAN_POINT('Ctrl Pts',(-39.6464198673376,-43.8153601802952,
40.0429800745037));
#190329=CARTESIAN_POINT('Ctrl Pts',(-39.6492939666538,-43.8157458841822,
40.0409176249753));
#190330=CARTESIAN_POINT('Ctrl Pts',(-39.6521348180507,-43.8161965332332,
40.0388310783333));
#190331=CARTESIAN_POINT('Ctrl Pts',(-39.654938997009,-43.8167075634908,
40.036725739981));
#190332=CARTESIAN_POINT('Ctrl Pts',(-39.6649942840467,-43.8185400271109,
40.0291763710718));
#190333=CARTESIAN_POINT('Ctrl Pts',(-39.6746561192247,-43.8211611138368,
40.0213310894594));
#190334=CARTESIAN_POINT('Ctrl Pts',(-39.6839173731634,-43.8244418968099,
40.0132837551319));
#190335=CARTESIAN_POINT('Ctrl Pts',(-39.6940945608669,-43.8280471477135,
40.0044405431322));
#190336=CARTESIAN_POINT('Ctrl Pts',(-39.7037886794679,-43.8324491002312,
39.9953528710595));
#190337=CARTESIAN_POINT('Ctrl Pts',(-39.7129876499617,-43.8375295667873,
39.9861103629547));
#190338=CARTESIAN_POINT('Ctrl Pts',(-39.7229202294689,-43.843015195645,
39.9761307737539));
#190339=CARTESIAN_POINT('Ctrl Pts',(-39.7322766233322,-43.8492922888427,
39.9659696935986));
#190340=CARTESIAN_POINT('Ctrl Pts',(-39.7410245486316,-43.8562669044117,
39.9557128217472));
#190341=CARTESIAN_POINT('Ctrl Pts',(-39.7496990878245,-43.8631830101212,
39.9455419945137));
#190342=CARTESIAN_POINT('Ctrl Pts',(-39.7577762496647,-43.8707860819069,
39.9352756289329));
#190343=CARTESIAN_POINT('Ctrl Pts',(-39.7651933659001,-43.8790236240218,
39.92499));
#190344=CARTESIAN_POINT('Origin',(0.0113255271402848,-0.0101975504409049,
39.92499));
#190345=CARTESIAN_POINT('Ctrl Pts',(-42.0411527846897,-46.714206243142,
40.10025));
#190346=CARTESIAN_POINT('Ctrl Pts',(-42.0347675597394,-46.7199506919421,
40.10025));
#190347=CARTESIAN_POINT('Ctrl Pts',(-42.0279592142787,-46.7251107020204,
40.0995859581842));
#190348=CARTESIAN_POINT('Ctrl Pts',(-42.0208774479597,-46.7296675019384,
40.0983275959623));
#190349=CARTESIAN_POINT('Ctrl Pts',(-42.0163525364106,-46.7325790801588,
40.097523562407));
#190350=CARTESIAN_POINT('Ctrl Pts',(-42.0117164852005,-46.7352451892135,
40.0964777059492));
#190351=CARTESIAN_POINT('Ctrl Pts',(-42.0070114066749,-46.737668963875,
40.0952149915962));
#190352=CARTESIAN_POINT('Ctrl Pts',(-42.00058991857,-46.7409769299533,40.0934916398702));
#190353=CARTESIAN_POINT('Ctrl Pts',(-41.994038348078,-46.7438276087418,
40.0913643921631));
#190354=CARTESIAN_POINT('Ctrl Pts',(-41.9874523371583,-46.7462229640886,
40.0889118607714));
#190355=CARTESIAN_POINT('Ctrl Pts',(-41.9841593316985,-46.747420641762,
40.0876855950755));
#190356=CARTESIAN_POINT('Ctrl Pts',(-41.9808575622225,-46.7485046297345,
40.0863782327527));
#190357=CARTESIAN_POINT('Ctrl Pts',(-41.977557880152,-46.7494761782931,
40.0850006373334));
#190358=CARTESIAN_POINT('Ctrl Pts',(-41.9759080391167,-46.7499619525724,
40.0843118396238));
#190359=CARTESIAN_POINT('Ctrl Pts',(-41.9742587070257,-46.7504196286879,
40.0836054919165));
#190360=CARTESIAN_POINT('Ctrl Pts',(-41.9726111592841,-46.7508494364811,
40.0828829920418));
#190361=CARTESIAN_POINT('Ctrl Pts',(-41.9721992723487,-46.7509568884294,
40.0827023670732));
#190362=CARTESIAN_POINT('Ctrl Pts',(-41.9717874966609,-46.7510625988573,
40.0825207326933));
#190363=CARTESIAN_POINT('Ctrl Pts',(-41.971375851596,-46.7511665718604,
40.0823381109276));
#190364=CARTESIAN_POINT('Ctrl Pts',(-41.9701409164013,-46.7514784908697,
40.0817902456304));
#190365=CARTESIAN_POINT('Ctrl Pts',(-41.968907158177,-46.7517747718022,
40.0812334935554));
#190366=CARTESIAN_POINT('Ctrl Pts',(-41.9676750878621,-46.7520555364231,
40.0806684524227));
#190367=CARTESIAN_POINT('Ctrl Pts',(-41.9591607175413,-46.7539957941552,
40.0767636676137));
#190368=CARTESIAN_POINT('Ctrl Pts',(-41.9507055072913,-46.7552464720207,
40.0724404510887));
#190369=CARTESIAN_POINT('Ctrl Pts',(-41.9423805287162,-46.7559027543579,
40.0677949937407));
#190370=CARTESIAN_POINT('Ctrl Pts',(-41.9382430372163,-46.756228924878,
40.0654862141904));
#190371=CARTESIAN_POINT('Ctrl Pts',(-41.9341372814968,-46.7564078446194,
40.0630972003215));
#190372=CARTESIAN_POINT('Ctrl Pts',(-41.9300700339485,-46.7564487173141,
40.0606363359906));
#190373=CARTESIAN_POINT('Ctrl Pts',(-41.9210970783571,-46.7565388885837,
40.0552073017124));
#190374=CARTESIAN_POINT('Ctrl Pts',(-41.9123126321655,-46.7559695796223,
40.0494204304519));
#190375=CARTESIAN_POINT('Ctrl Pts',(-41.9038465062686,-46.7548061840815,
40.0434049749851));
#190376=CARTESIAN_POINT('Ctrl Pts',(-41.900753723715,-46.7543811810193,
40.0412074532442));
#190377=CARTESIAN_POINT('Ctrl Pts',(-41.8976992635448,-46.7538836816022,
40.0389814735788));
#190378=CARTESIAN_POINT('Ctrl Pts',(-41.8946854937103,-46.7533184435776,
40.0367321210016));
#190379=CARTESIAN_POINT('Ctrl Pts',(-41.8845625597436,-46.7514198688647,
40.029176783714));
#190380=CARTESIAN_POINT('Ctrl Pts',(-41.8748360802682,-46.7487367327316,
40.0213235332574));
#190381=CARTESIAN_POINT('Ctrl Pts',(-41.8655137786585,-46.7453971060009,
40.0132649215856));
#190382=CARTESIAN_POINT('Ctrl Pts',(-41.8552674648902,-46.741726460619,
40.0044075527529));
#190383=CARTESIAN_POINT('Ctrl Pts',(-41.8455087367165,-46.7372626589218,
39.9953016253715));
#190384=CARTESIAN_POINT('Ctrl Pts',(-41.836250857546,-46.732122753097,39.9860353422352));
#190385=CARTESIAN_POINT('Ctrl Pts',(-41.8262797250108,-46.7265868542962,
39.9760551582687));
#190386=CARTESIAN_POINT('Ctrl Pts',(-41.8168884800893,-46.7202662104758,
39.9658879738146));
#190387=CARTESIAN_POINT('Ctrl Pts',(-41.8081115112103,-46.7132528291638,
39.9556174643242));
#190388=CARTESIAN_POINT('Ctrl Pts',(-41.799453061046,-46.7063341521797,
39.9454856413897));
#190389=CARTESIAN_POINT('Ctrl Pts',(-41.791391507519,-46.6987402031258,
39.9352519465109));
#190390=CARTESIAN_POINT('Ctrl Pts',(-41.7839914803029,-46.6905216402895,
39.92499));
#190391=CARTESIAN_POINT('Ctrl Pts',(-39.4820551873932,-44.1339623850445,
39.92499));
#190392=CARTESIAN_POINT('Ctrl Pts',(-39.4749733207259,-44.1260971752955,
39.934810724171));
#190393=CARTESIAN_POINT('Ctrl Pts',(-39.4685372764378,-44.1177016730317,
39.9446038383145));
#190394=CARTESIAN_POINT('Ctrl Pts',(-39.4627751762777,-44.1088266671127,
39.9543158069348));
#190395=CARTESIAN_POINT('Ctrl Pts',(-39.4572113616012,-44.1002570680403,
39.9636935671346));
#190396=CARTESIAN_POINT('Ctrl Pts',(-39.45227528373,-44.091239296907,39.9729968320934));
#190397=CARTESIAN_POINT('Ctrl Pts',(-39.4480294591832,-44.0817922708815,
39.9821731151272));
#190398=CARTESIAN_POINT('Ctrl Pts',(-39.4440158252765,-44.0728618726619,
39.9908475764281));
#190399=CARTESIAN_POINT('Ctrl Pts',(-39.4406186435318,-44.0635470605651,
39.9994093733768));
#190400=CARTESIAN_POINT('Ctrl Pts',(-39.4379312493424,-44.0538529442926,
40.0077966115757));
#190401=CARTESIAN_POINT('Ctrl Pts',(-39.4354562043783,-44.0449248258367,
40.0155211172504));
#190402=CARTESIAN_POINT('Ctrl Pts',(-39.4335831186709,-44.0356744386912,
40.0230979940924));
#190403=CARTESIAN_POINT('Ctrl Pts',(-39.4324230329139,-44.0261054688135,
40.0304554104645));
#190404=CARTESIAN_POINT('Ctrl Pts',(-39.4320771187584,-44.0232521951534,
40.0326492435113));
#190405=CARTESIAN_POINT('Ctrl Pts',(-39.431794878803,-44.0203706219375,
40.0348233715027));
#190406=CARTESIAN_POINT('Ctrl Pts',(-39.4315800126158,-44.0174609456694,
40.0369753512356));
#190407=CARTESIAN_POINT('Ctrl Pts',(-39.4313673418319,-44.0145809991273,
40.0391053430352));
#190408=CARTESIAN_POINT('Ctrl Pts',(-39.4312206224785,-44.0116765294503,
40.041211089324));
#190409=CARTESIAN_POINT('Ctrl Pts',(-39.4311433701096,-44.0087510493743,
40.0432881154904));
#190410=CARTESIAN_POINT('Ctrl Pts',(-39.431137998131,-44.0085476172112,
40.043432547828));
#190411=CARTESIAN_POINT('Ctrl Pts',(-39.4311329512713,-44.0083440782822,
40.0435768364421));
#190412=CARTESIAN_POINT('Ctrl Pts',(-39.4311282308204,-44.0081404327823,
40.0437209807855));
#190413=CARTESIAN_POINT('Ctrl Pts',(-39.4309212689595,-43.9992118680545,
40.0500407968419));
#190414=CARTESIAN_POINT('Ctrl Pts',(-39.4313859080978,-43.9900881971809,
40.0560490279341));
#190415=CARTESIAN_POINT('Ctrl Pts',(-39.4325966403785,-43.9808585737702,
40.061664710861));
#190416=CARTESIAN_POINT('Ctrl Pts',(-39.4337252532878,-43.9722549606539,
40.0668995033479));
#190417=CARTESIAN_POINT('Ctrl Pts',(-39.4355025470894,-43.9635585482867,
40.0717933267474));
#190418=CARTESIAN_POINT('Ctrl Pts',(-39.4380105519132,-43.9548613290796,
40.0762460303063));
#190419=CARTESIAN_POINT('Ctrl Pts',(-39.4389280125246,-43.951679773775,
40.0778748868742));
#190420=CARTESIAN_POINT('Ctrl Pts',(-39.4399434521993,-43.9484983634058,
40.0794443522244));
#190421=CARTESIAN_POINT('Ctrl Pts',(-39.4410615611725,-43.945322616547,
40.0809482021491));
#190422=CARTESIAN_POINT('Ctrl Pts',(-39.4413304290278,-43.9445589555199,
40.0813098278168));
#190423=CARTESIAN_POINT('Ctrl Pts',(-39.441605709343,-43.9437952833154,
40.0816679525671));
#190424=CARTESIAN_POINT('Ctrl Pts',(-39.4418874191263,-43.9430317345448,
40.082022419258));
#190425=CARTESIAN_POINT('Ctrl Pts',(-39.4421603254788,-43.9422920466732,
40.0823658088647));
#190426=CARTESIAN_POINT('Ctrl Pts',(-39.4424392657172,-43.9415524746577,
40.0827057654616));
#190427=CARTESIAN_POINT('Ctrl Pts',(-39.4427242524727,-43.9408131433997,
40.083042147015));
#190428=CARTESIAN_POINT('Ctrl Pts',(-39.4458466117312,-43.9327129150422,
40.086727595681));
#190429=CARTESIAN_POINT('Ctrl Pts',(-39.4496972096663,-43.9246364083414,
40.0899823432037));
#190430=CARTESIAN_POINT('Ctrl Pts',(-39.4542738890629,-43.9167721156712,
40.0926299529364));
#190431=CARTESIAN_POINT('Ctrl Pts',(-39.4561719744242,-43.9135105590926,
40.0937279956089));
#190432=CARTESIAN_POINT('Ctrl Pts',(-39.4581945203291,-43.9102855324941,
40.0947220371804));
#190433=CARTESIAN_POINT('Ctrl Pts',(-39.4603395741452,-43.9071101492107,
40.0956014538692));
#190434=CARTESIAN_POINT('Ctrl Pts',(-39.4639981869599,-43.9016942021213,
40.097101390674));
#190435=CARTESIAN_POINT('Ctrl Pts',(-39.4680136963363,-43.8964251099355,
40.0982667904316));
#190436=CARTESIAN_POINT('Ctrl Pts',(-39.472373749158,-43.8913745966872,
40.0990539325582));
#190437=CARTESIAN_POINT('Ctrl Pts',(-39.4745537755689,-43.888849340063,
40.0994475036216));
#190438=CARTESIAN_POINT('Ctrl Pts',(-39.4768209551509,-43.8863797569639,
40.0997467259952));
#190439=CARTESIAN_POINT('Ctrl Pts',(-39.4791737454928,-43.883974878609,
40.0999473488896));
#190440=CARTESIAN_POINT('Ctrl Pts',(-39.4815265358346,-43.8815700002541,
40.100147971784));
#190441=CARTESIAN_POINT('Ctrl Pts',(-39.4839648939619,-43.8792298420739,
40.10025));
#190442=CARTESIAN_POINT('Ctrl Pts',(-39.4864862581819,-43.8769616275872,
40.10025));
#190443=CARTESIAN_POINT('Origin',(-43.3086183250768,-38.9747476500511,39.92499));
#190444=CARTESIAN_POINT('Ctrl Pts',(-46.6905216402899,-41.7839914803024,
39.92499));
#190445=CARTESIAN_POINT('Ctrl Pts',(-46.6984066517724,-41.7910911765306,
39.9348354642025));
#190446=CARTESIAN_POINT('Ctrl Pts',(-46.705708077355,-41.7987919603592,
39.944644082847));
#190447=CARTESIAN_POINT('Ctrl Pts',(-46.7123936319708,-41.8070443420777,
39.9543641760349));
#190448=CARTESIAN_POINT('Ctrl Pts',(-46.7188619458713,-41.81502857053,39.9637684240734));
#190449=CARTESIAN_POINT('Ctrl Pts',(-46.7247545199422,-41.8235301761272,
39.9730909636421));
#190450=CARTESIAN_POINT('Ctrl Pts',(-46.7300083326618,-41.8325358446891,
39.9822808977169));
#190451=CARTESIAN_POINT('Ctrl Pts',(-46.7349781159835,-41.8410546526115,
39.9909740094681));
#190452=CARTESIAN_POINT('Ctrl Pts',(-46.7393768060097,-41.8500252953134,
39.9995492765035));
#190453=CARTESIAN_POINT('Ctrl Pts',(-46.7431119772982,-41.8594521748314,
40.007946232873));
#190454=CARTESIAN_POINT('Ctrl Pts',(-46.7465523401894,-41.8681350126368,
40.0156804369727));
#190455=CARTESIAN_POINT('Ctrl Pts',(-46.7494299450239,-41.8772054497814,
40.0232638017462));
#190456=CARTESIAN_POINT('Ctrl Pts',(-46.7516345991566,-41.8866715402948,
40.0306257270008));
#190457=CARTESIAN_POINT('Ctrl Pts',(-46.7522740855148,-41.8894172933178,
40.0327611416679));
#190458=CARTESIAN_POINT('Ctrl Pts',(-46.752856683342,-41.8921963397437,
40.0348777427285));
#190459=CARTESIAN_POINT('Ctrl Pts',(-46.7533790039318,-41.8950088623277,
40.0369733168701));
#190460=CARTESIAN_POINT('Ctrl Pts',(-46.7539452330337,-41.8980578176393,
40.0392450539741));
#190461=CARTESIAN_POINT('Ctrl Pts',(-46.7544408966255,-41.9011416752731,
40.0414878751951));
#190462=CARTESIAN_POINT('Ctrl Pts',(-46.7548620578768,-41.9042597210854,
40.0436985701601));
#190463=CARTESIAN_POINT('Ctrl Pts',(-46.7560179382356,-41.9128172222842,
40.0497658398386));
#190464=CARTESIAN_POINT('Ctrl Pts',(-46.756568484326,-41.9216270724808,
40.0555581699984));
#190465=CARTESIAN_POINT('Ctrl Pts',(-46.756455626462,-41.9306033478348,
40.0609828468886));
#190466=CARTESIAN_POINT('Ctrl Pts',(-46.7563523676437,-41.9388161524504,
40.0659461317305));
#190467=CARTESIAN_POINT('Ctrl Pts',(-46.7556849461648,-41.9471607721487,
40.0706039980708));
#190468=CARTESIAN_POINT('Ctrl Pts',(-46.754379504153,-41.9555881906108,
40.0748843180606));
#190469=CARTESIAN_POINT('Ctrl Pts',(-46.7537382753013,-41.9597277110297,
40.0769867972571));
#190470=CARTESIAN_POINT('Ctrl Pts',(-46.7529426662694,-41.9638869554867,
40.0789976708176));
#190471=CARTESIAN_POINT('Ctrl Pts',(-46.7519812517997,-41.9680580970362,
40.08090504915));
#190472=CARTESIAN_POINT('Ctrl Pts',(-46.7517988327683,-41.9688495305178,
40.0812669556105));
#190473=CARTESIAN_POINT('Ctrl Pts',(-46.7516099985532,-41.9696416823156,
40.0816253922033));
#190474=CARTESIAN_POINT('Ctrl Pts',(-46.7514147143009,-41.9704344168201,
40.0819801989139));
#190475=CARTESIAN_POINT('Ctrl Pts',(-46.7512255326815,-41.9712023783714,
40.0823239179149));
#190476=CARTESIAN_POINT('Ctrl Pts',(-46.7510302978708,-41.971970886761,
40.0826642303498));
#190477=CARTESIAN_POINT('Ctrl Pts',(-46.7508289807695,-41.9727398158586,
40.0830009916099));
#190478=CARTESIAN_POINT('Ctrl Pts',(-46.7486350684819,-41.9811194467225,
40.0866709464313));
#190479=CARTESIAN_POINT('Ctrl Pts',(-46.7457169794822,-41.9895544525281,
40.0899175831879));
#190480=CARTESIAN_POINT('Ctrl Pts',(-46.7420530111687,-41.9978556152123,
40.0925642067064));
#190481=CARTESIAN_POINT('Ctrl Pts',(-46.7405056945978,-42.0013612477613,
40.0936818922529));
#190482=CARTESIAN_POINT('Ctrl Pts',(-46.7388257854549,-42.0048429302643,
40.0946930094791));
#190483=CARTESIAN_POINT('Ctrl Pts',(-46.7370135816691,-42.0082865614561,
40.0955863397546));
#190484=CARTESIAN_POINT('Ctrl Pts',(-46.7339618757758,-42.0140855503364,
40.0970906856166));
#190485=CARTESIAN_POINT('Ctrl Pts',(-46.7305342346688,-42.0197742252484,
40.0982599215483));
#190486=CARTESIAN_POINT('Ctrl Pts',(-46.7267341265708,-42.02527845091,40.0990497370454));
#190487=CARTESIAN_POINT('Ctrl Pts',(-46.7257840995463,-42.0266545073254,
40.0992471909196));
#190488=CARTESIAN_POINT('Ctrl Pts',(-46.7248106099124,-42.0280188904103,
40.0994209989363));
#190489=CARTESIAN_POINT('Ctrl Pts',(-46.7238134778068,-42.0293702408566,
40.0995705982975));
#190490=CARTESIAN_POINT('Ctrl Pts',(-46.7223177796485,-42.0313972665261,
40.0997949973393));
#190491=CARTESIAN_POINT('Ctrl Pts',(-46.7207688863877,-42.0333949481515,
40.0999649129781));
#190492=CARTESIAN_POINT('Ctrl Pts',(-46.7191674503111,-42.0353598072042,
40.1000786629733));
#190493=CARTESIAN_POINT('Ctrl Pts',(-46.7175660142345,-42.037324666257,
40.1001924129685));
#190494=CARTESIAN_POINT('Ctrl Pts',(-46.7159120469165,-42.039256703586,
40.10025));
#190495=CARTESIAN_POINT('Ctrl Pts',(-46.7142062431425,-42.0411527846892,
40.10025));
#190496=CARTESIAN_POINT('Ctrl Pts',(-43.8769616275876,-39.4864862581814,
40.10025));
#190497=CARTESIAN_POINT('Ctrl Pts',(-43.8827333680735,-39.4800703482075,
40.10025));
#190498=CARTESIAN_POINT('Ctrl Pts',(-43.8889846873392,-39.4741864828759,
40.0995786334241));
#190499=CARTESIAN_POINT('Ctrl Pts',(-43.8955692023364,-39.4688721660176,
40.0983063763368));
#190500=CARTESIAN_POINT('Ctrl Pts',(-43.8998221234149,-39.465439662607,
40.0974846287994));
#190501=CARTESIAN_POINT('Ctrl Pts',(-43.9042134689397,-39.4622440309671,
40.0964130309339));
#190502=CARTESIAN_POINT('Ctrl Pts',(-43.9086997575136,-39.4592874976151,
40.0951176960923));
#190503=CARTESIAN_POINT('Ctrl Pts',(-43.9146460760273,-39.4553687820179,
40.0934008039614));
#190504=CARTESIAN_POINT('Ctrl Pts',(-43.9207613318565,-39.4518755008531,
40.0912909372156));
#190505=CARTESIAN_POINT('Ctrl Pts',(-43.9269559348856,-39.4488169076807,
40.0888630467851));
#190506=CARTESIAN_POINT('Ctrl Pts',(-43.9300532364002,-39.4472876110945,
40.0876491015699));
#190507=CARTESIAN_POINT('Ctrl Pts',(-43.9331705067654,-39.445866837238,
40.0863558569271));
#190508=CARTESIAN_POINT('Ctrl Pts',(-43.9362974878338,-39.4445546869046,
40.0849936342771));
#190509=CARTESIAN_POINT('Ctrl Pts',(-43.937860978368,-39.443898611738,40.0843125229521));
#190510=CARTESIAN_POINT('Ctrl Pts',(-43.9394269075363,-39.4432696802088,
40.0836141747074));
#190511=CARTESIAN_POINT('Ctrl Pts',(-43.9409940617757,-39.4426678279632,
40.082899916161));
#190512=CARTESIAN_POINT('Ctrl Pts',(-43.9413858503355,-39.4425173649018,
40.0827213515243));
#190513=CARTESIAN_POINT('Ctrl Pts',(-43.9417777156946,-39.4423685940346,
40.0825417925842));
#190514=CARTESIAN_POINT('Ctrl Pts',(-43.9421696393592,-39.4422215138291,
40.0823612602361));
#190515=CARTESIAN_POINT('Ctrl Pts',(-43.9433454103532,-39.4417802732126,
40.0818196631917));
#190516=CARTESIAN_POINT('Ctrl Pts',(-43.944521704943,-39.4413542498602,
40.0812693052022));
#190517=CARTESIAN_POINT('Ctrl Pts',(-43.9456980341197,-39.4409433907175,
40.0807107531875));
#190518=CARTESIAN_POINT('Ctrl Pts',(-43.9539839449482,-39.438049351968,
40.0767763849181));
#190519=CARTESIAN_POINT('Ctrl Pts',(-43.9622859173447,-39.4358558447891,
40.0724140586136));
#190520=CARTESIAN_POINT('Ctrl Pts',(-43.9705207686468,-39.4342768603232,
40.0677221223766));
#190521=CARTESIAN_POINT('Ctrl Pts',(-43.9745146626295,-39.4335110545635,
40.0654465383719));
#190522=CARTESIAN_POINT('Ctrl Pts',(-43.9784932254702,-39.4328901532272,
40.0630928000678));
#190523=CARTESIAN_POINT('Ctrl Pts',(-43.9824490059338,-39.4324063524313,
40.0606689262479));
#190524=CARTESIAN_POINT('Ctrl Pts',(-43.9885050294413,-39.4316656872151,
40.0569581447805));
#190525=CARTESIAN_POINT('Ctrl Pts',(-43.9945041897573,-39.4312456873366,
40.0530843804606));
#190526=CARTESIAN_POINT('Ctrl Pts',(-44.0004074287824,-39.431121842506,
40.0490800251458));
#190527=CARTESIAN_POINT('Ctrl Pts',(-44.003148923525,-39.4310643283259,
40.0472203818218));
#190528=CARTESIAN_POINT('Ctrl Pts',(-44.0058696426793,-39.431070447141,
40.0453323608819));
#190529=CARTESIAN_POINT('Ctrl Pts',(-44.0085654321302,-39.4311389525609,
40.0434201572162));
#190530=CARTESIAN_POINT('Ctrl Pts',(-44.0087720537697,-39.4311442032314,
40.0432735943397));
#190531=CARTESIAN_POINT('Ctrl Pts',(-44.00897854276,-39.4311497894111,40.0431268995707));
#190532=CARTESIAN_POINT('Ctrl Pts',(-44.009184898196,-39.4311557099538,
40.0429800745037));
#190533=CARTESIAN_POINT('Ctrl Pts',(-44.01208356993,-39.4312388757297,40.0409176249753));
#190534=CARTESIAN_POINT('Ctrl Pts',(-44.0149559644985,-39.4313901062472,
40.0388310783332));
#190535=CARTESIAN_POINT('Ctrl Pts',(-44.0177981990785,-39.4316052205103,
40.036725739981));
#190536=CARTESIAN_POINT('Ctrl Pts',(-44.0279899468075,-39.4323765820012,
40.029176371072));
#190537=CARTESIAN_POINT('Ctrl Pts',(-44.0378728316086,-39.4339733733562,
40.02133108946));
#190538=CARTESIAN_POINT('Ctrl Pts',(-44.0474262866314,-39.4362681192145,
40.0132837551329));
#190539=CARTESIAN_POINT('Ctrl Pts',(-44.0579245739715,-39.4387898143852,
40.0044405431339));
#190540=CARTESIAN_POINT('Ctrl Pts',(-44.0680257165077,-39.4421543412259,
39.995352871062));
#190541=CARTESIAN_POINT('Ctrl Pts',(-44.0777053474396,-39.4462454222047,
39.986110362958));
#190542=CARTESIAN_POINT('Ctrl Pts',(-44.08815691959,-39.4506627629405,39.9761307737591));
#190543=CARTESIAN_POINT('Ctrl Pts',(-44.0981181930529,-39.4559274600913,
39.9659696936056));
#190544=CARTESIAN_POINT('Ctrl Pts',(-44.1075472421482,-39.4619494607967,
39.955712821756));
#190545=CARTESIAN_POINT('Ctrl Pts',(-44.1168971912124,-39.4679209431054,
39.9455419945197));
#190546=CARTESIAN_POINT('Ctrl Pts',(-44.1257248429276,-39.4746380711552,
39.9352756289359));
#190547=CARTESIAN_POINT('Ctrl Pts',(-44.1339623850449,-39.4820551873928,
39.92499));
#190548=CARTESIAN_POINT('Origin',(0.0101975504409187,-0.0113255271402718,
39.92499));
#190549=CARTESIAN_POINT('Ctrl Pts',(-46.6938111422607,-42.0638038389698,
40.10025));
#190550=CARTESIAN_POINT('Ctrl Pts',(-46.6880613546458,-42.0701842568303,
40.10025));
#190551=CARTESIAN_POINT('Ctrl Pts',(-46.6818296739374,-42.0760276657222,
40.0995859581842));
#190552=CARTESIAN_POINT('Ctrl Pts',(-46.6752630175678,-42.0812997491642,
40.0983275959621));
#190553=CARTESIAN_POINT('Ctrl Pts',(-46.671067236755,-42.0846683595048,
40.0975235624068));
#190554=CARTESIAN_POINT('Ctrl Pts',(-46.6667352666012,-42.0878044626436,
40.096477705949));
#190555=CARTESIAN_POINT('Ctrl Pts',(-46.6623093164291,-42.0907067742415,
40.0952149915961));
#190556=CARTESIAN_POINT('Ctrl Pts',(-46.6562687825186,-42.0946678472189,
40.0934916398701));
#190557=CARTESIAN_POINT('Ctrl Pts',(-46.6500510792883,-42.0981877352863,
40.0913643921631));
#190558=CARTESIAN_POINT('Ctrl Pts',(-46.643751530039,-42.1012583942263,
40.0889118607713));
#190559=CARTESIAN_POINT('Ctrl Pts',(-46.6406017554143,-42.1027937236964,
40.0876855950754));
#190560=CARTESIAN_POINT('Ctrl Pts',(-46.637431380974,-42.1042169023588,
40.0863782327527));
#190561=CARTESIAN_POINT('Ctrl Pts',(-46.6342513293849,-42.1055280393688,
40.0850006373334));
#190562=CARTESIAN_POINT('Ctrl Pts',(-46.6326613035904,-42.1061836078738,
40.0843118396238));
#190563=CARTESIAN_POINT('Ctrl Pts',(-46.6310688468942,-42.1068111789405,
40.0836054919165));
#190564=CARTESIAN_POINT('Ctrl Pts',(-46.6294752517396,-42.1074108478352,
40.0828829920418));
#190565=CARTESIAN_POINT('Ctrl Pts',(-46.629076852951,-42.1075607650589,
40.0827023670731));
#190566=CARTESIAN_POINT('Ctrl Pts',(-46.628678382762,-42.1077089386739,
40.0825207326933));
#190567=CARTESIAN_POINT('Ctrl Pts',(-46.6282798608701,-42.1078553707281,
40.0823381109276));
#190568=CARTESIAN_POINT('Ctrl Pts',(-46.6270842951944,-42.1082946668906,
40.0817902456304));
#190569=CARTESIAN_POINT('Ctrl Pts',(-46.6258882654173,-42.1087182876163,
40.0812334935553));
#190570=CARTESIAN_POINT('Ctrl Pts',(-46.6246922924068,-42.1091263005959,
40.0806684524227));
#190571=CARTESIAN_POINT('Ctrl Pts',(-46.6164273768568,-42.1119459234384,
40.0767636676137));
#190572=CARTESIAN_POINT('Ctrl Pts',(-46.6081492165687,-42.1140735600937,
40.0724404510889));
#190573=CARTESIAN_POINT('Ctrl Pts',(-46.5999384432817,-42.1155964444647,
40.067794993741));
#190574=CARTESIAN_POINT('Ctrl Pts',(-46.5958577114962,-42.1163533138169,
40.0654862141906));
#190575=CARTESIAN_POINT('Ctrl Pts',(-46.5917931497415,-42.1169604217532,
40.0630972003216));
#190576=CARTESIAN_POINT('Ctrl Pts',(-46.5877524553607,-42.117426213679,
40.0606363359906));
#190577=CARTESIAN_POINT('Ctrl Pts',(-46.578838080023,-42.1184538202399,
40.0552073017124));
#190578=CARTESIAN_POINT('Ctrl Pts',(-46.570042246956,-42.1188058546736,
40.0494204304519));
#190579=CARTESIAN_POINT('Ctrl Pts',(-46.5615008914345,-42.1185337834651,
40.0434049749851));
#190580=CARTESIAN_POINT('Ctrl Pts',(-46.5583806265503,-42.1184343924217,
40.0412074532442));
#190581=CARTESIAN_POINT('Ctrl Pts',(-46.5552908961829,-42.1182588963861,
40.0389814735788));
#190582=CARTESIAN_POINT('Ctrl Pts',(-46.5522345526329,-42.118011779524,
40.0367321210017));
#190583=CARTESIAN_POINT('Ctrl Pts',(-46.5419686180598,-42.1171817401332,
40.0291767837136));
#190584=CARTESIAN_POINT('Ctrl Pts',(-46.5320149571592,-42.1155299964529,
40.0213235332566));
#190585=CARTESIAN_POINT('Ctrl Pts',(-46.5223946380425,-42.1131831104079,
40.0132649215844));
#190586=CARTESIAN_POINT('Ctrl Pts',(-46.5118207677315,-42.1106036046376,
40.0044075527513));
#190587=CARTESIAN_POINT('Ctrl Pts',(-46.5016489045595,-42.1071843209722,
39.9953016253694));
#190588=CARTESIAN_POINT('Ctrl Pts',(-46.4919044745621,-42.1030402839717,
39.9860353422326));
#190589=CARTESIAN_POINT('Ctrl Pts',(-46.4814093059391,-42.0985769785641,
39.9760551582655));
#190590=CARTESIAN_POINT('Ctrl Pts',(-46.471408820054,-42.0932726122912,
39.9658879738107));
#190591=CARTESIAN_POINT('Ctrl Pts',(-46.4619468343577,-42.0872150940844,
39.9556174643197));
#190592=CARTESIAN_POINT('Ctrl Pts',(-46.4526126174182,-42.0812393728275,
39.9454856413867));
#190593=CARTESIAN_POINT('Ctrl Pts',(-46.4438014421018,-42.0745296860239,
39.9352519465095));
#190594=CARTESIAN_POINT('Ctrl Pts',(-46.4355828792672,-42.0671296588093,
39.92499));
#190595=CARTESIAN_POINT('Ctrl Pts',(-43.8790236240222,-39.7651933658996,
39.92499));
#190596=CARTESIAN_POINT('Ctrl Pts',(-43.8711584142706,-39.7581114992301,
39.9348107241742));
#190597=CARTESIAN_POINT('Ctrl Pts',(-43.8638800583542,-39.7504347382225,
39.9446038383209));
#190598=CARTESIAN_POINT('Ctrl Pts',(-43.8572218328498,-39.7422106539865,
39.9543158069443));
#190599=CARTESIAN_POINT('Ctrl Pts',(-43.8507927303092,-39.7342695770704,
39.9636935671462));
#190600=CARTESIAN_POINT('Ctrl Pts',(-43.8449410790297,-39.725817166863,
39.972996832107));
#190601=CARTESIAN_POINT('Ctrl Pts',(-43.8397310304406,-39.7168657021472,
39.9821731151428));
#190602=CARTESIAN_POINT('Ctrl Pts',(-43.8348059028379,-39.7084037645658,
39.9908475764451));
#190603=CARTESIAN_POINT('Ctrl Pts',(-43.8304536682163,-39.6994950821693,
39.9994093733951));
#190604=CARTESIAN_POINT('Ctrl Pts',(-43.8267676847771,-39.6901349804625,
40.0077966115952));
#190605=CARTESIAN_POINT('Ctrl Pts',(-43.8233729558667,-39.6815144838182,
40.0155211172709));
#190606=CARTESIAN_POINT('Ctrl Pts',(-43.8205432023665,-39.6725105620296,
40.0230979941138));
#190607=CARTESIAN_POINT('Ctrl Pts',(-43.8183892419653,-39.6631152739492,
40.0304554104866));
#190608=CARTESIAN_POINT('Ctrl Pts',(-43.8177469744554,-39.660313788705,
40.0326492435259));
#190609=CARTESIAN_POINT('Ctrl Pts',(-43.8171650742221,-39.6574775031669,
40.0348233715099));
#190610=CARTESIAN_POINT('Ctrl Pts',(-43.8166472411072,-39.6546062260519,
40.0369753512356));
#190611=CARTESIAN_POINT('Ctrl Pts',(-43.8161346989697,-39.6517642863084,
40.0391053430352));
#190612=CARTESIAN_POINT('Ctrl Pts',(-43.8156851836083,-39.6488910639687,
40.041211089324));
#190613=CARTESIAN_POINT('Ctrl Pts',(-43.8153025584994,-39.6459896850502,
40.0432881154904));
#190614=CARTESIAN_POINT('Ctrl Pts',(-43.8152759514976,-39.6457879288344,
40.043432547828));
#190615=CARTESIAN_POINT('Ctrl Pts',(-43.8152496566737,-39.6455860324534,
40.0435768364421));
#190616=CARTESIAN_POINT('Ctrl Pts',(-43.8152236753307,-39.6453839959663,
40.0437209807855));
#190617=CARTESIAN_POINT('Ctrl Pts',(-43.8140845580784,-39.6365259762553,
40.050040796842));
#190618=CARTESIAN_POINT('Ctrl Pts',(-43.8135929685791,-39.62740371779,40.0560490279345));
#190619=CARTESIAN_POINT('Ctrl Pts',(-43.81383230999,-39.6180980992371,40.0616647108616));
#190620=CARTESIAN_POINT('Ctrl Pts',(-43.8140554177822,-39.6094236454403,
40.0668995033487));
#190621=CARTESIAN_POINT('Ctrl Pts',(-43.8149139527618,-39.6005890951398,
40.0717933267483));
#190622=CARTESIAN_POINT('Ctrl Pts',(-43.8164991115145,-39.591677362319,
40.0762460303074));
#190623=CARTESIAN_POINT('Ctrl Pts',(-43.8170789830938,-39.5884173351601,
40.0778748868749));
#190624=CARTESIAN_POINT('Ctrl Pts',(-43.8177563121467,-39.5851472105416,
40.0794443522248));
#190625=CARTESIAN_POINT('Ctrl Pts',(-43.8185363400629,-39.5818719865443,
40.0809482021492));
#190626=CARTESIAN_POINT('Ctrl Pts',(-43.8187239107183,-39.5810844045885,
40.0813098278169));
#190627=CARTESIAN_POINT('Ctrl Pts',(-43.8189178575372,-39.5802961412319,
40.0816679525673));
#190628=CARTESIAN_POINT('Ctrl Pts',(-43.8191182115052,-39.5795073285706,
40.0820224192581));
#190629=CARTESIAN_POINT('Ctrl Pts',(-43.8193123044117,-39.578743166305,
40.0823658088649));
#190630=CARTESIAN_POINT('Ctrl Pts',(-43.81951241026,-39.5779784885478,40.0827057654617));
#190631=CARTESIAN_POINT('Ctrl Pts',(-43.819718554668,-39.5772134181963,
40.0830421470152));
#190632=CARTESIAN_POINT('Ctrl Pts',(-43.8219771048932,-39.5688311883232,
40.0867275956806));
#190633=CARTESIAN_POINT('Ctrl Pts',(-43.8249623840155,-39.5603964284874,
40.089982343203));
#190634=CARTESIAN_POINT('Ctrl Pts',(-43.8286919494553,-39.552096823972,
40.0926299529355));
#190635=CARTESIAN_POINT('Ctrl Pts',(-43.8302387114097,-39.5486547305946,
40.0937279956084));
#190636=CARTESIAN_POINT('Ctrl Pts',(-43.8319130705227,-39.5452359574129,
40.0947220371802));
#190637=CARTESIAN_POINT('Ctrl Pts',(-43.8337144555752,-39.5418537500314,
40.0956014538693));
#190638=CARTESIAN_POINT('Ctrl Pts',(-43.8367869054997,-39.5360850428917,
40.097101390674));
#190639=CARTESIAN_POINT('Ctrl Pts',(-43.8402296473865,-39.5304250803198,
40.0982667904316));
#190640=CARTESIAN_POINT('Ctrl Pts',(-43.8440378929943,-39.5249464846903,
40.0990539325583));
#190641=CARTESIAN_POINT('Ctrl Pts',(-43.8459420157982,-39.5222071868756,
40.0994475036216));
#190642=CARTESIAN_POINT('Ctrl Pts',(-43.8479386338069,-39.5195141476134,
40.0997467259952));
#190643=CARTESIAN_POINT('Ctrl Pts',(-43.8500271570783,-39.5168765098749,
40.0999473488896));
#190644=CARTESIAN_POINT('Ctrl Pts',(-43.8521156803496,-39.5142388721364,
40.100147971784));
#190645=CARTESIAN_POINT('Ctrl Pts',(-43.8542960677575,-39.5116566557596,
40.10025));
#190646=CARTESIAN_POINT('Ctrl Pts',(-43.8565665267058,-39.509137312462,
40.10025));
#190647=CARTESIAN_POINT('Origin',(-47.145339660541,-34.2342565846634,39.92499));
#190648=CARTESIAN_POINT('Ctrl Pts',(-50.8023624960593,-36.6746059268175,
39.92499));
#190649=CARTESIAN_POINT('Ctrl Pts',(-50.8109464329598,-36.6808425220335,
39.9348354642014));
#190650=CARTESIAN_POINT('Ctrl Pts',(-50.8190128116682,-36.6877379133662,
39.944644082845));
#190651=CARTESIAN_POINT('Ctrl Pts',(-50.8265243508951,-36.6952462569234,
39.954364176032));
#190652=CARTESIAN_POINT('Ctrl Pts',(-50.8337918098254,-36.7025106240243,
39.9637684240698));
#190653=CARTESIAN_POINT('Ctrl Pts',(-50.840540763527,-36.7103497152236,
39.9730909636379));
#190654=CARTESIAN_POINT('Ctrl Pts',(-50.8467071440061,-36.7187568768201,
39.9822808977121));
#190655=CARTESIAN_POINT('Ctrl Pts',(-50.8525401602354,-36.7267095340072,
39.9909740094627));
#190656=CARTESIAN_POINT('Ctrl Pts',(-50.8578524412734,-36.7351712462802,
39.9995492764976));
#190657=CARTESIAN_POINT('Ctrl Pts',(-50.8625525281321,-36.74415605265,40.0079462328667));
#190658=CARTESIAN_POINT('Ctrl Pts',(-50.8668816480479,-36.7524317091144,
40.015680436966));
#190659=CARTESIAN_POINT('Ctrl Pts',(-50.8706916079178,-36.7611516658429,
40.023263801739));
#190660=CARTESIAN_POINT('Ctrl Pts',(-50.8738736606191,-36.7703354510124,
40.0306257269932));
#190661=CARTESIAN_POINT('Ctrl Pts',(-50.8747966531493,-36.7729993179897,
40.0327611416629));
#190662=CARTESIAN_POINT('Ctrl Pts',(-50.8756665488979,-36.775702242456,
40.034877742726));
#190663=CARTESIAN_POINT('Ctrl Pts',(-50.8764799968255,-36.7784447603817,
40.03697331687));
#190664=CARTESIAN_POINT('Ctrl Pts',(-50.8773618266784,-36.7814178261391,
40.039245053974));
#190665=CARTESIAN_POINT('Ctrl Pts',(-50.8781771258725,-36.7844329791245,
40.041487875195));
#190666=CARTESIAN_POINT('Ctrl Pts',(-50.8789219044955,-36.7874899206173,
40.0436985701601));
#190667=CARTESIAN_POINT('Ctrl Pts',(-50.8809659552704,-36.7958797205314,
40.0497658398386));
#190668=CARTESIAN_POINT('Ctrl Pts',(-50.8824343655145,-36.8045837617102,
40.0555581699984));
#190669=CARTESIAN_POINT('Ctrl Pts',(-50.8832604021663,-36.8135226609476,
40.0609828468886));
#190670=CARTESIAN_POINT('Ctrl Pts',(-50.8840161808562,-36.8217012684457,
40.0659461317305));
#190671=CARTESIAN_POINT('Ctrl Pts',(-50.8842246658556,-36.8300699399856,
40.0706039980707));
#190672=CARTESIAN_POINT('Ctrl Pts',(-50.8838072802929,-36.8385876480148,
40.0748843180603));
#190673=CARTESIAN_POINT('Ctrl Pts',(-50.883602261868,-36.8427715183744,
40.076986797257));
#190674=CARTESIAN_POINT('Ctrl Pts',(-50.8832457706971,-36.8469911418447,
40.0789976708175));
#190675=CARTESIAN_POINT('Ctrl Pts',(-50.8827256259726,-36.8512399286215,
40.08090504915));
#190676=CARTESIAN_POINT('Ctrl Pts',(-50.8826269335774,-36.8520460945287,
40.0812669556105));
#190677=CARTESIAN_POINT('Ctrl Pts',(-50.882521936226,-36.8528536453864,
40.0816253922033));
#190678=CARTESIAN_POINT('Ctrl Pts',(-50.8824105850808,-36.8536624499711,
40.0819801989139));
#190679=CARTESIAN_POINT('Ctrl Pts',(-50.8823027136589,-36.8544459794126,
40.0823239179149));
#190680=CARTESIAN_POINT('Ctrl Pts',(-50.8821888793659,-36.8552306854276,
40.0826642303498));
#190681=CARTESIAN_POINT('Ctrl Pts',(-50.8820690400776,-36.8560164456183,
40.0830009916099));
#190682=CARTESIAN_POINT('Ctrl Pts',(-50.8807630562081,-36.8645794982677,
40.0866709464313));
#190683=CARTESIAN_POINT('Ctrl Pts',(-50.8787426509998,-36.8732733195876,
40.0899175831879));
#190684=CARTESIAN_POINT('Ctrl Pts',(-50.8759664620667,-36.8819119966114,
40.0925642067064));
#190685=CARTESIAN_POINT('Ctrl Pts',(-50.874794060241,-36.8855601635618,
40.0936818922529));
#190686=CARTESIAN_POINT('Ctrl Pts',(-50.8734872887378,-36.8891983713649,
40.0946930094791));
#190687=CARTESIAN_POINT('Ctrl Pts',(-50.8720449698705,-36.8928125648615,
40.0955863397546));
#190688=CARTESIAN_POINT('Ctrl Pts',(-50.8696161409376,-36.8988987764014,
40.0970906856166));
#190689=CARTESIAN_POINT('Ctrl Pts',(-50.8668019052538,-36.9049145742146,
40.0982599215483));
#190690=CARTESIAN_POINT('Ctrl Pts',(-50.8635979627954,-36.9107858666119,
40.0990497370454));
#190691=CARTESIAN_POINT('Ctrl Pts',(-50.8627969771808,-36.9122536897112,
40.0992471909196));
#190692=CARTESIAN_POINT('Ctrl Pts',(-50.8619714372922,-36.9137123559381,
40.0994209989363));
#190693=CARTESIAN_POINT('Ctrl Pts',(-50.8611210221662,-36.915160532232,
40.0995705982975));
#190694=CARTESIAN_POINT('Ctrl Pts',(-50.8598453994771,-36.9173327966728,
40.0997949973393));
#190695=CARTESIAN_POINT('Ctrl Pts',(-50.858513805806,-36.9194814382215,
40.0999649129781));
#190696=CARTESIAN_POINT('Ctrl Pts',(-50.8571265262611,-36.9216029292229,
40.1000786629733));
#190697=CARTESIAN_POINT('Ctrl Pts',(-50.8557392467162,-36.9237244202243,
40.1001924129685));
#190698=CARTESIAN_POINT('Ctrl Pts',(-50.8542962928986,-36.9258187603138,
40.10025));
#190699=CARTESIAN_POINT('Ctrl Pts',(-50.8527980281401,-36.9278827595334,
40.10025));
#190700=CARTESIAN_POINT('Ctrl Pts',(-47.7640607692765,-34.6837837831344,
40.10025));
#190701=CARTESIAN_POINT('Ctrl Pts',(-47.7691302463542,-34.6767997090229,
40.10025));
#190702=CARTESIAN_POINT('Ctrl Pts',(-47.7747322888379,-34.6702946353247,
40.0995786334241));
#190703=CARTESIAN_POINT('Ctrl Pts',(-47.7807252357988,-34.664321161616,
40.0983063763367));
#190704=CARTESIAN_POINT('Ctrl Pts',(-47.7845960646237,-34.6604629105138,
40.0974846287993));
#190705=CARTESIAN_POINT('Ctrl Pts',(-47.7886293194335,-34.6568257642794,
40.0964130309339));
#190706=CARTESIAN_POINT('Ctrl Pts',(-47.7927819897609,-34.6534164822762,
40.0951176960924));
#190707=CARTESIAN_POINT('Ctrl Pts',(-47.7982861164003,-34.6488976742768,
40.0934008039615));
#190708=CARTESIAN_POINT('Ctrl Pts',(-47.8040027249064,-34.6447843113773,
40.0912909372157));
#190709=CARTESIAN_POINT('Ctrl Pts',(-47.8098436832079,-34.6410949611631,
40.0888630467852));
#190710=CARTESIAN_POINT('Ctrl Pts',(-47.8127641623586,-34.639250286056,
40.0876491015699));
#190711=CARTESIAN_POINT('Ctrl Pts',(-47.8157158446827,-34.6375114518665,
40.0863558569272));
#190712=CARTESIAN_POINT('Ctrl Pts',(-47.8186885387638,-34.6358796311042,
40.0849936342772));
#190713=CARTESIAN_POINT('Ctrl Pts',(-47.8201748858043,-34.6350637207231,
40.0843125229522));
#190714=CARTESIAN_POINT('Ctrl Pts',(-47.8216664954025,-34.634274550377,
40.0836141747075));
#190715=CARTESIAN_POINT('Ctrl Pts',(-47.8231621539167,-34.6335121829167,
40.082899916161));
#190716=CARTESIAN_POINT('Ctrl Pts',(-47.8235360685452,-34.6333215910516,
40.0827213515244));
#190717=CARTESIAN_POINT('Ctrl Pts',(-47.8239102364347,-34.6331326740829,
40.0825417925842));
#190718=CARTESIAN_POINT('Ctrl Pts',(-47.8242846390327,-34.6329454324198,
40.0823612602361));
#190719=CARTESIAN_POINT('Ctrl Pts',(-47.8254078468265,-34.6323837074305,
40.0818196631918));
#190720=CARTESIAN_POINT('Ctrl Pts',(-47.8265331659852,-34.6318370616127,
40.0812693052022));
#190721=CARTESIAN_POINT('Ctrl Pts',(-47.8276601046327,-34.6313054933183,
40.0807107531875));
#190722=CARTESIAN_POINT('Ctrl Pts',(-47.8355981149517,-34.6275611948901,
40.0767763849182));
#190723=CARTESIAN_POINT('Ctrl Pts',(-47.8436253243402,-34.6245119115564,
40.0724140586137));
#190724=CARTESIAN_POINT('Ctrl Pts',(-47.8516500154454,-34.6220808005807,
40.0677221223767));
#190725=CARTESIAN_POINT('Ctrl Pts',(-47.8555419819598,-34.6209017143847,
40.065446538372));
#190726=CARTESIAN_POINT('Ctrl Pts',(-47.8594338479544,-34.6198683413511,
40.0630928000679));
#190727=CARTESIAN_POINT('Ctrl Pts',(-47.863317387285,-34.6189736992138,
40.0606689262479));
#190728=CARTESIAN_POINT('Ctrl Pts',(-47.8692628146652,-34.6176040646083,
40.0569581447806));
#190729=CARTESIAN_POINT('Ctrl Pts',(-47.8751852090114,-34.6165592825244,
40.0530843804605));
#190730=CARTESIAN_POINT('Ctrl Pts',(-47.8810431641657,-34.6158190596251,
40.0490800251457));
#190731=CARTESIAN_POINT('Ctrl Pts',(-47.8837636288444,-34.6154752962812,
40.0472203818218));
#190732=CARTESIAN_POINT('Ctrl Pts',(-47.8864700832048,-34.6151969889846,
40.0453323608819));
#190733=CARTESIAN_POINT('Ctrl Pts',(-47.8891582656053,-34.614983332396,
40.0434201572162));
#190734=CARTESIAN_POINT('Ctrl Pts',(-47.8893643041943,-34.6149669564604,
40.0432735943397));
#190735=CARTESIAN_POINT('Ctrl Pts',(-47.8895702459311,-34.6149509280615,
40.0431268995707));
#190736=CARTESIAN_POINT('Ctrl Pts',(-47.8897760897957,-34.6149352461543,
40.0429800745037));
#190737=CARTESIAN_POINT('Ctrl Pts',(-47.8926675754934,-34.6147149626375,
40.0409176249753));
#190738=CARTESIAN_POINT('Ctrl Pts',(-47.8955400426775,-34.6145651177083,
40.0388310783332));
#190739=CARTESIAN_POINT('Ctrl Pts',(-47.8983891927624,-34.6144819591401,
40.036725739981));
#190740=CARTESIAN_POINT('Ctrl Pts',(-47.9086057382628,-34.6141837673038,
40.0291763710717));
#190741=CARTESIAN_POINT('Ctrl Pts',(-47.9186013937339,-34.6147387685079,
40.0213310894592));
#190742=CARTESIAN_POINT('Ctrl Pts',(-47.9283423801891,-34.616022335536,
40.0132837551316));
#190743=CARTESIAN_POINT('Ctrl Pts',(-47.9390467457342,-34.6174328467542,
40.0044405431322));
#190744=CARTESIAN_POINT('Ctrl Pts',(-47.9494442419754,-34.6197230854585,
39.9953528710599));
#190745=CARTESIAN_POINT('Ctrl Pts',(-47.9594984812846,-34.6227799581216,
39.9861103629555));
#190746=CARTESIAN_POINT('Ctrl Pts',(-47.9703545364684,-34.6260806134274,
39.9761307737559));
#190747=CARTESIAN_POINT('Ctrl Pts',(-47.9808115517362,-34.6302752334095,
39.9659696936019));
#190748=CARTESIAN_POINT('Ctrl Pts',(-47.9908184179939,-34.6352786409534,
39.9557128217518));
#190749=CARTESIAN_POINT('Ctrl Pts',(-48.0007413369265,-34.6402400750494,
39.9455419945169));
#190750=CARTESIAN_POINT('Ctrl Pts',(-48.0102227609131,-34.6459976651003,
39.9352756289345));
#190751=CARTESIAN_POINT('Ctrl Pts',(-48.0191904766738,-34.6525130919795,
39.92499));
#190752=CARTESIAN_POINT('Origin',(0.00895784724494739,-0.0123294189942709,
39.92499));
#190753=CARTESIAN_POINT('Ctrl Pts',(-50.8348823336488,-36.952541597521,
40.10025));
#190754=CARTESIAN_POINT('Ctrl Pts',(-50.8298309792457,-36.9594880792489,
40.10025));
#190755=CARTESIAN_POINT('Ctrl Pts',(-50.8242442388875,-36.965950865344,
40.0995859581841));
#190756=CARTESIAN_POINT('Ctrl Pts',(-50.8182646381283,-36.9718804702608,
40.0983275959618));
#190757=CARTESIAN_POINT('Ctrl Pts',(-50.8144439579046,-36.9756692055214,
40.0975235624066));
#190758=CARTESIAN_POINT('Ctrl Pts',(-50.8104635307789,-36.9792409429416,
40.0964777059489));
#190759=CARTESIAN_POINT('Ctrl Pts',(-50.8063652005968,-36.9825899931424,
40.0952149915962));
#190760=CARTESIAN_POINT('Ctrl Pts',(-50.8007718022343,-36.9871607746747,
40.0934916398702));
#190761=CARTESIAN_POINT('Ctrl Pts',(-50.7949560887234,-36.9913113073907,
40.0913643921631));
#190762=CARTESIAN_POINT('Ctrl Pts',(-50.7890120203241,-36.9950236271421,
40.0889118607714));
#190763=CARTESIAN_POINT('Ctrl Pts',(-50.7860399861245,-36.9968797870178,
40.0876855950755));
#190764=CARTESIAN_POINT('Ctrl Pts',(-50.7830357420057,-36.9986265637268,
40.0863782327527));
#190765=CARTESIAN_POINT('Ctrl Pts',(-50.7800101622087,-37.0002629240968,
40.0850006373334));
#190766=CARTESIAN_POINT('Ctrl Pts',(-50.7784973723102,-37.0010811042819,
40.0843118396238));
#190767=CARTESIAN_POINT('Ctrl Pts',(-50.7769792382976,-37.0018716944999,
40.0836054919165));
#190768=CARTESIAN_POINT('Ctrl Pts',(-50.775457055492,-37.0026346543982,
40.0828829920418));
#190769=CARTESIAN_POINT('Ctrl Pts',(-50.7750765097907,-37.0028253943728,
40.0827023670731));
#190770=CARTESIAN_POINT('Ctrl Pts',(-50.7746957108234,-37.0030144077538,
40.0825207326933));
#190771=CARTESIAN_POINT('Ctrl Pts',(-50.7743146783937,-37.0032016945188,
40.0823381109276));
#190772=CARTESIAN_POINT('Ctrl Pts',(-50.7731715811046,-37.0037635548137,
40.0817902456304));
#190773=CARTESIAN_POINT('Ctrl Pts',(-50.7720263837272,-37.0043098740554,
40.0812334935553));
#190774=CARTESIAN_POINT('Ctrl Pts',(-50.7708796113517,-37.0048406651181,
40.0806684524227));
#190775=CARTESIAN_POINT('Ctrl Pts',(-50.7629547027167,-37.0085087606931,
40.0767636676138));
#190776=CARTESIAN_POINT('Ctrl Pts',(-50.754944289647,-37.0114900453058,
40.072440451089));
#190777=CARTESIAN_POINT('Ctrl Pts',(-50.7469376805983,-37.0138628466708,
40.0677949937412));
#190778=CARTESIAN_POINT('Ctrl Pts',(-50.7429584178786,-37.015042122436,
40.0654862141907));
#190779=CARTESIAN_POINT('Ctrl Pts',(-50.738979582278,-37.0160707669656,
40.0630972003217));
#190780=CARTESIAN_POINT('Ctrl Pts',(-50.7350097117579,-37.0169563748087,
40.0606363359906));
#190781=CARTESIAN_POINT('Ctrl Pts',(-50.7262515844357,-37.0189101579884,
40.0552073017124));
#190782=CARTESIAN_POINT('Ctrl Pts',(-50.717540733481,-37.0201796788543,
40.0494204304519));
#190783=CARTESIAN_POINT('Ctrl Pts',(-50.7090177292134,-37.0208019128473,
40.0434049749852));
#190784=CARTESIAN_POINT('Ctrl Pts',(-50.7059041682737,-37.0210292227717,
40.0412074532442));
#190785=CARTESIAN_POINT('Ctrl Pts',(-50.7028130194416,-37.021177652889,
40.0389814735788));
#190786=CARTESIAN_POINT('Ctrl Pts',(-50.6997475881155,-37.0212513646534,
40.0367321210017));
#190787=CARTESIAN_POINT('Ctrl Pts',(-50.6894511286645,-37.0214989546702,
40.0291767837139));
#190788=CARTESIAN_POINT('Ctrl Pts',(-50.6793793407317,-37.0208967002924,
40.0213235332571));
#190789=CARTESIAN_POINT('Ctrl Pts',(-50.6695664063384,-37.0195682679084,
40.0132649215851));
#190790=CARTESIAN_POINT('Ctrl Pts',(-50.6587808290217,-37.0181081633552,
40.0044075527522));
#190791=CARTESIAN_POINT('Ctrl Pts',(-50.6483072759139,-37.0157708601097,
39.9953016253706));
#190792=CARTESIAN_POINT('Ctrl Pts',(-50.6381830571046,-37.0126680948708,
39.9860353422341));
#190793=CARTESIAN_POINT('Ctrl Pts',(-50.6272788396587,-37.0093262837655,
39.9760551582674));
#190794=CARTESIAN_POINT('Ctrl Pts',(-50.6167786802271,-37.005096310788,
39.9658879738132));
#190795=CARTESIAN_POINT('Ctrl Pts',(-50.6067353452094,-37.0000610231244,
39.9556174643228));
#190796=CARTESIAN_POINT('Ctrl Pts',(-50.5968276291256,-36.9950937288458,
39.9454856413887));
#190797=CARTESIAN_POINT('Ctrl Pts',(-50.5873633690976,-36.9893418170233,
39.9352519465104));
#190798=CARTESIAN_POINT('Ctrl Pts',(-50.5784163149359,-36.9828414016744,
39.92499));
#190799=CARTESIAN_POINT('Ctrl Pts',(-47.7952442955504,-34.9607485668363,
39.92499));
#190800=CARTESIAN_POINT('Ctrl Pts',(-47.7866819156022,-34.954527633663,
39.9348107241725));
#190801=CARTESIAN_POINT('Ctrl Pts',(-47.7786409912514,-34.9476537221158,
39.9446038383174));
#190802=CARTESIAN_POINT('Ctrl Pts',(-47.7711595893171,-34.9401706643553,
39.9543158069391));
#190803=CARTESIAN_POINT('Ctrl Pts',(-47.7639356375068,-34.9329451136992,
39.96369356714));
#190804=CARTESIAN_POINT('Ctrl Pts',(-47.7572325247358,-34.9251506707962,
39.9729968320999));
#190805=CARTESIAN_POINT('Ctrl Pts',(-47.7511153344876,-34.9167928415144,
39.9821731151347));
#190806=CARTESIAN_POINT('Ctrl Pts',(-47.7453326739177,-34.908892075333,
39.9908475764366));
#190807=CARTESIAN_POINT('Ctrl Pts',(-47.7400730704119,-34.9004871280284,
39.9994093733862));
#190808=CARTESIAN_POINT('Ctrl Pts',(-47.7354288821281,-34.8915635921236,
40.0077966115859));
#190809=CARTESIAN_POINT('Ctrl Pts',(-47.7311516626307,-34.8833451652587,
40.0155211172615));
#190810=CARTESIAN_POINT('Ctrl Pts',(-47.727396244708,-34.8746863576813,
40.0230979941043));
#190811=CARTESIAN_POINT('Ctrl Pts',(-47.7242720089018,-34.8655676881434,
40.0304554104772));
#190812=CARTESIAN_POINT('Ctrl Pts',(-47.7233404248515,-34.8628486849605,
40.0326492435196));
#190813=CARTESIAN_POINT('Ctrl Pts',(-47.7224652397586,-34.8600887620247,
40.0348233715068));
#190814=CARTESIAN_POINT('Ctrl Pts',(-47.7216501132021,-34.8572873423618,
40.0369753512356));
#190815=CARTESIAN_POINT('Ctrl Pts',(-47.72084331523,-34.8545145463036,40.0391053430352));
#190816=CARTESIAN_POINT('Ctrl Pts',(-47.720095928845,-34.8517040509265,
40.041211089324));
#190817=CARTESIAN_POINT('Ctrl Pts',(-47.7194121231167,-34.8488585612799,
40.0432881154904));
#190818=CARTESIAN_POINT('Ctrl Pts',(-47.7193645726037,-34.8486606914947,
40.043432547828));
#190819=CARTESIAN_POINT('Ctrl Pts',(-47.7193173179071,-34.8484626496808,
40.0435768364421));
#190820=CARTESIAN_POINT('Ctrl Pts',(-47.7192703603292,-34.8482644357606,
40.0437209807855));
#190821=CARTESIAN_POINT('Ctrl Pts',(-47.7172115680923,-34.8395740113842,
40.0500407968421));
#190822=CARTESIAN_POINT('Ctrl Pts',(-47.7157691359129,-34.8305531107002,
40.0560490279346));
#190823=CARTESIAN_POINT('Ctrl Pts',(-47.7150344641794,-34.8212734513095,
40.0616647108616));
#190824=CARTESIAN_POINT('Ctrl Pts',(-47.7143496224387,-34.8126231959632,
40.0668995033489));
#190825=CARTESIAN_POINT('Ctrl Pts',(-47.7142799923072,-34.8037473009113,
40.0717933267486));
#190826=CARTESIAN_POINT('Ctrl Pts',(-47.7149249376577,-34.7947186932867,
40.0762460303077));
#190827=CARTESIAN_POINT('Ctrl Pts',(-47.7151608670106,-34.7914159118128,
40.0778748868751));
#190828=CARTESIAN_POINT('Ctrl Pts',(-47.7154926644831,-34.7880929011144,
40.0794443522249));
#190829=CARTESIAN_POINT('Ctrl Pts',(-47.7159260651934,-34.7847540840178,
40.0809482021492));
#190830=CARTESIAN_POINT('Ctrl Pts',(-47.7160302835856,-34.7839512100459,
40.0813098278169));
#190831=CARTESIAN_POINT('Ctrl Pts',(-47.7161407719862,-34.7831469919156,
40.0816679525672));
#190832=CARTESIAN_POINT('Ctrl Pts',(-47.7162575750189,-34.7823415577602,
40.0820224192581));
#190833=CARTESIAN_POINT('Ctrl Pts',(-47.7163707279568,-34.7815612934222,
40.0823658088648));
#190834=CARTESIAN_POINT('Ctrl Pts',(-47.7164898070135,-34.780779887893,
40.0827057654617));
#190835=CARTESIAN_POINT('Ctrl Pts',(-47.7166148505127,-34.7799974607187,
40.0830421470151));
#190836=CARTESIAN_POINT('Ctrl Pts',(-47.717984846556,-34.7714250667938,
40.0867275956805));
#190837=CARTESIAN_POINT('Ctrl Pts',(-47.7200720995232,-34.7627244668161,
40.0899823432028));
#190838=CARTESIAN_POINT('Ctrl Pts',(-47.7229136891075,-34.7540804826588,
40.0926299529353));
#190839=CARTESIAN_POINT('Ctrl Pts',(-47.724092181007,-34.7504955647788,
40.0937279956083));
#190840=CARTESIAN_POINT('Ctrl Pts',(-47.7254000086987,-34.7469205018089,
40.0947220371802));
#190841=CARTESIAN_POINT('Ctrl Pts',(-47.7268379886354,-34.7433685265019,
40.0956014538693));
#190842=CARTESIAN_POINT('Ctrl Pts',(-47.7292906132653,-34.7373102624744,
40.097101390674));
#190843=CARTESIAN_POINT('Ctrl Pts',(-47.7321228682622,-34.7313214412508,
40.0982667904316));
#190844=CARTESIAN_POINT('Ctrl Pts',(-47.7353375827202,-34.7254747878805,
40.0990539325583));
#190845=CARTESIAN_POINT('Ctrl Pts',(-47.7369449399493,-34.7225514611953,
40.0994475036216));
#190846=CARTESIAN_POINT('Ctrl Pts',(-47.73864912102,-34.7196644712718,40.0997467259952));
#190847=CARTESIAN_POINT('Ctrl Pts',(-47.7404504949228,-34.7168229726607,
40.0999473488896));
#190848=CARTESIAN_POINT('Ctrl Pts',(-47.7422518688256,-34.7139814740496,
40.100147971784));
#190849=CARTESIAN_POINT('Ctrl Pts',(-47.7441503967333,-34.7111854907791,
40.10025));
#190850=CARTESIAN_POINT('Ctrl Pts',(-47.7461450747866,-34.7084426211229,
40.10025));
#190851=CARTESIAN_POINT('Origin',(-50.4655267888877,-29.1186878401553,39.92499));
#190852=CARTESIAN_POINT('Ctrl Pts',(-54.357602037244,-31.1634057161437,
39.92499));
#190853=CARTESIAN_POINT('Ctrl Pts',(-54.3667908521539,-31.1687108809055,
39.9348354642015));
#190854=CARTESIAN_POINT('Ctrl Pts',(-54.3755338070554,-31.1747253323925,
39.9446440828451));
#190855=CARTESIAN_POINT('Ctrl Pts',(-54.3837890328982,-31.1814073748059,
39.9543641760321));
#190856=CARTESIAN_POINT('Ctrl Pts',(-54.3917760130578,-31.18787229063,39.96376842407));
#190857=CARTESIAN_POINT('Ctrl Pts',(-54.3993074034413,-31.1949629807083,
39.9730909636381));
#190858=CARTESIAN_POINT('Ctrl Pts',(-54.406318791525,-31.2026795247186,
39.9822808977123));
#190859=CARTESIAN_POINT('Ctrl Pts',(-54.4129511329158,-31.2099789001949,
39.9909740094629));
#190860=CARTESIAN_POINT('Ctrl Pts',(-54.4191188025029,-31.2178389737493,
39.9995492764979));
#190861=CARTESIAN_POINT('Ctrl Pts',(-54.4247323097967,-31.2262832675533,
40.007946232867));
#190862=CARTESIAN_POINT('Ctrl Pts',(-54.4299027559934,-31.2340610728536,
40.0156804369663));
#190863=CARTESIAN_POINT('Ctrl Pts',(-54.4346033281811,-31.2423350114965,
40.0232638017393));
#190864=CARTESIAN_POINT('Ctrl Pts',(-54.4387279162155,-31.2511358718512,
40.0306257269936));
#190865=CARTESIAN_POINT('Ctrl Pts',(-54.4399243024176,-31.2536886668955,
40.0327611416631));
#190866=CARTESIAN_POINT('Ctrl Pts',(-54.441071965327,-31.2562858555929,
40.0348777427261));
#190867=CARTESIAN_POINT('Ctrl Pts',(-54.4421676282859,-31.2589283212564,
40.0369733168701));
#190868=CARTESIAN_POINT('Ctrl Pts',(-54.4433553973774,-31.2617929239292,
40.039245053974));
#190869=CARTESIAN_POINT('Ctrl Pts',(-54.4444813995853,-31.2647063376192,
40.041487875195));
#190870=CARTESIAN_POINT('Ctrl Pts',(-54.4455416356296,-31.2676686823016,
40.0436985701601));
#190871=CARTESIAN_POINT('Ctrl Pts',(-54.4484514617727,-31.2757988605277,
40.0497658398386));
#190872=CARTESIAN_POINT('Ctrl Pts',(-54.4508216479604,-31.2843017293919,
40.0555581699984));
#190873=CARTESIAN_POINT('Ctrl Pts',(-54.4525775288976,-31.2931053160622,
40.0609828468886));
#190874=CARTESIAN_POINT('Ctrl Pts',(-54.4541840646262,-31.3011601199077,
40.0659461317305));
#190875=CARTESIAN_POINT('Ctrl Pts',(-54.4552661718987,-31.3094611543727,
40.0706039980707));
#190876=CARTESIAN_POINT('Ctrl Pts',(-54.4557414157486,-31.3179758301776,
40.0748843180604));
#190877=CARTESIAN_POINT('Ctrl Pts',(-54.4559748539753,-31.3221582111184,
40.076986797257));
#190878=CARTESIAN_POINT('Ctrl Pts',(-54.4560613864572,-31.3263919825241,
40.0789976708175));
#190879=CARTESIAN_POINT('Ctrl Pts',(-54.4559882102925,-31.3306718639311,
40.08090504915));
#190880=CARTESIAN_POINT('Ctrl Pts',(-54.455974325828,-31.3314839297415,
40.0812669556105));
#190881=CARTESIAN_POINT('Ctrl Pts',(-54.4559543157132,-31.3322980319628,
40.0816253922032));
#190882=CARTESIAN_POINT('Ctrl Pts',(-54.4559281176616,-31.3331140451956,
40.0819801989139));
#190883=CARTESIAN_POINT('Ctrl Pts',(-54.455902738299,-31.3339045580148,
40.0823239179149));
#190884=CARTESIAN_POINT('Ctrl Pts',(-54.4558715517161,-31.3346968642518,
40.0826642303498));
#190885=CARTESIAN_POINT('Ctrl Pts',(-54.4558345032252,-31.3354908465826,
40.0830009916099));
#190886=CARTESIAN_POINT('Ctrl Pts',(-54.4554307564063,-31.3441435024201,
40.0866709464311));
#190887=CARTESIAN_POINT('Ctrl Pts',(-54.4543301709717,-31.3530008879284,
40.0899175831876));
#190888=CARTESIAN_POINT('Ctrl Pts',(-54.4524721779261,-31.361882432138,
40.092564206706));
#190889=CARTESIAN_POINT('Ctrl Pts',(-54.4516875359254,-31.3656331634098,
40.0936818922526));
#190890=CARTESIAN_POINT('Ctrl Pts',(-54.4507682193238,-31.3693880355473,
40.094693009479));
#190891=CARTESIAN_POINT('Ctrl Pts',(-54.4497115877222,-31.373133193489,
40.0955863397546));
#190892=CARTESIAN_POINT('Ctrl Pts',(-54.4479322465077,-31.3794399458811,
40.0970906856166));
#190893=CARTESIAN_POINT('Ctrl Pts',(-54.4457622496022,-31.3857169562557,
40.0982599215483));
#190894=CARTESIAN_POINT('Ctrl Pts',(-54.4431895758471,-31.3918909882803,
40.0990497370454));
#190895=CARTESIAN_POINT('Ctrl Pts',(-54.4425464074084,-31.3934344962864,
40.0992471909196));
#190896=CARTESIAN_POINT('Ctrl Pts',(-54.4418778620528,-31.3949714642032,
40.0994209989363));
#190897=CARTESIAN_POINT('Ctrl Pts',(-54.4411834812323,-31.396500599822,
40.0995705982975));
#190898=CARTESIAN_POINT('Ctrl Pts',(-54.4401419100017,-31.3987943032504,
40.0997949973393));
#190899=CARTESIAN_POINT('Ctrl Pts',(-54.4390422051394,-31.401070363756,
40.0999649129781));
#190900=CARTESIAN_POINT('Ctrl Pts',(-54.4378842814512,-31.4033252432067,
40.1000786629733));
#190901=CARTESIAN_POINT('Ctrl Pts',(-54.4367263577631,-31.4055801226574,
40.1001924129685));
#190902=CARTESIAN_POINT('Ctrl Pts',(-54.4355102267488,-31.407813819478,
40.10025));
#190903=CARTESIAN_POINT('Ctrl Pts',(-54.434235916308,-31.4100231232067,
40.10025));
#190904=CARTESIAN_POINT('Ctrl Pts',(-51.1278468659049,-29.5010785149108,
40.10025));
#190905=CARTESIAN_POINT('Ctrl Pts',(-51.1321585373226,-29.4936027956393,
40.10025));
#190906=CARTESIAN_POINT('Ctrl Pts',(-51.1370499258746,-29.4865477845233,
40.099578633424));
#190907=CARTESIAN_POINT('Ctrl Pts',(-51.142385644818,-29.4799806005921,
40.0983063763365));
#190908=CARTESIAN_POINT('Ctrl Pts',(-51.1458319717788,-29.4757388736048,
40.0974846287991));
#190909=CARTESIAN_POINT('Ctrl Pts',(-51.1494629466901,-29.4717000621109,
40.0964130309337));
#190910=CARTESIAN_POINT('Ctrl Pts',(-51.1532365012461,-29.4678753842637,
40.0951176960923));
#190911=CARTESIAN_POINT('Ctrl Pts',(-51.1582381316479,-29.462805992868,
40.0934008039614));
#190912=CARTESIAN_POINT('Ctrl Pts',(-51.1634934604717,-29.4581176150987,
40.0912909372156));
#190913=CARTESIAN_POINT('Ctrl Pts',(-51.1689167792841,-29.4538379291358,
40.0888630467851));
#190914=CARTESIAN_POINT('Ctrl Pts',(-51.1716284386903,-29.4516980861543,
40.0876491015698));
#190915=CARTESIAN_POINT('Ctrl Pts',(-51.174382193724,-29.449660242663,40.0863558569271));
#190916=CARTESIAN_POINT('Ctrl Pts',(-51.1771680313593,-29.4477266300416,
40.0849936342771));
#190917=CARTESIAN_POINT('Ctrl Pts',(-51.1785609501769,-29.4467598237308,
40.084312522952));
#190918=CARTESIAN_POINT('Ctrl Pts',(-51.1799618978181,-29.4458190608834,
40.0836141747074));
#190919=CARTESIAN_POINT('Ctrl Pts',(-51.1813696738593,-29.4449045308658,
40.0828999161609));
#190920=CARTESIAN_POINT('Ctrl Pts',(-51.1817216178696,-29.4446758983613,
40.0827213515243));
#190921=CARTESIAN_POINT('Ctrl Pts',(-51.1820739888279,-29.4444489051051,
40.0825417925841));
#190922=CARTESIAN_POINT('Ctrl Pts',(-51.182426768326,-29.4442235534432,
40.082361260236));
#190923=CARTESIAN_POINT('Ctrl Pts',(-51.1834851068201,-29.4435474984575,
40.0818196631917));
#190924=CARTESIAN_POINT('Ctrl Pts',(-51.1845471213153,-29.4428862193404,
40.0812693052021));
#190925=CARTESIAN_POINT('Ctrl Pts',(-51.1856123224581,-29.4422397658677,
40.0807107531874));
#190926=CARTESIAN_POINT('Ctrl Pts',(-51.1931154617649,-29.4376862310782,
40.0767763849183));
#190927=CARTESIAN_POINT('Ctrl Pts',(-51.2007799603592,-29.4338145801761,
40.072414058614));
#190928=CARTESIAN_POINT('Ctrl Pts',(-51.2085065710723,-29.4305579784514,
40.0677221223772));
#190929=CARTESIAN_POINT('Ctrl Pts',(-51.212253968919,-29.4289785301338,
40.0654465383723));
#190930=CARTESIAN_POINT('Ctrl Pts',(-51.2160164979697,-29.4275440072541,
40.0630928000681));
#190931=CARTESIAN_POINT('Ctrl Pts',(-51.219785247298,-29.4262483256616,
40.0606689262479));
#190932=CARTESIAN_POINT('Ctrl Pts',(-51.2255549392045,-29.4242647276703,
40.0569581447806));
#190933=CARTESIAN_POINT('Ctrl Pts',(-51.2313356805891,-29.4226066102321,
40.0530843804606));
#190934=CARTESIAN_POINT('Ctrl Pts',(-51.23708417089,-29.4212581193011,40.0490800251458));
#190935=CARTESIAN_POINT('Ctrl Pts',(-51.2397537995245,-29.4206318731365,
40.0472203818218));
#190936=CARTESIAN_POINT('Ctrl Pts',(-51.2424163366106,-29.4200721889212,
40.0453323608819));
#190937=CARTESIAN_POINT('Ctrl Pts',(-51.2450674596718,-29.4195787111905,
40.0434201572162));
#190938=CARTESIAN_POINT('Ctrl Pts',(-51.2452706578085,-29.4195408880668,
40.0432735943397));
#190939=CARTESIAN_POINT('Ctrl Pts',(-51.245473795951,-29.4195034207,40.0431268995707));
#190940=CARTESIAN_POINT('Ctrl Pts',(-51.2456768729757,-29.4194663081571,
40.0429800745037));
#190941=CARTESIAN_POINT('Ctrl Pts',(-51.2485294929147,-29.4189449888199,
40.0409176249753));
#190942=CARTESIAN_POINT('Ctrl Pts',(-51.2513705613629,-29.4184957101763,
40.0388310783332));
#190943=CARTESIAN_POINT('Ctrl Pts',(-51.2541954110682,-29.4181151898794,
40.036725739981));
#190944=CARTESIAN_POINT('Ctrl Pts',(-51.2643248197284,-29.4167507117682,
40.0291763710721));
#190945=CARTESIAN_POINT('Ctrl Pts',(-51.2743237313754,-29.4162578421119,
40.0213310894601));
#190946=CARTESIAN_POINT('Ctrl Pts',(-51.284145524976,-29.4165161672806,
40.0132837551329));
#190947=CARTESIAN_POINT('Ctrl Pts',(-51.2949386894566,-29.4168000406899,
40.0044405431337));
#190948=CARTESIAN_POINT('Ctrl Pts',(-51.3055186222576,-29.417990898923,
39.9953528710615));
#190949=CARTESIAN_POINT('Ctrl Pts',(-51.3158373135936,-29.4199800715334,
39.9861103629572));
#190950=CARTESIAN_POINT('Ctrl Pts',(-51.3269789105987,-29.4221278787384,
39.9761307737573));
#190951=CARTESIAN_POINT('Ctrl Pts',(-51.3378170984239,-29.4252064644172,
39.9659696936028));
#190952=CARTESIAN_POINT('Ctrl Pts',(-51.3482921445234,-29.4291364604192,
39.9557128217522));
#190953=CARTESIAN_POINT('Ctrl Pts',(-51.3586793157496,-29.4330334877929,
39.9455419945171));
#190954=CARTESIAN_POINT('Ctrl Pts',(-51.3687106315439,-29.4377684584842,
39.9352756289346));
#190955=CARTESIAN_POINT('Ctrl Pts',(-51.3783102687786,-29.4433108116258,
39.92499));
#190956=CARTESIAN_POINT('Origin',(0.00762000000001041,-0.0131982271536721,
39.92499));
#190957=CARTESIAN_POINT('Ctrl Pts',(-54.4189959163065,-31.4364195775132,
40.10025));
#190958=CARTESIAN_POINT('Ctrl Pts',(-54.4146983388119,-31.4438560159999,
40.10025));
#190959=CARTESIAN_POINT('Ctrl Pts',(-54.4098177483014,-31.4508673716601,
40.0995859581842));
#190960=CARTESIAN_POINT('Ctrl Pts',(-54.4044907169112,-31.4573895320586,
40.0983275959621));
#190961=CARTESIAN_POINT('Ctrl Pts',(-54.4010869974475,-31.4615568820642,
40.0975235624069));
#190962=CARTESIAN_POINT('Ctrl Pts',(-54.3975017237412,-31.4655251210644,
40.0964777059491));
#190963=CARTESIAN_POINT('Ctrl Pts',(-54.393775915711,-31.4692842169743,
40.0952149915961));
#190964=CARTESIAN_POINT('Ctrl Pts',(-54.3886909353394,-31.4744146286223,
40.0934916398701));
#190965=CARTESIAN_POINT('Ctrl Pts',(-54.3833409297223,-31.4791503318818,
40.091364392163));
#190966=CARTESIAN_POINT('Ctrl Pts',(-54.3778174666304,-31.4834636394926,
40.0889118607713));
#190967=CARTESIAN_POINT('Ctrl Pts',(-54.3750557350845,-31.4856202932979,
40.0876855950754));
#190968=CARTESIAN_POINT('Ctrl Pts',(-54.3722505364144,-31.4876715300024,
40.0863782327526));
#190969=CARTESIAN_POINT('Ctrl Pts',(-54.3694125772949,-31.4896151854257,
40.0850006373334));
#190970=CARTESIAN_POINT('Ctrl Pts',(-54.3679935977352,-31.4905870131374,
40.0843118396237));
#190971=CARTESIAN_POINT('Ctrl Pts',(-54.3665664194001,-31.4915319606349,
40.0836054919164));
#190972=CARTESIAN_POINT('Ctrl Pts',(-54.365132326297,-31.4924498523885,
40.0828829920417));
#190973=CARTESIAN_POINT('Ctrl Pts',(-54.3647738030212,-31.4926793253269,
40.0827023670731));
#190974=CARTESIAN_POINT('Ctrl Pts',(-54.3644148473887,-31.4929071076037,
40.0825207326933));
#190975=CARTESIAN_POINT('Ctrl Pts',(-54.3640554790923,-31.4931331971265,
40.0823381109275));
#190976=CARTESIAN_POINT('Ctrl Pts',(-54.362977374203,-31.493811465695,40.0817902456303));
#190977=CARTESIAN_POINT('Ctrl Pts',(-54.3618955562474,-31.4944744978647,
40.0812334935553));
#190978=CARTESIAN_POINT('Ctrl Pts',(-54.3608105487851,-31.4951222515525,
40.0806684524227));
#190979=CARTESIAN_POINT('Ctrl Pts',(-54.3533124740222,-31.4995986314374,
40.0767636676137));
#190980=CARTESIAN_POINT('Ctrl Pts',(-54.3456575719325,-31.5034009004294,
40.0724404510888));
#190981=CARTESIAN_POINT('Ctrl Pts',(-54.3379428492061,-31.5065976218801,
40.0677949937409));
#190982=CARTESIAN_POINT('Ctrl Pts',(-54.3341086531876,-31.5081863836663,
40.0654862141906));
#190983=CARTESIAN_POINT('Ctrl Pts',(-54.3302591366968,-31.5096252947444,
40.0630972003216));
#190984=CARTESIAN_POINT('Ctrl Pts',(-54.3264035847697,-31.5109210155999,
40.0606363359906));
#190985=CARTESIAN_POINT('Ctrl Pts',(-54.3178976613387,-31.5137795693409,
40.0552073017123));
#190986=CARTESIAN_POINT('Ctrl Pts',(-54.3093672304021,-31.5159526675028,
40.0494204304519));
#190987=CARTESIAN_POINT('Ctrl Pts',(-54.3009559572068,-31.5174623893714,
40.0434049749851));
#190988=CARTESIAN_POINT('Ctrl Pts',(-54.2978832130368,-31.5180139098085,
40.0412074532442));
#190989=CARTESIAN_POINT('Ctrl Pts',(-54.2948245130135,-31.5184846398473,
40.0389814735788));
#190990=CARTESIAN_POINT('Ctrl Pts',(-54.2917835794184,-31.5188783726367,
40.0367321210017));
#190991=CARTESIAN_POINT('Ctrl Pts',(-54.2815694052539,-31.5202008794129,
40.0291767837141));
#190992=CARTESIAN_POINT('Ctrl Pts',(-54.2714898389049,-31.5206547127626,
40.0213235332576));
#190993=CARTESIAN_POINT('Ctrl Pts',(-54.2615918017975,-31.5203592886225,
40.0132649215858));
#190994=CARTESIAN_POINT('Ctrl Pts',(-54.250712686517,-31.5200345824972,
40.0044075527532));
#190995=CARTESIAN_POINT('Ctrl Pts',(-54.2400521939127,-31.5188048676548,
39.9953016253719));
#190996=CARTESIAN_POINT('Ctrl Pts',(-54.2296591093513,-31.5167773687226,
39.9860353422357));
#190997=CARTESIAN_POINT('Ctrl Pts',(-54.2184653119704,-31.5145936655011,
39.9760551582693));
#190998=CARTESIAN_POINT('Ctrl Pts',(-54.207580520936,-31.5114844302878,
39.9658879738153));
#190999=CARTESIAN_POINT('Ctrl Pts',(-54.197065873477,-31.5075265408326,
39.9556174643251));
#191000=CARTESIAN_POINT('Ctrl Pts',(-54.1866932092603,-31.5036220962484,
39.9454856413903));
#191001=CARTESIAN_POINT('Ctrl Pts',(-54.1766795569346,-31.4988909785571,
39.9352519465112));
#191002=CARTESIAN_POINT('Ctrl Pts',(-54.167102037244,-31.4933613949856,
39.92499));
#191003=CARTESIAN_POINT('Ctrl Pts',(-51.1878102687787,-29.7732664904677,
39.92499));
#191004=CARTESIAN_POINT('Ctrl Pts',(-51.1786445298599,-29.7679746486356,
39.9348107241716));
#191005=CARTESIAN_POINT('Ctrl Pts',(-51.1699291351241,-29.7619788985613,
39.9446038383157));
#191006=CARTESIAN_POINT('Ctrl Pts',(-51.1617065245647,-29.7553188532221,
39.9543158069366));
#191007=CARTESIAN_POINT('Ctrl Pts',(-51.1537668706124,-29.7488879934705,
39.9636935671368));
#191008=CARTESIAN_POINT('Ctrl Pts',(-51.1462857370563,-29.741836915419,
39.9729968320961));
#191009=CARTESIAN_POINT('Ctrl Pts',(-51.1393284263655,-29.7341642916973,
39.9821731151303));
#191010=CARTESIAN_POINT('Ctrl Pts',(-51.1327515888678,-29.7269112593634,
39.9908475764318));
#191011=CARTESIAN_POINT('Ctrl Pts',(-51.126642241795,-29.719102133512,39.9994093733809));
#191012=CARTESIAN_POINT('Ctrl Pts',(-51.1210907313655,-29.7107129315358,
40.0077966115803));
#191013=CARTESIAN_POINT('Ctrl Pts',(-51.1159778833935,-29.702986617255,
40.0155211172554));
#191014=CARTESIAN_POINT('Ctrl Pts',(-51.1113379461932,-29.6947677915966,
40.023097994098));
#191015=CARTESIAN_POINT('Ctrl Pts',(-51.1072776647637,-29.6860256466531,
40.0304554104705));
#191016=CARTESIAN_POINT('Ctrl Pts',(-51.1060669708027,-29.6834189155008,
40.0326492435153));
#191017=CARTESIAN_POINT('Ctrl Pts',(-51.1049080895609,-29.6807655934617,
40.0348233715046));
#191018=CARTESIAN_POINT('Ctrl Pts',(-51.1038046002594,-29.6780647241925,
40.0369753512356));
#191019=CARTESIAN_POINT('Ctrl Pts',(-51.1027123859001,-29.6753914511534,
40.0391053430352));
#191020=CARTESIAN_POINT('Ctrl Pts',(-51.1016753170131,-29.6726744751144,
40.041211089324));
#191021=CARTESIAN_POINT('Ctrl Pts',(-51.1006978225842,-29.6699160505197,
40.0432881154904));
#191022=CARTESIAN_POINT('Ctrl Pts',(-51.1006298495333,-29.669724235068,
40.043432547828));
#191023=CARTESIAN_POINT('Ctrl Pts',(-51.1005621526964,-29.6695322176087,
40.0435768364421));
#191024=CARTESIAN_POINT('Ctrl Pts',(-51.1004947333605,-29.6693399979285,
40.0437209807855));
#191025=CARTESIAN_POINT('Ctrl Pts',(-51.0975388226978,-29.660912382995,
40.050040796842));
#191026=CARTESIAN_POINT('Ctrl Pts',(-51.095161351427,-29.652091674968,40.0560490279343));
#191027=CARTESIAN_POINT('Ctrl Pts',(-51.0934607157664,-29.6429396446298,
40.0616647108613));
#191028=CARTESIAN_POINT('Ctrl Pts',(-51.0918754277622,-29.6344083617426,
40.0668995033484));
#191029=CARTESIAN_POINT('Ctrl Pts',(-51.090878395402,-29.6255883681034,
40.071793326748));
#191030=CARTESIAN_POINT('Ctrl Pts',(-51.0905760611938,-29.61654180499,40.076246030307));
#191031=CARTESIAN_POINT('Ctrl Pts',(-51.0904654634291,-29.6132324551655,
40.0778748868746));
#191032=CARTESIAN_POINT('Ctrl Pts',(-51.0904480940785,-29.609892965987,
40.0794443522246));
#191033=CARTESIAN_POINT('Ctrl Pts',(-51.0905301191541,-29.606527136569,
40.0809482021492));
#191034=CARTESIAN_POINT('Ctrl Pts',(-51.0905498434446,-29.6057177670364,
40.0813098278168));
#191035=CARTESIAN_POINT('Ctrl Pts',(-51.090575662893,-29.6049064053144,
40.0816679525672));
#191036=CARTESIAN_POINT('Ctrl Pts',(-51.0906076352719,-29.60409317417,40.082022419258));
#191037=CARTESIAN_POINT('Ctrl Pts',(-51.0906386085139,-29.603305356499,
40.0823658088648));
#191038=CARTESIAN_POINT('Ctrl Pts',(-51.090675356124,-29.6025157844402,
40.0827057654616));
#191039=CARTESIAN_POINT('Ctrl Pts',(-51.0907179287116,-29.601724572879,
40.0830421470151));
#191040=CARTESIAN_POINT('Ctrl Pts',(-51.0911843606098,-29.5930559358435,
40.0867275956807));
#191041=CARTESIAN_POINT('Ctrl Pts',(-51.0923507190418,-29.5841848213171,
40.0899823432032));
#191042=CARTESIAN_POINT('Ctrl Pts',(-51.0942731997207,-29.5752911628165,
40.0926299529357));
#191043=CARTESIAN_POINT('Ctrl Pts',(-51.0950705097613,-29.571602697545,
40.0937279956085));
#191044=CARTESIAN_POINT('Ctrl Pts',(-51.0959974771976,-29.5679105139259,
40.0947220371803));
#191045=CARTESIAN_POINT('Ctrl Pts',(-51.0970562972092,-29.5642276868787,
40.0956014538692));
#191046=CARTESIAN_POINT('Ctrl Pts',(-51.0988622250759,-29.5579462415719,
40.097101390674));
#191047=CARTESIAN_POINT('Ctrl Pts',(-51.1010529624042,-29.5516941764752,
40.0982667904316));
#191048=CARTESIAN_POINT('Ctrl Pts',(-51.1036389246278,-29.5455435225215,
40.0990539325582));
#191049=CARTESIAN_POINT('Ctrl Pts',(-51.1049319057396,-29.5424681955446,
40.0994475036216));
#191050=CARTESIAN_POINT('Ctrl Pts',(-51.106324978508,-29.5394188854256,
40.0997467259952));
#191051=CARTESIAN_POINT('Ctrl Pts',(-51.107819466813,-29.5364046579954,
40.0999473488896));
#191052=CARTESIAN_POINT('Ctrl Pts',(-51.109313955118,-29.5333904305652,
40.100147971784));
#191053=CARTESIAN_POINT('Ctrl Pts',(-51.1109098228568,-29.530411313779,
40.10025));
#191054=CARTESIAN_POINT('Ctrl Pts',(-51.1126068659049,-29.5274749692182,
40.10025));
#191055=CARTESIAN_POINT('Origin',(-53.2328030451449,-23.6840886581933,39.92499));
#191056=CARTESIAN_POINT('Ctrl Pts',(-57.3172883154491,-25.3107727110819,
39.92499));
#191057=CARTESIAN_POINT('Ctrl Pts',(-57.3269813337899,-25.3150883208945,
39.9348354642018));
#191058=CARTESIAN_POINT('Ctrl Pts',(-57.3363050752413,-25.3201559369469,
39.9446440828457));
#191059=CARTESIAN_POINT('Ctrl Pts',(-57.3452135417184,-25.3259384683618,
39.9543641760331));
#191060=CARTESIAN_POINT('Ctrl Pts',(-57.3538325360815,-25.3315331019385,
39.9637684240712));
#191061=CARTESIAN_POINT('Ctrl Pts',(-57.3620638476581,-25.3377977038119,
39.9730909636396));
#191062=CARTESIAN_POINT('Ctrl Pts',(-57.3698434251116,-25.3447390861652,
39.9822808977141));
#191063=CARTESIAN_POINT('Ctrl Pts',(-57.3772024263438,-25.3513052064458,
39.990974009465));
#191064=CARTESIAN_POINT('Ctrl Pts',(-57.3841579102015,-25.3584775246713,
39.9995492765002));
#191065=CARTESIAN_POINT('Ctrl Pts',(-57.3906233351697,-25.3662887884596,
40.0079462328695));
#191066=CARTESIAN_POINT('Ctrl Pts',(-57.3965784591569,-25.3734835273337,
40.015680436969));
#191067=CARTESIAN_POINT('Ctrl Pts',(-57.4021181432099,-25.3812207968882,
40.0232638017423));
#191068=CARTESIAN_POINT('Ctrl Pts',(-57.4071400767278,-25.3895423083605,
40.0306257269968));
#191069=CARTESIAN_POINT('Ctrl Pts',(-57.4085967487433,-25.3919560625142,
40.0327611416652));
#191070=CARTESIAN_POINT('Ctrl Pts',(-57.4100096047778,-25.3944190600986,
40.0348777427271));
#191071=CARTESIAN_POINT('Ctrl Pts',(-57.4113754784548,-25.3969325220922,
40.0369733168701));
#191072=CARTESIAN_POINT('Ctrl Pts',(-57.4128561733382,-25.399657276494,
40.039245053974));
#191073=CARTESIAN_POINT('Ctrl Pts',(-57.4142805418441,-25.4024370309185,
40.041487875195));
#191074=CARTESIAN_POINT('Ctrl Pts',(-57.4156446191418,-25.4052723227224,
40.0436985701601));
#191075=CARTESIAN_POINT('Ctrl Pts',(-57.4193883399888,-25.4130538033264,
40.0497658398386));
#191076=CARTESIAN_POINT('Ctrl Pts',(-57.4226343338644,-25.4212623406654,
40.0555581699984));
#191077=CARTESIAN_POINT('Ctrl Pts',(-57.425300821288,-25.4298341608307,
40.0609828468886));
#191078=CARTESIAN_POINT('Ctrl Pts',(-57.4277405125136,-25.4376769109069,
40.0659461317304));
#191079=CARTESIAN_POINT('Ctrl Pts',(-57.4296843862653,-25.445819360426,
40.0706039980705));
#191080=CARTESIAN_POINT('Ctrl Pts',(-57.4310470526568,-25.4542377154364,
40.0748843180601));
#191081=CARTESIAN_POINT('Ctrl Pts',(-57.431716389937,-25.4583727839179,
40.0769867972569));
#191082=CARTESIAN_POINT('Ctrl Pts',(-57.4322449980039,-25.4625743171737,
40.0789976708174));
#191083=CARTESIAN_POINT('Ctrl Pts',(-57.4326195921323,-25.4668384019348,
40.08090504915));
#191084=CARTESIAN_POINT('Ctrl Pts',(-57.4326906677196,-25.4676474704855,
40.0812669556105));
#191085=CARTESIAN_POINT('Ctrl Pts',(-57.4327558640765,-25.4684592045962,
40.0816253922033));
#191086=CARTESIAN_POINT('Ctrl Pts',(-57.4328151061497,-25.4692734860652,
40.081980198914));
#191087=CARTESIAN_POINT('Ctrl Pts',(-57.4328724969081,-25.4700623212382,
40.082323917915));
#191088=CARTESIAN_POINT('Ctrl Pts',(-57.4329242997219,-25.4708535470243,
40.0826642303499));
#191089=CARTESIAN_POINT('Ctrl Pts',(-57.4329704479395,-25.4716470524587,
40.08300099161));
#191090=CARTESIAN_POINT('Ctrl Pts',(-57.4334733617057,-25.4802945111766,
40.0866709464311));
#191091=CARTESIAN_POINT('Ctrl Pts',(-57.433304654289,-25.4892184175044,
40.0899175831876));
#191092=CARTESIAN_POINT('Ctrl Pts',(-57.4323852136915,-25.4982455208433,
40.0925642067059));
#191093=CARTESIAN_POINT('Ctrl Pts',(-57.4319969282177,-25.5020577226393,
40.0936818922526));
#191094=CARTESIAN_POINT('Ctrl Pts',(-57.4314751387429,-25.5058881199461,
40.094693009479));
#191095=CARTESIAN_POINT('Ctrl Pts',(-57.4308157710842,-25.5097232095984,
40.0955863397546));
#191096=CARTESIAN_POINT('Ctrl Pts',(-57.4297054124227,-25.5161814047439,
40.0970906856167));
#191097=CARTESIAN_POINT('Ctrl Pts',(-57.4282034292357,-25.5226508554406,
40.0982599215483));
#191098=CARTESIAN_POINT('Ctrl Pts',(-57.426290210937,-25.5290599831061,
40.0990497370454));
#191099=CARTESIAN_POINT('Ctrl Pts',(-57.4258119063623,-25.5306622650225,
40.0992471909196));
#191100=CARTESIAN_POINT('Ctrl Pts',(-57.4253076802625,-25.5322606952868,
40.0994209989363));
#191101=CARTESIAN_POINT('Ctrl Pts',(-57.4247769415292,-25.5338540367008,
40.0995705982975));
#191102=CARTESIAN_POINT('Ctrl Pts',(-57.4239808334292,-25.5362440488219,
40.0997949973393));
#191103=CARTESIAN_POINT('Ctrl Pts',(-57.423125065972,-25.5386225912892,
40.0999649129781));
#191104=CARTESIAN_POINT('Ctrl Pts',(-57.4222091845947,-25.540986154258,
40.1000786629733));
#191105=CARTESIAN_POINT('Ctrl Pts',(-57.4212933032174,-25.5433497172268,
40.1001924129685));
#191106=CARTESIAN_POINT('Ctrl Pts',(-57.4203173191918,-25.5456982979284,
40.10025));
#191107=CARTESIAN_POINT('Ctrl Pts',(-57.4192809246806,-25.5480287005722,
40.10025));
#191108=CARTESIAN_POINT('Ctrl Pts',(-53.9314655730806,-23.9951532569804,
40.10025));
#191109=CARTESIAN_POINT('Ctrl Pts',(-53.9349721992636,-23.9872677980944,
40.10025));
#191110=CARTESIAN_POINT('Ctrl Pts',(-53.9390993428067,-23.9797401457394,
40.0995786334242));
#191111=CARTESIAN_POINT('Ctrl Pts',(-53.9437193744788,-23.9726512030277,
40.0983063763368));
#191112=CARTESIAN_POINT('Ctrl Pts',(-53.9467034408966,-23.968072473403,
40.0974846287994));
#191113=CARTESIAN_POINT('Ctrl Pts',(-53.9498923541887,-23.963676246713,
40.0964130309339));
#191114=CARTESIAN_POINT('Ctrl Pts',(-53.9532454491206,-23.9594780769919,
40.0951176960924));
#191115=CARTESIAN_POINT('Ctrl Pts',(-53.9576897843754,-23.953913643513,
40.0934008039614));
#191116=CARTESIAN_POINT('Ctrl Pts',(-53.9624262550345,-23.9487016177218,
40.0912909372157));
#191117=CARTESIAN_POINT('Ctrl Pts',(-53.9673725153421,-23.943878485145,
40.0888630467852));
#191118=CARTESIAN_POINT('Ctrl Pts',(-53.9698456454959,-23.9414669188567,
40.0876491015699));
#191119=CARTESIAN_POINT('Ctrl Pts',(-53.9723713025229,-23.9391523931033,
40.0863558569271));
#191120=CARTESIAN_POINT('Ctrl Pts',(-53.9749397614923,-23.9369381736872,
40.0849936342771));
#191121=CARTESIAN_POINT('Ctrl Pts',(-53.9762239909769,-23.9358310639792,
40.0843125229521));
#191122=CARTESIAN_POINT('Ctrl Pts',(-53.9775189275856,-23.934749015825,
40.0836141747074));
#191123=CARTESIAN_POINT('Ctrl Pts',(-53.978823397265,-23.9336923430323,
40.082899916161));
#191124=CARTESIAN_POINT('Ctrl Pts',(-53.9791495146849,-23.9334281748341,
40.0827213515243));
#191125=CARTESIAN_POINT('Ctrl Pts',(-53.9794762280619,-23.9331655922759,
40.0825417925842));
#191126=CARTESIAN_POINT('Ctrl Pts',(-53.979803519334,-23.9329045996151,
40.0823612602361));
#191127=CARTESIAN_POINT('Ctrl Pts',(-53.9807853931504,-23.932121621633,
40.0818196631917));
#191128=CARTESIAN_POINT('Ctrl Pts',(-53.9817724673293,-23.9313529543289,
40.0812693052022));
#191129=CARTESIAN_POINT('Ctrl Pts',(-53.9827642604006,-23.9305986983574,
40.0807107531875));
#191130=CARTESIAN_POINT('Ctrl Pts',(-53.9897503227313,-23.9252858166865,
40.0767763849183));
#191131=CARTESIAN_POINT('Ctrl Pts',(-53.9969681366814,-23.9206342168333,
40.0724140586139));
#191132=CARTESIAN_POINT('Ctrl Pts',(-54.0043120126389,-23.9165878043694,
40.0677221223771));
#191133=CARTESIAN_POINT('Ctrl Pts',(-54.0078737845426,-23.9146252986969,
40.0654465383722));
#191134=CARTESIAN_POINT('Ctrl Pts',(-54.0114657535932,-23.912805342904,
40.063092800068));
#191135=CARTESIAN_POINT('Ctrl Pts',(-54.0150784217125,-23.9111228176151,
40.0606689262479));
#191136=CARTESIAN_POINT('Ctrl Pts',(-54.0206091641933,-23.9085469889526,
40.0569581447805));
#191137=CARTESIAN_POINT('Ctrl Pts',(-54.026184917604,-23.9062937028418,
40.0530843804606));
#191138=CARTESIAN_POINT('Ctrl Pts',(-54.0317609613888,-23.904351718228,
40.0490800251458));
#191139=CARTESIAN_POINT('Ctrl Pts',(-54.0343505049691,-23.9034498505268,
40.0472203818218));
#191140=CARTESIAN_POINT('Ctrl Pts',(-54.0369399534675,-23.9026149214102,
40.0453323608819));
#191141=CARTESIAN_POINT('Ctrl Pts',(-54.0395249709303,-23.9018470291825,
40.0434201572162));
#191142=CARTESIAN_POINT('Ctrl Pts',(-54.0397231023334,-23.9017881732689,
40.0432735943397));
#191143=CARTESIAN_POINT('Ctrl Pts',(-54.0399212112576,-23.9017296774344,
40.0431268995707));
#191144=CARTESIAN_POINT('Ctrl Pts',(-54.040119296488,-23.9016715408685,
40.0429800745037));
#191145=CARTESIAN_POINT('Ctrl Pts',(-54.0429017967674,-23.9008548973947,
40.0409176249753));
#191146=CARTESIAN_POINT('Ctrl Pts',(-54.0456803391391,-23.9001111074276,
40.0388310783332));
#191147=CARTESIAN_POINT('Ctrl Pts',(-54.0484499388203,-23.8994373944621,
40.036725739981));
#191148=CARTESIAN_POINT('Ctrl Pts',(-54.0583812307206,-23.8970215795835,
40.0291763710715));
#191149=CARTESIAN_POINT('Ctrl Pts',(-54.0682738483764,-23.8954862390498,
40.0213310894589));
#191150=CARTESIAN_POINT('Ctrl Pts',(-54.0780688394977,-23.8947164920947,
40.0132837551311));
#191151=CARTESIAN_POINT('Ctrl Pts',(-54.0888325507459,-23.8938706175189,
40.0044405431312));
#191152=CARTESIAN_POINT('Ctrl Pts',(-54.0994790041498,-23.8939490479889,
39.9953528710584));
#191153=CARTESIAN_POINT('Ctrl Pts',(-54.1099490937719,-23.8948487267556,
39.9861103629534));
#191154=CARTESIAN_POINT('Ctrl Pts',(-54.1212541629301,-23.8958201540352,
39.9761307737527));
#191155=CARTESIAN_POINT('Ctrl Pts',(-54.1323547778592,-23.8977489757819,
39.9659696935974));
#191156=CARTESIAN_POINT('Ctrl Pts',(-54.1431832370035,-23.9005625023838,
39.955712821746));
#191157=CARTESIAN_POINT('Ctrl Pts',(-54.1539208564994,-23.9033524263876,
39.9455419945129));
#191158=CARTESIAN_POINT('Ctrl Pts',(-54.1643921589038,-23.907012900389,
39.9352756289325));
#191159=CARTESIAN_POINT('Ctrl Pts',(-54.1745185419761,-23.9115214566111,
39.92499));
#191160=CARTESIAN_POINT('Origin',(0.00619866644048587,-0.013922432774471,
39.92499));
#191161=CARTESIAN_POINT('Ctrl Pts',(-57.4068835917981,-25.5758735661205,
40.10025));
#191162=CARTESIAN_POINT('Ctrl Pts',(-57.4033868763699,-25.5837184861902,
40.10025));
#191163=CARTESIAN_POINT('Ctrl Pts',(-57.3992659084775,-25.5912015935365,
40.0995859581842));
#191164=CARTESIAN_POINT('Ctrl Pts',(-57.3946498105264,-25.5982448512628,
40.0983275959622));
#191165=CARTESIAN_POINT('Ctrl Pts',(-57.391700343686,-25.602745157654,40.0975235624069));
#191166=CARTESIAN_POINT('Ctrl Pts',(-57.3885495044088,-25.6070664213767,
40.0964777059491));
#191167=CARTESIAN_POINT('Ctrl Pts',(-57.3852370392634,-25.6111943775537,
40.0952149915962));
#191168=CARTESIAN_POINT('Ctrl Pts',(-57.3807161889919,-25.6168282094539,
40.0934916398702));
#191169=CARTESIAN_POINT('Ctrl Pts',(-57.3758905070495,-25.6220971979012,
40.0913643921631));
#191170=CARTESIAN_POINT('Ctrl Pts',(-57.3708481654825,-25.6269642358704,
40.0889118607713));
#191171=CARTESIAN_POINT('Ctrl Pts',(-57.368326994699,-25.629397754855,40.0876855950754));
#191172=CARTESIAN_POINT('Ctrl Pts',(-57.3657515758212,-25.6317309777763,
40.0863782327527));
#191173=CARTESIAN_POINT('Ctrl Pts',(-57.3631323306533,-25.6339606331575,
40.0850006373334));
#191174=CARTESIAN_POINT('Ctrl Pts',(-57.3618227080694,-25.6350754608481,
40.0843118396238));
#191175=CARTESIAN_POINT('Ctrl Pts',(-57.3605021218763,-25.6361644125824,
40.0836054919165));
#191176=CARTESIAN_POINT('Ctrl Pts',(-57.3591718306997,-25.6372271795773,
40.0828829920418));
#191177=CARTESIAN_POINT('Ctrl Pts',(-57.3588392579055,-25.637492871326,
40.0827023670731));
#191178=CARTESIAN_POINT('Ctrl Pts',(-57.3585060784009,-25.6377569268682,
40.0825207326933));
#191179=CARTESIAN_POINT('Ctrl Pts',(-57.358172311552,-25.6380193420648,
40.0823381109276));
#191180=CARTESIAN_POINT('Ctrl Pts',(-57.3571710110052,-25.6388065876544,
40.0817902456304));
#191181=CARTESIAN_POINT('Ctrl Pts',(-57.3561644250954,-25.6395790684329,
40.0812334935553));
#191182=CARTESIAN_POINT('Ctrl Pts',(-57.3551530701151,-25.6403366878209,
40.0806684524227));
#191183=CARTESIAN_POINT('Ctrl Pts',(-57.3481639797007,-25.6455723078608,
40.0767636676138));
#191184=CARTESIAN_POINT('Ctrl Pts',(-57.3409484573003,-25.6501539027773,
40.072440451089));
#191185=CARTESIAN_POINT('Ctrl Pts',(-57.3336101450131,-25.6541395203645,
40.0677949937412));
#191186=CARTESIAN_POINT('Ctrl Pts',(-57.3299630239495,-25.6561203613651,
40.0654862141907));
#191187=CARTESIAN_POINT('Ctrl Pts',(-57.3262850026764,-25.6579537739809,
40.0630972003217));
#191188=CARTESIAN_POINT('Ctrl Pts',(-57.322586011576,-25.6596454116601,
40.0606363359906));
#191189=CARTESIAN_POINT('Ctrl Pts',(-57.3144254847133,-25.6633774170495,
40.0552073017124));
#191190=CARTESIAN_POINT('Ctrl Pts',(-57.3061689349813,-25.6664302835891,
40.0494204304519));
#191191=CARTESIAN_POINT('Ctrl Pts',(-57.2979615485275,-25.6688109525045,
40.0434049749851));
#191192=CARTESIAN_POINT('Ctrl Pts',(-57.2949632867553,-25.6696806408811,
40.0412074532442));
#191193=CARTESIAN_POINT('Ctrl Pts',(-57.2919705472984,-25.6704685134245,
40.0389814735788));
#191194=CARTESIAN_POINT('Ctrl Pts',(-57.2889874285391,-25.6711779534201,
40.0367321210017));
#191195=CARTESIAN_POINT('Ctrl Pts',(-57.2789674482897,-25.6735608872949,
40.0291767837137));
#191196=CARTESIAN_POINT('Ctrl Pts',(-57.2689905373618,-25.675065836079,
40.0213235332567));
#191197=CARTESIAN_POINT('Ctrl Pts',(-57.2591158425054,-25.6758066569113,
40.0132649215845));
#191198=CARTESIAN_POINT('Ctrl Pts',(-57.2482623831237,-25.6766209067621,
40.0044075527514));
#191199=CARTESIAN_POINT('Ctrl Pts',(-57.2375317496099,-25.6765122533357,
39.9953016253696));
#191200=CARTESIAN_POINT('Ctrl Pts',(-57.226983668105,-25.6755822344123,
39.9860353422328));
#191201=CARTESIAN_POINT('Ctrl Pts',(-57.2156229323747,-25.6745805641837,
39.9760551582659));
#191202=CARTESIAN_POINT('Ctrl Pts',(-57.204472765785,-25.6726261321656,
39.9658879738112));
#191203=CARTESIAN_POINT('Ctrl Pts',(-57.1936020065619,-25.6697890043832,
39.9556174643203));
#191204=CARTESIAN_POINT('Ctrl Pts',(-57.1828780392947,-25.6669901874057,
39.9454856413871));
#191205=CARTESIAN_POINT('Ctrl Pts',(-57.1724247063442,-25.6633316989619,
39.9352519465097));
#191206=CARTESIAN_POINT('Ctrl Pts',(-57.1623216544372,-25.6588335304438,
39.92499));
#191207=CARTESIAN_POINT('Ctrl Pts',(-54.0195518809642,-24.259582275973,
39.92499));
#191208=CARTESIAN_POINT('Ctrl Pts',(-54.009883204825,-24.2552775040068,
39.9348107241744));
#191209=CARTESIAN_POINT('Ctrl Pts',(-54.0005888273895,-24.2502256060956,
39.9446038383213));
#191210=CARTESIAN_POINT('Ctrl Pts',(-53.9917150968443,-24.2444615420256,
39.9543158069449));
#191211=CARTESIAN_POINT('Ctrl Pts',(-53.9831467292584,-24.2388958310217,
39.9636935671468));
#191212=CARTESIAN_POINT('Ctrl Pts',(-53.9749695397803,-24.232665370906,
39.9729968321077));
#191213=CARTESIAN_POINT('Ctrl Pts',(-53.9672483343977,-24.2257620156131,
39.9821731151436));
#191214=CARTESIAN_POINT('Ctrl Pts',(-53.9599493771797,-24.2192361828646,
39.9908475764458));
#191215=CARTESIAN_POINT('Ctrl Pts',(-53.9530572218243,-24.2121084368813,
39.9994093733958));
#191216=CARTESIAN_POINT('Ctrl Pts',(-53.9466592127591,-24.2043454826836,
40.0077966115958));
#191217=CARTESIAN_POINT('Ctrl Pts',(-53.9407667537449,-24.197195932101,
40.0155211172713));
#191218=CARTESIAN_POINT('Ctrl Pts',(-53.9352931333904,-24.1895071355333,
40.0230979941141));
#191219=CARTESIAN_POINT('Ctrl Pts',(-53.9303412916313,-24.1812372959513,
40.0304554104869));
#191220=CARTESIAN_POINT('Ctrl Pts',(-53.9288647523808,-24.17877139673,40.0326492435261));
#191221=CARTESIAN_POINT('Ctrl Pts',(-53.9274348719401,-24.1762537459482,
40.03482337151));
#191222=CARTESIAN_POINT('Ctrl Pts',(-53.9260551099577,-24.1736830183707,
40.0369753512355));
#191223=CARTESIAN_POINT('Ctrl Pts',(-53.9246894457403,-24.1711385572896,
40.0391053430352));
#191224=CARTESIAN_POINT('Ctrl Pts',(-53.923374056695,-24.1685448683466,
40.041211089324));
#191225=CARTESIAN_POINT('Ctrl Pts',(-53.9221135831989,-24.1659037306809,
40.0432881154904));
#191226=CARTESIAN_POINT('Ctrl Pts',(-53.9220259323371,-24.1657200711329,
40.043432547828));
#191227=CARTESIAN_POINT('Ctrl Pts',(-53.9219385350607,-24.1655361818117,
40.0435768364421));
#191228=CARTESIAN_POINT('Ctrl Pts',(-53.9218513926272,-24.1653520623706,
40.0437209807855));
#191229=CARTESIAN_POINT('Ctrl Pts',(-53.9180307491142,-24.1572795915924,
40.0500407968421));
#191230=CARTESIAN_POINT('Ctrl Pts',(-53.9147442868247,-24.1487557177452,
40.0560490279346));
#191231=CARTESIAN_POINT('Ctrl Pts',(-53.9120963197572,-24.1398315880188,
40.0616647108617));
#191232=CARTESIAN_POINT('Ctrl Pts',(-53.9096279542366,-24.1315127481104,
40.0668995033489));
#191233=CARTESIAN_POINT('Ctrl Pts',(-53.9077144433429,-24.1228452895794,
40.0717933267486));
#191234=CARTESIAN_POINT('Ctrl Pts',(-53.906468142013,-24.1138798870151,
40.0762460303077));
#191235=CARTESIAN_POINT('Ctrl Pts',(-53.9060122288629,-24.1106002267701,
40.0778748868751));
#191236=CARTESIAN_POINT('Ctrl Pts',(-53.9056458829917,-24.1072808472547,
40.0794443522249));
#191237=CARTESIAN_POINT('Ctrl Pts',(-53.9053756337487,-24.1039248822478,
40.0809482021492));
#191238=CARTESIAN_POINT('Ctrl Pts',(-53.905310647834,-24.1031178847765,
40.0813098278169));
#191239=CARTESIAN_POINT('Ctrl Pts',(-53.9052515154467,-24.1023082689116,
40.0816679525672));
#191240=CARTESIAN_POINT('Ctrl Pts',(-53.9051983068758,-24.101496150709,
40.0820224192581));
#191241=CARTESIAN_POINT('Ctrl Pts',(-53.9051467610727,-24.1007094112001,
40.0823658088648));
#191242=CARTESIAN_POINT('Ctrl Pts',(-53.9051007746215,-24.0999203233285,
40.0827057654617));
#191243=CARTESIAN_POINT('Ctrl Pts',(-53.9050604098635,-24.0991289960599,
40.0830421470151));
#191244=CARTESIAN_POINT('Ctrl Pts',(-53.904618167291,-24.090459091316,40.0867275956805));
#191245=CARTESIAN_POINT('Ctrl Pts',(-53.9048508523205,-24.0815146560292,
40.0899823432028));
#191246=CARTESIAN_POINT('Ctrl Pts',(-53.9058331609931,-24.0724687639699,
40.0926299529353));
#191247=CARTESIAN_POINT('Ctrl Pts',(-53.9062405536792,-24.0687171629032,
40.0937279956083));
#191248=CARTESIAN_POINT('Ctrl Pts',(-53.9067765048111,-24.0649483109702,
40.0947220371802));
#191249=CARTESIAN_POINT('Ctrl Pts',(-53.9074445642443,-24.0611749820058,
40.0956014538693));
#191250=CARTESIAN_POINT('Ctrl Pts',(-53.9085840092242,-24.0547391762489,
40.097101390674));
#191251=CARTESIAN_POINT('Ctrl Pts',(-53.9101092267074,-24.0482923662126,
40.0982667904316));
#191252=CARTESIAN_POINT('Ctrl Pts',(-53.9120381043537,-24.0419050995276,
40.0990539325583));
#191253=CARTESIAN_POINT('Ctrl Pts',(-53.9130025431769,-24.0387114661851,
40.0994475036216));
#191254=CARTESIAN_POINT('Ctrl Pts',(-53.9140692448461,-24.0355332447502,
40.0997467259952));
#191255=CARTESIAN_POINT('Ctrl Pts',(-53.9152404736265,-24.0323793130073,
40.0999473488896));
#191256=CARTESIAN_POINT('Ctrl Pts',(-53.9164117024069,-24.0292253812645,
40.100147971784));
#191257=CARTESIAN_POINT('Ctrl Pts',(-53.9176874253155,-24.0260957707894,
40.10025));
#191258=CARTESIAN_POINT('Ctrl Pts',(-53.9190682401996,-24.0229981225294,
40.10025));
#191259=CARTESIAN_POINT('Origin',(-55.4168495715593,-17.9900016446779,39.92499));
#191260=CARTESIAN_POINT('Ctrl Pts',(-59.6489943884565,-19.1808295835778,
39.92499));
#191261=CARTESIAN_POINT('Ctrl Pts',(-59.6590854114904,-19.1841083557167,
39.934835464202));
#191262=CARTESIAN_POINT('Ctrl Pts',(-59.668887786629,-19.1881736144724,
39.9446440828463));
#191263=CARTESIAN_POINT('Ctrl Pts',(-59.6783518907174,-19.1929932802643,
39.9543641760338));
#191264=CARTESIAN_POINT('Ctrl Pts',(-59.6875084677779,-19.1976563356173,
39.9637684240721));
#191265=CARTESIAN_POINT('Ctrl Pts',(-59.6963495165753,-19.2030262129965,
39.9730909636406));
#191266=CARTESIAN_POINT('Ctrl Pts',(-59.70481204872,-19.2091163824551,39.9822808977152));
#191267=CARTESIAN_POINT('Ctrl Pts',(-59.7128170830362,-19.2148773077518,
39.9909740094662));
#191268=CARTESIAN_POINT('Ctrl Pts',(-59.7204841754278,-19.2212832892289,
39.9995492765015));
#191269=CARTESIAN_POINT('Ctrl Pts',(-59.7277306815217,-19.2283759411608,
40.0079462328709));
#191270=CARTESIAN_POINT('Ctrl Pts',(-59.7344052377148,-19.2349087865438,
40.0156804369706));
#191271=CARTESIAN_POINT('Ctrl Pts',(-59.7407233396955,-19.2420246158653,
40.0232638017439));
#191272=CARTESIAN_POINT('Ctrl Pts',(-59.7465875973425,-19.2497756062341,
40.0306257269984));
#191273=CARTESIAN_POINT('Ctrl Pts',(-59.7482885955682,-19.2520238739022,
40.0327611416664));
#191274=CARTESIAN_POINT('Ctrl Pts',(-59.7499511651817,-19.2543256952574,
40.0348777427277));
#191275=CARTESIAN_POINT('Ctrl Pts',(-59.751572284779,-19.2566826155661,
40.0369733168701));
#191276=CARTESIAN_POINT('Ctrl Pts',(-59.7533296826513,-19.2592376687175,
40.039245053974));
#191277=CARTESIAN_POINT('Ctrl Pts',(-59.7550368117758,-19.2618533083053,
40.041487875195));
#191278=CARTESIAN_POINT('Ctrl Pts',(-59.7566897852105,-19.2645304831804,
40.0436985701601));
#191279=CARTESIAN_POINT('Ctrl Pts',(-59.7612263837726,-19.2718780106324,
40.0497658398386));
#191280=CARTESIAN_POINT('Ctrl Pts',(-59.7653126215477,-19.2797022819934,
40.0555581699984));
#191281=CARTESIAN_POINT('Ctrl Pts',(-59.7688605008635,-19.2879484209983,
40.0609828468886));
#191282=CARTESIAN_POINT('Ctrl Pts',(-59.7721066178186,-19.2954931904946,
40.0659461317305));
#191283=CARTESIAN_POINT('Ctrl Pts',(-59.7748909605621,-19.3033878446875,
40.0706039980708));
#191284=CARTESIAN_POINT('Ctrl Pts',(-59.7771261198371,-19.3116176456448,
40.0748843180605));
#191285=CARTESIAN_POINT('Ctrl Pts',(-59.7782240227714,-19.3156600969909,
40.0769867972571));
#191286=CARTESIAN_POINT('Ctrl Pts',(-59.7791889148824,-19.3197833592187,
40.0789976708175));
#191287=CARTESIAN_POINT('Ctrl Pts',(-59.7800071751723,-19.3239849291284,
40.08090504915));
#191288=CARTESIAN_POINT('Ctrl Pts',(-59.7801624320924,-19.324782136095,
40.0812669556105));
#191289=CARTESIAN_POINT('Ctrl Pts',(-59.780312120616,-19.3255826085664,
40.0816253922032));
#191290=CARTESIAN_POINT('Ctrl Pts',(-59.7804561537455,-19.3263862368333,
40.0819801989139));
#191291=CARTESIAN_POINT('Ctrl Pts',(-59.7805956858398,-19.327164751717,
40.0823239179149));
#191292=CARTESIAN_POINT('Ctrl Pts',(-59.7807299104879,-19.327946228217,
40.0826642303498));
#191293=CARTESIAN_POINT('Ctrl Pts',(-59.7808587498044,-19.3287305629433,
40.0830009916099));
#191294=CARTESIAN_POINT('Ctrl Pts',(-59.7822628141274,-19.3372780811746,
40.0866709464312));
#191295=CARTESIAN_POINT('Ctrl Pts',(-59.7830278331223,-19.3461707361371,
40.0899175831877));
#191296=CARTESIAN_POINT('Ctrl Pts',(-59.7830570185564,-19.3552444957724,
40.0925642067062));
#191297=CARTESIAN_POINT('Ctrl Pts',(-59.7830693437464,-19.3590764008118,
40.0936818922527));
#191298=CARTESIAN_POINT('Ctrl Pts',(-59.7829507982331,-19.362940356653,
40.0946930094791));
#191299=CARTESIAN_POINT('Ctrl Pts',(-59.7826959186873,-19.3668233599707,
40.0955863397546));
#191300=CARTESIAN_POINT('Ctrl Pts',(-59.7822667079008,-19.373362240532,
40.0970906856166));
#191301=CARTESIAN_POINT('Ctrl Pts',(-59.7814491944743,-19.3799532508953,
40.0982599215483));
#191302=CARTESIAN_POINT('Ctrl Pts',(-59.780216393251,-19.3865272544574,
40.0990497370454));
#191303=CARTESIAN_POINT('Ctrl Pts',(-59.7799081929452,-19.3881707553479,
40.0992471909196));
#191304=CARTESIAN_POINT('Ctrl Pts',(-59.7795738105079,-19.3898131352233,
40.0994209989363));
#191305=CARTESIAN_POINT('Ctrl Pts',(-59.7792125287464,-19.3914532254506,
40.0995705982975));
#191306=CARTESIAN_POINT('Ctrl Pts',(-59.7786706061041,-19.3939133607915,
40.0997949973393));
#191307=CARTESIAN_POINT('Ctrl Pts',(-59.7780681520196,-19.3963683254115,
40.0999649129781));
#191308=CARTESIAN_POINT('Ctrl Pts',(-59.7774043475413,-19.398814676208,
40.1000786629733));
#191309=CARTESIAN_POINT('Ctrl Pts',(-59.7767405430631,-19.4012610270045,
40.1001924129685));
#191310=CARTESIAN_POINT('Ctrl Pts',(-59.7760153991102,-19.4036987600451,
40.10025));
#191311=CARTESIAN_POINT('Ctrl Pts',(-59.7752282754838,-19.406124729225,
40.10025));
#191312=CARTESIAN_POINT('Ctrl Pts',(-56.1441998575528,-18.2263320786579,
40.10025));
#191313=CARTESIAN_POINT('Ctrl Pts',(-56.1468630191714,-18.2181232748941,
40.10025));
#191314=CARTESIAN_POINT('Ctrl Pts',(-56.1501806998579,-18.2102054558337,
40.0995786334241));
#191315=CARTESIAN_POINT('Ctrl Pts',(-56.1540344262254,-18.2026724222806,
40.0983063763366));
#191316=CARTESIAN_POINT('Ctrl Pts',(-56.1565235380436,-18.1978068555394,
40.0974846287992));
#191317=CARTESIAN_POINT('Ctrl Pts',(-56.1592354513148,-18.1931013796336,
40.0964130309338));
#191318=CARTESIAN_POINT('Ctrl Pts',(-56.1621313494121,-18.1885757140655,
40.0951176960924));
#191319=CARTESIAN_POINT('Ctrl Pts',(-56.1659696964528,-18.182577203601,
40.0934008039614));
#191320=CARTESIAN_POINT('Ctrl Pts',(-56.1701354151837,-18.176898633833,
40.0912909372157));
#191321=CARTESIAN_POINT('Ctrl Pts',(-56.1745504247234,-18.1715848978924,
40.0888630467852));
#191322=CARTESIAN_POINT('Ctrl Pts',(-56.1767579294932,-18.168928029922,
40.0876491015699));
#191323=CARTESIAN_POINT('Ctrl Pts',(-56.1790278168866,-18.1663621803351,
40.0863558569271));
#191324=CARTESIAN_POINT('Ctrl Pts',(-56.181350756616,-18.1638916135756,
40.0849936342771));
#191325=CARTESIAN_POINT('Ctrl Pts',(-56.1825122264807,-18.1626563301959,
40.0843125229521));
#191326=CARTESIAN_POINT('Ctrl Pts',(-56.1836869644605,-18.161444851881,
40.0836141747074));
#191327=CARTESIAN_POINT('Ctrl Pts',(-56.1848738357353,-18.1602576134414,
40.082899916161));
#191328=CARTESIAN_POINT('Ctrl Pts',(-56.185170553554,-18.1599608038315,
40.0827213515244));
#191329=CARTESIAN_POINT('Ctrl Pts',(-56.1854680298097,-18.1596655088808,
40.0825417925842));
#191330=CARTESIAN_POINT('Ctrl Pts',(-56.1857662469842,-18.1593717347115,
40.0823612602361));
#191331=CARTESIAN_POINT('Ctrl Pts',(-56.1866608985078,-18.1584904122035,
40.0818196631918));
#191332=CARTESIAN_POINT('Ctrl Pts',(-56.187562217779,-18.1576227783922,
40.0812693052022));
#191333=CARTESIAN_POINT('Ctrl Pts',(-56.1884697364865,-18.1567689837083,
40.0807107531875));
#191334=CARTESIAN_POINT('Ctrl Pts',(-56.1948621810804,-18.1507549641992,
40.0767763849182));
#191335=CARTESIAN_POINT('Ctrl Pts',(-56.2015542305061,-18.1453743792963,
40.0724140586137));
#191336=CARTESIAN_POINT('Ctrl Pts',(-56.2084349106663,-18.1405824894349,
40.0677221223768));
#191337=CARTESIAN_POINT('Ctrl Pts',(-56.2117720331086,-18.1382584280303,
40.0654465383721));
#191338=CARTESIAN_POINT('Ctrl Pts',(-56.2151540877945,-18.1360729791408,
40.0630928000679));
#191339=CARTESIAN_POINT('Ctrl Pts',(-56.2185710935569,-18.1340220442548,
40.0606689262479));
#191340=CARTESIAN_POINT('Ctrl Pts',(-56.2238022906399,-18.130882206239,
40.0569581447806));
#191341=CARTESIAN_POINT('Ctrl Pts',(-56.2291119669556,-18.1280584389296,
40.0530843804606));
#191342=CARTESIAN_POINT('Ctrl Pts',(-56.2344544719217,-18.1255442374228,
40.0490800251458));
#191343=CARTESIAN_POINT('Ctrl Pts',(-56.2369355588664,-18.1243766292362,
40.0472203818218));
#191344=CARTESIAN_POINT('Ctrl Pts',(-56.2394235482376,-18.1232756028764,
40.0453323608819));
#191345=CARTESIAN_POINT('Ctrl Pts',(-56.2419141381098,-18.1222417093398,
40.0434201572162));
#191346=CARTESIAN_POINT('Ctrl Pts',(-56.2421050320101,-18.122162465474,
40.0432735943397));
#191347=CARTESIAN_POINT('Ctrl Pts',(-56.2422959411932,-18.1220835820643,
40.0431268995708));
#191348=CARTESIAN_POINT('Ctrl Pts',(-56.2424868643661,-18.1220050584319,
40.0429800745037));
#191349=CARTESIAN_POINT('Ctrl Pts',(-56.2451687593304,-18.1209020381383,
40.0409176249753));
#191350=CARTESIAN_POINT('Ctrl Pts',(-56.247854333334,-18.1198718859662,
40.0388310783333));
#191351=CARTESIAN_POINT('Ctrl Pts',(-56.2505383386774,-18.1189123616723,
40.036725739981));
#191352=CARTESIAN_POINT('Ctrl Pts',(-56.2601627045042,-18.1154716782,40.029176371072));
#191353=CARTESIAN_POINT('Ctrl Pts',(-56.2698406425781,-18.1129106883012,
40.0213310894599));
#191354=CARTESIAN_POINT('Ctrl Pts',(-56.2795015152461,-18.1111213027308,
40.0132837551327));
#191355=CARTESIAN_POINT('Ctrl Pts',(-56.2901178437879,-18.1091549477487,
40.0044405431333));
#191356=CARTESIAN_POINT('Ctrl Pts',(-56.3007141730221,-18.1081200911547,
39.9953528710609));
#191357=CARTESIAN_POINT('Ctrl Pts',(-56.3112209484361,-18.1079204190084,
39.9861103629564));
#191358=CARTESIAN_POINT('Ctrl Pts',(-56.3225656290429,-18.1077048232012,
39.9761307737561));
#191359=CARTESIAN_POINT('Ctrl Pts',(-56.3338070504147,-18.1084627484405,
39.9659696936013));
#191360=CARTESIAN_POINT('Ctrl Pts',(-56.3448702837385,-18.1101289800549,
39.9557128217503));
#191361=CARTESIAN_POINT('Ctrl Pts',(-56.3558407079016,-18.1117812336981,
39.9455419945158));
#191362=CARTESIAN_POINT('Ctrl Pts',(-56.3666372711396,-18.1143271060913,
39.9352756289339));
#191363=CARTESIAN_POINT('Ctrl Pts',(-56.3771794532808,-18.1177524687103,
39.92499));
#191364=CARTESIAN_POINT('Origin',(0.00470941899428508,-0.0144941013083364,
39.92499));
#191365=CARTESIAN_POINT('Ctrl Pts',(-59.7658094374952,-19.4351129318417,
40.10025));
#191366=CARTESIAN_POINT('Ctrl Pts',(-59.7631518948791,-19.4432803829096,
40.10025));
#191367=CARTESIAN_POINT('Ctrl Pts',(-59.7598356997909,-19.4511532554527,
40.0995859581841));
#191368=CARTESIAN_POINT('Ctrl Pts',(-59.7559811102133,-19.4586404431021,
40.0983275959617));
#191369=CARTESIAN_POINT('Ctrl Pts',(-59.7535182109725,-19.4634243995794,
40.0975235624065));
#191370=CARTESIAN_POINT('Ctrl Pts',(-59.7508363273792,-19.4680513433541,
40.0964777059489));
#191371=CARTESIAN_POINT('Ctrl Pts',(-59.7479734971807,-19.4725029330458,
40.0952149915961));
#191372=CARTESIAN_POINT('Ctrl Pts',(-59.7440663083908,-19.4785784597569,
40.0934916398701));
#191373=CARTESIAN_POINT('Ctrl Pts',(-59.7398178213043,-19.4843230052518,
40.0913643921631));
#191374=CARTESIAN_POINT('Ctrl Pts',(-59.7353118462117,-19.489690449293,
40.0889118607713));
#191375=CARTESIAN_POINT('Ctrl Pts',(-59.7330588586654,-19.4923741713137,
40.0876855950754));
#191376=CARTESIAN_POINT('Ctrl Pts',(-59.7307414364081,-19.4949638171732,
40.0863782327527));
#191377=CARTESIAN_POINT('Ctrl Pts',(-59.7283696021899,-19.4974550439412,
40.0850006373334));
#191378=CARTESIAN_POINT('Ctrl Pts',(-59.7271836850807,-19.4987006573253,
40.0843118396237));
#191379=CARTESIAN_POINT('Ctrl Pts',(-59.7259841596484,-19.4999216825135,
40.0836054919164));
#191380=CARTESIAN_POINT('Ctrl Pts',(-59.7247722453468,-19.5011176808519,
40.0828829920418));
#191381=CARTESIAN_POINT('Ctrl Pts',(-59.7244692667714,-19.5014166804365,
40.0827023670731));
#191382=CARTESIAN_POINT('Ctrl Pts',(-59.7241655137791,-19.5017141161965,
40.0825207326933));
#191383=CARTESIAN_POINT('Ctrl Pts',(-59.7238610051971,-19.5020099819909,
40.0823381109275));
#191384=CARTESIAN_POINT('Ctrl Pts',(-59.7229474794512,-19.5028975793742,
40.0817902456303));
#191385=CARTESIAN_POINT('Ctrl Pts',(-59.722027153953,-19.5037710453005,
40.0812334935553));
#191386=CARTESIAN_POINT('Ctrl Pts',(-59.7211005320715,-19.5046302297522,
40.0806684524227));
#191387=CARTESIAN_POINT('Ctrl Pts',(-59.7146969999426,-19.5105677273984,
40.0767636676136));
#191388=CARTESIAN_POINT('Ctrl Pts',(-59.7079999120046,-19.5158784513269,
40.0724404510887));
#191389=CARTESIAN_POINT('Ctrl Pts',(-59.7011184102413,-19.5206092977904,
40.0677949937408));
#191390=CARTESIAN_POINT('Ctrl Pts',(-59.6976983227544,-19.5229605154967,
40.0654862141905));
#191391=CARTESIAN_POINT('Ctrl Pts',(-59.6942320938702,-19.5251683423979,
40.0630972003216));
#191392=CARTESIAN_POINT('Ctrl Pts',(-59.6907301905172,-19.527237362964,
40.0606363359906));
#191393=CARTESIAN_POINT('Ctrl Pts',(-59.6830044686627,-19.5318019313699,
40.0552073017124));
#191394=CARTESIAN_POINT('Ctrl Pts',(-59.675112260622,-19.5357011184425,
40.0494204304519));
#191395=CARTESIAN_POINT('Ctrl Pts',(-59.6671986827532,-19.538926651298,
40.0434049749851));
#191396=CARTESIAN_POINT('Ctrl Pts',(-59.6643077529623,-19.5401049791262,
40.0412074532442));
#191397=CARTESIAN_POINT('Ctrl Pts',(-59.6614137631514,-19.5412013620777,
40.0389814735788));
#191398=CARTESIAN_POINT('Ctrl Pts',(-59.6585211429014,-19.5422187365065,
40.0367321210017));
#191399=CARTESIAN_POINT('Ctrl Pts',(-59.6488051375686,-19.5456359895575,
40.0291767837139));
#191400=CARTESIAN_POINT('Ctrl Pts',(-59.6390401911867,-19.5481755652421,
40.0213235332572));
#191401=CARTESIAN_POINT('Ctrl Pts',(-59.6292970278053,-19.549944514459,
40.0132649215852));
#191402=CARTESIAN_POINT('Ctrl Pts',(-59.6185881370957,-19.5518887991941,
40.0044075527524));
#191403=CARTESIAN_POINT('Ctrl Pts',(-59.6079049297397,-19.5529023976137,
39.9953016253709));
#191404=CARTESIAN_POINT('Ctrl Pts',(-59.5973174182803,-19.5530800481815,
39.9860353422344));
#191405=CARTESIAN_POINT('Ctrl Pts',(-59.5859142147997,-19.5532713854548,
39.9760551582678));
#191406=CARTESIAN_POINT('Ctrl Pts',(-59.5746208362142,-19.5524931697987,
39.9658879738135));
#191407=CARTESIAN_POINT('Ctrl Pts',(-59.5635130675406,-19.5508078878555,
39.9556174643229));
#191408=CARTESIAN_POINT('Ctrl Pts',(-59.5525552912495,-19.5491453629089,
39.9454856413888));
#191409=CARTESIAN_POINT('Ctrl Pts',(-59.5417768065749,-19.5465995868768,
39.9352519465105));
#191410=CARTESIAN_POINT('Ctrl Pts',(-59.5312589135997,-19.5431821162863,
39.92499));
#191411=CARTESIAN_POINT('Ctrl Pts',(-56.259443978424,-18.4801050014187,
39.92499));
#191412=CARTESIAN_POINT('Ctrl Pts',(-56.2493782971083,-18.4768344633033,
39.934810724172));
#191413=CARTESIAN_POINT('Ctrl Pts',(-56.2396067681219,-18.4727817672089,
39.9446038383166));
#191414=CARTESIAN_POINT('Ctrl Pts',(-56.2301791400438,-18.4679768367037,
39.9543158069379));
#191415=CARTESIAN_POINT('Ctrl Pts',(-56.221075935655,-18.4633372535445,
39.9636935671385));
#191416=CARTESIAN_POINT('Ctrl Pts',(-56.2122922812561,-18.4579956735924,
39.9729968320981));
#191417=CARTESIAN_POINT('Ctrl Pts',(-56.2038917763252,-18.4519372213367,
39.9821731151327));
#191418=CARTESIAN_POINT('Ctrl Pts',(-56.1959506682901,-18.4462100865652,
39.9908475764345));
#191419=CARTESIAN_POINT('Ctrl Pts',(-56.1883512165489,-18.4398418135292,
39.9994093733839));
#191420=CARTESIAN_POINT('Ctrl Pts',(-56.1811768067742,-18.4327901596635,
40.0077966115835));
#191421=CARTESIAN_POINT('Ctrl Pts',(-56.1745692957314,-18.4262957047536,
40.015521117259));
#191422=CARTESIAN_POINT('Ctrl Pts',(-56.1683219623521,-18.419221177343,
40.0230979941019));
#191423=CARTESIAN_POINT('Ctrl Pts',(-56.1625328136768,-18.4115142492179,
40.0304554104747));
#191424=CARTESIAN_POINT('Ctrl Pts',(-56.1608066064034,-18.4092161988253,
40.032649243518));
#191425=CARTESIAN_POINT('Ctrl Pts',(-56.1591213928268,-18.4068618031988,
40.034823371506));
#191426=CARTESIAN_POINT('Ctrl Pts',(-56.1574804751188,-18.4044493827312,
40.0369753512356));
#191427=CARTESIAN_POINT('Ctrl Pts',(-56.1558563235462,-18.4020616112561,
40.0391053430352));
#191428=CARTESIAN_POINT('Ctrl Pts',(-56.1542770260204,-18.399619626408,
40.041211089324));
#191429=CARTESIAN_POINT('Ctrl Pts',(-56.1527473834685,-18.3971247125284,
40.0432881154904));
#191430=CARTESIAN_POINT('Ctrl Pts',(-56.1526410151169,-18.3969512210965,
40.043432547828));
#191431=CARTESIAN_POINT('Ctrl Pts',(-56.1525348749437,-18.3967774746432,
40.0435768364421));
#191432=CARTESIAN_POINT('Ctrl Pts',(-56.1524289641634,-18.3966034726923,
40.0437209807855));
#191433=CARTESIAN_POINT('Ctrl Pts',(-56.1477854475702,-18.3889745897489,
40.050040796842));
#191434=CARTESIAN_POINT('Ctrl Pts',(-56.1436260014306,-18.3808409394271,
40.0560490279345));
#191435=CARTESIAN_POINT('Ctrl Pts',(-56.1400597146374,-18.3722424849456,
40.0616647108616));
#191436=CARTESIAN_POINT('Ctrl Pts',(-56.1367353155297,-18.3642272309674,
40.0668995033487));
#191437=CARTESIAN_POINT('Ctrl Pts',(-56.1339262909282,-18.3558072700344,
40.0717933267484));
#191438=CARTESIAN_POINT('Ctrl Pts',(-56.1317496772148,-18.3470212548463,
40.0762460303075));
#191439=CARTESIAN_POINT('Ctrl Pts',(-56.1309534437592,-18.343807216824,
40.077874886875));
#191440=CARTESIAN_POINT('Ctrl Pts',(-56.1302421351291,-18.3405443147878,
40.0794443522248));
#191441=CARTESIAN_POINT('Ctrl Pts',(-56.1296225724748,-18.3372349828462,
40.0809482021492));
#191442=CARTESIAN_POINT('Ctrl Pts',(-56.1294735883542,-18.3364391990693,
40.0813098278168));
#191443=CARTESIAN_POINT('Ctrl Pts',(-56.1293301519981,-18.3356401993824,
40.0816679525672));
#191444=CARTESIAN_POINT('Ctrl Pts',(-56.1291923454416,-18.3348380918583,
40.0820224192581));
#191445=CARTESIAN_POINT('Ctrl Pts',(-56.12905884534,-18.3340610501944,40.0823658088648));
#191446=CARTESIAN_POINT('Ctrl Pts',(-56.1289306286648,-18.3332810919218,
40.0827057654617));
#191447=CARTESIAN_POINT('Ctrl Pts',(-56.1288077688059,-18.3324983188929,
40.0830421470151));
#191448=CARTESIAN_POINT('Ctrl Pts',(-56.1274616970649,-18.3239221357306,
40.0867275956806));
#191449=CARTESIAN_POINT('Ctrl Pts',(-56.126758159346,-18.3150023767874,
40.089982343203));
#191450=CARTESIAN_POINT('Ctrl Pts',(-56.1267895336332,-18.3059033598551,
40.0926299529355));
#191451=CARTESIAN_POINT('Ctrl Pts',(-56.1268025454852,-18.3021297263204,
40.0937279956084));
#191452=CARTESIAN_POINT('Ctrl Pts',(-56.1269416083199,-18.2983254984046,
40.0947220371802));
#191453=CARTESIAN_POINT('Ctrl Pts',(-56.1272115877755,-18.2945030089054,
40.0956014538692));
#191454=CARTESIAN_POINT('Ctrl Pts',(-56.127672065871,-18.2879833547331,
40.097101390674));
#191455=CARTESIAN_POINT('Ctrl Pts',(-56.1285150529071,-18.2814124323571,
40.0982667904316));
#191456=CARTESIAN_POINT('Ctrl Pts',(-56.1297657127887,-18.274858533171,
40.0990539325583));
#191457=CARTESIAN_POINT('Ctrl Pts',(-56.1303910427295,-18.271581583578,
40.0994475036216));
#191458=CARTESIAN_POINT('Ctrl Pts',(-56.1311196862928,-18.2683092720864,
40.0997467259952));
#191459=CARTESIAN_POINT('Ctrl Pts',(-56.1319548233211,-18.2650501911671,
40.0999473488896));
#191460=CARTESIAN_POINT('Ctrl Pts',(-56.1327899603494,-18.2617911102478,
40.100147971784));
#191461=CARTESIAN_POINT('Ctrl Pts',(-56.1337315613409,-18.2585452947512,
40.10025));
#191462=CARTESIAN_POINT('Ctrl Pts',(-56.1347810195643,-18.2553202812746,
40.10025));
#191463=CARTESIAN_POINT('Origin',(-56.9937374973464,-12.0988124084936,39.92499));
#191464=CARTESIAN_POINT('Ctrl Pts',(-61.3271735965894,-12.8407372733094,
39.92499));
#191465=CARTESIAN_POINT('Ctrl Pts',(-61.3375520649564,-12.8429432848609,
39.9348354642022));
#191466=CARTESIAN_POINT('Ctrl Pts',(-61.347725676909,-12.8459616464942,
39.9446440828466));
#191467=CARTESIAN_POINT('Ctrl Pts',(-61.3576417279037,-12.8497656413962,
39.9543641760342));
#191468=CARTESIAN_POINT('Ctrl Pts',(-61.3672355662873,-12.8534460291151,
39.9637684240726));
#191469=CARTESIAN_POINT('Ctrl Pts',(-61.3765894879248,-12.8578623484998,
39.9730909636412));
#191470=CARTESIAN_POINT('Ctrl Pts',(-61.3856422574875,-12.8630345798924,
39.9822808977158));
#191471=CARTESIAN_POINT('Ctrl Pts',(-61.3942056200565,-12.8679271923022,
39.9909740094669));
#191472=CARTESIAN_POINT('Ctrl Pts',(-61.4025003187134,-12.8734966517571,
39.9995492765022));
#191473=CARTESIAN_POINT('Ctrl Pts',(-61.4104485116956,-12.8797929832537,
40.0079462328716));
#191474=CARTESIAN_POINT('Ctrl Pts',(-61.4177693722602,-12.8855923599243,
40.0156804369713));
#191475=CARTESIAN_POINT('Ctrl Pts',(-61.4247966697211,-12.8920087864975,
40.0232638017446));
#191476=CARTESIAN_POINT('Ctrl Pts',(-61.4314390014632,-12.8991043342901,
40.0306257269992));
#191477=CARTESIAN_POINT('Ctrl Pts',(-61.4333656894068,-12.9011624829819,
40.0327611416669));
#191478=CARTESIAN_POINT('Ctrl Pts',(-61.4352597571387,-12.9032779088719,
40.0348777427279));
#191479=CARTESIAN_POINT('Ctrl Pts',(-61.4371183613309,-12.905452464584,
40.0369733168701));
#191480=CARTESIAN_POINT('Ctrl Pts',(-61.4391332077732,-12.9078098227879,
40.039245053974));
#191481=CARTESIAN_POINT('Ctrl Pts',(-61.4411043938524,-12.9102326900445,
40.041487875195));
#191482=CARTESIAN_POINT('Ctrl Pts',(-61.4430281531012,-12.9127224163025,
40.0436985701601));
#191483=CARTESIAN_POINT('Ctrl Pts',(-61.448307925455,-12.9195554895542,
40.0497658398386));
#191484=CARTESIAN_POINT('Ctrl Pts',(-61.4531896374536,-12.9269097705828,
40.0555581699984));
#191485=CARTESIAN_POINT('Ctrl Pts',(-61.4575800373534,-12.9347398820027,
40.0609828468886));
#191486=CARTESIAN_POINT('Ctrl Pts',(-61.4615970149013,-12.9419040088453,
40.0659461317306));
#191487=CARTESIAN_POINT('Ctrl Pts',(-61.4651913207948,-12.9494643722284,
40.0706039980708));
#191488=CARTESIAN_POINT('Ctrl Pts',(-61.4682744840804,-12.9574154517107,
40.0748843180606));
#191489=CARTESIAN_POINT('Ctrl Pts',(-61.4697889238147,-12.9613209959789,
40.0769867972571));
#191490=CARTESIAN_POINT('Ctrl Pts',(-61.4711795284101,-12.9653208118552,
40.0789976708176));
#191491=CARTESIAN_POINT('Ctrl Pts',(-61.4724324898305,-12.9694138336347,
40.08090504915));
#191492=CARTESIAN_POINT('Ctrl Pts',(-61.472670227056,-12.9701904446508,
40.0812669556105));
#191493=CARTESIAN_POINT('Ctrl Pts',(-61.4729027677275,-12.9709708853389,
40.0816253922033));
#191494=CARTESIAN_POINT('Ctrl Pts',(-61.4731300138563,-12.9717550556844,
40.081980198914));
#191495=CARTESIAN_POINT('Ctrl Pts',(-61.4733501585436,-12.9725147207067,
40.0823239179149));
#191496=CARTESIAN_POINT('Ctrl Pts',(-61.4735653344326,-12.9732778859004,
40.0826642303499));
#191497=CARTESIAN_POINT('Ctrl Pts',(-61.4737754532574,-12.9740444565833,
40.08300099161));
#191498=CARTESIAN_POINT('Ctrl Pts',(-61.4760652849146,-12.9823983859292,
40.0866709464311));
#191499=CARTESIAN_POINT('Ctrl Pts',(-61.477755648613,-12.9911623597372,
40.0899175831876));
#191500=CARTESIAN_POINT('Ctrl Pts',(-61.4787331403169,-13.0001833616589,
40.0925642067059));
#191501=CARTESIAN_POINT('Ctrl Pts',(-61.4791459411335,-13.0039929867886,
40.0936818922526));
#191502=CARTESIAN_POINT('Ctrl Pts',(-61.4794319383912,-13.007848166856,
40.094693009479));
#191503=CARTESIAN_POINT('Ctrl Pts',(-61.4795843394718,-13.0117365408428,
40.0955863397546));
#191504=CARTESIAN_POINT('Ctrl Pts',(-61.4798409790835,-13.0182844654761,
40.0970906856167));
#191505=CARTESIAN_POINT('Ctrl Pts',(-61.4797168922658,-13.0249248230172,
40.0982599215483));
#191506=CARTESIAN_POINT('Ctrl Pts',(-61.4791780149462,-13.0315916763173,
40.0990497370454));
#191507=CARTESIAN_POINT('Ctrl Pts',(-61.4790432956163,-13.0332583896423,
40.0992471909196));
#191508=CARTESIAN_POINT('Ctrl Pts',(-61.4788824204055,-13.0349267248713,
40.0994209989363));
#191509=CARTESIAN_POINT('Ctrl Pts',(-61.4786945538944,-13.03659559474,40.0995705982975));
#191510=CARTESIAN_POINT('Ctrl Pts',(-61.4784127541277,-13.039098899543,
40.0997949973393));
#191511=CARTESIAN_POINT('Ctrl Pts',(-61.4780702140288,-13.0416033892097,
40.0999649129781));
#191512=CARTESIAN_POINT('Ctrl Pts',(-61.4776657592304,-13.0441057251026,
40.1000786629733));
#191513=CARTESIAN_POINT('Ctrl Pts',(-61.477261304432,-13.0466080609954,
40.1001924129685));
#191514=CARTESIAN_POINT('Ctrl Pts',(-61.4767949453822,-13.0491082380625,
40.10025));
#191515=CARTESIAN_POINT('Ctrl Pts',(-61.4762657165316,-13.0516031943525,
40.10025));
#191516=CARTESIAN_POINT('Ctrl Pts',(-57.7418065394566,-12.2578193919764,
40.10025));
#191517=CARTESIAN_POINT('Ctrl Pts',(-57.7435970583545,-12.2493771807074,
40.10025));
#191518=CARTESIAN_POINT('Ctrl Pts',(-57.7460689269801,-12.2411559442247,
40.0995786334241));
#191519=CARTESIAN_POINT('Ctrl Pts',(-57.7491141258102,-12.2332613533229,
40.0983063763367));
#191520=CARTESIAN_POINT('Ctrl Pts',(-57.7510810117991,-12.2281622576318,
40.0974846287993));
#191521=CARTESIAN_POINT('Ctrl Pts',(-57.7532862127604,-12.2231990866883,
40.0964130309338));
#191522=CARTESIAN_POINT('Ctrl Pts',(-57.7556931859579,-12.2183955094115,
40.0951176960923));
#191523=CARTESIAN_POINT('Ctrl Pts',(-57.7588834910512,-12.2120286428973,
40.0934008039614));
#191524=CARTESIAN_POINT('Ctrl Pts',(-57.7624328173676,-12.2059457447514,
40.0912909372156));
#191525=CARTESIAN_POINT('Ctrl Pts',(-57.7662682043709,-12.2001996238497,
40.0888630467851));
#191526=CARTESIAN_POINT('Ctrl Pts',(-57.7681858978726,-12.1973265633989,
40.0876491015699));
#191527=CARTESIAN_POINT('Ctrl Pts',(-57.7701751462711,-12.1945375019635,
40.0863558569271));
#191528=CARTESIAN_POINT('Ctrl Pts',(-57.7722271161468,-12.191837655907,
40.0849936342771));
#191529=CARTESIAN_POINT('Ctrl Pts',(-57.7732531010847,-12.1904877328788,
40.0843125229521));
#191530=CARTESIAN_POINT('Ctrl Pts',(-57.7742947697604,-12.1891600976131,
40.0836141747074));
#191531=CARTESIAN_POINT('Ctrl Pts',(-57.7753510390205,-12.1878553011595,
40.0828999161609));
#191532=CARTESIAN_POINT('Ctrl Pts',(-57.7756151063355,-12.187529102046,
40.0827213515243));
#191533=CARTESIAN_POINT('Ctrl Pts',(-57.7758800862578,-12.1872043300161,
40.0825417925841));
#191534=CARTESIAN_POINT('Ctrl Pts',(-57.776145962005,-12.1868809929894,
40.082361260236));
#191535=CARTESIAN_POINT('Ctrl Pts',(-57.7769435892465,-12.1859109819095,
40.0818196631917));
#191536=CARTESIAN_POINT('Ctrl Pts',(-57.7777492785674,-12.1849538875687,
40.0812693052021));
#191537=CARTESIAN_POINT('Ctrl Pts',(-57.7785625799463,-12.1840099085254,
40.0807107531875));
#191538=CARTESIAN_POINT('Ctrl Pts',(-57.7842913698424,-12.1773606420347,
40.0767763849182));
#191539=CARTESIAN_POINT('Ctrl Pts',(-57.7903843352498,-12.1713100228962,
40.0724140586138));
#191540=CARTESIAN_POINT('Ctrl Pts',(-57.7967264334407,-12.1658251565856,
40.0677221223769));
#191541=CARTESIAN_POINT('Ctrl Pts',(-57.79980234421,-12.1631650023519,40.0654465383721));
#191542=CARTESIAN_POINT('Ctrl Pts',(-57.8029374300325,-12.160638004601,
40.0630928000679));
#191543=CARTESIAN_POINT('Ctrl Pts',(-57.806121336008,-12.1582411305895,
40.0606689262479));
#191544=CARTESIAN_POINT('Ctrl Pts',(-57.8109956736033,-12.1545716839427,
40.0569581447805));
#191545=CARTESIAN_POINT('Ctrl Pts',(-57.8159810988991,-12.1512083732204,
40.0530843804606));
#191546=CARTESIAN_POINT('Ctrl Pts',(-57.8210315314441,-12.1481495009383,
40.0490800251458));
#191547=CARTESIAN_POINT('Ctrl Pts',(-57.8233769784455,-12.146728944826,
40.0472203818218));
#191548=CARTESIAN_POINT('Ctrl Pts',(-57.8257362497572,-12.1453738842982,
40.0453323608818));
#191549=CARTESIAN_POINT('Ctrl Pts',(-57.8281051246149,-12.1440853170067,
40.0434201572162));
#191550=CARTESIAN_POINT('Ctrl Pts',(-57.8282866895389,-12.143986553401,
40.0432735943397));
#191551=CARTESIAN_POINT('Ctrl Pts',(-57.82846830734,-12.1438881466793,40.0431268995708));
#191552=CARTESIAN_POINT('Ctrl Pts',(-57.8286499766611,-12.1437900963018,
40.0429800745037));
#191553=CARTESIAN_POINT('Ctrl Pts',(-57.8312018829079,-12.1424127841094,
40.0409176249753));
#191554=CARTESIAN_POINT('Ctrl Pts',(-57.8337650648327,-12.1411075562951,
40.0388310783332));
#191555=CARTESIAN_POINT('Ctrl Pts',(-57.8363340693141,-12.1398727334217,
40.036725739981));
#191556=CARTESIAN_POINT('Ctrl Pts',(-57.845546062502,-12.1354448782037,
40.0291763710719));
#191557=CARTESIAN_POINT('Ctrl Pts',(-57.8549032874802,-12.131886297681,
40.0213310894597));
#191558=CARTESIAN_POINT('Ctrl Pts',(-57.8643241951532,-12.1290968783782,
40.0132837551324));
#191559=CARTESIAN_POINT('Ctrl Pts',(-57.8746768262719,-12.1260315867863,
40.0044405431328));
#191560=CARTESIAN_POINT('Ctrl Pts',(-57.8851069357366,-12.1238947812339,
39.9953528710603));
#191561=CARTESIAN_POINT('Ctrl Pts',(-57.895535282513,-12.1225979458246,
39.9861103629557));
#191562=CARTESIAN_POINT('Ctrl Pts',(-57.9067952798742,-12.1211976890437,
39.9761307737553));
#191563=CARTESIAN_POINT('Ctrl Pts',(-57.9180543443241,-12.1207764137884,
39.9659696936003));
#191564=CARTESIAN_POINT('Ctrl Pts',(-57.9292311407285,-12.1212770948337,
39.9557128217492));
#191565=CARTESIAN_POINT('Ctrl Pts',(-57.940314175294,-12.1217735756794,
39.9455419945151));
#191566=CARTESIAN_POINT('Ctrl Pts',(-57.9513177099575,-12.1231769533535,
39.9352756289336));
#191567=CARTESIAN_POINT('Ctrl Pts',(-57.9621601888121,-12.1254815933788,
39.92499));
#191568=CARTESIAN_POINT('Origin',(0.00316857416807368,-0.0149069694351821,
39.92499));
#191569=CARTESIAN_POINT('Ctrl Pts',(-61.4699285681955,-13.0814171332229,
40.10025));
#191570=CARTESIAN_POINT('Ctrl Pts',(-61.4681393149849,-13.0898176309845,
40.10025));
#191571=CARTESIAN_POINT('Ctrl Pts',(-61.465664225629,-13.097994011884,40.0995859581841));
#191572=CARTESIAN_POINT('Ctrl Pts',(-61.4626133761159,-13.1058430982607,
40.098327595962));
#191573=CARTESIAN_POINT('Ctrl Pts',(-61.4606640285136,-13.1108582907972,
40.0975235624067));
#191574=CARTESIAN_POINT('Ctrl Pts',(-61.4584804838815,-13.1157402208609,
40.096477705949));
#191575=CARTESIAN_POINT('Ctrl Pts',(-61.4560986543957,-13.1204666715201,
40.0952149915962));
#191576=CARTESIAN_POINT('Ctrl Pts',(-61.4528479350655,-13.1269173283001,
40.0934916398702));
#191577=CARTESIAN_POINT('Ctrl Pts',(-61.4492231901485,-13.1330744924001,
40.0913643921631));
#191578=CARTESIAN_POINT('Ctrl Pts',(-61.4453029499362,-13.1388835356733,
40.0889118607714));
#191579=CARTESIAN_POINT('Ctrl Pts',(-61.44334282983,-13.1417880573098,40.0876855950755));
#191580=CARTESIAN_POINT('Ctrl Pts',(-61.4413087943565,-13.1446057534057,
40.0863782327527));
#191581=CARTESIAN_POINT('Ctrl Pts',(-61.4392103574,-13.1473312571588,40.0850006373334));
#191582=CARTESIAN_POINT('Ctrl Pts',(-61.4381611389217,-13.1486940090354,
40.0843118396238));
#191583=CARTESIAN_POINT('Ctrl Pts',(-61.4370958165018,-13.1500337298699,
40.0836054919165));
#191584=CARTESIAN_POINT('Ctrl Pts',(-61.4360155570619,-13.1513498559439,
40.0828829920418));
#191585=CARTESIAN_POINT('Ctrl Pts',(-61.4357454922019,-13.1516788874624,
40.0827023670731));
#191586=CARTESIAN_POINT('Ctrl Pts',(-61.4354744937032,-13.1520064446716,
40.0825207326933));
#191587=CARTESIAN_POINT('Ctrl Pts',(-61.4352025796479,-13.1523325194964,
40.0823381109276));
#191588=CARTESIAN_POINT('Ctrl Pts',(-61.4343868374821,-13.1533107439708,
40.0817902456304));
#191589=CARTESIAN_POINT('Ctrl Pts',(-61.4335628556743,-13.1542756251694,
40.0812334935554));
#191590=CARTESIAN_POINT('Ctrl Pts',(-61.4327311191547,-13.15522696128,40.0806684524227));
#191591=CARTESIAN_POINT('Ctrl Pts',(-61.4269833037494,-13.1618012840659,
40.0767636676136));
#191592=CARTESIAN_POINT('Ctrl Pts',(-61.4208780249709,-13.1677829516035,
40.0724404510887));
#191593=CARTESIAN_POINT('Ctrl Pts',(-61.414528728905,-13.1732071947995,
40.0677949937407));
#191594=CARTESIAN_POINT('Ctrl Pts',(-61.4113731461889,-13.1759030287784,
40.0654862141904));
#191595=CARTESIAN_POINT('Ctrl Pts',(-61.4081566864224,-13.1784610805513,
40.0630972003215));
#191596=CARTESIAN_POINT('Ctrl Pts',(-61.4048902384027,-13.1808848153823,
40.0606363359906));
#191597=CARTESIAN_POINT('Ctrl Pts',(-61.3976839661818,-13.1862319364379,
40.0552073017124));
#191598=CARTESIAN_POINT('Ctrl Pts',(-61.3902425685153,-13.190934723734,
40.0494204304519));
#191599=CARTESIAN_POINT('Ctrl Pts',(-61.3827095020467,-13.1949697809166,
40.0434049749851));
#191600=CARTESIAN_POINT('Ctrl Pts',(-61.3799575778688,-13.1964438381902,
40.0412074532442));
#191601=CARTESIAN_POINT('Ctrl Pts',(-61.377194044862,-13.1978367193488,
40.0389814735788));
#191602=CARTESIAN_POINT('Ctrl Pts',(-61.3744236152739,-13.1991508816435,
40.0367321210016));
#191603=CARTESIAN_POINT('Ctrl Pts',(-61.3651180354454,-13.2035650137312,
40.0291767837141));
#191604=CARTESIAN_POINT('Ctrl Pts',(-61.3556720404056,-13.2071113921936,
40.0213235332577));
#191605=CARTESIAN_POINT('Ctrl Pts',(-61.3461671566363,-13.2098890888172,
40.013264921586));
#191606=CARTESIAN_POINT('Ctrl Pts',(-61.3357201634464,-13.2129421064463,
40.0044075527534));
#191607=CARTESIAN_POINT('Ctrl Pts',(-61.3252014297037,-13.2150668515154,
39.9953016253721));
#191608=CARTESIAN_POINT('Ctrl Pts',(-61.314690487281,-13.2163502251975,
39.986035342236));
#191609=CARTESIAN_POINT('Ctrl Pts',(-61.3033697519337,-13.2177324736414,
39.9760551582696));
#191610=CARTESIAN_POINT('Ctrl Pts',(-61.2920568939714,-13.2181390006409,
39.9658879738157));
#191611=CARTESIAN_POINT('Ctrl Pts',(-61.2808338148855,-13.2176240288385,
39.9556174643255));
#191612=CARTESIAN_POINT('Ctrl Pts',(-61.2697622852605,-13.2171160108941,
39.9454856413905));
#191613=CARTESIAN_POINT('Ctrl Pts',(-61.2587767401951,-13.2157108393288,
39.9352519465114));
#191614=CARTESIAN_POINT('Ctrl Pts',(-61.2479592423879,-13.213411509189,
39.92499));
#191615=CARTESIAN_POINT('Ctrl Pts',(-57.8829458346106,-12.4981558292584,
39.92499));
#191616=CARTESIAN_POINT('Ctrl Pts',(-57.8725934298278,-12.4959553576927,
39.9348107241713));
#191617=CARTESIAN_POINT('Ctrl Pts',(-57.8624518082055,-12.4929462656006,
39.9446038383151));
#191618=CARTESIAN_POINT('Ctrl Pts',(-57.8525735736593,-12.4891531124831,
39.9543158069358));
#191619=CARTESIAN_POINT('Ctrl Pts',(-57.8430352690791,-12.4854904894117,
39.963693567136));
#191620=CARTESIAN_POINT('Ctrl Pts',(-57.8337413853147,-12.48109631309,39.9729968320952));
#191621=CARTESIAN_POINT('Ctrl Pts',(-57.824753618525,-12.4759491415411,
39.9821731151294));
#191622=CARTESIAN_POINT('Ctrl Pts',(-57.8162573641141,-12.471083452433,
39.990847576431));
#191623=CARTESIAN_POINT('Ctrl Pts',(-57.8080338771707,-12.4655444244754,
39.9994093733803));
#191624=CARTESIAN_POINT('Ctrl Pts',(-57.8001616710214,-12.4592813303365,
40.0077966115798));
#191625=CARTESIAN_POINT('Ctrl Pts',(-57.7929115012238,-12.4535131257056,
40.0155211172553));
#191626=CARTESIAN_POINT('Ctrl Pts',(-57.7859589019118,-12.4471303774544,
40.0230979940982));
#191627=CARTESIAN_POINT('Ctrl Pts',(-57.7793958734452,-12.4400707995028,
40.030455410471));
#191628=CARTESIAN_POINT('Ctrl Pts',(-57.7774389108387,-12.4379657758633,
40.0326492435156));
#191629=CARTESIAN_POINT('Ctrl Pts',(-57.7755168276805,-12.4358004306465,
40.0348233715048));
#191630=CARTESIAN_POINT('Ctrl Pts',(-57.7736327324861,-12.4335727482758,
40.0369753512356));
#191631=CARTESIAN_POINT('Ctrl Pts',(-57.7717678881028,-12.4313678273307,
40.0391053430352));
#191632=CARTESIAN_POINT('Ctrl Pts',(-57.7699419852106,-12.4291043014745,
40.041211089324));
#191633=CARTESIAN_POINT('Ctrl Pts',(-57.7681599326868,-12.4267829461795,
40.0432881154904));
#191634=CARTESIAN_POINT('Ctrl Pts',(-57.7680360122395,-12.4266215236722,
40.043432547828));
#191635=CARTESIAN_POINT('Ctrl Pts',(-57.7679122920635,-12.4264598236893,
40.0435768364421));
#191636=CARTESIAN_POINT('Ctrl Pts',(-57.767788773317,-12.4262978456305,
40.0437209807855));
#191637=CARTESIAN_POINT('Ctrl Pts',(-57.7623732589829,-12.4191961341595,
40.0500407968421));
#191638=CARTESIAN_POINT('Ctrl Pts',(-57.7573864007556,-12.4115418213382,
40.0560490279347));
#191639=CARTESIAN_POINT('Ctrl Pts',(-57.7529408672212,-12.4033632485679,
40.0616647108618));
#191640=CARTESIAN_POINT('Ctrl Pts',(-57.7487968573385,-12.3957393973195,
40.066899503349));
#191641=CARTESIAN_POINT('Ctrl Pts',(-57.7451230952905,-12.3876591848382,
40.0717933267488));
#191642=CARTESIAN_POINT('Ctrl Pts',(-57.7420400166289,-12.379148818447,
40.0762460303079));
#191643=CARTESIAN_POINT('Ctrl Pts',(-57.7409121865682,-12.3760356163211,
40.0778748868753));
#191644=CARTESIAN_POINT('Ctrl Pts',(-57.7398637084257,-12.3728649408019,
40.079444352225));
#191645=CARTESIAN_POINT('Ctrl Pts',(-57.7389016204182,-12.3696384996594,
40.0809482021492));
#191646=CARTESIAN_POINT('Ctrl Pts',(-57.7386702703929,-12.3688626483504,
40.0813098278168));
#191647=CARTESIAN_POINT('Ctrl Pts',(-57.7384441015868,-12.3680830188493,
40.0816679525672));
#191648=CARTESIAN_POINT('Ctrl Pts',(-57.7382232068821,-12.3672997100618,
40.0820224192581));
#191649=CARTESIAN_POINT('Ctrl Pts',(-57.738009215137,-12.3665408796739,
40.0823658088648));
#191650=CARTESIAN_POINT('Ctrl Pts',(-57.7378001730066,-12.3657785963864,
40.0827057654616));
#191651=CARTESIAN_POINT('Ctrl Pts',(-57.737596164125,-12.3650129538222,
40.0830421470151));
#191652=CARTESIAN_POINT('Ctrl Pts',(-57.7353610110592,-12.3566244546993,
40.0867275956805));
#191653=CARTESIAN_POINT('Ctrl Pts',(-57.7337289586986,-12.3478270988457,
40.0899823432029));
#191654=CARTESIAN_POINT('Ctrl Pts',(-57.7328090548569,-12.3387746477743,
40.0926299529353));
#191655=CARTESIAN_POINT('Ctrl Pts',(-57.7324275433143,-12.3350203264899,
40.0937279956083));
#191656=CARTESIAN_POINT('Ctrl Pts',(-57.7321681942503,-12.3312224025081,
40.0947220371802));
#191657=CARTESIAN_POINT('Ctrl Pts',(-57.732037135777,-12.3273926324685,
40.0956014538692));
#191658=CARTESIAN_POINT('Ctrl Pts',(-57.7318136018936,-12.3208605605763,
40.097101390674));
#191659=CARTESIAN_POINT('Ctrl Pts',(-57.7319651225403,-12.3142375182611,
40.0982667904316));
#191660=CARTESIAN_POINT('Ctrl Pts',(-57.7325238621659,-12.3075887924651,
40.0990539325582));
#191661=CARTESIAN_POINT('Ctrl Pts',(-57.7328032319787,-12.3042644295671,
40.0994475036216));
#191662=CARTESIAN_POINT('Ctrl Pts',(-57.7331858342648,-12.3009338801483,
40.0997467259952));
#191663=CARTESIAN_POINT('Ctrl Pts',(-57.7336757296049,-12.2976053572251,
40.0999473488896));
#191664=CARTESIAN_POINT('Ctrl Pts',(-57.734165624945,-12.2942768343019,
40.100147971784));
#191665=CARTESIAN_POINT('Ctrl Pts',(-57.7347627876418,-12.2909503756175,
40.10025));
#191666=CARTESIAN_POINT('Ctrl Pts',(-57.7354693911205,-12.2876333308468,
40.10025));
#191667=CARTESIAN_POINT('Origin',(-57.9461901084062,-6.07506605172262,39.92499));
#191668=CARTESIAN_POINT('Ctrl Pts',(-62.3334394572619,-6.35995915837761,
39.92499));
#191669=CARTESIAN_POINT('Ctrl Pts',(-62.3439916622905,-6.3610682398175,
39.9348354642018));
#191670=CARTESIAN_POINT('Ctrl Pts',(-62.3544250468351,-6.36300663452657,
39.9446440828458));
#191671=CARTESIAN_POINT('Ctrl Pts',(-62.364684402406,-6.36575328117415,
39.9543641760332));
#191672=CARTESIAN_POINT('Ctrl Pts',(-62.3746103900114,-6.36841067816089,
39.9637684240713));
#191673=CARTESIAN_POINT('Ctrl Pts',(-62.3843747009658,-6.37182505343141,
39.9730909636396));
#191674=CARTESIAN_POINT('Ctrl Pts',(-62.3939185239085,-6.37602267870842,
39.982280897714));
#191675=CARTESIAN_POINT('Ctrl Pts',(-62.4029463927377,-6.37999337374561,
39.9909740094649));
#191676=CARTESIAN_POINT('Ctrl Pts',(-62.4117778192053,-6.38466529101478,
39.9995492765));
#191677=CARTESIAN_POINT('Ctrl Pts',(-62.4203406170101,-6.39009631815015,
40.0079462328694));
#191678=CARTESIAN_POINT('Ctrl Pts',(-62.4282275730657,-6.39509868692369,
40.0156804369688));
#191679=CARTESIAN_POINT('Ctrl Pts',(-62.4358870734649,-6.40074541103591,
40.023263801742));
#191680=CARTESIAN_POINT('Ctrl Pts',(-62.4432347045254,-6.40710777594541,
40.0306257269964));
#191681=CARTESIAN_POINT('Ctrl Pts',(-62.4453659729917,-6.40895325615409,
40.032761141665));
#191682=CARTESIAN_POINT('Ctrl Pts',(-62.4474707870407,-6.41085910953121,
40.034877742727));
#191683=CARTESIAN_POINT('Ctrl Pts',(-62.4495465125725,-6.41282747576041,
40.0369733168701));
#191684=CARTESIAN_POINT('Ctrl Pts',(-62.4517967325056,-6.41496131130705,
40.039245053974));
#191685=CARTESIAN_POINT('Ctrl Pts',(-62.4540103788122,-6.41716486079161,
40.041487875195));
#191686=CARTESIAN_POINT('Ctrl Pts',(-62.4561838467663,-6.41943986047071,
40.0436985701601));
#191687=CARTESIAN_POINT('Ctrl Pts',(-62.4621489466211,-6.42568361494159,
40.0497658398386));
#191688=CARTESIAN_POINT('Ctrl Pts',(-62.467772647785,-6.43248733059594,
40.0555581699984));
#191689=CARTESIAN_POINT('Ctrl Pts',(-62.4729574661286,-6.43981562609152,
40.0609828468886));
#191690=CARTESIAN_POINT('Ctrl Pts',(-62.477701293423,-6.44652061860789,
40.0659461317307));
#191691=CARTESIAN_POINT('Ctrl Pts',(-62.4820661824989,-6.45366385825802,
40.0706039980711));
#191692=CARTESIAN_POINT('Ctrl Pts',(-62.4859635700132,-6.46124910257504,
40.074884318061));
#191693=CARTESIAN_POINT('Ctrl Pts',(-62.4878779540285,-6.4649749498047,
40.0769867972574));
#191694=CARTESIAN_POINT('Ctrl Pts',(-62.4896790353532,-6.46880749650946,
40.0789976708177));
#191695=CARTESIAN_POINT('Ctrl Pts',(-62.4913529701965,-6.47274712615531,
40.08090504915));
#191696=CARTESIAN_POINT('Ctrl Pts',(-62.4916705830287,-6.47349463250819,
40.0812669556105));
#191697=CARTESIAN_POINT('Ctrl Pts',(-62.4919834280839,-6.47424649074148,
40.0816253922033));
#191698=CARTESIAN_POINT('Ctrl Pts',(-62.4922913974558,-6.4750026116312,
40.0819801989139));
#191699=CARTESIAN_POINT('Ctrl Pts',(-62.4925897427848,-6.47573510374311,
40.0823239179149));
#191700=CARTESIAN_POINT('Ctrl Pts',(-62.4928835124027,-6.47647159623306,
40.0826642303498));
#191701=CARTESIAN_POINT('Ctrl Pts',(-62.4931726086301,-6.47721200416365,
40.0830009916099));
#191702=CARTESIAN_POINT('Ctrl Pts',(-62.4963231197466,-6.48528081722612,
40.086670946431));
#191703=CARTESIAN_POINT('Ctrl Pts',(-62.4989203081701,-6.4938200899487,
40.0899175831875));
#191704=CARTESIAN_POINT('Ctrl Pts',(-62.5008353965401,-6.50268949817225,
40.0925642067058));
#191705=CARTESIAN_POINT('Ctrl Pts',(-62.5016441502511,-6.50643510434198,
40.0936818922525));
#191706=CARTESIAN_POINT('Ctrl Pts',(-62.502331556834,-6.51023927047592,
40.094693009479));
#191707=CARTESIAN_POINT('Ctrl Pts',(-62.502889568803,-6.51409041329249,
40.0955863397546));
#191708=CARTESIAN_POINT('Ctrl Pts',(-62.5038292470155,-6.52057564156532,
40.0970906856166));
#191709=CARTESIAN_POINT('Ctrl Pts',(-62.5043999463277,-6.52719259313743,
40.0982599215483));
#191710=CARTESIAN_POINT('Ctrl Pts',(-62.5045608969645,-6.53387925273567,
40.0990497370454));
#191711=CARTESIAN_POINT('Ctrl Pts',(-62.5046011346237,-6.53555091763522,
40.0992471909196));
#191712=CARTESIAN_POINT('Ctrl Pts',(-62.5046155292218,-6.53722692958775,
40.0994209989363));
#191713=CARTESIAN_POINT('Ctrl Pts',(-62.5046031362659,-6.53890629461041,
40.0995705982975));
#191714=CARTESIAN_POINT('Ctrl Pts',(-62.504584546832,-6.54142534214441,
40.0997949973393));
#191715=CARTESIAN_POINT('Ctrl Pts',(-62.5045056736598,-6.54395191714475,
40.0999649129781));
#191716=CARTESIAN_POINT('Ctrl Pts',(-62.5043649998326,-6.54648282201833,
40.1000786629733));
#191717=CARTESIAN_POINT('Ctrl Pts',(-62.5042243260054,-6.54901372689191,
40.1001924129685));
#191718=CARTESIAN_POINT('Ctrl Pts',(-62.5040218613861,-6.55154895552219,
40.10025));
#191719=CARTESIAN_POINT('Ctrl Pts',(-62.5037563256535,-6.55408556365905,
40.10025));
#191720=CARTESIAN_POINT('Ctrl Pts',(-58.7067819056643,-6.15500747092277,
40.10025));
#191721=CARTESIAN_POINT('Ctrl Pts',(-58.7076801645418,-6.1464243467814,
40.10025));
#191722=CARTESIAN_POINT('Ctrl Pts',(-58.7092791387968,-6.13798976646334,
40.0995786334241));
#191723=CARTESIAN_POINT('Ctrl Pts',(-58.711482446254,-6.12982011300221,
40.0983063763366));
#191724=CARTESIAN_POINT('Ctrl Pts',(-58.712905556799,-6.12454335512122,
40.0974846287992));
#191725=CARTESIAN_POINT('Ctrl Pts',(-58.714579884807,-6.11937686668002,
40.0964130309338));
#191726=CARTESIAN_POINT('Ctrl Pts',(-58.7164715618025,-6.11434800669293,
40.0951176960924));
#191727=CARTESIAN_POINT('Ctrl Pts',(-58.7189788712981,-6.10768254085093,
40.0934008039614));
#191728=CARTESIAN_POINT('Ctrl Pts',(-58.7218729180381,-6.101261959832,40.0912909372156));
#191729=CARTESIAN_POINT('Ctrl Pts',(-58.7250866612026,-6.09514640967233,
40.0888630467851));
#191730=CARTESIAN_POINT('Ctrl Pts',(-58.7266935327848,-6.0920886345925,
40.0876491015699));
#191731=CARTESIAN_POINT('Ctrl Pts',(-58.7283803475666,-6.08910691884932,
40.0863558569271));
#191732=CARTESIAN_POINT('Ctrl Pts',(-58.7301388657774,-6.08620737357425,
40.0849936342771));
#191733=CARTESIAN_POINT('Ctrl Pts',(-58.7310181248827,-6.08475760093672,
40.0843125229521));
#191734=CARTESIAN_POINT('Ctrl Pts',(-58.7319153115143,-6.08332835457004,
40.0836141747074));
#191735=CARTESIAN_POINT('Ctrl Pts',(-58.7328294060527,-6.08192029572531,
40.0828999161609));
#191736=CARTESIAN_POINT('Ctrl Pts',(-58.7330579296874,-6.08156828101413,
40.0827213515243));
#191737=CARTESIAN_POINT('Ctrl Pts',(-58.7332875101006,-6.08121759017528,
40.0825417925842));
#191738=CARTESIAN_POINT('Ctrl Pts',(-58.7335181314301,-6.08086823283941,
40.0823612602361));
#191739=CARTESIAN_POINT('Ctrl Pts',(-58.7342099954187,-6.0798201608318,
40.0818196631917));
#191740=CARTESIAN_POINT('Ctrl Pts',(-58.7349112274885,-6.07878409208739,
40.0812693052022));
#191741=CARTESIAN_POINT('Ctrl Pts',(-58.7356214008386,-6.0777602711168,
40.0807107531875));
#191742=CARTESIAN_POINT('Ctrl Pts',(-58.7406237702161,-6.07054860839944,
40.0767763849182));
#191743=CARTESIAN_POINT('Ctrl Pts',(-58.7460508958009,-6.06389424687505,
40.0724140586139));
#191744=CARTESIAN_POINT('Ctrl Pts',(-58.7517849266676,-6.05777649745821,
40.0677221223771));
#191745=CARTESIAN_POINT('Ctrl Pts',(-58.7545659254418,-6.05480939560177,
40.0654465383722));
#191746=CARTESIAN_POINT('Ctrl Pts',(-58.7574196937447,-6.05196853530565,
40.063092800068));
#191747=CARTESIAN_POINT('Ctrl Pts',(-58.7603356163931,-6.04925198282193,
40.0606689262479));
#191748=CARTESIAN_POINT('Ctrl Pts',(-58.764799690238,-6.04509313076954,
40.0569581447806));
#191749=CARTESIAN_POINT('Ctrl Pts',(-58.7694062431511,-6.04122712577039,
40.0530843804606));
#191750=CARTESIAN_POINT('Ctrl Pts',(-58.7741092696793,-6.03765709635796,
40.0490800251458));
#191751=CARTESIAN_POINT('Ctrl Pts',(-58.7762933795292,-6.03599915622994,
40.0472203818218));
#191752=CARTESIAN_POINT('Ctrl Pts',(-58.7784980841112,-6.03440490786083,
40.0453323608819));
#191753=CARTESIAN_POINT('Ctrl Pts',(-58.7807192900657,-6.03287578462717,
40.0434201572162));
#191754=CARTESIAN_POINT('Ctrl Pts',(-58.7808895367502,-6.03275858335636,
40.0432735943397));
#191755=CARTESIAN_POINT('Ctrl Pts',(-58.7810598733265,-6.0326417314874,
40.0431268995707));
#191756=CARTESIAN_POINT('Ctrl Pts',(-58.7812302983888,-6.03252522862511,
40.0429800745037));
#191757=CARTESIAN_POINT('Ctrl Pts',(-58.7836242566993,-6.03088871465466,
40.0409176249753));
#191758=CARTESIAN_POINT('Ctrl Pts',(-58.7860369637877,-6.02932271154724,
40.0388310783332));
#191759=CARTESIAN_POINT('Ctrl Pts',(-58.7884628208563,-6.02782611907218,
40.036725739981));
#191760=CARTESIAN_POINT('Ctrl Pts',(-58.7971615128803,-6.02245960461667,
40.0291763710718));
#191761=CARTESIAN_POINT('Ctrl Pts',(-58.8060955050476,-6.01794242202301,
40.0213310894595));
#191762=CARTESIAN_POINT('Ctrl Pts',(-58.8151732302896,-6.01418353044932,
40.0132837551321));
#191763=CARTESIAN_POINT('Ctrl Pts',(-58.825148738392,-6.01005288622405,
40.0044405431328));
#191764=CARTESIAN_POINT('Ctrl Pts',(-58.8352983536247,-6.00683754300209,
39.9953528710605));
#191765=CARTESIAN_POINT('Ctrl Pts',(-58.8455340166136,-6.0044577527299,
39.9861103629562));
#191766=CARTESIAN_POINT('Ctrl Pts',(-58.8565859638406,-6.00188817648184,
39.9761307737567));
#191767=CARTESIAN_POINT('Ctrl Pts',(-58.8677393147013,-6.00029231631163,
39.9659696936026));
#191768=CARTESIAN_POINT('Ctrl Pts',(-58.8789072188648,-5.99962196122124,
39.9557128217525));
#191769=CARTESIAN_POINT('Ctrl Pts',(-58.8899814357884,-5.99895722972121,
39.9455419945173));
#191770=CARTESIAN_POINT('Ctrl Pts',(-58.9010713848505,-5.9992027369765,
39.9352756289347));
#191771=CARTESIAN_POINT('Ctrl Pts',(-58.912095367953,-6.00036140429007,
39.92499));
#191772=CARTESIAN_POINT('Origin',(0.00159301378021015,-0.0151565136854118,
39.92499));
#191773=CARTESIAN_POINT('Ctrl Pts',(-62.5005702980931,-6.58439859102987,
40.10025));
#191774=CARTESIAN_POINT('Ctrl Pts',(-62.4996689377206,-6.59294009787395,
40.10025));
#191775=CARTESIAN_POINT('Ctrl Pts',(-62.4980620716938,-6.60133040498981,
40.0995859581842));
#191776=CARTESIAN_POINT('Ctrl Pts',(-62.4958483879906,-6.60945539386104,
40.0983275959622));
#191777=CARTESIAN_POINT('Ctrl Pts',(-62.4944339494873,-6.6146468749577,
40.0975235624069));
#191778=CARTESIAN_POINT('Ctrl Pts',(-62.4927726671883,-6.61973030386296,
40.0964777059491));
#191779=CARTESIAN_POINT('Ctrl Pts',(-62.4908979342376,-6.62467983150725,
40.0952149915962));
#191780=CARTESIAN_POINT('Ctrl Pts',(-62.4883392999283,-6.63143494361054,
40.0934916398702));
#191781=CARTESIAN_POINT('Ctrl Pts',(-62.4853780106448,-6.63793726713725,
40.0913643921631));
#191782=CARTESIAN_POINT('Ctrl Pts',(-62.4820864562849,-6.64412426454855,
40.0889118607714));
#191783=CARTESIAN_POINT('Ctrl Pts',(-62.480440679105,-6.6472177632542,40.0876855950755));
#191784=CARTESIAN_POINT('Ctrl Pts',(-62.4787123157334,-6.65023263831835,
40.0863782327527));
#191785=CARTESIAN_POINT('Ctrl Pts',(-62.4769102669531,-6.65316255786702,
40.0850006373335));
#191786=CARTESIAN_POINT('Ctrl Pts',(-62.4760092425629,-6.65462751764136,
40.0843118396238));
#191787=CARTESIAN_POINT('Ctrl Pts',(-62.4750897950507,-6.65607125586043,
40.0836054919165));
#191788=CARTESIAN_POINT('Ctrl Pts',(-62.474153026021,-6.65749308991723,
40.0828829920418));
#191789=CARTESIAN_POINT('Ctrl Pts',(-62.4739188337636,-6.65784854843143,
40.0827023670732));
#191790=CARTESIAN_POINT('Ctrl Pts',(-62.4736835588747,-6.65820263830465,
40.0825207326933));
#191791=CARTESIAN_POINT('Ctrl Pts',(-62.4734472184934,-6.65855534961576,
40.0823381109276));
#191792=CARTESIAN_POINT('Ctrl Pts',(-62.4727381973496,-6.6596134835491,
40.0817902456304));
#191793=CARTESIAN_POINT('Ctrl Pts',(-62.4720195869492,-6.66065920857969,
40.0812334935554));
#191794=CARTESIAN_POINT('Ctrl Pts',(-62.471291848471,-6.66169227331179,
40.0806684524228));
#191795=CARTESIAN_POINT('Ctrl Pts',(-62.4662627240578,-6.66883139158093,
40.0767636676137));
#191796=CARTESIAN_POINT('Ctrl Pts',(-62.4608161451509,-6.67541846632637,
40.0724404510889));
#191797=CARTESIAN_POINT('Ctrl Pts',(-62.4550686189989,-6.68147667711105,
40.0677949937409));
#191798=CARTESIAN_POINT('Ctrl Pts',(-62.4522121142781,-6.68448759124153,
40.0654862141906));
#191799=CARTESIAN_POINT('Ctrl Pts',(-62.4492806638354,-6.68736784133579,
40.0630972003216));
#191800=CARTESIAN_POINT('Ctrl Pts',(-62.4462854590369,-6.69011973548569,
40.0606363359906));
#191801=CARTESIAN_POINT('Ctrl Pts',(-62.4396775898761,-6.69619082501382,
40.0552073017124));
#191802=CARTESIAN_POINT('Ctrl Pts',(-62.4327685320937,-6.70164568781174,
40.0494204304519));
#191803=CARTESIAN_POINT('Ctrl Pts',(-62.4256985108779,-6.70644606039053,
40.0434049749851));
#191804=CARTESIAN_POINT('Ctrl Pts',(-62.4231157429701,-6.70819969702944,
40.0412074532442));
#191805=CARTESIAN_POINT('Ctrl Pts',(-62.4205129446133,-6.70987381569775,
40.0389814735788));
#191806=CARTESIAN_POINT('Ctrl Pts',(-62.4178950590936,-6.71147036762136,
40.0367321210017));
#191807=CARTESIAN_POINT('Ctrl Pts',(-62.4091018586482,-6.71683301659123,
40.0291767837137));
#191808=CARTESIAN_POINT('Ctrl Pts',(-62.4000783072478,-6.72134734296709,
40.0213235332568));
#191809=CARTESIAN_POINT('Ctrl Pts',(-62.3909158405852,-6.725103353972,40.0132649215846));
#191810=CARTESIAN_POINT('Ctrl Pts',(-62.3808452043575,-6.72923165499515,
40.0044075527515));
#191811=CARTESIAN_POINT('Ctrl Pts',(-62.3706061896751,-6.73244426756212,
39.9953016253697));
#191812=CARTESIAN_POINT('Ctrl Pts',(-62.360286976373,-6.73481930344785,
39.986035342233));
#191813=CARTESIAN_POINT('Ctrl Pts',(-62.3491727415035,-6.73737731885899,
39.9760551582661));
#191814=CARTESIAN_POINT('Ctrl Pts',(-62.3379643502027,-6.73896413451883,
39.9658879738115));
#191815=CARTESIAN_POINT('Ctrl Pts',(-62.3267489231065,-6.73962511499552,
39.9556174643206));
#191816=CARTESIAN_POINT('Ctrl Pts',(-62.3156849421461,-6.74027717000391,
39.9454856413873));
#191817=CARTESIAN_POINT('Ctrl Pts',(-62.3046126966235,-6.74002799825921,
39.9352519465098));
#191818=CARTESIAN_POINT('Ctrl Pts',(-62.293614112757,-6.73887200051292,
39.92499));
#191819=CARTESIAN_POINT('Ctrl Pts',(-58.8722700234481,-6.37927424642539,
39.92499));
#191820=CARTESIAN_POINT('Ctrl Pts',(-58.8617443183087,-6.37816795023608,
39.9348107241732));
#191821=CARTESIAN_POINT('Ctrl Pts',(-58.8513437177767,-6.376235430388,39.9446038383188));
#191822=CARTESIAN_POINT('Ctrl Pts',(-58.8411231047647,-6.37349561323631,
39.9543158069412));
#191823=CARTESIAN_POINT('Ctrl Pts',(-58.8312542036529,-6.37085007871673,
39.9636935671424));
#191824=CARTESIAN_POINT('Ctrl Pts',(-58.821551916257,-6.36745144953966,
39.9729968321027));
#191825=CARTESIAN_POINT('Ctrl Pts',(-58.8120753594611,-6.36327195218493,
39.9821731151378));
#191826=CARTESIAN_POINT('Ctrl Pts',(-58.8031170454153,-6.35932101824728,
39.9908475764397));
#191827=CARTESIAN_POINT('Ctrl Pts',(-58.7943596215132,-6.35467192211664,
39.9994093733894));
#191828=CARTESIAN_POINT('Ctrl Pts',(-58.785875868527,-6.34926600747317,
40.0077966115891));
#191829=CARTESIAN_POINT('Ctrl Pts',(-58.7780624743525,-6.34428725077761,
40.0155211172645));
#191830=CARTESIAN_POINT('Ctrl Pts',(-58.770480783241,-6.33866621241035,
40.0230979941072));
#191831=CARTESIAN_POINT('Ctrl Pts',(-58.7632157808967,-6.33233133084482,
40.0304554104799));
#191832=CARTESIAN_POINT('Ctrl Pts',(-58.7610495038528,-6.33044239704131,
40.0326492435214));
#191833=CARTESIAN_POINT('Ctrl Pts',(-58.7589116098623,-6.32848982621358,
40.0348233715077));
#191834=CARTESIAN_POINT('Ctrl Pts',(-58.7568049797265,-6.32647128889798,
40.0369753512356));
#191835=CARTESIAN_POINT('Ctrl Pts',(-58.7547198741578,-6.32447337605812,
40.0391053430352));
#191836=CARTESIAN_POINT('Ctrl Pts',(-58.7526673708734,-6.32241310885685,
40.041211089324));
#191837=CARTESIAN_POINT('Ctrl Pts',(-58.7506524329181,-6.32029074540079,
40.0432881154904));
#191838=CARTESIAN_POINT('Ctrl Pts',(-58.7505123180733,-6.32014316039674,
40.043432547828));
#191839=CARTESIAN_POINT('Ctrl Pts',(-58.7503723733987,-6.31999527850315,
40.0435768364421));
#191840=CARTESIAN_POINT('Ctrl Pts',(-58.7502325999832,-6.31984709900185,
40.0437209807855));
#191841=CARTESIAN_POINT('Ctrl Pts',(-58.7441044214167,-6.31335036684059,
40.0500407968421));
#191842=CARTESIAN_POINT('Ctrl Pts',(-58.738344788164,-6.30625925377284,
40.0560490279347));
#191843=CARTESIAN_POINT('Ctrl Pts',(-58.7330687140839,-6.29859016886869,
40.0616647108618));
#191844=CARTESIAN_POINT('Ctrl Pts',(-58.7281504960658,-6.2914412488599,
40.066899503349));
#191845=CARTESIAN_POINT('Ctrl Pts',(-58.7236522470771,-6.28378931332922,
40.0717933267488));
#191846=CARTESIAN_POINT('Ctrl Pts',(-58.7196964823223,-6.27564783709016,
40.076246030308));
#191847=CARTESIAN_POINT('Ctrl Pts',(-58.7182494123986,-6.27266957975434,
40.0778748868753));
#191848=CARTESIAN_POINT('Ctrl Pts',(-58.7168752520896,-6.26962586933641,
40.079444352225));
#191849=CARTESIAN_POINT('Ctrl Pts',(-58.7155811795664,-6.26651766855713,
40.0809482021492));
#191850=CARTESIAN_POINT('Ctrl Pts',(-58.7152699983557,-6.26577025010539,
40.0813098278169));
#191851=CARTESIAN_POINT('Ctrl Pts',(-58.7149635750523,-6.26501853257399,
40.0816679525672));
#191852=CARTESIAN_POINT('Ctrl Pts',(-58.7146620123681,-6.26426260461801,
40.082022419258));
#191853=CARTESIAN_POINT('Ctrl Pts',(-58.7143698735178,-6.26353029941065,
40.0823658088648));
#191854=CARTESIAN_POINT('Ctrl Pts',(-58.7140822962414,-6.26279404284336,
40.0827057654617));
#191855=CARTESIAN_POINT('Ctrl Pts',(-58.7137993735012,-6.2620539192842,
40.0830421470151));
#191856=CARTESIAN_POINT('Ctrl Pts',(-58.7106996279153,-6.25394501035234,
40.0867275956805));
#191857=CARTESIAN_POINT('Ctrl Pts',(-58.7081569420201,-6.24536644325977,
40.0899823432029));
#191858=CARTESIAN_POINT('Ctrl Pts',(-58.7062958387086,-6.23645973859744,
40.0926299529353));
#191859=CARTESIAN_POINT('Ctrl Pts',(-58.7055239836917,-6.23276586269315,
40.0937279956083));
#191860=CARTESIAN_POINT('Ctrl Pts',(-58.7048690642116,-6.22901585349541,
40.0947220371802));
#191861=CARTESIAN_POINT('Ctrl Pts',(-58.7043384037134,-6.2252207626776,
40.0956014538692));
#191862=CARTESIAN_POINT('Ctrl Pts',(-58.7034333069351,-6.21874783981196,
40.097101390674));
#191863=CARTESIAN_POINT('Ctrl Pts',(-58.7028917011005,-6.21214524099522,
40.0982667904316));
#191864=CARTESIAN_POINT('Ctrl Pts',(-58.7027523988021,-6.20547453342035,
40.0990539325583));
#191865=CARTESIAN_POINT('Ctrl Pts',(-58.7026827476529,-6.20213917963292,
40.0994475036216));
#191866=CARTESIAN_POINT('Ctrl Pts',(-58.7027151167909,-6.19878688248331,
40.0997467259952));
#191867=CARTESIAN_POINT('Ctrl Pts',(-58.7028544030469,-6.19542538554988,
40.0999473488896));
#191868=CARTESIAN_POINT('Ctrl Pts',(-58.7029936893029,-6.19206388861645,
40.100147971784));
#191869=CARTESIAN_POINT('Ctrl Pts',(-58.7032398710655,-6.18869323212177,
40.10025));
#191870=CARTESIAN_POINT('Ctrl Pts',(-58.7035958781039,-6.1853204982936,
40.10025));
#191871=CARTESIAN_POINT('Origin',(-58.2637721346185,0.01524,39.92499));
#191872=CARTESIAN_POINT('Ctrl Pts',(-62.6567671111299,0.1905,39.92499));
#191873=CARTESIAN_POINT('Ctrl Pts',(-62.6673774406538,0.1905,39.9348354642018));
#191874=CARTESIAN_POINT('Ctrl Pts',(-62.6779562874464,0.189662809673088,
39.9446440828458));
#191875=CARTESIAN_POINT('Ctrl Pts',(-62.6884465439472,0.188003604115171,
39.9543641760331));
#191876=CARTESIAN_POINT('Ctrl Pts',(-62.6985959295772,0.186398312857959,
39.9637684240713));
#191877=CARTESIAN_POINT('Ctrl Pts',(-62.7086636500146,0.184023290311342,
39.9730909636396));
#191878=CARTESIAN_POINT('Ctrl Pts',(-62.7185939622163,0.180846261210701,
39.9822808977141));
#191879=CARTESIAN_POINT('Ctrl Pts',(-62.7279874260857,0.177840987311675,
39.990974009465));
#191880=CARTESIAN_POINT('Ctrl Pts',(-62.7372588214078,0.17411779873125,
39.9995492765001));
#191881=CARTESIAN_POINT('Ctrl Pts',(-62.7463424082307,0.169611579426592,
40.0079462328694));
#191882=CARTESIAN_POINT('Ctrl Pts',(-62.7547090486364,0.165461025548926,
40.0156804369689));
#191883=CARTESIAN_POINT('Ctrl Pts',(-62.762916832885,0.160645870588327,
40.0232638017421));
#191884=CARTESIAN_POINT('Ctrl Pts',(-62.7708892610805,0.155086395962896,
40.0306257269966));
#191885=CARTESIAN_POINT('Ctrl Pts',(-62.7732017594453,0.153473803705521,
40.0327611416651));
#191886=CARTESIAN_POINT('Ctrl Pts',(-62.7754942590274,0.151798403770651,
40.0348777427271));
#191887=CARTESIAN_POINT('Ctrl Pts',(-62.7777643638145,0.150057792857645,
40.0369733168701));
#191888=CARTESIAN_POINT('Ctrl Pts',(-62.780225303358,0.148170858717027,
40.039245053974));
#191889=CARTESIAN_POINT('Ctrl Pts',(-62.7826571567198,0.146210769553757,
40.041487875195));
#191890=CARTESIAN_POINT('Ctrl Pts',(-62.7850565204094,0.144175421826141,
40.0436985701601));
#191891=CARTESIAN_POINT('Ctrl Pts',(-62.791641592883,0.138589394016616,
40.0497658398386));
#191892=CARTESIAN_POINT('Ctrl Pts',(-62.7979456687653,0.132410786669038,
40.0555581699984));
#191893=CARTESIAN_POINT('Ctrl Pts',(-62.8038680995981,0.12566459743673,
40.0609828468886));
#191894=CARTESIAN_POINT('Ctrl Pts',(-62.8092868022738,0.119492200548389,
40.0659461317304));
#191895=CARTESIAN_POINT('Ctrl Pts',(-62.8143744518938,0.112844347460359,
40.0706039980705));
#191896=CARTESIAN_POINT('Ctrl Pts',(-62.8190433630432,0.105708043833492,
40.0748843180602));
#191897=CARTESIAN_POINT('Ctrl Pts',(-62.8213367169482,0.102202714803617,
40.0769867972569));
#191898=CARTESIAN_POINT('Ctrl Pts',(-62.8235285419787,0.0985794274533612,
40.0789976708174));
#191899=CARTESIAN_POINT('Ctrl Pts',(-62.8256051102647,0.0948363533472193,
40.08090504915));
#191900=CARTESIAN_POINT('Ctrl Pts',(-62.8259991188709,0.09412614149362,
40.0812669556104));
#191901=CARTESIAN_POINT('Ctrl Pts',(-62.8263888407139,0.093411103231266,
40.0816253922033));
#191902=CARTESIAN_POINT('Ctrl Pts',(-62.826774159152,0.09269131601607,40.0819801989139));
#191903=CARTESIAN_POINT('Ctrl Pts',(-62.8271474363889,0.0919940221513489,
40.0823239179149));
#191904=CARTESIAN_POINT('Ctrl Pts',(-62.8275165811343,0.0912922715310365,
40.0826642303498));
#191905=CARTESIAN_POINT('Ctrl Pts',(-62.8278814873655,0.0905861384169469,
40.0830009916099));
#191906=CARTESIAN_POINT('Ctrl Pts',(-62.8318581602824,0.0828908452418441,
40.0866709464312));
#191907=CARTESIAN_POINT('Ctrl Pts',(-62.8353337180912,0.0746698316630267,
40.0899175831877));
#191908=CARTESIAN_POINT('Ctrl Pts',(-62.8381654210186,0.0660491922296554,
40.0925642067062));
#191909=CARTESIAN_POINT('Ctrl Pts',(-62.8393612667489,0.0624086426653834,
40.0936818922528));
#191910=CARTESIAN_POINT('Ctrl Pts',(-62.8404425512865,0.0586971697057181,
40.0946930094791));
#191911=CARTESIAN_POINT('Ctrl Pts',(-62.8414000604479,0.0549254519864736,
40.0955863397546));
#191912=CARTESIAN_POINT('Ctrl Pts',(-62.8430124819501,0.048573973592213,
40.0970906856166));
#191913=CARTESIAN_POINT('Ctrl Pts',(-62.8442717146912,0.0420529246952702,
40.0982599215483));
#191914=CARTESIAN_POINT('Ctrl Pts',(-62.8451307298764,0.0354197192407063,
40.0990497370454));
#191915=CARTESIAN_POINT('Ctrl Pts',(-62.8453454836727,0.0337614178770653,
40.0992471909196));
#191916=CARTESIAN_POINT('Ctrl Pts',(-62.8455349903695,0.032096091938589,
40.0994209989363));
#191917=CARTESIAN_POINT('Ctrl Pts',(-62.8456982067485,0.0304246312365876,
40.0995705982975));
#191918=CARTESIAN_POINT('Ctrl Pts',(-62.845943031317,0.0279174401835856,
40.0997949973393));
#191919=CARTESIAN_POINT('Ctrl Pts',(-62.8461286892223,0.0253964615339666,
40.0999649129781));
#191920=CARTESIAN_POINT('Ctrl Pts',(-62.846253337618,0.0228647168031101,
40.1000786629733));
#191921=CARTESIAN_POINT('Ctrl Pts',(-62.8463779860137,0.0203329720722537,
40.1001924129685));
#191922=CARTESIAN_POINT('Ctrl Pts',(-62.8464416340693,0.017790468374154,
40.10025));
#191923=CARTESIAN_POINT('Ctrl Pts',(-62.8464427007196,0.01524,40.10025));
#191924=CARTESIAN_POINT('Ctrl Pts',(-59.0285534841296,0.0152400000000004,
40.10025));
#191925=CARTESIAN_POINT('Ctrl Pts',(-59.0285496414744,0.0238699985096171,
40.10025));
#191926=CARTESIAN_POINT('Ctrl Pts',(-59.0292582026622,0.032425511636119,
40.099578633424));
#191927=CARTESIAN_POINT('Ctrl Pts',(-59.0305954788491,0.0407807192236517,
40.0983063763365));
#191928=CARTESIAN_POINT('Ctrl Pts',(-59.0314592220533,0.0461773260308832,
40.0974846287991));
#191929=CARTESIAN_POINT('Ctrl Pts',(-59.0325843328199,0.0514905268412107,
40.0964130309337));
#191930=CARTESIAN_POINT('Ctrl Pts',(-59.0339399880044,0.0566895722961695,
40.0951176960924));
#191931=CARTESIAN_POINT('Ctrl Pts',(-59.0357368312948,0.0635806092273947,
40.0934008039614));
#191932=CARTESIAN_POINT('Ctrl Pts',(-59.0379438906768,0.0702685278900844,
40.0912909372157));
#191933=CARTESIAN_POINT('Ctrl Pts',(-59.0405007795597,0.0766865040604244,
40.0888630467851));
#191934=CARTESIAN_POINT('Ctrl Pts',(-59.0417792240012,0.0798954921455943,
40.0876491015699));
#191935=CARTESIAN_POINT('Ctrl Pts',(-59.0431451240705,0.0830371938949132,
40.0863558569271));
#191936=CARTESIAN_POINT('Ctrl Pts',(-59.0445909239228,0.0861046703637849,
40.0849936342771));
#191937=CARTESIAN_POINT('Ctrl Pts',(-59.0453138238489,0.0876384085982208,
40.0843125229521));
#191938=CARTESIAN_POINT('Ctrl Pts',(-59.0460566986719,0.0891536069436204,
40.0836141747074));
#191939=CARTESIAN_POINT('Ctrl Pts',(-59.0468186034775,0.0906495011920575,
40.0828999161609));
#191940=CARTESIAN_POINT('Ctrl Pts',(-59.047009079679,0.0910234747541668,
40.0827213515243));
#191941=CARTESIAN_POINT('Ctrl Pts',(-59.0472007452523,0.0913962421596926,
40.0825417925842));
#191942=CARTESIAN_POINT('Ctrl Pts',(-59.0473935854286,0.091767792172695,
40.0823612602361));
#191943=CARTESIAN_POINT('Ctrl Pts',(-59.0479721059574,0.0928824422117024,
40.0818196631917));
#191944=CARTESIAN_POINT('Ctrl Pts',(-59.0485611979309,0.0939861339737884,
40.0812693052021));
#191945=CARTESIAN_POINT('Ctrl Pts',(-59.0491604624443,0.0950785796749106,
40.0807107531875));
#191946=CARTESIAN_POINT('Ctrl Pts',(-59.0533816042976,0.102773626133156,
40.0767763849182));
#191947=CARTESIAN_POINT('Ctrl Pts',(-59.0580834293366,0.109958823466292,
40.0724140586138));
#191948=CARTESIAN_POINT('Ctrl Pts',(-59.063146569637,0.116642428646605,
40.0677221223769));
#191949=CARTESIAN_POINT('Ctrl Pts',(-59.0656021872115,0.119883969936752,
40.0654465383721));
#191950=CARTESIAN_POINT('Ctrl Pts',(-59.0681433715119,0.123007567718065,
40.063092800068));
#191951=CARTESIAN_POINT('Ctrl Pts',(-59.0707593633743,0.126014035556406,
40.0606689262479));
#191952=CARTESIAN_POINT('Ctrl Pts',(-59.0747642641417,0.130616727761033,
40.0569581447806));
#191953=CARTESIAN_POINT('Ctrl Pts',(-59.0789414743143,0.134943070277265,
40.0530843804606));
#191954=CARTESIAN_POINT('Ctrl Pts',(-59.0832455674828,0.138985142830727,
40.0490800251458));
#191955=CARTESIAN_POINT('Ctrl Pts',(-59.0852444106166,0.140862302235468,
40.0472203818218));
#191956=CARTESIAN_POINT('Ctrl Pts',(-59.0872703932641,0.142678271527114,
40.0453323608819));
#191957=CARTESIAN_POINT('Ctrl Pts',(-59.0893195943183,0.144431197308737,
40.0434201572162));
#191958=CARTESIAN_POINT('Ctrl Pts',(-59.0894766575049,0.144565552163021,
40.0432735943397));
#191959=CARTESIAN_POINT('Ctrl Pts',(-59.0896338466133,0.144699568925786,
40.0431268995707));
#191960=CARTESIAN_POINT('Ctrl Pts',(-59.0897911602042,0.144833247843074,
40.0429800745037));
#191961=CARTESIAN_POINT('Ctrl Pts',(-59.0920009418701,0.14671103360208,
40.0409176249753));
#191962=CARTESIAN_POINT('Ctrl Pts',(-59.0942367399983,0.148520654544882,
40.0388310783332));
#191963=CARTESIAN_POINT('Ctrl Pts',(-59.0964928714566,0.150262619641264,
40.036725739981));
#191964=CARTESIAN_POINT('Ctrl Pts',(-59.1045829576263,0.156508996678799,
40.0291763710718));
#191965=CARTESIAN_POINT('Ctrl Pts',(-59.112995834295,0.161935290145674,
40.0213310894595));
#191966=CARTESIAN_POINT('Ctrl Pts',(-59.1216309196485,0.166622470787548,
40.0132837551321));
#191967=CARTESIAN_POINT('Ctrl Pts',(-59.1311200109809,0.171773211443978,
40.0044405431325));
#191968=CARTESIAN_POINT('Ctrl Pts',(-59.1408779306738,0.176031864362474,
39.99535287106));
#191969=CARTESIAN_POINT('Ctrl Pts',(-59.1508087658101,0.179468536017358,
39.9861103629554));
#191970=CARTESIAN_POINT('Ctrl Pts',(-59.1615315754582,0.183179278917879,
39.9761307737551));
#191971=CARTESIAN_POINT('Ctrl Pts',(-59.1724570142857,0.185932239424941,
39.9659696936002));
#191972=CARTESIAN_POINT('Ctrl Pts',(-59.1834936683151,0.187766286100067,
39.9557128217492));
#191973=CARTESIAN_POINT('Ctrl Pts',(-59.1944377361563,0.189584947007898,
39.9455419945151));
#191974=CARTESIAN_POINT('Ctrl Pts',(-59.205492595812,0.1905,39.9352756289336));
#191975=CARTESIAN_POINT('Ctrl Pts',(-59.2165773020941,0.1905,39.92499));
#191976=CARTESIAN_POINT('Origin',(1.12442271988212E-14,-0.01524,39.92499));
#191977=CARTESIAN_POINT('Ctrl Pts',(-62.8464427007196,-0.01524,40.10025));
#191978=CARTESIAN_POINT('Ctrl Pts',(-62.8464391086779,-0.0238289333904583,
40.10025));
#191979=CARTESIAN_POINT('Ctrl Pts',(-62.8457180711405,-0.0323412407624883,
40.0995859581842));
#191980=CARTESIAN_POINT('Ctrl Pts',(-62.8443658068291,-0.0406531130501973,
40.0983275959621));
#191981=CARTESIAN_POINT('Ctrl Pts',(-62.843501774309,-0.0459640037533824,
40.0975235624069));
#191982=CARTESIAN_POINT('Ctrl Pts',(-62.8423809556999,-0.0511932363889938,
40.0964777059491));
#191983=CARTESIAN_POINT('Ctrl Pts',(-62.841033859251,-0.0563116129573706,
40.0952149915961));
#191984=CARTESIAN_POINT('Ctrl Pts',(-62.8391953428955,-0.0632971699621705,
40.0934916398701));
#191985=CARTESIAN_POINT('Ctrl Pts',(-62.8369299537504,-0.070073412098335,
40.0913643921631));
#191986=CARTESIAN_POINT('Ctrl Pts',(-62.8343031482014,-0.0765705776094529,
40.0889118607713));
#191987=CARTESIAN_POINT('Ctrl Pts',(-62.8329897454269,-0.0798191603650119,
40.0876855950755));
#191988=CARTESIAN_POINT('Ctrl Pts',(-62.8315859904681,-0.08299818279531,
40.0863782327527));
#191989=CARTESIAN_POINT('Ctrl Pts',(-62.8301000734874,-0.0861004173278655,
40.0850006373334));
#191990=CARTESIAN_POINT('Ctrl Pts',(-62.8293571149971,-0.0876515345941433,
40.0843118396238));
#191991=CARTESIAN_POINT('Ctrl Pts',(-62.8285936160519,-0.0891834722997116,
40.0836054919165));
#191992=CARTESIAN_POINT('Ctrl Pts',(-62.82781060087,-0.0906954364278793,
40.0828829920418));
#191993=CARTESIAN_POINT('Ctrl Pts',(-62.8276148470746,-0.0910734274599212,
40.0827023670731));
#191994=CARTESIAN_POINT('Ctrl Pts',(-62.8274178735164,-0.0914501705143456,
40.0825207326933));
#191995=CARTESIAN_POINT('Ctrl Pts',(-62.8272196962038,-0.0918256539328543,
40.0823381109276));
#191996=CARTESIAN_POINT('Ctrl Pts',(-62.8266251642659,-0.0929521041883804,
40.0817902456304));
#191997=CARTESIAN_POINT('Ctrl Pts',(-62.826019798519,-0.0940672158686678,
40.0812334935554));
#191998=CARTESIAN_POINT('Ctrl Pts',(-62.8254040313373,-0.0951706907488606,
40.0806684524227));
#191999=CARTESIAN_POINT('Ctrl Pts',(-62.8211486980557,-0.102796386827432,
40.0767636676138));
#192000=CARTESIAN_POINT('Ctrl Pts',(-62.8164204928786,-0.109916699411237,
40.0724404510891));
#192001=CARTESIAN_POINT('Ctrl Pts',(-62.8113377077399,-0.116542502759463,
40.0677949937413));
#192002=CARTESIAN_POINT('Ctrl Pts',(-62.8088115774777,-0.119835508836266,
40.0654862141908));
#192003=CARTESIAN_POINT('Ctrl Pts',(-62.8061972539434,-0.123006400629238,
40.0630972003217));
#192004=CARTESIAN_POINT('Ctrl Pts',(-62.8035061084565,-0.126056303769975,
40.0606363359906));
#192005=CARTESIAN_POINT('Ctrl Pts',(-62.7975690395532,-0.132784845643289,
40.0552073017124));
#192006=CARTESIAN_POINT('Ctrl Pts',(-62.7912680187378,-0.138932019324687,
40.0494204304519));
#192007=CARTESIAN_POINT('Ctrl Pts',(-62.7847385034067,-0.144445113413174,
40.0434049749851));
#192008=CARTESIAN_POINT('Ctrl Pts',(-62.7823531891148,-0.146459116207472,
40.0412074532442));
#192009=CARTESIAN_POINT('Ctrl Pts',(-62.7799396422115,-0.148396130390986,
40.0389814735788));
#192010=CARTESIAN_POINT('Ctrl Pts',(-62.7775029828616,-0.150257579786495,
40.0367321210016));
#192011=CARTESIAN_POINT('Ctrl Pts',(-62.7693185019448,-0.156509991333542,
40.0291767837141));
#192012=CARTESIAN_POINT('Ctrl Pts',(-62.7608162581025,-0.161942805717962,
40.0213235332578));
#192013=CARTESIAN_POINT('Ctrl Pts',(-62.7520965944499,-0.166635979461348,
40.0132649215861));
#192014=CARTESIAN_POINT('Ctrl Pts',(-62.7425126511837,-0.17179433334833,
40.0044075527536));
#192015=CARTESIAN_POINT('Ctrl Pts',(-62.7326655363505,-0.176059615357533,
39.9953016253724));
#192016=CARTESIAN_POINT('Ctrl Pts',(-62.7226511116306,-0.179500292056757,
39.9860353422363));
#192017=CARTESIAN_POINT('Ctrl Pts',(-62.7118651471232,-0.183206048283122,
39.97605515827));
#192018=CARTESIAN_POINT('Ctrl Pts',(-62.7008840239659,-0.185955767119226,
39.9658879738161));
#192019=CARTESIAN_POINT('Ctrl Pts',(-62.689799127427,-0.187785458035178,
39.955617464326));
#192020=CARTESIAN_POINT('Ctrl Pts',(-62.6788639144179,-0.189590441946077,
39.9454856413909));
#192021=CARTESIAN_POINT('Ctrl Pts',(-62.6678262782733,-0.1905,39.9352519465115));
#192022=CARTESIAN_POINT('Ctrl Pts',(-62.6567671111299,-0.1905,39.92499));
#192023=CARTESIAN_POINT('Ctrl Pts',(-59.2165773020941,-0.1905,39.92499));
#192024=CARTESIAN_POINT('Ctrl Pts',(-59.2059936184286,-0.1905,39.9348107241729));
#192025=CARTESIAN_POINT('Ctrl Pts',(-59.1954479901449,-0.18966522548857,
39.9446038383182));
#192026=CARTESIAN_POINT('Ctrl Pts',(-59.1849969778442,-0.188008762313808,
39.9543158069403));
#192027=CARTESIAN_POINT('Ctrl Pts',(-59.1749056059476,-0.186409301376566,
39.9636935671413));
#192028=CARTESIAN_POINT('Ctrl Pts',(-59.1649012152123,-0.184043455437504,
39.9729968321014));
#192029=CARTESIAN_POINT('Ctrl Pts',(-59.1550396955505,-0.180877423725678,
39.9821731151364));
#192030=CARTESIAN_POINT('Ctrl Pts',(-59.1457174710335,-0.177884532218296,
39.9908475764383));
#192031=CARTESIAN_POINT('Ctrl Pts',(-59.1365220583417,-0.174176304385485,
39.9994093733879));
#192032=CARTESIAN_POINT('Ctrl Pts',(-59.1275197082918,-0.169686797570574,
40.0077966115876));
#192033=CARTESIAN_POINT('Ctrl Pts',(-59.1192286949217,-0.165552037111176,
40.015521117263));
#192034=CARTESIAN_POINT('Ctrl Pts',(-59.1111009786049,-0.16075429390116,
40.0230979941058));
#192035=CARTESIAN_POINT('Ctrl Pts',(-59.1032135992685,-0.155213515010445,
40.0304554104785));
#192036=CARTESIAN_POINT('Ctrl Pts',(-59.1008617419687,-0.15356136659404,
40.0326492435205));
#192037=CARTESIAN_POINT('Ctrl Pts',(-59.0985314603567,-0.151842962926721,
40.0348233715073));
#192038=CARTESIAN_POINT('Ctrl Pts',(-59.096225375957,-0.150055686180148,
40.0369753512356));
#192039=CARTESIAN_POINT('Ctrl Pts',(-59.0939428540559,-0.148286670996711,
40.0391053430352));
#192040=CARTESIAN_POINT('Ctrl Pts',(-59.0916862380348,-0.146452235168912,
40.041211089324));
#192041=CARTESIAN_POINT('Ctrl Pts',(-59.0894604907299,-0.144552116609974,
40.0432881154904));
#192042=CARTESIAN_POINT('Ctrl Pts',(-59.0893057166152,-0.144419986081426,
40.043432547828));
#192043=CARTESIAN_POINT('Ctrl Pts',(-59.089151080705,-0.144287542502105,
40.0435768364421));
#192044=CARTESIAN_POINT('Ctrl Pts',(-59.0889965840074,-0.144154785043949,
40.0437209807855));
#192045=CARTESIAN_POINT('Ctrl Pts',(-59.0822228828153,-0.138334211749519,
40.050040796842));
#192046=CARTESIAN_POINT('Ctrl Pts',(-59.0757535782845,-0.131883990154123,
40.0560490279344));
#192047=CARTESIAN_POINT('Ctrl Pts',(-59.0697047694307,-0.124808417215326,
40.0616647108615));
#192048=CARTESIAN_POINT('Ctrl Pts',(-59.0640662283031,-0.118212753510071,
40.0668995033485));
#192049=CARTESIAN_POINT('Ctrl Pts',(-59.0587927761312,-0.111072931137358,
40.0717933267482));
#192050=CARTESIAN_POINT('Ctrl Pts',(-59.0540076654697,-0.103389544768211,
40.0762460303072));
#192051=CARTESIAN_POINT('Ctrl Pts',(-59.0522572100836,-0.100578862632643,
40.0778748868748));
#192052=CARTESIAN_POINT('Ctrl Pts',(-59.0505724231957,-0.0976954648438018,
40.0794443522247));
#192053=CARTESIAN_POINT('Ctrl Pts',(-59.048960544286,-0.0947395585253491,
40.0809482021492));
#192054=CARTESIAN_POINT('Ctrl Pts',(-59.0485729412563,-0.0940287618038531,
40.0813098278168));
#192055=CARTESIAN_POINT('Ctrl Pts',(-59.0481896206935,-0.0933131922167578,
40.0816679525672));
#192056=CARTESIAN_POINT('Ctrl Pts',(-59.0478106940136,-0.0925929271971714,
40.082022419258));
#192057=CARTESIAN_POINT('Ctrl Pts',(-59.0474436087926,-0.0918951704594471,
40.0823658088648));
#192058=CARTESIAN_POINT('Ctrl Pts',(-59.047080647127,-0.0911930071934237,
40.0827057654616));
#192059=CARTESIAN_POINT('Ctrl Pts',(-59.0467219102889,-0.0904865115878252,
40.0830421470151));
#192060=CARTESIAN_POINT('Ctrl Pts',(-59.042791533644,-0.0827460357497621,
40.0867275956807));
#192061=CARTESIAN_POINT('Ctrl Pts',(-59.0393660724129,-0.0744802459940775,
40.0899823432032));
#192062=CARTESIAN_POINT('Ctrl Pts',(-59.0365841602688,-0.0658168714604773,
40.0926299529357));
#192063=CARTESIAN_POINT('Ctrl Pts',(-59.0354304183829,-0.0622239118140861,
40.0937279956085));
#192064=CARTESIAN_POINT('Ctrl Pts',(-59.0343871039216,-0.05856290328636,
40.0947220371803));
#192065=CARTESIAN_POINT('Ctrl Pts',(-59.0334626554261,-0.0548440714999749,
40.0956014538692));
#192066=CARTESIAN_POINT('Ctrl Pts',(-59.0318859121827,-0.048501216358408,
40.097101390674));
#192067=CARTESIAN_POINT('Ctrl Pts',(-59.0306571138137,-0.041991400494417,
40.0982667904316));
#192068=CARTESIAN_POINT('Ctrl Pts',(-59.0298212958158,-0.0353717968088207,
40.0990539325583));
#192069=CARTESIAN_POINT('Ctrl Pts',(-59.0294033868168,-0.0320619949660225,
40.0994475036216));
#192070=CARTESIAN_POINT('Ctrl Pts',(-59.029085168164,-0.0287246785546771,
40.0997467259952));
#192071=CARTESIAN_POINT('Ctrl Pts',(-59.0288723192866,-0.0253670368748687,
40.0999473488896));
#192072=CARTESIAN_POINT('Ctrl Pts',(-59.0286594704093,-0.0220093951950603,
40.100147971784));
#192073=CARTESIAN_POINT('Ctrl Pts',(-59.0285519740191,-0.0186314705080073,
40.10025));
#192074=CARTESIAN_POINT('Ctrl Pts',(-59.0285534841296,-0.01524,40.10025));
#192075=CARTESIAN_POINT('Origin',(-57.9430040808457,6.10537907909423,39.92499));
#192076=CARTESIAN_POINT('Ctrl Pts',(-62.2936141127569,6.73887200051376,
39.92499));
#192077=CARTESIAN_POINT('Ctrl Pts',(-62.3041663177853,6.73998108195364,
39.9348354642015));
#192078=CARTESIAN_POINT('Ctrl Pts',(-62.3147747227664,6.74025426844133,
39.9446440828452));
#192079=CARTESIAN_POINT('Ctrl Pts',(-62.3253809467515,6.73970068257644,
39.9543641760322));
#192080=CARTESIAN_POINT('Ctrl Pts',(-62.3356425316131,6.73916508495577,
39.9637684240701));
#192081=CARTESIAN_POINT('Ctrl Pts',(-62.3459033574813,6.73785543637718,
39.9730909636382));
#192082=CARTESIAN_POINT('Ctrl Pts',(-62.3561113603631,6.73573381164871,
39.9822808977125));
#192083=CARTESIAN_POINT('Ctrl Pts',(-62.3657675025168,6.73372688529769,
39.9909740094633));
#192084=CARTESIAN_POINT('Ctrl Pts',(-62.3753772873457,6.73099321743938,
39.9995492764983));
#192085=CARTESIAN_POINT('Ctrl Pts',(-62.3848821415084,6.72746117704732,
40.0079462328675));
#192086=CARTESIAN_POINT('Ctrl Pts',(-62.3936367996008,6.72420791240257,
40.0156804369668));
#192087=CARTESIAN_POINT('Ctrl Pts',(-62.4023029414968,6.72027708243923,
40.02326380174));
#192088=CARTESIAN_POINT('Ctrl Pts',(-62.4108128192354,6.71558140886554,
40.0306257269943));
#192089=CARTESIAN_POINT('Ctrl Pts',(-62.4132812112836,6.71421937245723,
40.0327611416636));
#192090=CARTESIAN_POINT('Ctrl Pts',(-62.4157362792946,6.71279278199639,
40.0348777427263));
#192091=CARTESIAN_POINT('Ctrl Pts',(-62.4181758915949,6.71129899689642,
40.03697331687));
#192092=CARTESIAN_POINT('Ctrl Pts',(-62.4208205881801,6.70967963780713,
40.039245053974));
#192093=CARTESIAN_POINT('Ctrl Pts',(-62.4234440047028,6.70798448411218,
40.041487875195));
#192094=CARTESIAN_POINT('Ctrl Pts',(-62.4260429761973,6.70621108803167,
40.0436985701601));
#192095=CARTESIAN_POINT('Ctrl Pts',(-62.4331758738575,6.70134398857313,
40.0497658398386));
#192096=CARTESIAN_POINT('Ctrl Pts',(-62.4400912556837,6.69585818364737,
40.0555581699984));
#192097=CARTESIAN_POINT('Ctrl Pts',(-62.4466864116141,6.6897680133393,40.0609828468885));
#192098=CARTESIAN_POINT('Ctrl Pts',(-62.4527206212309,6.68419583815059,
40.0659461317303));
#192099=CARTESIAN_POINT('Ctrl Pts',(-62.4584752900412,6.67811620689384,
40.0706039980705));
#192100=CARTESIAN_POINT('Ctrl Pts',(-62.4638645712584,6.67150703079258,
40.0748843180601));
#192101=CARTESIAN_POINT('Ctrl Pts',(-62.4665117685875,6.66826062508126,
40.0769867972568));
#192102=CARTESIAN_POINT('Ctrl Pts',(-62.4690703232299,6.66488629458035,
40.0789976708174));
#192103=CARTESIAN_POINT('Ctrl Pts',(-62.4715267736418,6.66138078591754,
40.08090504915));
#192104=CARTESIAN_POINT('Ctrl Pts',(-62.4719928611813,6.66071564979291,
40.0812669556104));
#192105=CARTESIAN_POINT('Ctrl Pts',(-62.472455189938,6.66004526561032,40.0816253922032));
#192106=CARTESIAN_POINT('Ctrl Pts',(-62.4729136358128,6.659369698209,40.0819801989139));
#192107=CARTESIAN_POINT('Ctrl Pts',(-62.4733577552541,6.65871524228898,
40.0823239179149));
#192108=CARTESIAN_POINT('Ctrl Pts',(-62.4737982306999,6.65805592206494,
40.0826642303498));
#192109=CARTESIAN_POINT('Ctrl Pts',(-62.4742349489459,6.65739180030952,
40.0830009916099));
#192110=CARTESIAN_POINT('Ctrl Pts',(-62.4789942144025,6.65015433826453,
40.0866709464312));
#192111=CARTESIAN_POINT('Ctrl Pts',(-62.4833100626578,6.64234165497502,
40.0899175831877));
#192112=CARTESIAN_POINT('Ctrl Pts',(-62.4870273554127,6.63406423386189,
40.0925642067062));
#192113=CARTESIAN_POINT('Ctrl Pts',(-62.4885971912263,6.63056862752554,
40.0936818922527));
#192114=CARTESIAN_POINT('Ctrl Pts',(-62.4900605069389,6.62699051141415,
40.0946930094791));
#192115=CARTESIAN_POINT('Ctrl Pts',(-62.491407022622,6.62333954252043,40.0955863397546));
#192116=CARTESIAN_POINT('Ctrl Pts',(-62.4936745213866,6.61719140213115,
40.0970906856166));
#192117=CARTESIAN_POINT('Ctrl Pts',(-62.495608491139,6.61083770188569,40.0982599215483));
#192118=CARTESIAN_POINT('Ctrl Pts',(-62.4971561593219,6.60433062536189,
40.0990497370453));
#192119=CARTESIAN_POINT('Ctrl Pts',(-62.4975430763677,6.60270385623094,
40.0992471909196));
#192120=CARTESIAN_POINT('Ctrl Pts',(-62.4979056188881,6.60106746196599,
40.0994209989363));
#192121=CARTESIAN_POINT('Ctrl Pts',(-62.4982426563693,6.59942221845788,
40.0995705982975));
#192122=CARTESIAN_POINT('Ctrl Pts',(-62.4987482125911,6.59695435319572,
40.0997949973393));
#192123=CARTESIAN_POINT('Ctrl Pts',(-62.4991963674672,6.59446659126645,
40.0999649129781));
#192124=CARTESIAN_POINT('Ctrl Pts',(-62.499584972412,6.59196174500338,40.1000786629733));
#192125=CARTESIAN_POINT('Ctrl Pts',(-62.4999735773569,6.58945689874031,
40.1001924129685));
#192126=CARTESIAN_POINT('Ctrl Pts',(-62.5003026407461,6.58693497617694,
40.10025));
#192127=CARTESIAN_POINT('Ctrl Pts',(-62.500570298093,6.58439859103072,40.10025));
#192128=CARTESIAN_POINT('Ctrl Pts',(-58.7035958781038,6.18532049829439,
40.10025));
#192129=CARTESIAN_POINT('Ctrl Pts',(-58.7026899760169,6.19390281910191,
40.10025));
#192130=CARTESIAN_POINT('Ctrl Pts',(-58.7025003609928,6.20248552904397,
40.0995786334241));
#192131=CARTESIAN_POINT('Ctrl Pts',(-58.7029569544313,6.21093474935446,
40.0983063763367));
#192132=CARTESIAN_POINT('Ctrl Pts',(-58.7032518669434,6.21639207873522,
40.0974846287993));
#192133=CARTESIAN_POINT('Ctrl Pts',(-58.7038154335198,6.22179377937549,
40.0964130309338));
#192134=CARTESIAN_POINT('Ctrl Pts',(-58.7046202140516,6.22710604846907,
40.0951176960924));
#192135=CARTESIAN_POINT('Ctrl Pts',(-58.7056869045457,6.23414715684684,
40.0934008039614));
#192136=CARTESIAN_POINT('Ctrl Pts',(-58.7071827955652,6.24102913891686,
40.0912909372157));
#192137=CARTESIAN_POINT('Ctrl Pts',(-58.7090548163569,6.24767922440788,
40.0888630467852));
#192138=CARTESIAN_POINT('Ctrl Pts',(-58.7099908267527,6.25100426715339,
40.0876491015699));
#192139=CARTESIAN_POINT('Ctrl Pts',(-58.7110208470227,6.25427153376702,
40.0863558569271));
#192140=CARTESIAN_POINT('Ctrl Pts',(-58.7121380880307,6.25747333351558,
40.0849936342771));
#192141=CARTESIAN_POINT('Ctrl Pts',(-58.7126967085346,6.25907423338986,
40.0843125229521));
#192142=CARTESIAN_POINT('Ctrl Pts',(-58.713277132457,6.26065878288383,40.0836141747074));
#192143=CARTESIAN_POINT('Ctrl Pts',(-58.7138784999414,6.26222612320555,
40.082899916161));
#192144=CARTESIAN_POINT('Ctrl Pts',(-58.7140288418126,6.26261795828598,
40.0827213515243));
#192145=CARTESIAN_POINT('Ctrl Pts',(-58.7141804926178,6.26300871814051,
40.0825417925842));
#192146=CARTESIAN_POINT('Ctrl Pts',(-58.7143334388435,6.26339839005094,
40.0823612602361));
#192147=CARTESIAN_POINT('Ctrl Pts',(-58.7147922775207,6.26456740578226,
40.0818196631917));
#192148=CARTESIAN_POINT('Ctrl Pts',(-58.7152627751829,6.2657266282841,40.0812693052022));
#192149=CARTESIAN_POINT('Ctrl Pts',(-58.7157445651923,6.26687572965204,
40.0807107531875));
#192150=CARTESIAN_POINT('Ctrl Pts',(-58.7191382318077,6.27496985131173,
40.0767763849182));
#192151=CARTESIAN_POINT('Ctrl Pts',(-58.7230632421216,6.2826071619279,40.0724140586139));
#192152=CARTESIAN_POINT('Ctrl Pts',(-58.7274000190312,6.28978339589459,
40.067722122377));
#192153=CARTESIAN_POINT('Ctrl Pts',(-58.729503351146,6.29326386161387,40.0654465383722));
#192154=CARTESIAN_POINT('Ctrl Pts',(-58.731704109697,6.29663597408956,40.063092800068));
#192155=CARTESIAN_POINT('Ctrl Pts',(-58.7339915094193,6.29989941779187,
40.0606689262479));
#192156=CARTESIAN_POINT('Ctrl Pts',(-58.7374933585782,6.30489552208976,
40.0569581447806));
#192157=CARTESIAN_POINT('Ctrl Pts',(-58.7411954596216,6.3096348018091,40.0530843804606));
#192158=CARTESIAN_POINT('Ctrl Pts',(-58.7450534628849,6.31410463171084,
40.0490800251458));
#192159=CARTESIAN_POINT('Ctrl Pts',(-58.7468451395591,6.31618044384105,
40.0472203818218));
#192160=CARTESIAN_POINT('Ctrl Pts',(-58.7486702031823,6.31819823791566,
40.0453323608819));
#192161=CARTESIAN_POINT('Ctrl Pts',(-58.7505249478605,6.32015576082356,
40.0434201572162));
#192162=CARTESIAN_POINT('Ctrl Pts',(-58.750667106732,6.32030579724142,40.0432735943397));
#192163=CARTESIAN_POINT('Ctrl Pts',(-58.7508094261758,6.32045551058229,
40.0431268995707));
#192164=CARTESIAN_POINT('Ctrl Pts',(-58.7509519047345,6.32060490094039,
40.0429800745037));
#192165=CARTESIAN_POINT('Ctrl Pts',(-58.7529532989256,6.32270338507423,
40.0409176249753));
#192166=CARTESIAN_POINT('Ctrl Pts',(-58.7549876922214,6.32473679726668,
40.0388310783332));
#192167=CARTESIAN_POINT('Ctrl Pts',(-58.7570493794209,6.32670504965026,
40.036725739981));
#192168=CARTESIAN_POINT('Ctrl Pts',(-58.7644422230594,6.33376285265585,
40.0291763710718));
#192169=CARTESIAN_POINT('Ctrl Pts',(-58.7722418109921,6.34003880538919,
40.0213310894595));
#192170=CARTESIAN_POINT('Ctrl Pts',(-58.780339648655,6.34560292136727,40.013283755132));
#192171=CARTESIAN_POINT('Ctrl Pts',(-58.7892383587467,6.35171732586219,
40.0044405431325));
#192172=CARTESIAN_POINT('Ctrl Pts',(-58.7984976730893,6.35697262978456,
39.9953528710601));
#192173=CARTESIAN_POINT('Ctrl Pts',(-58.8080148760648,6.36142852992827,
39.9861103629555));
#192174=CARTESIAN_POINT('Ctrl Pts',(-58.8182910667864,6.36623978380521,
39.9761307737555));
#192175=CARTESIAN_POINT('Ctrl Pts',(-58.8288688921852,6.37011968263765,
39.9659696936009));
#192176=CARTESIAN_POINT('Ctrl Pts',(-58.8396533761882,6.37309732669848,
39.9557128217502));
#192177=CARTESIAN_POINT('Ctrl Pts',(-58.8503473894511,6.37604999138507,
39.9455419945158));
#192178=CARTESIAN_POINT('Ctrl Pts',(-58.8612460403463,6.3781155791127,39.9352756289339));
#192179=CARTESIAN_POINT('Ctrl Pts',(-58.872270023448,6.37927424642618,39.92499));
#192180=CARTESIAN_POINT('Origin',(-0.00159301378018793,-0.015156513685413,
39.92499));
#192181=CARTESIAN_POINT('Ctrl Pts',(-62.5037563256534,6.5540855636599,40.10025));
#192182=CARTESIAN_POINT('Ctrl Pts',(-62.5046505412977,6.54554330587477,
40.10025));
#192183=CARTESIAN_POINT('Ctrl Pts',(-62.5048232320878,6.53700226086759,
40.0995859581842));
#192184=CARTESIAN_POINT('Ctrl Pts',(-62.5043472028589,6.5285945717757,40.0983275959622));
#192185=CARTESIAN_POINT('Ctrl Pts',(-62.5040430428431,6.52322245869582,
40.0975235624069));
#192186=CARTESIAN_POINT('Ctrl Pts',(-62.5034749678471,6.51790471489682,
40.0964777059491));
#192187=CARTESIAN_POINT('Ctrl Pts',(-62.5026702669707,6.51267356740905,
40.0952149915962));
#192188=CARTESIAN_POINT('Ctrl Pts',(-62.5015720117389,6.50553410072708,
40.0934916398702));
#192189=CARTESIAN_POINT('Ctrl Pts',(-62.5000273428098,6.49855818190828,
40.0913643921631));
#192190=CARTESIAN_POINT('Ctrl Pts',(-62.4980940659029,6.49182203260229,
40.0889118607714));
#192191=CARTESIAN_POINT('Ctrl Pts',(-62.4971274274494,6.48845395794929,
40.0876855950755));
#192192=CARTESIAN_POINT('Ctrl Pts',(-62.4960636607365,6.48514561818783,
40.0863782327527));
#192193=CARTESIAN_POINT('Ctrl Pts',(-62.4949101555729,6.4819050574021,40.0850006373334));
#192194=CARTESIAN_POINT('Ctrl Pts',(-62.4943334029912,6.48028477700923,
40.0843118396238));
#192195=CARTESIAN_POINT('Ctrl Pts',(-62.4937342176673,6.47868142404725,
40.0836054919165));
#192196=CARTESIAN_POINT('Ctrl Pts',(-62.4931135352113,6.4770958952431,40.0828829920418));
#192197=CARTESIAN_POINT('Ctrl Pts',(-62.4929583645973,6.47669951304206,
40.0827023670731));
#192198=CARTESIAN_POINT('Ctrl Pts',(-62.4928018504535,6.47630424448216,
40.0825207326933));
#192199=CARTESIAN_POINT('Ctrl Pts',(-62.4926440074816,6.47591010283116,
40.0823381109276));
#192200=CARTESIAN_POINT('Ctrl Pts',(-62.4921704785661,6.47472767787817,
40.0817902456304));
#192201=CARTESIAN_POINT('Ctrl Pts',(-62.4916849899864,6.4735553969451,40.0812334935553));
#192202=CARTESIAN_POINT('Ctrl Pts',(-62.4911879405752,6.47239360181852,
40.0806684524227));
#192203=CARTESIAN_POINT('Ctrl Pts',(-62.4877530207469,6.46436487665211,
40.0767636676137));
#192204=CARTESIAN_POINT('Ctrl Pts',(-62.4837949925047,6.45678933786425,
40.0724404510888));
#192205=CARTESIAN_POINT('Ctrl Pts',(-62.4794326364365,6.44966853564018,
40.0677949937409));
#192206=CARTESIAN_POINT('Ctrl Pts',(-62.4772645574451,6.44612951648112,
40.0654862141905));
#192207=CARTESIAN_POINT('Ctrl Pts',(-62.4749960038951,6.44270272394384,
40.0630972003216));
#192208=CARTESIAN_POINT('Ctrl Pts',(-62.4726384024734,6.43938822718966,
40.0606363359906));
#192209=CARTESIAN_POINT('Ctrl Pts',(-62.4674371815967,6.43207595228396,
40.0552073017124));
#192210=CARTESIAN_POINT('Ctrl Pts',(-62.461813233051,6.42530381744033,40.049420430452));
#192211=CARTESIAN_POINT('Ctrl Pts',(-62.455895762341,6.41913840445467,40.0434049749852));
#192212=CARTESIAN_POINT('Ctrl Pts',(-62.4537340356674,6.41688610134107,
40.0412074532442));
#192213=CARTESIAN_POINT('Ctrl Pts',(-62.4515361835425,6.4147074139751,40.0389814735788));
#192214=CARTESIAN_POINT('Ctrl Pts',(-62.4493074469123,6.4126014615368,40.0367321210017));
#192215=CARTESIAN_POINT('Ctrl Pts',(-62.4418213564085,6.40552779014114,
40.0291767837138));
#192216=CARTESIAN_POINT('Ctrl Pts',(-62.4339335724859,6.39923601079889,
40.0213235332569));
#192217=CARTESIAN_POINT('Ctrl Pts',(-62.4257522463019,6.39365709371027,
40.0132649215848));
#192218=CARTESIAN_POINT('Ctrl Pts',(-62.416759999684,6.38752520296373,40.0044075527519));
#192219=CARTESIAN_POINT('Ctrl Pts',(-62.4074126717495,6.38225398283438,
39.9953016253702));
#192220=CARTESIAN_POINT('Ctrl Pts',(-62.3978127557435,6.37778536209557,
39.9860353422336));
#192221=CARTESIAN_POINT('Ctrl Pts',(-62.3874732348813,6.37297246609468,
39.9760551582668));
#192222=CARTESIAN_POINT('Ctrl Pts',(-62.3768396913494,6.36908997057751,
39.9658879738124));
#192223=CARTESIAN_POINT('Ctrl Pts',(-62.3660067738128,6.36611161569927,
39.9556174643217));
#192224=CARTESIAN_POINT('Ctrl Pts',(-62.3553201372407,6.36317347866842,
39.945485641388));
#192225=CARTESIAN_POINT('Ctrl Pts',(-62.3444380411289,6.3611151561248,39.9352519465101));
#192226=CARTESIAN_POINT('Ctrl Pts',(-62.3334394572618,6.35995915837845,
39.92499));
#192227=CARTESIAN_POINT('Ctrl Pts',(-58.9120953679529,6.00036140429087,
39.92499));
#192228=CARTESIAN_POINT('Ctrl Pts',(-58.9015696628139,5.9992551081016,39.9348107241729));
#192229=CARTESIAN_POINT('Ctrl Pts',(-58.8909945468885,5.99898299131223,
39.9446038383182));
#192230=CARTESIAN_POINT('Ctrl Pts',(-58.8804276387766,5.99953795195303,
39.9543158069403));
#192231=CARTESIAN_POINT('Ctrl Pts',(-58.8702243592773,6.00007381527929,
39.9636935671413));
#192232=CARTESIAN_POINT('Ctrl Pts',(-58.8600274754009,6.00138095727726,
39.9729968321014));
#192233=CARTESIAN_POINT('Ctrl Pts',(-58.8498890377462,6.00349883564037,
39.9821731151364));
#192234=CARTESIAN_POINT('Ctrl Pts',(-58.8403050390005,6.00550089397191,
39.9908475764382));
#192235=CARTESIAN_POINT('Ctrl Pts',(-58.8307723843848,6.00822762538685,
39.9994093733878));
#192236=CARTESIAN_POINT('Ctrl Pts',(-58.8213500689023,6.01175153639715,
40.0077966115874));
#192237=CARTESIAN_POINT('Ctrl Pts',(-58.8126722744142,6.01499699931957,
40.0155211172628));
#192238=CARTESIAN_POINT('Ctrl Pts',(-58.804087581853,6.01891888229376,40.0230979941055));
#192239=CARTESIAN_POINT('Ctrl Pts',(-58.7956642413032,6.02360485257665,
40.0304554104781));
#192240=CARTESIAN_POINT('Ctrl Pts',(-58.7931525711886,6.02500211432187,
40.0326492435203));
#192241=CARTESIAN_POINT('Ctrl Pts',(-58.7906554330083,6.02646752363828,
40.0348233715071));
#192242=CARTESIAN_POINT('Ctrl Pts',(-58.7881751602883,6.02800395803745,
40.0369753512356));
#192243=CARTESIAN_POINT('Ctrl Pts',(-58.7857202298424,6.02952469386392,
40.0391053430352));
#192244=CARTESIAN_POINT('Ctrl Pts',(-58.7832842250419,6.03111319985544,
40.041211089324));
#192245=CARTESIAN_POINT('Ctrl Pts',(-58.7808720541407,6.0327702554207,40.0432881154904));
#192246=CARTESIAN_POINT('Ctrl Pts',(-58.7807043164937,6.03288548382402,
40.043432547828));
#192247=CARTESIAN_POINT('Ctrl Pts',(-58.7805366835714,6.03300103800951,
40.0435768364421));
#192248=CARTESIAN_POINT('Ctrl Pts',(-58.7803691562897,6.03311691890603,
40.0437209807855));
#192249=CARTESIAN_POINT('Ctrl Pts',(-58.7730241465597,6.03819756191476,
40.0500407968421));
#192250=CARTESIAN_POINT('Ctrl Pts',(-58.7659160498048,6.04393622206041,
40.0560490279346));
#192251=CARTESIAN_POINT('Ctrl Pts',(-58.7591607781927,6.05034076157632,
40.0616647108616));
#192252=CARTESIAN_POINT('Ctrl Pts',(-58.7528636909919,6.05631090550667,
40.0668995033488));
#192253=CARTESIAN_POINT('Ctrl Pts',(-58.746872812682,6.06286038933388,40.0717933267485));
#192254=CARTESIAN_POINT('Ctrl Pts',(-58.7413107827875,6.07000150504474,
40.0762460303077));
#192255=CARTESIAN_POINT('Ctrl Pts',(-58.739276120295,6.07261381755775,40.0778748868751));
#192256=CARTESIAN_POINT('Ctrl Pts',(-58.7372991657062,6.07530531160724,
40.0794443522249));
#192257=CARTESIAN_POINT('Ctrl Pts',(-58.735387140493,6.07807653793596,40.0809482021492));
#192258=CARTESIAN_POINT('Ctrl Pts',(-58.7349273623042,6.07874292528959,
40.0813098278168));
#192259=CARTESIAN_POINT('Ctrl Pts',(-58.7344713442223,6.07941450700224,
40.0816679525672));
#192260=CARTESIAN_POINT('Ctrl Pts',(-58.7340192051468,6.08009121771116,
40.0820224192581));
#192261=CARTESIAN_POINT('Ctrl Pts',(-58.7335811954175,6.08074678121042,
40.0823658088648));
#192262=CARTESIAN_POINT('Ctrl Pts',(-58.7331468260467,6.08140715812747,
40.0827057654617));
#192263=CARTESIAN_POINT('Ctrl Pts',(-58.7327162055066,6.08207228526581,
40.0830421470151));
#192264=CARTESIAN_POINT('Ctrl Pts',(-58.7279982598322,6.08935952173621,
40.0867275956805));
#192265=CARTESIAN_POINT('Ctrl Pts',(-58.7237275533353,6.09722197243184,
40.0899823432029));
#192266=CARTESIAN_POINT('Ctrl Pts',(-58.7200553115705,6.10554709909145,
40.0926299529353));
#192267=CARTESIAN_POINT('Ctrl Pts',(-58.7185323234527,6.10899977726302,
40.0937279956083));
#192268=CARTESIAN_POINT('Ctrl Pts',(-58.7171120447816,6.11253167434606,
40.0947220371802));
#192269=CARTESIAN_POINT('Ctrl Pts',(-58.7158039367398,6.11613350280266,
40.0956014538693));
#192270=CARTESIAN_POINT('Ctrl Pts',(-58.7135728221601,6.12227679657189,
40.097101390674));
#192271=CARTESIAN_POINT('Ctrl Pts',(-58.7116702942287,6.12862250657827,
40.0982667904316));
#192272=CARTESIAN_POINT('Ctrl Pts',(-58.7101471179288,6.13511848061139,
40.0990539325583));
#192273=CARTESIAN_POINT('Ctrl Pts',(-58.7093855297788,6.13836646762795,
40.0994475036216));
#192274=CARTESIAN_POINT('Ctrl Pts',(-58.7087202098051,6.14165223896403,
40.0997467259952));
#192275=CARTESIAN_POINT('Ctrl Pts',(-58.7081575578111,6.14496923836534,
40.0999473488896));
#192276=CARTESIAN_POINT('Ctrl Pts',(-58.7075949058172,6.14828623776664,
40.100147971784));
#192277=CARTESIAN_POINT('Ctrl Pts',(-58.7071349090267,6.15163442139633,
40.10025));
#192278=CARTESIAN_POINT('Ctrl Pts',(-58.7067819056642,6.15500747092357,
40.10025));
#192279=CARTESIAN_POINT('Origin',(-56.9874003490101,12.1286263473648,39.92499));
#192280=CARTESIAN_POINT('Ctrl Pts',(-61.2479592423877,13.2134115091898,
39.92499));
#192281=CARTESIAN_POINT('Ctrl Pts',(-61.2583377107548,13.2156175207413,
39.934835464202));
#192282=CARTESIAN_POINT('Ctrl Pts',(-61.2688594460202,13.2169980909553,
39.9446440828463));
#192283=CARTESIAN_POINT('Ctrl Pts',(-61.2794654334808,13.2175561899859,
39.9543641760338));
#192284=CARTESIAN_POINT('Ctrl Pts',(-61.2897267895035,13.2180961541212,
39.9637684240722));
#192285=CARTESIAN_POINT('Ctrl Pts',(-61.3000683010478,13.2178662282943,
39.9730909636408));
#192286=CARTESIAN_POINT('Ctrl Pts',(-61.3104421535948,13.2168232529021,
39.9822808977154));
#192287=CARTESIAN_POINT('Ctrl Pts',(-61.3202551793192,13.2158366624039,
39.9909740094666));
#192288=CARTESIAN_POINT('Ctrl Pts',(-61.3300980668421,13.2141224659043,
39.9995492765019));
#192289=CARTESIAN_POINT('Ctrl Pts',(-61.3399200511741,13.2116033021979,
40.0079462328714));
#192290=CARTESIAN_POINT('Ctrl Pts',(-61.3489668090879,13.2092829702338,
40.0156804369712));
#192291=CARTESIAN_POINT('Ctrl Pts',(-61.3579963605677,13.2062795322627,
40.0232638017446));
#192292=CARTESIAN_POINT('Ctrl Pts',(-61.3669504518488,13.2024991065222,
40.0306257269992));
#192293=CARTESIAN_POINT('Ctrl Pts',(-61.3695476933578,13.2014025487201,
40.0327611416669));
#192294=CARTESIAN_POINT('Ctrl Pts',(-61.372138431556,13.2002403977583,40.0348777427279));
#192295=CARTESIAN_POINT('Ctrl Pts',(-61.3747208224639,13.1990098046951,
40.0369733168701));
#192296=CARTESIAN_POINT('Ctrl Pts',(-61.3775203002415,13.1976757626942,
40.0392450539741));
#192297=CARTESIAN_POINT('Ctrl Pts',(-61.3803065372248,13.1962641169262,
40.0414878751951));
#192298=CARTESIAN_POINT('Ctrl Pts',(-61.3830766416485,13.1947721021914,
40.0436985701601));
#192299=CARTESIAN_POINT('Ctrl Pts',(-61.3906792149761,13.190677256044,40.0497658398386));
#192300=CARTESIAN_POINT('Ctrl Pts',(-61.3981301363757,13.1859443571668,
40.0555581699984));
#192301=CARTESIAN_POINT('Ctrl Pts',(-61.4053257594952,13.1805769309634,
40.0609828468886));
#192302=CARTESIAN_POINT('Ctrl Pts',(-61.4119093639902,13.1756660273914,
40.0659461317306));
#192303=CARTESIAN_POINT('Ctrl Pts',(-61.4182680026354,13.170221227678,40.0706039980708));
#192304=CARTESIAN_POINT('Ctrl Pts',(-61.4243186078276,13.1642115906184,
40.0748843180606));
#192305=CARTESIAN_POINT('Ctrl Pts',(-61.4272906453327,13.1612596765262,
40.0769867972571));
#192306=CARTESIAN_POINT('Ctrl Pts',(-61.4301878975267,13.158171272746,40.0789976708175));
#192307=CARTESIAN_POINT('Ctrl Pts',(-61.4329973166795,13.1549417366134,
40.08090504915));
#192308=CARTESIAN_POINT('Ctrl Pts',(-61.4335303765996,13.1543289635883,
40.0812669556104));
#192309=CARTESIAN_POINT('Ctrl Pts',(-61.4340602468994,13.1537105783548,
40.0816253922033));
#192310=CARTESIAN_POINT('Ctrl Pts',(-61.4345867973821,13.1530866324252,
40.0819801989139));
#192311=CARTESIAN_POINT('Ctrl Pts',(-61.4350968931622,13.1524821848059,
40.0823239179149));
#192312=CARTESIAN_POINT('Ctrl Pts',(-61.4356038733672,13.1518725186285,
40.0826642303498));
#192313=CARTESIAN_POINT('Ctrl Pts',(-61.4361076188514,13.1512576844887,
40.0830009916099));
#192314=CARTESIAN_POINT('Ctrl Pts',(-61.4415973333393,13.1445573487227,
40.0866709464311));
#192315=CARTESIAN_POINT('Ctrl Pts',(-61.4467061867045,13.1372385931157,
40.0899175831876));
#192316=CARTESIAN_POINT('Ctrl Pts',(-61.4512683418493,13.1293950794809,
40.092564206706));
#192317=CARTESIAN_POINT('Ctrl Pts',(-61.4531949682968,13.1260827149668,
40.0936818922526));
#192318=CARTESIAN_POINT('Ctrl Pts',(-61.4550242827915,13.1226771582924,
40.094693009479));
#192319=CARTESIAN_POINT('Ctrl Pts',(-61.4567450522888,13.1191869390032,
40.0955863397546));
#192320=CARTESIAN_POINT('Ctrl Pts',(-61.4596427851247,13.1133094969316,
40.0970906856166));
#192321=CARTESIAN_POINT('Ctrl Pts',(-61.4622303029112,13.1071927578071,
40.0982599215483));
#192322=CARTESIAN_POINT('Ctrl Pts',(-61.4644496675148,13.100883103106,40.0990497370454));
#192323=CARTESIAN_POINT('Ctrl Pts',(-61.4650045086657,13.0993056894308,
40.0992471909196));
#192324=CARTESIAN_POINT('Ctrl Pts',(-61.4655361149182,13.0977161555174,
40.0994209989363));
#192325=CARTESIAN_POINT('Ctrl Pts',(-61.4660432808484,13.0961151548353,
40.0995705982975));
#192326=CARTESIAN_POINT('Ctrl Pts',(-61.4668040297438,13.0937136538123,
40.0997949973393));
#192327=CARTESIAN_POINT('Ctrl Pts',(-61.467509771512,13.0912863650436,40.0999649129781));
#192328=CARTESIAN_POINT('Ctrl Pts',(-61.468158075369,13.0888358608682,40.1000786629733));
#192329=CARTESIAN_POINT('Ctrl Pts',(-61.468806379226,13.0863853566928,40.1001924129685));
#192330=CARTESIAN_POINT('Ctrl Pts',(-61.4693972526618,13.0839116459755,
40.10025));
#192331=CARTESIAN_POINT('Ctrl Pts',(-61.4699285681953,13.0814171332237,
40.10025));
#192332=CARTESIAN_POINT('Ctrl Pts',(-57.7354693911204,12.2876333308475,
40.10025));
#192333=CARTESIAN_POINT('Ctrl Pts',(-57.7336713548545,12.2960739442511,
40.10025));
#192334=CARTESIAN_POINT('Ctrl Pts',(-57.7325856410804,12.3045898170434,
40.099578633424));
#192335=CARTESIAN_POINT('Ctrl Pts',(-57.7321565492374,12.3130404786519,
40.0983063763365));
#192336=CARTESIAN_POINT('Ctrl Pts',(-57.7318793999343,12.3184987389625,
40.0974846287992));
#192337=CARTESIAN_POINT('Ctrl Pts',(-57.7318752477671,12.3239297572693,
40.0964130309338));
#192338=CARTESIAN_POINT('Ctrl Pts',(-57.7321203363021,12.3292970476687,
40.0951176960924));
#192339=CARTESIAN_POINT('Ctrl Pts',(-57.7324451871156,12.3364110836362,
40.0934008039614));
#192340=CARTESIAN_POINT('Ctrl Pts',(-57.7332135204775,12.3434117286779,
40.0912909372157));
#192341=CARTESIAN_POINT('Ctrl Pts',(-57.7343801629265,12.3502210637613,
40.0888630467852));
#192342=CARTESIAN_POINT('Ctrl Pts',(-57.734963484151,12.3536257313031,40.0876491015699));
#192343=CARTESIAN_POINT('Ctrl Pts',(-57.735646339504,12.3569827659243,40.0863558569272));
#192344=CARTESIAN_POINT('Ctrl Pts',(-57.7364227809414,12.3602838093645,
40.0849936342771));
#192345=CARTESIAN_POINT('Ctrl Pts',(-57.7368110016601,12.3619343310846,
40.0843125229521));
#192346=CARTESIAN_POINT('Ctrl Pts',(-57.7372226154359,12.3635708710713,
40.0836141747074));
#192347=CARTESIAN_POINT('Ctrl Pts',(-57.7376568568911,12.3651924853577,
40.082899916161));
#192348=CARTESIAN_POINT('Ctrl Pts',(-57.7377654172549,12.3655978889293,
40.0827213515244));
#192349=CARTESIAN_POINT('Ctrl Pts',(-57.737875391774,12.3660023599861,40.0825417925842));
#192350=CARTESIAN_POINT('Ctrl Pts',(-57.7379867683383,12.366405884467,40.0823612602361));
#192351=CARTESIAN_POINT('Ctrl Pts',(-57.7383208980313,12.3676164579096,
40.0818196631918));
#192352=CARTESIAN_POINT('Ctrl Pts',(-57.7386676465114,12.3688185104669,
40.0812693052022));
#192353=CARTESIAN_POINT('Ctrl Pts',(-57.7390266834246,12.3700116777066,
40.0807107531875));
#192354=CARTESIAN_POINT('Ctrl Pts',(-57.7415556930807,12.3784161936775,
40.0767763849181));
#192355=CARTESIAN_POINT('Ctrl Pts',(-57.7446608854354,12.3864219416038,
40.0724140586135));
#192356=CARTESIAN_POINT('Ctrl Pts',(-57.7482237843189,12.3940121800362,
40.0677221223764));
#192357=CARTESIAN_POINT('Ctrl Pts',(-57.7499517864271,12.3976934374734,
40.0654465383717));
#192358=CARTESIAN_POINT('Ctrl Pts',(-57.7517880072572,12.4012771190731,
40.0630928000678));
#192359=CARTESIAN_POINT('Ctrl Pts',(-57.7537217536092,12.4047617836669,
40.0606689262479));
#192360=CARTESIAN_POINT('Ctrl Pts',(-57.7566821841673,12.4100965616938,
40.0569581447806));
#192361=CARTESIAN_POINT('Ctrl Pts',(-57.7598686150879,12.4151968540759,
40.0530843804606));
#192362=CARTESIAN_POINT('Ctrl Pts',(-57.763238259355,12.4200454689342,40.0490800251458));
#192363=CARTESIAN_POINT('Ctrl Pts',(-57.7648031395849,12.4222971907578,
40.0472203818218));
#192364=CARTESIAN_POINT('Ctrl Pts',(-57.7664072884047,12.4244947022412,
40.0453323608819));
#192365=CARTESIAN_POINT('Ctrl Pts',(-57.7680472557361,12.4266353752448,
40.0434201572162));
#192366=CARTESIAN_POINT('Ctrl Pts',(-57.7681729527703,12.4267994493958,
40.0432735943397));
#192367=CARTESIAN_POINT('Ctrl Pts',(-57.7682988432679,12.4269632190241,
40.0431268995708));
#192368=CARTESIAN_POINT('Ctrl Pts',(-57.7684249257696,12.427126684071,40.0429800745037));
#192369=CARTESIAN_POINT('Ctrl Pts',(-57.7701960047921,12.4294228751483,
40.0409176249753));
#192370=CARTESIAN_POINT('Ctrl Pts',(-57.772006704017,12.4316578001009,40.0388310783332));
#192371=CARTESIAN_POINT('Ctrl Pts',(-57.7738513586813,12.4338307751867,
40.036725739981));
#192372=CARTESIAN_POINT('Ctrl Pts',(-57.780465962247,12.4416226773942,40.0291763710713));
#192373=CARTESIAN_POINT('Ctrl Pts',(-57.7875668075266,12.4486795287429,
40.0213310894585));
#192374=CARTESIAN_POINT('Ctrl Pts',(-57.7950386758954,12.4550596184385,
40.0132837551305));
#192375=CARTESIAN_POINT('Ctrl Pts',(-57.803249508617,12.4620706960771,40.0044405431304));
#192376=CARTESIAN_POINT('Ctrl Pts',(-57.8119087706244,12.4682650727941,
39.9953528710574));
#192377=CARTESIAN_POINT('Ctrl Pts',(-57.8209080689723,12.4736913816524,
39.9861103629522));
#192378=CARTESIAN_POINT('Ctrl Pts',(-57.8306250526725,12.4795504334018,
39.9761307737515));
#192379=CARTESIAN_POINT('Ctrl Pts',(-57.8407393717752,12.4845147615762,
39.9659696935962));
#192380=CARTESIAN_POINT('Ctrl Pts',(-57.8511535286894,12.4886033793312,
39.9557128217448));
#192381=CARTESIAN_POINT('Ctrl Pts',(-57.8614803215248,12.4926576977832,
39.9455419945121));
#192382=CARTESIAN_POINT('Ctrl Pts',(-57.8721033557573,12.4958511892341,
39.9352756289321));
#192383=CARTESIAN_POINT('Ctrl Pts',(-57.8829458346104,12.4981558292591,
39.92499));
#192384=CARTESIAN_POINT('Origin',(-0.00316857416805164,-0.0149069694351843,
39.92499));
#192385=CARTESIAN_POINT('Ctrl Pts',(-61.4762657165315,13.0516031943533,
40.10025));
#192386=CARTESIAN_POINT('Ctrl Pts',(-61.4780479426481,13.0432012029369,
40.10025));
#192387=CARTESIAN_POINT('Ctrl Pts',(-61.4791124697293,13.0347249977705,
40.0995859581842));
#192388=CARTESIAN_POINT('Ctrl Pts',(-61.4795178910587,13.026313608275,40.0983275959621));
#192389=CARTESIAN_POINT('Ctrl Pts',(-61.479776935988,13.020939130814,40.0975235624068));
#192390=CARTESIAN_POINT('Ctrl Pts',(-61.4797678285536,13.0155911381659,
40.096477705949));
#192391=CARTESIAN_POINT('Ctrl Pts',(-61.4795143397207,13.0103045333057,
40.0952149915961));
#192392=CARTESIAN_POINT('Ctrl Pts',(-61.4791683783269,13.0030893784376,
40.0934916398701));
#192393=CARTESIAN_POINT('Ctrl Pts',(-61.4783613533298,12.9959902125626,
40.0913643921631));
#192394=CARTESIAN_POINT('Ctrl Pts',(-61.4771427864514,12.9890888821232,
40.0889118607713));
#192395=CARTESIAN_POINT('Ctrl Pts',(-61.4765335030122,12.9856382169035,
40.0876855950755));
#192396=CARTESIAN_POINT('Ctrl Pts',(-61.4758213793958,12.9822368066736,
40.0863782327527));
#192397=CARTESIAN_POINT('Ctrl Pts',(-61.4750129240933,12.9788934238968,
40.0850006373334));
#192398=CARTESIAN_POINT('Ctrl Pts',(-61.474608696442,12.9772217325084,40.0843118396238));
#192399=CARTESIAN_POINT('Ctrl Pts',(-61.4741803895392,12.9755645309606,
40.0836054919165));
#192400=CARTESIAN_POINT('Ctrl Pts',(-61.4737288401361,12.9739228088659,
40.0828829920418));
#192401=CARTESIAN_POINT('Ctrl Pts',(-61.4736159527853,12.9735123783422,
40.0827023670731));
#192402=CARTESIAN_POINT('Ctrl Pts',(-61.4735016128574,12.9731029149219,
40.0825207326933));
#192403=CARTESIAN_POINT('Ctrl Pts',(-61.473385833587,12.9726944333368,40.0823381109276));
#192404=CARTESIAN_POINT('Ctrl Pts',(-61.4730384957757,12.9714689885816,
40.0817902456304));
#192405=CARTESIAN_POINT('Ctrl Pts',(-61.4726782034776,12.9702523821509,
40.0812334935553));
#192406=CARTESIAN_POINT('Ctrl Pts',(-61.4723053176143,12.9690449956485,
40.0806684524227));
#192407=CARTESIAN_POINT('Ctrl Pts',(-61.46972844494,12.9607012057877,40.0767636676138));
#192408=CARTESIAN_POINT('Ctrl Pts',(-61.4665839586186,12.9527534399845,
40.072440451089));
#192409=CARTESIAN_POINT('Ctrl Pts',(-61.4629898265073,12.9452156558842,
40.0677949937413));
#192410=CARTESIAN_POINT('Ctrl Pts',(-61.4612035527136,12.941469397877,40.0654862141908));
#192411=CARTESIAN_POINT('Ctrl Pts',(-61.4593056238949,12.9378242492511,
40.0630972003217));
#192412=CARTESIAN_POINT('Ctrl Pts',(-61.4573073969126,12.9342814732032,
40.0606363359906));
#192413=CARTESIAN_POINT('Ctrl Pts',(-61.452899009727,12.9264655800791,40.0552073017124));
#192414=CARTESIAN_POINT('Ctrl Pts',(-61.4480137506081,12.9191426809998,
40.049420430452));
#192415=CARTESIAN_POINT('Ctrl Pts',(-61.4427731575667,12.9123924986718,
40.0434049749852));
#192416=CARTESIAN_POINT('Ctrl Pts',(-61.4408587028413,12.9099265719431,
40.0412074532442));
#192417=CARTESIAN_POINT('Ctrl Pts',(-61.4389006256225,12.9075300815494,
40.0389814735788));
#192418=CARTESIAN_POINT('Ctrl Pts',(-61.4369042302168,12.9052026993239,
40.0367321210017));
#192419=CARTESIAN_POINT('Ctrl Pts',(-61.4301985493006,12.8973852687039,
40.0291767837136));
#192420=CARTESIAN_POINT('Ctrl Pts',(-61.4230116455093,12.890303458455,40.0213235332567));
#192421=CARTESIAN_POINT('Ctrl Pts',(-61.415458293116,12.8838999218043,40.0132649215844));
#192422=CARTESIAN_POINT('Ctrl Pts',(-61.4071562640824,12.8768616764765,
40.0044075527513));
#192423=CARTESIAN_POINT('Ctrl Pts',(-61.3984111343277,12.8706422708178,
39.9953016253694));
#192424=CARTESIAN_POINT('Ctrl Pts',(-61.3893309057246,12.8651946651833,
39.9860353422326));
#192425=CARTESIAN_POINT('Ctrl Pts',(-61.3795511104622,12.8593273605036,
39.9760551582656));
#192426=CARTESIAN_POINT('Ctrl Pts',(-61.3693816498842,12.8543546257386,
39.965887973811));
#192427=CARTESIAN_POINT('Ctrl Pts',(-61.3589193990615,12.8502602383772,
39.95561746432));
#192428=CARTESIAN_POINT('Ctrl Pts',(-61.348598423952,12.8462211390704,39.9454856413869));
#192429=CARTESIAN_POINT('Ctrl Pts',(-61.3379910943943,12.8430366034496,
39.9352519465096));
#192430=CARTESIAN_POINT('Ctrl Pts',(-61.3271735965892,12.8407372733102,
39.92499));
#192431=CARTESIAN_POINT('Ctrl Pts',(-57.962160188812,12.1254815933796,39.92499));
#192432=CARTESIAN_POINT('Ctrl Pts',(-57.9518077840282,12.1232811218137,
39.9348107241723));
#192433=CARTESIAN_POINT('Ctrl Pts',(-57.9413190436447,12.1219050950921,
39.9446038383171));
#192434=CARTESIAN_POINT('Ctrl Pts',(-57.9307520129787,12.1213524729339,
39.9543158069387));
#192435=CARTESIAN_POINT('Ctrl Pts',(-57.9205486151424,12.1208188676184,
39.9636935671395));
#192436=CARTESIAN_POINT('Ctrl Pts',(-57.9102709573187,12.1210529843539,
39.9729968320992));
#192437=CARTESIAN_POINT('Ctrl Pts',(-57.8999666805159,12.1220995054496,
39.9821731151339));
#192438=CARTESIAN_POINT('Ctrl Pts',(-57.8902259118375,12.1230887956351,
39.9908475764357));
#192439=CARTESIAN_POINT('Ctrl Pts',(-57.8804604570568,12.1248041559921,
39.9994093733852));
#192440=CARTESIAN_POINT('Ctrl Pts',(-57.870721409002,12.1273238624911,40.0077966115848));
#192441=CARTESIAN_POINT('Ctrl Pts',(-57.8617519091282,12.1296444699055,
40.0155211172602));
#192442=CARTESIAN_POINT('Ctrl Pts',(-57.8528042960106,12.1326475236732,
40.0230979941029));
#192443=CARTESIAN_POINT('Ctrl Pts',(-57.8439372821291,12.1364273448771,
40.0304554104756));
#192444=CARTESIAN_POINT('Ctrl Pts',(-57.8412933175822,12.1375544112594,
40.0326492435186));
#192445=CARTESIAN_POINT('Ctrl Pts',(-57.8386566820011,12.1387507708941,
40.0348233715063));
#192446=CARTESIAN_POINT('Ctrl Pts',(-57.836029395347,12.1400195294494,40.0369753512356));
#192447=CARTESIAN_POINT('Ctrl Pts',(-57.833428953088,12.141275324419,40.0391053430352));
#192448=CARTESIAN_POINT('Ctrl Pts',(-57.8308402488865,12.1426004965702,
40.041211089324));
#192449=CARTESIAN_POINT('Ctrl Pts',(-57.828268082638,12.1439963340942,40.0432881154904));
#192450=CARTESIAN_POINT('Ctrl Pts',(-57.8280892192275,12.1440933979058,
40.043432547828));
#192451=CARTESIAN_POINT('Ctrl Pts',(-57.8279104259145,12.1441907966616,
40.0435768364421));
#192452=CARTESIAN_POINT('Ctrl Pts',(-57.8277317035127,12.1442885313812,
40.0437209807855));
#192453=CARTESIAN_POINT('Ctrl Pts',(-57.8198958587085,12.1485735795161,
40.050040796842));
#192454=CARTESIAN_POINT('Ctrl Pts',(-57.8122268475251,12.1535378042504,
40.0560490279344));
#192455=CARTESIAN_POINT('Ctrl Pts',(-57.8048391253243,12.1592011408681,
40.0616647108615));
#192456=CARTESIAN_POINT('Ctrl Pts',(-57.7979524842556,12.1644803548771,
40.0668995033486));
#192457=CARTESIAN_POINT('Ctrl Pts',(-57.7913098171243,12.1703677426432,
40.0717933267483));
#192458=CARTESIAN_POINT('Ctrl Pts',(-57.7850318067603,12.1768883481374,
40.0762460303074));
#192459=CARTESIAN_POINT('Ctrl Pts',(-57.7827352293492,12.1792736699856,
40.0778748868749));
#192460=CARTESIAN_POINT('Ctrl Pts',(-57.7804877669874,12.1817437717241,
40.0794443522248));
#192461=CARTESIAN_POINT('Ctrl Pts',(-57.7782965440187,12.1842999559279,
40.0809482021492));
#192462=CARTESIAN_POINT('Ctrl Pts',(-57.777769628097,12.1849146328344,40.0813098278168));
#192463=CARTESIAN_POINT('Ctrl Pts',(-57.7772459087254,12.1855348686828,
40.0816679525672));
#192464=CARTESIAN_POINT('Ctrl Pts',(-57.7767255109846,12.1861606108969,
40.082022419258));
#192465=CARTESIAN_POINT('Ctrl Pts',(-57.7762213756733,12.1867667986668,
40.0823658088648));
#192466=CARTESIAN_POINT('Ctrl Pts',(-57.7757203576391,12.1873781540072,
40.0827057654616));
#192467=CARTESIAN_POINT('Ctrl Pts',(-57.7752225713656,12.1879946254062,
40.0830421470151));
#192468=CARTESIAN_POINT('Ctrl Pts',(-57.7697687474614,12.1947487820219,
40.0867275956806));
#192469=CARTESIAN_POINT('Ctrl Pts',(-57.7646995864527,12.202121751003,40.0899823432031));
#192470=CARTESIAN_POINT('Ctrl Pts',(-57.7601772489162,12.2100174179596,
40.0926299529356));
#192471=CARTESIAN_POINT('Ctrl Pts',(-57.7583017007433,12.2132919863911,
40.0937279956084));
#192472=CARTESIAN_POINT('Ctrl Pts',(-57.7565200187331,12.2166560758252,
40.0947220371802));
#192473=CARTESIAN_POINT('Ctrl Pts',(-57.7548425830506,12.220101438565,40.0956014538692));
#192474=CARTESIAN_POINT('Ctrl Pts',(-57.751981541693,12.2259778637498,40.097101390674));
#192475=CARTESIAN_POINT('Ctrl Pts',(-57.7494261286933,12.2320899429718,
40.0982667904316));
#192476=CARTESIAN_POINT('Ctrl Pts',(-57.7472322823293,12.2383911161015,
40.0990539325583));
#192477=CARTESIAN_POINT('Ctrl Pts',(-57.7461353591473,12.2415417026664,
40.0994475036216));
#192478=CARTESIAN_POINT('Ctrl Pts',(-57.7451302272376,12.2447399293288,
40.0997467259952));
#192479=CARTESIAN_POINT('Ctrl Pts',(-57.7442239366601,12.2479799447121,
40.0999473488896));
#192480=CARTESIAN_POINT('Ctrl Pts',(-57.7433176460826,12.2512199600953,
40.100147971784));
#192481=CARTESIAN_POINT('Ctrl Pts',(-57.7425101887131,12.2545017192672,
40.10025));
#192482=CARTESIAN_POINT('Ctrl Pts',(-57.7418065394565,12.2578193919772,
40.10025));
#192483=CARTESIAN_POINT('Origin',(-55.4074307335705,18.0189898472954,39.92499));
#192484=CARTESIAN_POINT('Ctrl Pts',(-59.5312589135994,19.5431821162871,
39.92499));
#192485=CARTESIAN_POINT('Ctrl Pts',(-59.5413499366325,19.5464608884257,
39.9348354642013));
#192486=CARTESIAN_POINT('Ctrl Pts',(-59.5516697238474,19.5489337165496,
39.9446440828448));
#192487=CARTESIAN_POINT('Ctrl Pts',(-59.5621592733641,19.550597385826,39.9543641760316));
#192488=CARTESIAN_POINT('Ctrl Pts',(-59.5723079749828,19.5522069957574,
39.9637684240692));
#192489=CARTESIAN_POINT('Ctrl Pts',(-59.5826168684374,19.5530593117979,
39.9730909636371));
#192490=CARTESIAN_POINT('Ctrl Pts',(-59.5930429125488,19.5531064127993,
39.982280897711));
#192491=CARTESIAN_POINT('Ctrl Pts',(-59.6029053082795,19.5531509674463,
39.9909740094615));
#192492=CARTESIAN_POINT('Ctrl Pts',(-59.6128734577597,19.5524750234018,
39.9995492764962));
#192493=CARTESIAN_POINT('Ctrl Pts',(-59.622904960544,19.5509963368668,40.0079462328651));
#192494=CARTESIAN_POINT('Ctrl Pts',(-59.6321447001049,19.5496343596267,
40.0156804369641));
#192495=CARTESIAN_POINT('Ctrl Pts',(-59.6414387315116,19.5475912199439,
40.0232638017369));
#192496=CARTESIAN_POINT('Ctrl Pts',(-59.650738933436,19.5447674611737,40.0306257269909));
#192497=CARTESIAN_POINT('Ctrl Pts',(-59.6534365684897,19.5439483960927,
40.0327611416613));
#192498=CARTESIAN_POINT('Ctrl Pts',(-59.6561345922104,19.543063417397,40.0348777427252));
#192499=CARTESIAN_POINT('Ctrl Pts',(-59.658831468516,19.5421094990033,40.03697331687));
#192500=CARTESIAN_POINT('Ctrl Pts',(-59.6617550558217,19.5410753901341,
40.039245053974));
#192501=CARTESIAN_POINT('Ctrl Pts',(-59.6646735866701,19.5399627185794,
40.041487875195));
#192502=CARTESIAN_POINT('Ctrl Pts',(-59.6675844741793,19.5387684320159,
40.0436985701601));
#192503=CARTESIAN_POINT('Ctrl Pts',(-59.6755734277898,19.535490703171,40.0497658398386));
#192504=CARTESIAN_POINT('Ctrl Pts',(-59.6834782549088,19.5315625649729,
40.0555581699984));
#192505=CARTESIAN_POINT('Ctrl Pts',(-59.6911955084647,19.5269766895187,
40.0609828468885));
#192506=CARTESIAN_POINT('Ctrl Pts',(-59.698256376489,19.522780862451,40.0659461317305));
#192507=CARTESIAN_POINT('Ctrl Pts',(-59.7051493183932,19.5180305486462,
40.0706039980708));
#192508=CARTESIAN_POINT('Ctrl Pts',(-59.7117949558637,19.5126862934698,
40.0748843180605));
#192509=CARTESIAN_POINT('Ctrl Pts',(-59.7150592712802,19.5100612127851,
40.0769867972571));
#192510=CARTESIAN_POINT('Ctrl Pts',(-59.7182634781246,19.5072925729234,
40.0789976708175));
#192511=CARTESIAN_POINT('Ctrl Pts',(-59.7213950854344,19.5043743927943,
40.08090504915));
#192512=CARTESIAN_POINT('Ctrl Pts',(-59.7219892774191,19.5038206965383,
40.0812669556104));
#192513=CARTESIAN_POINT('Ctrl Pts',(-59.7225808838921,19.503261085412,40.0816253922032));
#192514=CARTESIAN_POINT('Ctrl Pts',(-59.7231697699854,19.5026955970363,
40.0819801989139));
#192515=CARTESIAN_POINT('Ctrl Pts',(-59.7237402533882,19.5021477801723,
40.0823239179149));
#192516=CARTESIAN_POINT('Ctrl Pts',(-59.7243081837712,19.5015944476717,
40.0826642303498));
#192517=CARTESIAN_POINT('Ctrl Pts',(-59.7248734373528,19.501035637399,40.0830009916099));
#192518=CARTESIAN_POINT('Ctrl Pts',(-59.7310334544114,19.4949458381924,
40.0866709464312));
#192519=CARTESIAN_POINT('Ctrl Pts',(-59.7368793392201,19.4882011960855,
40.0899175831877));
#192520=CARTESIAN_POINT('Ctrl Pts',(-59.7422363728287,19.4808775251053,
40.0925642067062));
#192521=CARTESIAN_POINT('Ctrl Pts',(-59.7444986813872,19.4777846933727,
40.0936818922527));
#192522=CARTESIAN_POINT('Ctrl Pts',(-59.7466739523113,19.4745890081272,
40.094693009479));
#192523=CARTESIAN_POINT('Ctrl Pts',(-59.7487501225119,19.4712977780159,
40.0955863397546));
#192524=CARTESIAN_POINT('Ctrl Pts',(-59.7522463412518,19.4657554287472,
40.0970906856166));
#192525=CARTESIAN_POINT('Ctrl Pts',(-59.755459057686,19.4599426670175,40.0982599215483));
#192526=CARTESIAN_POINT('Ctrl Pts',(-59.7583258028879,19.4538995640366,
40.0990497370454));
#192527=CARTESIAN_POINT('Ctrl Pts',(-59.7590424891884,19.4523887882914,
40.0992471909196));
#192528=CARTESIAN_POINT('Ctrl Pts',(-59.7597373347834,19.4508635299957,
40.0994209989363));
#192529=CARTESIAN_POINT('Ctrl Pts',(-59.7604090725466,19.4493243130382,
40.0995705982975));
#192530=CARTESIAN_POINT('Ctrl Pts',(-59.7614166791914,19.447015487602,40.0997949973393));
#192531=CARTESIAN_POINT('Ctrl Pts',(-59.7623722755973,19.4446752658777,
40.0999649129781));
#192532=CARTESIAN_POINT('Ctrl Pts',(-59.7632731754136,19.4423059520264,
40.1000786629733));
#192533=CARTESIAN_POINT('Ctrl Pts',(-59.7641740752299,19.4399366381752,
40.1001924129685));
#192534=CARTESIAN_POINT('Ctrl Pts',(-59.765020284979,19.4375382417963,40.10025));
#192535=CARTESIAN_POINT('Ctrl Pts',(-59.765809437495,19.4351129318425,40.10025));
#192536=CARTESIAN_POINT('Ctrl Pts',(-56.134781019564,18.2553202812753,40.10025));
#192537=CARTESIAN_POINT('Ctrl Pts',(-56.1321105487809,18.2635267101475,
40.10025));
#192538=CARTESIAN_POINT('Ctrl Pts',(-56.1301406315642,18.2718824441051,
40.0995786334241));
#192539=CARTESIAN_POINT('Ctrl Pts',(-56.1288305556597,18.2802419597939,
40.0983063763366));
#192540=CARTESIAN_POINT('Ctrl Pts',(-56.1279843810469,18.2856413491929,
40.0974846287992));
#192541=CARTESIAN_POINT('Ctrl Pts',(-56.1274125556282,18.2910421817937,
40.0964130309338));
#192542=CARTESIAN_POINT('Ctrl Pts',(-56.1270952669251,18.2964056883429,
40.0951176960923));
#192543=CARTESIAN_POINT('Ctrl Pts',(-56.1266747189246,18.3035147090333,
40.0934008039614));
#192544=CARTESIAN_POINT('Ctrl Pts',(-56.126707076608,18.3105573165145,40.0912909372156));
#192545=CARTESIAN_POINT('Ctrl Pts',(-56.1271555587354,18.3174512966903,
40.0888630467851));
#192546=CARTESIAN_POINT('Ctrl Pts',(-56.1273797997991,18.3208982867782,
40.0876491015699));
#192547=CARTESIAN_POINT('Ctrl Pts',(-56.1277080087289,18.3243083090332,
40.0863558569271));
#192548=CARTESIAN_POINT('Ctrl Pts',(-56.1281351437408,18.3276724292423,
40.0849936342771));
#192549=CARTESIAN_POINT('Ctrl Pts',(-56.1283487112468,18.3293544893468,
40.0843125229521));
#192550=CARTESIAN_POINT('Ctrl Pts',(-56.1285870051494,18.3310250895517,
40.0836141747074));
#192551=CARTESIAN_POINT('Ctrl Pts',(-56.1288493629351,18.3326832110574,
40.0828999161609));
#192552=CARTESIAN_POINT('Ctrl Pts',(-56.1289149523815,18.3330977414338,
40.0827213515243));
#192553=CARTESIAN_POINT('Ctrl Pts',(-56.1289820457107,18.3335114922233,
40.0825417925842));
#192554=CARTESIAN_POINT('Ctrl Pts',(-56.1290506323487,18.333924448176,40.082361260236));
#192555=CARTESIAN_POINT('Ctrl Pts',(-56.1292563922627,18.335163316034,40.0818196631917));
#192556=CARTESIAN_POINT('Ctrl Pts',(-56.1294755925117,18.3363950287073,
40.0812693052021));
#192557=CARTESIAN_POINT('Ctrl Pts',(-56.1297079426451,18.3376191892289,
40.0807107531875));
#192558=CARTESIAN_POINT('Ctrl Pts',(-56.1313445869827,18.3462420178745,
40.0767763849182));
#192559=CARTESIAN_POINT('Ctrl Pts',(-56.1335959402407,18.3545284904607,
40.0724140586137));
#192560=CARTESIAN_POINT('Ctrl Pts',(-56.1363459252319,18.3624495731175,
40.0677221223769));
#192561=CARTESIAN_POINT('Ctrl Pts',(-56.1376796649811,18.3662912896465,
40.0654465383721));
#192562=CARTESIAN_POINT('Ctrl Pts',(-56.139131230071,18.3700472768054,40.0630928000679));
#192563=CARTESIAN_POINT('Ctrl Pts',(-56.1406901365233,18.3737149835767,
40.0606689262479));
#192564=CARTESIAN_POINT('Ctrl Pts',(-56.143076713384,18.3793299863883,40.0569581447805));
#192565=CARTESIAN_POINT('Ctrl Pts',(-56.1457125629777,18.3847354115625,
40.0530843804606));
#192566=CARTESIAN_POINT('Ctrl Pts',(-56.1485569297208,18.3899096889383,
40.0490800251458));
#192567=CARTESIAN_POINT('Ctrl Pts',(-56.1498778683511,18.3923126501197,
40.0472203818218));
#192568=CARTESIAN_POINT('Ctrl Pts',(-56.1512435269775,18.3946658026163,
40.0453323608818));
#192569=CARTESIAN_POINT('Ctrl Pts',(-56.1526507491369,18.3969661720541,
40.0434201572162));
#192570=CARTESIAN_POINT('Ctrl Pts',(-56.1527586071707,18.3971424863076,
40.0432735943397));
#192571=CARTESIAN_POINT('Ctrl Pts',(-56.1528666894394,18.397318517929,40.0431268995707));
#192572=CARTESIAN_POINT('Ctrl Pts',(-56.1529749944978,18.3974942667074,
40.0429800745037));
#192573=CARTESIAN_POINT('Ctrl Pts',(-56.1544963540394,18.3999630071783,
40.0409176249753));
#192574=CARTESIAN_POINT('Ctrl Pts',(-56.1560635207937,18.4023749585856,
40.0388310783332));
#192575=CARTESIAN_POINT('Ctrl Pts',(-56.1576709325003,18.4047288488038,
40.036725739981));
#192576=CARTESIAN_POINT('Ctrl Pts',(-56.1634348250113,18.4131694805007,
40.0291763710721));
#192577=CARTESIAN_POINT('Ctrl Pts',(-56.1697591292898,18.4209299141236,
40.0213310894601));
#192578=CARTESIAN_POINT('Ctrl Pts',(-56.1765231650097,18.4280560759379,
40.013283755133));
#192579=CARTESIAN_POINT('Ctrl Pts',(-56.1839561607582,18.4358870118855,
40.004440543134));
#192580=CARTESIAN_POINT('Ctrl Pts',(-56.1919204977421,18.4429525945088,
39.995352871062));
#192581=CARTESIAN_POINT('Ctrl Pts',(-56.2003032932647,18.4492898603057,
39.986110362958));
#192582=CARTESIAN_POINT('Ctrl Pts',(-56.2093546086345,18.4561325169297,
39.9761307737587));
#192583=CARTESIAN_POINT('Ctrl Pts',(-56.2188946068421,18.4621268842274,
39.9659696936049));
#192584=CARTESIAN_POINT('Ctrl Pts',(-56.2288243369826,18.4672816799249,
39.955712821755));
#192585=CARTESIAN_POINT('Ctrl Pts',(-56.238670766892,18.4723932321841,39.945541994519));
#192586=CARTESIAN_POINT('Ctrl Pts',(-56.2489017962809,18.4766796388,39.9352756289355));
#192587=CARTESIAN_POINT('Ctrl Pts',(-56.2594439784237,18.4801050014195,
39.92499));
#192588=CARTESIAN_POINT('Origin',(-0.00470941899426334,-0.0144941013083398,
39.92499));
#192589=CARTESIAN_POINT('Ctrl Pts',(-59.7752282754835,19.4061247292258,
40.10025));
#192590=CARTESIAN_POINT('Ctrl Pts',(-59.7778789856303,19.3979550581542,
40.10025));
#192591=CARTESIAN_POINT('Ctrl Pts',(-59.7798236858212,19.3896365599059,
40.0995859581841));
#192592=CARTESIAN_POINT('Ctrl Pts',(-59.7811061158281,19.3813136269502,
40.0983275959618));
#192593=CARTESIAN_POINT('Ctrl Pts',(-59.7819255275519,19.3759956690079,
40.0975235624066));
#192594=CARTESIAN_POINT('Ctrl Pts',(-59.782475487462,19.3706760212375,40.0964777059489));
#192595=CARTESIAN_POINT('Ctrl Pts',(-59.7827759879494,19.3653918801542,
40.0952149915961));
#192596=CARTESIAN_POINT('Ctrl Pts',(-59.7831861108188,19.3581800878466,
40.0934916398701));
#192597=CARTESIAN_POINT('Ctrl Pts',(-59.7831255716886,19.3510354548623,
40.091364392163));
#192598=CARTESIAN_POINT('Ctrl Pts',(-59.7826350657123,19.3440445557099,
40.0889118607713));
#192599=CARTESIAN_POINT('Ctrl Pts',(-59.7823898127242,19.3405491061338,
40.0876855950754));
#192600=CARTESIAN_POINT('Ctrl Pts',(-59.7820371343798,19.3370918919978,
40.0863782327527));
#192601=CARTESIAN_POINT('Ctrl Pts',(-59.7815825865438,19.3336823180313,
40.0850006373334));
#192602=CARTESIAN_POINT('Ctrl Pts',(-59.7813553126258,19.331977531048,40.0843118396237));
#192603=CARTESIAN_POINT('Ctrl Pts',(-59.7811025767641,19.3302846375614,
40.0836054919165));
#192604=CARTESIAN_POINT('Ctrl Pts',(-59.7808251076835,19.3286047092268,
40.0828829920418));
#192605=CARTESIAN_POINT('Ctrl Pts',(-59.7807557404133,19.3281847271432,
40.0827023670731));
#192606=CARTESIAN_POINT('Ctrl Pts',(-59.7806848274336,19.3277655550294,
40.0825207326933));
#192607=CARTESIAN_POINT('Ctrl Pts',(-59.7806123803665,19.3273472089199,
40.0823381109276));
#192608=CARTESIAN_POINT('Ctrl Pts',(-59.7803950391652,19.3260921705916,
40.0817902456304));
#192609=CARTESIAN_POINT('Ctrl Pts',(-59.7801638905866,19.3248445680581,
40.0812334935553));
#192610=CARTESIAN_POINT('Ctrl Pts',(-59.7799192536868,19.323604818559,40.0806684524227));
#192611=CARTESIAN_POINT('Ctrl Pts',(-59.7782286609225,19.3150373803111,
40.0767636676136));
#192612=CARTESIAN_POINT('Ctrl Pts',(-59.7759321681719,19.3068044648773,
40.0724404510887));
#192613=CARTESIAN_POINT('Ctrl Pts',(-59.7731456380807,19.2989322844405,
40.0677949937408));
#192614=CARTESIAN_POINT('Ctrl Pts',(-59.7717607402743,19.2950198323722,
40.0654862141905));
#192615=CARTESIAN_POINT('Ctrl Pts',(-59.7702542302926,19.2911962646694,
40.0630972003215));
#192616=CARTESIAN_POINT('Ctrl Pts',(-59.7686372707429,19.2874640247238,
40.0606363359906));
#192617=CARTESIAN_POINT('Ctrl Pts',(-59.7650700164609,19.2792301459421,
40.0552073017124));
#192618=CARTESIAN_POINT('Ctrl Pts',(-59.7609769706901,19.2714367138418,
40.0494204304519));
#192619=CARTESIAN_POINT('Ctrl Pts',(-59.7564706723511,19.2641757185816,
40.0434049749851));
#192620=CARTESIAN_POINT('Ctrl Pts',(-59.7548244647405,19.2615231854471,
40.0412074532442));
#192621=CARTESIAN_POINT('Ctrl Pts',(-59.7531276155318,19.2589351484759,
40.0389814735788));
#192622=CARTESIAN_POINT('Ctrl Pts',(-59.7513854342765,19.25641183575,40.0367321210017));
#192623=CARTESIAN_POINT('Ctrl Pts',(-59.7455336317917,19.247936295312,40.029176783714));
#192624=CARTESIAN_POINT('Ctrl Pts',(-59.7391263493543,19.2401420439521,
40.0213235332574));
#192625=CARTESIAN_POINT('Ctrl Pts',(-59.7322837268617,19.2329840462273,
40.0132649215856));
#192626=CARTESIAN_POINT('Ctrl Pts',(-59.7247628741805,19.2251165588073,
40.0044075527529));
#192627=CARTESIAN_POINT('Ctrl Pts',(-59.7167157560782,19.2180171087295,
39.9953016253715));
#192628=CARTESIAN_POINT('Ctrl Pts',(-59.7082546997634,19.2116502033068,
39.9860353422352));
#192629=CARTESIAN_POINT('Ctrl Pts',(-59.699141779585,19.2047927733664,39.9760551582687));
#192630=CARTESIAN_POINT('Ctrl Pts',(-59.6895478207,19.1987842816764,39.9658879738147));
#192631=CARTESIAN_POINT('Ctrl Pts',(-59.6795708632015,19.1936187207966,
39.9556174643244));
#192632=CARTESIAN_POINT('Ctrl Pts',(-59.6697286283157,19.1885229124297,
39.9454856413898));
#192633=CARTESIAN_POINT('Ctrl Pts',(-59.6595122814323,19.1842470541694,
39.935251946511));
#192634=CARTESIAN_POINT('Ctrl Pts',(-59.6489943884562,19.1808295835786,
39.92499));
#192635=CARTESIAN_POINT('Ctrl Pts',(-56.3771794532806,18.117752468711,39.92499));
#192636=CARTESIAN_POINT('Ctrl Pts',(-56.3671137719635,18.1144819305951,
39.9348107241734));
#192637=CARTESIAN_POINT('Ctrl Pts',(-56.3568263239548,18.1120170699777,
39.9446038383193));
#192638=CARTESIAN_POINT('Ctrl Pts',(-56.3463749453322,18.1103629196648,
39.9543158069419));
#192639=CARTESIAN_POINT('Ctrl Pts',(-56.3362832197197,18.1087656919991,
39.9636935671433));
#192640=CARTESIAN_POINT('Ctrl Pts',(-56.3260373921176,18.1079242184405,
39.9729968321037));
#192641=CARTESIAN_POINT('Ctrl Pts',(-56.3156801719786,18.1078879163651,
39.9821731151391));
#192642=CARTESIAN_POINT('Ctrl Pts',(-56.3058893552668,18.1078535995347,
39.9908475764413));
#192643=CARTESIAN_POINT('Ctrl Pts',(-56.2959980926866,18.1085387949872,
39.9994093733911));
#192644=CARTESIAN_POINT('Ctrl Pts',(-56.2860490151071,18.1100266905441,
40.0077966115911));
#192645=CARTESIAN_POINT('Ctrl Pts',(-56.2768860815648,18.1113970173906,
40.0155211172668));
#192646=CARTESIAN_POINT('Ctrl Pts',(-56.2676735798122,18.113448339867,40.0230979941098));
#192647=CARTESIAN_POINT('Ctrl Pts',(-56.2584600414581,18.1162805994807,
40.0304554104827));
#192648=CARTESIAN_POINT('Ctrl Pts',(-56.2557127503117,18.1171251221236,
40.0326492435233));
#192649=CARTESIAN_POINT('Ctrl Pts',(-56.252965504865,18.1180393245087,40.0348233715086));
#192650=CARTESIAN_POINT('Ctrl Pts',(-56.250219989383,18.1190265064344,40.0369753512356));
#192651=CARTESIAN_POINT('Ctrl Pts',(-56.2475025263004,18.1200036017945,
40.0391053430352));
#192652=CARTESIAN_POINT('Ctrl Pts',(-56.2447894850829,18.121050921242,40.041211089324));
#192653=CARTESIAN_POINT('Ctrl Pts',(-56.2420855046789,18.1221702476368,
40.0432881154904));
#192654=CARTESIAN_POINT('Ctrl Pts',(-56.2418974751697,18.1222480834052,
40.043432547828));
#192655=CARTESIAN_POINT('Ctrl Pts',(-56.241709480363,18.1223262596102,40.0435768364421));
#192656=CARTESIAN_POINT('Ctrl Pts',(-56.2415215209612,18.1224047773507,
40.0437209807855));
#192657=CARTESIAN_POINT('Ctrl Pts',(-56.233280692238,18.1258472827278,40.050040796842));
#192658=CARTESIAN_POINT('Ctrl Pts',(-56.2251347899175,18.1299826829659,
40.0560490279345));
#192659=CARTESIAN_POINT('Ctrl Pts',(-56.2171955585582,18.1348427679844,
40.0616647108616));
#192660=CARTESIAN_POINT('Ctrl Pts',(-56.2097948151022,18.1393732118987,
40.0668995033488));
#192661=CARTESIAN_POINT('Ctrl Pts',(-56.2025731376007,18.1445340001514,
40.0717933267484));
#192662=CARTESIAN_POINT('Ctrl Pts',(-56.1956479299625,18.1503626543107,
40.0762460303075));
#192663=CARTESIAN_POINT('Ctrl Pts',(-56.1931145994155,18.1524948514087,
40.077874886875));
#192664=CARTESIAN_POINT('Ctrl Pts',(-56.190621252949,18.1547164978844,40.0794443522248));
#192665=CARTESIAN_POINT('Ctrl Pts',(-56.1881748397224,18.1570296338741,
40.0809482021492));
#192666=CARTESIAN_POINT('Ctrl Pts',(-56.1875865590688,18.1575858658046,
40.0813098278169));
#192667=CARTESIAN_POINT('Ctrl Pts',(-56.1870008763866,18.158147960355,40.0816679525672));
#192668=CARTESIAN_POINT('Ctrl Pts',(-56.186417921567,18.1587158783117,40.0820224192581));
#192669=CARTESIAN_POINT('Ctrl Pts',(-56.1858531840856,18.1592660488322,
40.0823658088648));
#192670=CARTESIAN_POINT('Ctrl Pts',(-56.1852910066464,18.1598216844589,
40.0827057654617));
#192671=CARTESIAN_POINT('Ctrl Pts',(-56.1847315084903,18.1603827459288,
40.0830421470151));
#192672=CARTESIAN_POINT('Ctrl Pts',(-56.1786015595925,18.166529822736,40.0867275956805));
#192673=CARTESIAN_POINT('Ctrl Pts',(-56.172789482861,18.1733325302111,40.0899823432029));
#192674=CARTESIAN_POINT('Ctrl Pts',(-56.1674665972294,18.1807122308847,
40.0926299529354));
#192675=CARTESIAN_POINT('Ctrl Pts',(-56.1652590378995,18.1837728127196,
40.0937279956083));
#192676=CARTESIAN_POINT('Ctrl Pts',(-56.1631354730307,18.1869322368374,
40.0947220371802));
#192677=CARTESIAN_POINT('Ctrl Pts',(-56.1611070880437,18.1901833857457,
40.0956014538693));
#192678=CARTESIAN_POINT('Ctrl Pts',(-56.1576474660759,18.195728559002,40.097101390674));
#192679=CARTESIAN_POINT('Ctrl Pts',(-56.1544671656476,18.2015400422207,
40.0982667904316));
#192680=CARTESIAN_POINT('Ctrl Pts',(-56.1516266854594,18.2075773774756,
40.0990539325583));
#192681=CARTESIAN_POINT('Ctrl Pts',(-56.1502064453653,18.210596045103,40.0994475036216));
#192682=CARTESIAN_POINT('Ctrl Pts',(-56.1488725139552,18.2136716866513,
40.0997467259952));
#192683=CARTESIAN_POINT('Ctrl Pts',(-56.1476325143034,18.21679921973,40.0999473488896));
#192684=CARTESIAN_POINT('Ctrl Pts',(-56.1463925146515,18.2199267528086,
40.100147971784));
#192685=CARTESIAN_POINT('Ctrl Pts',(-56.145246443375,18.2231061318824,40.10025));
#192686=CARTESIAN_POINT('Ctrl Pts',(-56.1441998575526,18.2263320786586,
40.10025));
#192687=CARTESIAN_POINT('Origin',(-53.2204057122636,23.7119335237429,39.92499));
#192688=CARTESIAN_POINT('Ctrl Pts',(-57.1623216544369,25.6588335304445,
39.92499));
#192689=CARTESIAN_POINT('Ctrl Pts',(-57.1720146727776,25.663149140257,39.9348354642022));
#192690=CARTESIAN_POINT('Ctrl Pts',(-57.1820194461954,25.6666871334687,
39.9446440828466));
#192691=CARTESIAN_POINT('Ctrl Pts',(-57.1922776320703,25.6694381454822,
39.9543641760342));
#192692=CARTESIAN_POINT('Ctrl Pts',(-57.2022024879877,25.6720997659864,
39.9637684240726));
#192693=CARTESIAN_POINT('Ctrl Pts',(-57.2123658169602,25.6740249857413,
39.9730909636411));
#192694=CARTESIAN_POINT('Ctrl Pts',(-57.2227298227166,25.6751616470872,
39.9822808977157));
#192695=CARTESIAN_POINT('Ctrl Pts',(-57.2325335339835,25.6762368587288,
39.9909740094667));
#192696=CARTESIAN_POINT('Ctrl Pts',(-57.242517732291,25.6766065729231,39.9995492765019));
#192697=CARTESIAN_POINT('Ctrl Pts',(-57.2526488462854,25.6761845643575,
40.0079462328713));
#192698=CARTESIAN_POINT('Ctrl Pts',(-57.261980334975,25.6757958639482,40.0156804369709));
#192699=CARTESIAN_POINT('Ctrl Pts',(-57.2714370189575,25.6747354076183,
40.0232638017442));
#192700=CARTESIAN_POINT('Ctrl Pts',(-57.2809814365685,25.6728992535086,
40.0306257269986));
#192701=CARTESIAN_POINT('Ctrl Pts',(-57.283749909306,25.672366654999,40.0327611416665));
#192702=CARTESIAN_POINT('Ctrl Pts',(-57.2865256584303,25.6717685445833,
40.0348777427277));
#192703=CARTESIAN_POINT('Ctrl Pts',(-57.2893074725858,25.6711017521909,
40.0369733168701));
#192704=CARTESIAN_POINT('Ctrl Pts',(-57.2923231379853,25.6703789063666,
40.039245053974));
#192705=CARTESIAN_POINT('Ctrl Pts',(-57.2953419866641,25.6695773996878,
40.041487875195));
#192706=CARTESIAN_POINT('Ctrl Pts',(-57.2983617649662,25.6686939261491,
40.0436985701601));
#192707=CARTESIAN_POINT('Ctrl Pts',(-57.3066495702121,25.6662692260898,
40.0497658398386));
#192708=CARTESIAN_POINT('Ctrl Pts',(-57.3149216961104,25.6631888860749,
40.0555581699984));
#192709=CARTESIAN_POINT('Ctrl Pts',(-57.3230760282578,25.6594348051811,
40.0609828468886));
#192710=CARTESIAN_POINT('Ctrl Pts',(-57.3305367994637,25.6560000249771,
40.0659461317305));
#192711=CARTESIAN_POINT('Ctrl Pts',(-57.3378885241129,25.651996242513,40.0706039980707));
#192712=CARTESIAN_POINT('Ctrl Pts',(-57.3450563828669,25.647375921998,40.0748843180603));
#192713=CARTESIAN_POINT('Ctrl Pts',(-57.3485772116719,25.6451064356539,
40.076986797257));
#192714=CARTESIAN_POINT('Ctrl Pts',(-57.3520532672061,25.6426878935086,
40.0789976708175));
#192715=CARTESIAN_POINT('Ctrl Pts',(-57.3554727521279,25.6401130415751,
40.08090504915));
#192716=CARTESIAN_POINT('Ctrl Pts',(-57.3561215660856,25.6396244885001,
40.0812669556104));
#192717=CARTESIAN_POINT('Ctrl Pts',(-57.3567684269675,25.6391297826976,
40.0816253922032));
#192718=CARTESIAN_POINT('Ctrl Pts',(-57.357413196712,25.6386289474847,40.0819801989139));
#192719=CARTESIAN_POINT('Ctrl Pts',(-57.358037817402,25.6381437633723,40.0823239179149));
#192720=CARTESIAN_POINT('Ctrl Pts',(-57.3586604755989,25.6376528269752,
40.0826642303498));
#192721=CARTESIAN_POINT('Ctrl Pts',(-57.3592810442413,25.6371561630119,
40.0830009916099));
#192722=CARTESIAN_POINT('Ctrl Pts',(-57.3660438734347,25.6317436214794,
40.0866709464312));
#192723=CARTESIAN_POINT('Ctrl Pts',(-57.3725627409494,25.6256469885832,
40.0899175831878));
#192724=CARTESIAN_POINT('Ctrl Pts',(-57.3786559602404,25.6189233999297,
40.0925642067062));
#192725=CARTESIAN_POINT('Ctrl Pts',(-57.381229164584,25.6160839866899,40.0936818922528));
#192726=CARTESIAN_POINT('Ctrl Pts',(-57.3837265592142,25.6131331854695,
40.094693009479));
#192727=CARTESIAN_POINT('Ctrl Pts',(-57.386135383163,25.6100770039416,40.0955863397546));
#192728=CARTESIAN_POINT('Ctrl Pts',(-57.3901917825029,25.6049304706143,
40.0970906856166));
#192729=CARTESIAN_POINT('Ctrl Pts',(-57.3939944983912,25.5994853721133,
40.0982599215483));
#192730=CARTESIAN_POINT('Ctrl Pts',(-57.3974772155309,25.5937750303534,
40.0990497370454));
#192731=CARTESIAN_POINT('Ctrl Pts',(-57.3983478948158,25.5923474449134,
40.0992471909196));
#192732=CARTESIAN_POINT('Ctrl Pts',(-57.3991983668797,25.5909031732845,
40.0994209989363));
#192733=CARTESIAN_POINT('Ctrl Pts',(-57.4000273167764,25.5894426040346,
40.0995705982975));
#192734=CARTESIAN_POINT('Ctrl Pts',(-57.4012707416213,25.5872517501599,
40.0997949973393));
#192735=CARTESIAN_POINT('Ctrl Pts',(-57.4024657229506,25.5850242354389,
40.0999649129781));
#192736=CARTESIAN_POINT('Ctrl Pts',(-57.4036093482793,25.5827620706102,
40.1000786629733));
#192737=CARTESIAN_POINT('Ctrl Pts',(-57.404752973608,25.5804999057814,40.1001924129685));
#192738=CARTESIAN_POINT('Ctrl Pts',(-57.4058452484194,25.5782031010735,
40.10025));
#192739=CARTESIAN_POINT('Ctrl Pts',(-57.4068835917977,25.5758735661212,
40.10025));
#192740=CARTESIAN_POINT('Ctrl Pts',(-53.9190682401993,24.0229981225301,
40.10025));
#192741=CARTESIAN_POINT('Ctrl Pts',(-53.9155545931357,24.030880455519,40.10025));
#192742=CARTESIAN_POINT('Ctrl Pts',(-53.9127220553015,24.038984503472,40.0995786334241));
#192743=CARTESIAN_POINT('Ctrl Pts',(-53.9105453488013,24.047161284638,40.0983063763367));
#192744=CARTESIAN_POINT('Ctrl Pts',(-53.9091394197451,24.0524426462852,
40.0974846287993));
#192745=CARTESIAN_POINT('Ctrl Pts',(-53.9080061861137,24.0577541205278,
40.0964130309338));
#192746=CARTESIAN_POINT('Ctrl Pts',(-53.907129996454,24.0630550795266,40.0951176960924));
#192747=CARTESIAN_POINT('Ctrl Pts',(-53.9059686572513,24.0700811970216,
40.0934008039614));
#192748=CARTESIAN_POINT('Ctrl Pts',(-53.9052646847384,24.077088606661,40.0912909372157));
#192749=CARTESIAN_POINT('Ctrl Pts',(-53.9049900928803,24.0839917000397,
40.0888630467852));
#192750=CARTESIAN_POINT('Ctrl Pts',(-53.9048527969512,24.087443246729,40.0876491015699));
#192751=CARTESIAN_POINT('Ctrl Pts',(-53.9048227635321,24.0908688957003,
40.0863558569271));
#192752=CARTESIAN_POINT('Ctrl Pts',(-53.9048959123381,24.0942592346733,
40.0849936342771));
#192753=CARTESIAN_POINT('Ctrl Pts',(-53.9049324867411,24.0959544041598,
40.0843125229521));
#192754=CARTESIAN_POINT('Ctrl Pts',(-53.9049948499726,24.0976407611374,
40.0836141747074));
#192755=CARTESIAN_POINT('Ctrl Pts',(-53.905082449642,24.0993172231362,40.082899916161));
#192756=CARTESIAN_POINT('Ctrl Pts',(-53.9051043495593,24.0997363386359,
40.0827213515244));
#192757=CARTESIAN_POINT('Ctrl Pts',(-53.90512782661,24.1001548360178,40.0825417925842));
#192758=CARTESIAN_POINT('Ctrl Pts',(-53.9051528718721,24.1005726990104,
40.0823612602361));
#192759=CARTESIAN_POINT('Ctrl Pts',(-53.9052280076583,24.1018262879883,
40.0818196631918));
#192760=CARTESIAN_POINT('Ctrl Pts',(-53.9053172580726,24.103074165876,40.0812693052022));
#192761=CARTESIAN_POINT('Ctrl Pts',(-53.9054203757495,24.1043159075204,
40.0807107531875));
#192762=CARTESIAN_POINT('Ctrl Pts',(-53.9061467233509,24.1130625753261,
40.0767763849182));
#192763=CARTESIAN_POINT('Ctrl Pts',(-53.9075195712147,24.1215389842448,
40.0724140586138));
#192764=CARTESIAN_POINT('Ctrl Pts',(-53.909426512903,24.1297041260872,40.0677221223768));
#192765=CARTESIAN_POINT('Ctrl Pts',(-53.9103513775611,24.1336642110574,
40.0654465383721));
#192766=CARTESIAN_POINT('Ctrl Pts',(-53.9114023832598,24.1375513523938,
40.0630928000679));
#192767=CARTESIAN_POINT('Ctrl Pts',(-53.9125693701069,24.1413619171795,
40.0606689262479));
#192768=CARTESIAN_POINT('Ctrl Pts',(-53.9143559454348,24.1471956256299,
40.0569581447806));
#192769=CARTESIAN_POINT('Ctrl Pts',(-53.9164123347818,24.1528469606268,
40.0530843804606));
#192770=CARTESIAN_POINT('Ctrl Pts',(-53.9187002605237,24.1582902100543,
40.0490800251458));
#192771=CARTESIAN_POINT('Ctrl Pts',(-53.9197627850744,24.1608180832481,
40.0472203818218));
#192772=CARTESIAN_POINT('Ctrl Pts',(-53.9208749910656,24.1633010951267,
40.0453323608819));
#192773=CARTESIAN_POINT('Ctrl Pts',(-53.9220340502325,24.1657359576698,
40.0434201572162));
#192774=CARTESIAN_POINT('Ctrl Pts',(-53.9221228875507,24.1659225802899,
40.0432735943397));
#192775=CARTESIAN_POINT('Ctrl Pts',(-53.9222119774186,24.1661089452651,
40.0431268995707));
#192776=CARTESIAN_POINT('Ctrl Pts',(-53.9223013184208,24.1662950522346,
40.0429800745037));
#192777=CARTESIAN_POINT('Ctrl Pts',(-53.9235562901481,24.1689092940619,
40.0409176249753));
#192778=CARTESIAN_POINT('Ctrl Pts',(-53.9248627542248,24.1714718460795,
40.0388310783333));
#192779=CARTESIAN_POINT('Ctrl Pts',(-53.9262153118346,24.1739808617164,
40.036725739981));
#192780=CARTESIAN_POINT('Ctrl Pts',(-53.9310653428793,24.1829777455765,
40.0291763710719));
#192781=CARTESIAN_POINT('Ctrl Pts',(-53.9365438157565,24.1913567365397,
40.0213310894597));
#192782=CARTESIAN_POINT('Ctrl Pts',(-53.9425259106377,24.1991508947535,
40.0132837551323));
#192783=CARTESIAN_POINT('Ctrl Pts',(-53.9490996319574,24.2077158916377,
40.0044405431331));
#192784=CARTESIAN_POINT('Ctrl Pts',(-53.9562817849765,24.2155752681661,
39.995352871061));
#192785=CARTESIAN_POINT('Ctrl Pts',(-53.9639562340132,24.222754058492,39.9861103629567));
#192786=CARTESIAN_POINT('Ctrl Pts',(-53.972242712949,24.2305053504132,39.9761307737573));
#192787=CARTESIAN_POINT('Ctrl Pts',(-53.9811038680465,24.2374640812918,
39.9659696936033));
#192788=CARTESIAN_POINT('Ctrl Pts',(-53.9904403792137,24.2436285779114,
39.9557128217533));
#192789=CARTESIAN_POINT('Ctrl Pts',(-53.9996985666468,24.2497413607391,
39.9455419945179));
#192790=CARTESIAN_POINT('Ctrl Pts',(-54.0094254978892,24.2550737197504,
39.935275628935));
#192791=CARTESIAN_POINT('Ctrl Pts',(-54.0195518809639,24.2595822759737,
39.92499));
#192792=CARTESIAN_POINT('Origin',(-0.00619866644046454,-0.0139224327744755,
39.92499));
#192793=CARTESIAN_POINT('Ctrl Pts',(-57.4192809246787,25.5480287005723,
40.10025));
#192794=CARTESIAN_POINT('Ctrl Pts',(-57.4227710771204,25.5401808584719,
40.10025));
#192795=CARTESIAN_POINT('Ctrl Pts',(-57.4255746438788,25.53211120635,40.0995859581841));
#192796=CARTESIAN_POINT('Ctrl Pts',(-57.4277200319916,25.5239679177298,
40.0983275959618));
#192797=CARTESIAN_POINT('Ctrl Pts',(-57.4290908328637,25.5187647439658,
40.0975235624066));
#192798=CARTESIAN_POINT('Ctrl Pts',(-57.4301938346425,25.5135317242467,
40.0964777059489));
#192799=CARTESIAN_POINT('Ctrl Pts',(-57.4310450321039,25.5083079410952,
40.0952149915961));
#192800=CARTESIAN_POINT('Ctrl Pts',(-57.4322067458447,25.5011785252537,
40.0934916398701));
#192801=CARTESIAN_POINT('Ctrl Pts',(-57.4328933558605,25.4940667032542,
40.0913643921631));
#192802=CARTESIAN_POINT('Ctrl Pts',(-57.4331362848726,25.4870628291429,
40.0889118607713));
#192803=CARTESIAN_POINT('Ctrl Pts',(-57.4332577493786,25.4835608920873,
40.0876855950754));
#192804=CARTESIAN_POINT('Ctrl Pts',(-57.4332683803239,25.4800857520067,
40.0863782327526));
#192805=CARTESIAN_POINT('Ctrl Pts',(-57.4331727200756,25.4766473428563,
40.0850006373334));
#192806=CARTESIAN_POINT('Ctrl Pts',(-57.4331248899515,25.4749281382812,
40.0843118396237));
#192807=CARTESIAN_POINT('Ctrl Pts',(-57.433050494158,25.4732181005509,40.0836054919164));
#192808=CARTESIAN_POINT('Ctrl Pts',(-57.4329501454092,25.4715183716229,
40.0828829920417));
#192809=CARTESIAN_POINT('Ctrl Pts',(-57.4329250582221,25.4710934393909,
40.0827023670731));
#192810=CARTESIAN_POINT('Ctrl Pts',(-57.432898349128,25.470669151121,40.0825207326933));
#192811=CARTESIAN_POINT('Ctrl Pts',(-57.4328700280094,25.4702455239748,
40.0823381109275));
#192812=CARTESIAN_POINT('Ctrl Pts',(-57.4327850646537,25.468974642536,40.0817902456303));
#192813=CARTESIAN_POINT('Ctrl Pts',(-57.4326855923069,25.467709712894,40.0812334935553));
#192814=CARTESIAN_POINT('Ctrl Pts',(-57.4325718846635,25.4664511833531,
40.0806684524227));
#192815=CARTESIAN_POINT('Ctrl Pts',(-57.4317860942974,25.4577539633646,
40.0767636676136));
#192816=CARTESIAN_POINT('Ctrl Pts',(-57.430362755973,25.4493260998447,40.0724404510886));
#192817=CARTESIAN_POINT('Ctrl Pts',(-57.4284143577087,25.4412057723275,
40.0677949937405));
#192818=CARTESIAN_POINT('Ctrl Pts',(-57.4274460091197,25.4371699918417,
40.0654862141903));
#192819=CARTESIAN_POINT('Ctrl Pts',(-57.4263474236136,25.4332098968697,
40.0630972003214));
#192820=CARTESIAN_POINT('Ctrl Pts',(-57.4251294472435,25.4293290842283,
40.0606363359906));
#192821=CARTESIAN_POINT('Ctrl Pts',(-57.4224424094495,25.4207674318879,
40.0552073017123));
#192822=CARTESIAN_POINT('Ctrl Pts',(-57.4191864212927,25.4125888532395,
40.0494204304519));
#192823=CARTESIAN_POINT('Ctrl Pts',(-57.4154637896039,25.4048965980308,
40.0434049749851));
#192824=CARTESIAN_POINT('Ctrl Pts',(-57.4141038653031,25.4020865201986,
40.0412074532442));
#192825=CARTESIAN_POINT('Ctrl Pts',(-57.4126868351393,25.3993352917245,
40.0389814735788));
#192826=CARTESIAN_POINT('Ctrl Pts',(-57.4112179557368,25.3966436944403,
40.0367321210017));
#192827=CARTESIAN_POINT('Ctrl Pts',(-57.4062841452556,25.3876029039784,
40.0291767837139));
#192828=CARTESIAN_POINT('Ctrl Pts',(-57.4007266836985,25.3791816069559,
40.0213235332573));
#192829=CARTESIAN_POINT('Ctrl Pts',(-57.39466976031,25.3713475726776,40.0132649215853));
#192830=CARTESIAN_POINT('Ctrl Pts',(-57.3880124840164,25.3627370410035,
40.0044075527525));
#192831=CARTESIAN_POINT('Ctrl Pts',(-57.3807515434754,25.3548353295669,
39.995301625371));
#192832=CARTESIAN_POINT('Ctrl Pts',(-57.3730023605519,25.3476188815041,
39.9860353422346));
#192833=CARTESIAN_POINT('Ctrl Pts',(-57.3646561585171,25.3398464577401,
39.9760551582679));
#192834=CARTESIAN_POINT('Ctrl Pts',(-57.3557428147453,25.3328680394173,
39.9658879738137));
#192835=CARTESIAN_POINT('Ctrl Pts',(-57.3463604602045,25.326687899985,39.9556174643232));
#192836=CARTESIAN_POINT('Ctrl Pts',(-57.3371047991293,25.3205912133023,
39.945485641389));
#192837=CARTESIAN_POINT('Ctrl Pts',(-57.3273913673568,25.3152708796013,
39.9352519465106));
#192838=CARTESIAN_POINT('Ctrl Pts',(-57.3172883154488,25.3107727110827,
39.92499));
#192839=CARTESIAN_POINT('Ctrl Pts',(-54.1745185419758,23.9115214566119,
39.92499));
#192840=CARTESIAN_POINT('Ctrl Pts',(-54.164849865839,23.9072166846468,39.9348107241718));
#192841=CARTESIAN_POINT('Ctrl Pts',(-54.154876421641,23.903689995663,39.9446038383162));
#192842=CARTESIAN_POINT('Ctrl Pts',(-54.144655202556,23.9009524404123,39.9543158069373));
#192843=CARTESIAN_POINT('Ctrl Pts',(-54.1347857162268,23.8983090899569,
39.9636935671377));
#192844=CARTESIAN_POINT('Ctrl Pts',(-54.1246839742795,23.8964012454643,
39.9729968320972));
#192845=CARTESIAN_POINT('Ctrl Pts',(-54.1143872866774,23.8952825179503,
39.9821731151316));
#192846=CARTESIAN_POINT('Ctrl Pts',(-54.1046536921704,23.8942249700858,
39.9908475764331));
#192847=CARTESIAN_POINT('Ctrl Pts',(-54.0947449925347,23.8938724934881,
39.9994093733825));
#192848=CARTESIAN_POINT('Ctrl Pts',(-54.084694889608,23.8943122764065,40.0077966115819));
#192849=CARTESIAN_POINT('Ctrl Pts',(-54.0754389134156,23.8947173090964,
40.0155211172572));
#192850=CARTESIAN_POINT('Ctrl Pts',(-54.0660624571261,23.8957944255618,
40.0230979940999));
#192851=CARTESIAN_POINT('Ctrl Pts',(-54.0566033397549,23.8976480927548,
40.0304554104726));
#192852=CARTESIAN_POINT('Ctrl Pts',(-54.0537828218984,23.8982008188933,
40.0326492435166));
#192853=CARTESIAN_POINT('Ctrl Pts',(-54.050955065975,23.8988228478381,40.0348233715053));
#192854=CARTESIAN_POINT('Ctrl Pts',(-54.0481214021001,23.8995176373648,
40.0369753512355));
#192855=CARTESIAN_POINT('Ctrl Pts',(-54.0453166912881,23.9002053278543,
40.0391053430352));
#192856=CARTESIAN_POINT('Ctrl Pts',(-54.0425090377018,23.900963319947,40.041211089324));
#192857=CARTESIAN_POINT('Ctrl Pts',(-54.0397028685175,23.9017938716384,
40.0432881154904));
#192858=CARTESIAN_POINT('Ctrl Pts',(-54.0395077330004,23.9018516265787,
40.043432547828));
#192859=CARTESIAN_POINT('Ctrl Pts',(-54.0393125964103,23.901909723718,40.0435768364421));
#192860=CARTESIAN_POINT('Ctrl Pts',(-54.039117459331,23.9019681642227,40.0437209807855));
#192861=CARTESIAN_POINT('Ctrl Pts',(-54.0305619349331,23.9045304100326,
40.0500407968419));
#192862=CARTESIAN_POINT('Ctrl Pts',(-54.0220283896861,23.9077916774639,
40.0560490279344));
#192863=CARTESIAN_POINT('Ctrl Pts',(-54.0136246330487,23.9117952627745,
40.0616647108613));
#192864=CARTESIAN_POINT('Ctrl Pts',(-54.0057908712997,23.9155273001024,
40.0668995033483));
#192865=CARTESIAN_POINT('Ctrl Pts',(-53.9980693056381,23.9199049461654,
40.0717933267479));
#192866=CARTESIAN_POINT('Ctrl Pts',(-53.9905727747499,23.9249777890349,
40.0762460303068));
#192867=CARTESIAN_POINT('Ctrl Pts',(-53.9878304467663,23.9268335005853,
40.0778748868746));
#192868=CARTESIAN_POINT('Ctrl Pts',(-53.9851185338202,23.9287823509749,
40.0794443522246));
#192869=CARTESIAN_POINT('Ctrl Pts',(-53.9824437337505,23.9308270955488,
40.0809482021492));
#192870=CARTESIAN_POINT('Ctrl Pts',(-53.981800533691,23.9313187883098,40.0813098278169));
#192871=CARTESIAN_POINT('Ctrl Pts',(-53.9811593045603,23.9318165831368,
40.0816679525672));
#192872=CARTESIAN_POINT('Ctrl Pts',(-53.9805201796369,23.932320454608,40.0820224192581));
#192873=CARTESIAN_POINT('Ctrl Pts',(-53.9799010273675,23.9328085800958,
40.0823658088648));
#192874=CARTESIAN_POINT('Ctrl Pts',(-53.9792838498569,23.9333024083486,
40.0827057654617));
#192875=CARTESIAN_POINT('Ctrl Pts',(-53.9786687697969,23.9338019127826,
40.0830421470151));
#192876=CARTESIAN_POINT('Ctrl Pts',(-53.9719298569082,23.9392745611218,
40.0867275956807));
#192877=CARTESIAN_POINT('Ctrl Pts',(-53.9654385427826,23.9454324752047,
40.0899823432031));
#192878=CARTESIAN_POINT('Ctrl Pts',(-53.9593734277044,23.9522153560508,
40.0926299529356));
#192879=CARTESIAN_POINT('Ctrl Pts',(-53.9568580436998,23.9550284189137,
40.0937279956085));
#192880=CARTESIAN_POINT('Ctrl Pts',(-53.9544158621939,23.9579485624031,
40.0947220371803));
#192881=CARTESIAN_POINT('Ctrl Pts',(-53.952058751313,23.9609698772116,40.0956014538693));
#192882=CARTESIAN_POINT('Ctrl Pts',(-53.9480384530773,23.9661230444609,
40.097101390674));
#192883=CARTESIAN_POINT('Ctrl Pts',(-53.9442681092574,23.9715702598499,
40.0982667904316));
#192884=CARTESIAN_POINT('Ctrl Pts',(-53.9408121161402,23.9772776109215,
40.0990539325583));
#192885=CARTESIAN_POINT('Ctrl Pts',(-53.9390841195816,23.9801312864573,
40.0994475036216));
#192886=CARTESIAN_POINT('Ctrl Pts',(-53.9374360035028,23.983050645519,40.0997467259952));
#192887=CARTESIAN_POINT('Ctrl Pts',(-53.9358758804723,23.9860314303861,
40.0999473488896));
#192888=CARTESIAN_POINT('Ctrl Pts',(-53.9343157574418,23.9890122152533,
40.100147971784));
#192889=CARTESIAN_POINT('Ctrl Pts',(-53.9328436288551,23.9920543802865,
40.10025));
#192890=CARTESIAN_POINT('Ctrl Pts',(-53.9314655730802,23.9951532569811,
40.10025));
#192891=CARTESIAN_POINT('Origin',(-50.4502867888873,29.1450842944633,39.92499));
#192892=CARTESIAN_POINT('Ctrl Pts',(-54.1671020372436,31.4933613949863,
39.92499));
#192893=CARTESIAN_POINT('Ctrl Pts',(-54.1762908521541,31.4986665597485,
39.9348354642022));
#192894=CARTESIAN_POINT('Ctrl Pts',(-54.185870997383,31.503230955054,39.9446440828465));
#192895=CARTESIAN_POINT('Ctrl Pts',(-54.1957854287843,31.5070391691412,
39.9543641760342));
#192896=CARTESIAN_POINT('Ctrl Pts',(-54.2053777002016,31.5107236389471,
39.9637684240726));
#192897=CARTESIAN_POINT('Ctrl Pts',(-54.2152841131322,31.5137006693058,
39.9730909636412));
#192898=CARTESIAN_POINT('Ctrl Pts',(-54.225472530317,31.5159144374969,39.982280897716));
#192899=CARTESIAN_POINT('Ctrl Pts',(-54.2351101456073,31.5180085258897,
39.9909740094671));
#192900=CARTESIAN_POINT('Ctrl Pts',(-54.2450010037753,31.5194198476569,
39.9995492765025));
#192901=CARTESIAN_POINT('Ctrl Pts',(-54.2551207303742,31.5200591406754,
40.0079462328721));
#192902=CARTESIAN_POINT('Ctrl Pts',(-54.264441730449,31.5206479757802,40.0156804369718));
#192903=CARTESIAN_POINT('Ctrl Pts',(-54.2739574575979,31.5205818213853,
40.0232638017453));
#192904=CARTESIAN_POINT('Ctrl Pts',(-54.2836415202582,31.5197533892255,
40.0306257269999));
#192905=CARTESIAN_POINT('Ctrl Pts',(-54.2864504987155,31.5195130925471,
40.0327611416674));
#192906=CARTESIAN_POINT('Ctrl Pts',(-54.2892735615578,31.5192084034332,
40.0348777427282));
#192907=CARTESIAN_POINT('Ctrl Pts',(-54.2921098354277,31.5188360425582,
40.0369733168701));
#192908=CARTESIAN_POINT('Ctrl Pts',(-54.2951845386599,31.5184323794289,
40.039245053974));
#192909=CARTESIAN_POINT('Ctrl Pts',(-54.2982706300311,31.5179508191008,
40.041487875195));
#192910=CARTESIAN_POINT('Ctrl Pts',(-54.301366213803,31.5173878381079,40.0436985701601));
#192911=CARTESIAN_POINT('Ctrl Pts',(-54.3098620677557,31.5158427323554,
40.0497658398386));
#192912=CARTESIAN_POINT('Ctrl Pts',(-54.3184108612909,31.5136439393736,
40.0555581699984));
#192913=CARTESIAN_POINT('Ctrl Pts',(-54.3269129314605,31.5107627835361,
40.0609828468885));
#192914=CARTESIAN_POINT('Ctrl Pts',(-54.3346918640774,31.5081266823664,
40.0659461317304));
#192915=CARTESIAN_POINT('Ctrl Pts',(-54.3424218244378,31.5049132975215,
40.0706039980706));
#192916=CARTESIAN_POINT('Ctrl Pts',(-54.3500333719147,31.5010675328662,
40.0748843180602));
#192917=CARTESIAN_POINT('Ctrl Pts',(-54.3537721391712,31.4991785058302,
40.0769867972569));
#192918=CARTESIAN_POINT('Ctrl Pts',(-54.3574819590034,31.497136559455,40.0789976708174));
#192919=CARTESIAN_POINT('Ctrl Pts',(-54.3611518569448,31.4949332463338,
40.08090504915));
#192920=CARTESIAN_POINT('Ctrl Pts',(-54.3618481843339,31.4945151891296,
40.0812669556105));
#192921=CARTESIAN_POINT('Ctrl Pts',(-54.3625432124815,31.4940908087512,
40.0816253922032));
#192922=CARTESIAN_POINT('Ctrl Pts',(-54.3632368016451,31.4936601139566,
40.0819801989139));
#192923=CARTESIAN_POINT('Ctrl Pts',(-54.3639087161472,31.4932428783743,
40.0823239179149));
#192924=CARTESIAN_POINT('Ctrl Pts',(-54.3645792801846,31.4928197168827,
40.0826642303498));
#192925=CARTESIAN_POINT('Ctrl Pts',(-54.3652483648078,31.492390640783,40.0830009916099));
#192926=CARTESIAN_POINT('Ctrl Pts',(-54.3725399111639,31.4877146578623,
40.0866709464311));
#192927=CARTESIAN_POINT('Ctrl Pts',(-54.3796603393079,31.4823328301627,
40.0899175831876));
#192928=CARTESIAN_POINT('Ctrl Pts',(-54.3864229856956,31.4762829888804,
40.0925642067061));
#192929=CARTESIAN_POINT('Ctrl Pts',(-54.3892788932592,31.473728103339,40.0936818922527));
#192930=CARTESIAN_POINT('Ctrl Pts',(-54.3920710496174,31.4710545157392,
40.094693009479));
#192931=CARTESIAN_POINT('Ctrl Pts',(-54.3947861357353,31.468266866959,40.0955863397546));
#192932=CARTESIAN_POINT('Ctrl Pts',(-54.399358272915,31.4635725360691,40.0970906856166));
#192933=CARTESIAN_POINT('Ctrl Pts',(-54.4037093249065,31.4585547584355,
40.0982599215483));
#192934=CARTESIAN_POINT('Ctrl Pts',(-54.4077698566062,31.4532397415958,
40.0990497370454));
#192935=CARTESIAN_POINT('Ctrl Pts',(-54.4087849895311,31.4519109873859,
40.0992471909196));
#192936=CARTESIAN_POINT('Ctrl Pts',(-54.4097817701139,31.450563526166,40.0994209989363));
#192937=CARTESIAN_POINT('Ctrl Pts',(-54.4107588499955,31.4491976069261,
40.0995705982975));
#192938=CARTESIAN_POINT('Ctrl Pts',(-54.4122244698178,31.4471487280664,
40.0997949973393));
#192939=CARTESIAN_POINT('Ctrl Pts',(-54.4136457436051,31.4450583254661,
40.0999649129781));
#192940=CARTESIAN_POINT('Ctrl Pts',(-54.4150195646478,31.4429280944112,
40.1000786629733));
#192941=CARTESIAN_POINT('Ctrl Pts',(-54.4163933856905,31.4407978633562,
40.1001924129685));
#192942=CARTESIAN_POINT('Ctrl Pts',(-54.4177197583742,31.4386278145932,
40.10025));
#192943=CARTESIAN_POINT('Ctrl Pts',(-54.4189959163076,31.4364195775148,
40.10025));
#192944=CARTESIAN_POINT('Ctrl Pts',(-51.1126068659044,29.5274749692189,
40.10025));
#192945=CARTESIAN_POINT('Ctrl Pts',(-51.1082885388128,29.534946845835,40.10025));
#192946=CARTESIAN_POINT('Ctrl Pts',(-51.1046244142384,29.5427104181386,
40.0995786334241));
#192947=CARTESIAN_POINT('Ctrl Pts',(-51.1016049255944,29.5506148782564,
40.0983063763366));
#192948=CARTESIAN_POINT('Ctrl Pts',(-51.0996546457477,29.5557203484481,
40.0974846287992));
#192949=CARTESIAN_POINT('Ctrl Pts',(-51.0979724198485,29.5608842707089,
40.0964130309338));
#192950=CARTESIAN_POINT('Ctrl Pts',(-51.0965469289494,29.5660646037408,
40.0951176960923));
#192951=CARTESIAN_POINT('Ctrl Pts',(-51.09465752242,29.5729308384269,40.0934008039614));
#192952=CARTESIAN_POINT('Ctrl Pts',(-51.0932249325811,29.5798262755782,
40.0912909372156));
#192953=CARTESIAN_POINT('Ctrl Pts',(-51.0922302752232,29.586662850424,40.0888630467851));
#192954=CARTESIAN_POINT('Ctrl Pts',(-51.0917329465443,29.590081137847,40.0876491015698));
#192955=CARTESIAN_POINT('Ctrl Pts',(-51.0913449998287,29.5934848814077,
40.0863558569271));
#192956=CARTESIAN_POINT('Ctrl Pts',(-51.0910633609951,29.5968642938813,
40.0849936342771));
#192957=CARTESIAN_POINT('Ctrl Pts',(-51.0909225415783,29.5985540001181,
40.084312522952));
#192958=CARTESIAN_POINT('Ctrl Pts',(-51.0908082908741,29.6002376377885,
40.0836141747074));
#192959=CARTESIAN_POINT('Ctrl Pts',(-51.0907201726668,29.6019140726119,
40.0828999161609));
#192960=CARTESIAN_POINT('Ctrl Pts',(-51.090698143115,29.6023331813177,40.0827213515243));
#192961=CARTESIAN_POINT('Ctrl Pts',(-51.0906777466678,29.6027518401473,
40.0825417925841));
#192962=CARTESIAN_POINT('Ctrl Pts',(-51.0906589761528,29.6031700319854,
40.082361260236));
#192963=CARTESIAN_POINT('Ctrl Pts',(-51.0906026646079,29.6044246075,40.0818196631917));
#192964=CARTESIAN_POINT('Ctrl Pts',(-51.0905609873411,29.6056749785907,
40.0812693052021));
#192965=CARTESIAN_POINT('Ctrl Pts',(-51.0905337427828,29.6069206965768,
40.0807107531874));
#192966=CARTESIAN_POINT('Ctrl Pts',(-51.0903418356315,29.6156953732196,
40.0767763849181));
#192967=CARTESIAN_POINT('Ctrl Pts',(-51.0908211368928,29.6242688491608,
40.0724140586137));
#192968=CARTESIAN_POINT('Ctrl Pts',(-51.0918641424258,29.6325885911861,
40.0677221223768));
#192969=CARTESIAN_POINT('Ctrl Pts',(-51.0923699989822,29.636623657078,40.065446538372));
#192970=CARTESIAN_POINT('Ctrl Pts',(-51.0930089302514,29.640599364258,40.0630928000679));
#192971=CARTESIAN_POINT('Ctrl Pts',(-51.0937712117412,29.6445110377128,
40.0606689262479));
#192972=CARTESIAN_POINT('Ctrl Pts',(-51.094938211443,29.6504995364715,40.0569581447805));
#192973=CARTESIAN_POINT('Ctrl Pts',(-51.0963926103114,29.6563348640824,
40.0530843804605));
#192974=CARTESIAN_POINT('Ctrl Pts',(-51.0980990280588,29.6619874481818,
40.0490800251458));
#192975=CARTESIAN_POINT('Ctrl Pts',(-51.0988914972885,29.6646125374802,
40.0472203818218));
#192976=CARTESIAN_POINT('Ctrl Pts',(-51.0997380650831,29.667198204343,40.0453323608818));
#192977=CARTESIAN_POINT('Ctrl Pts',(-51.1006362623626,29.6697408831279,
40.0434201572162));
#192978=CARTESIAN_POINT('Ctrl Pts',(-51.100705105645,29.6699357694381,40.0432735943397));
#192979=CARTESIAN_POINT('Ctrl Pts',(-51.1007742270248,29.6701304259135,
40.0431268995707));
#192980=CARTESIAN_POINT('Ctrl Pts',(-51.1008436251322,29.6703248520472,
40.0429800745037));
#192981=CARTESIAN_POINT('Ctrl Pts',(-51.1018184593122,29.6730559530504,
40.0409176249753));
#192982=CARTESIAN_POINT('Ctrl Pts',(-51.1028499068175,29.6757410298221,
40.0388310783332));
#192983=CARTESIAN_POINT('Ctrl Pts',(-51.1039327914265,29.6783776815772,
40.036725739981));
#192984=CARTESIAN_POINT('Ctrl Pts',(-51.1078158230491,29.6878322458572,
40.0291763710725));
#192985=CARTESIAN_POINT('Ctrl Pts',(-51.1123884412291,29.6967379921813,
40.0213310894611));
#192986=CARTESIAN_POINT('Ctrl Pts',(-51.1175230541875,29.7051147523653,
40.0132837551345));
#192987=CARTESIAN_POINT('Ctrl Pts',(-51.1231654780111,29.7143199702871,
40.0044405431362));
#192988=CARTESIAN_POINT('Ctrl Pts',(-51.129486757893,29.7228870317459,39.995352871065));
#192989=CARTESIAN_POINT('Ctrl Pts',(-51.1363687775732,29.7308286942709,
39.9861103629617));
#192990=CARTESIAN_POINT('Ctrl Pts',(-51.1437996316763,29.7394036967122,
39.9761307737635));
#192991=CARTESIAN_POINT('Ctrl Pts',(-51.1518848589927,29.7472505498595,
39.9659696936109));
#192992=CARTESIAN_POINT('Ctrl Pts',(-51.1605258584151,29.7543572078857,
39.9557128217622));
#192993=CARTESIAN_POINT('Ctrl Pts',(-51.1690943687355,29.7614042483571,
39.9455419945238));
#192994=CARTESIAN_POINT('Ctrl Pts',(-51.1782106315403,29.767724137325,39.935275628938));
#192995=CARTESIAN_POINT('Ctrl Pts',(-51.1878102687782,29.7732664904684,
39.92499));
#192996=CARTESIAN_POINT('Origin',(-0.00761999999998962,-0.0131982271536776,
39.92499));
#192997=CARTESIAN_POINT('Ctrl Pts',(-54.4342359163061,31.4100231232066,
40.10025));
#192998=CARTESIAN_POINT('Ctrl Pts',(-54.4385272722018,31.4025830926783,
40.10025));
#192999=CARTESIAN_POINT('Ctrl Pts',(-54.4421589890633,31.3948506994807,
40.0995859581842));
#193000=CARTESIAN_POINT('Ctrl Pts',(-54.4451438299608,31.386976274771,40.0983275959622));
#193001=CARTESIAN_POINT('Ctrl Pts',(-54.4470510012003,31.3819448922451,
40.0975235624069));
#193002=CARTESIAN_POINT('Ctrl Pts',(-54.4486949601297,31.3768558346356,
40.0964777059491));
#193003=CARTESIAN_POINT('Ctrl Pts',(-54.4500875286679,31.3717496422767,
40.0952149915961));
#193004=CARTESIAN_POINT('Ctrl Pts',(-54.4519881053011,31.3647807142732,
40.0934916398701));
#193005=CARTESIAN_POINT('Ctrl Pts',(-54.4534143418201,31.3577796218686,
40.091364392163));
#193006=CARTESIAN_POINT('Ctrl Pts',(-54.4543880442394,31.3508395087089,
40.0889118607713));
#193007=CARTESIAN_POINT('Ctrl Pts',(-54.454874895449,31.347369452129,40.0876855950754));
#193008=CARTESIAN_POINT('Ctrl Pts',(-54.4552487192092,31.3439144604658,
40.0863782327526));
#193009=CARTESIAN_POINT('Ctrl Pts',(-54.4555129946223,31.3404848880618,
40.0850006373334));
#193010=CARTESIAN_POINT('Ctrl Pts',(-54.4556451323288,31.3387701018598,
40.0843118396237));
#193011=CARTESIAN_POINT('Ctrl Pts',(-54.4557498916994,31.3370616554172,
40.0836054919164));
#193012=CARTESIAN_POINT('Ctrl Pts',(-54.4558277627244,31.3353607484816,
40.0828829920417));
#193013=CARTESIAN_POINT('Ctrl Pts',(-54.4558472304806,31.3349355217477,
40.0827023670731));
#193014=CARTESIAN_POINT('Ctrl Pts',(-54.4558650179026,31.3345107659128,
40.0825207326933));
#193015=CARTESIAN_POINT('Ctrl Pts',(-54.4558811330247,31.3340864990774,
40.0823381109275));
#193016=CARTESIAN_POINT('Ctrl Pts',(-54.4559294783909,31.3328136985711,
40.0817902456303));
#193017=CARTESIAN_POINT('Ctrl Pts',(-54.4559627721156,31.3315453006544,
40.0812334935553));
#193018=CARTESIAN_POINT('Ctrl Pts',(-54.4559812395335,31.3302817797849,
40.0806684524227));
#193019=CARTESIAN_POINT('Ctrl Pts',(-54.4561088608494,31.3215500666185,
40.0767636676138));
#193020=CARTESIAN_POINT('Ctrl Pts',(-54.4555742713436,31.3130195924495,
40.072440451089));
#193021=CARTESIAN_POINT('Ctrl Pts',(-54.4544853519656,31.30474008586,40.0677949937412));
#193022=CARTESIAN_POINT('Ctrl Pts',(-54.4539441620237,31.3006251938117,
40.0654862141908));
#193023=CARTESIAN_POINT('Ctrl Pts',(-54.4532655373257,31.2965719591991,
40.0630972003217));
#193024=CARTESIAN_POINT('Ctrl Pts',(-54.4524598885392,31.2925850928568,
40.0606363359906));
#193025=CARTESIAN_POINT('Ctrl Pts',(-54.4506825069816,31.2837894702124,
40.0552073017124));
#193026=CARTESIAN_POINT('Ctrl Pts',(-54.4482992497264,31.2753153512351,
40.0494204304519));
#193027=CARTESIAN_POINT('Ctrl Pts',(-54.4454010706195,31.2672761140355,
40.0434049749852));
#193028=CARTESIAN_POINT('Ctrl Pts',(-54.4443423292438,31.2643392793063,
40.0412074532442));
#193029=CARTESIAN_POINT('Ctrl Pts',(-54.443220643404,31.2614550023643,40.0389814735788));
#193030=CARTESIAN_POINT('Ctrl Pts',(-54.4420411592044,31.258624610225,40.0367321210017));
#193031=CARTESIAN_POINT('Ctrl Pts',(-54.438079396587,31.2491176225317,40.029176783714));
#193032=CARTESIAN_POINT('Ctrl Pts',(-54.4334326446225,31.2401615453394,
40.0213235332575));
#193033=CARTESIAN_POINT('Ctrl Pts',(-54.4282277812585,31.2317373058269,
40.0132649215856));
#193034=CARTESIAN_POINT('Ctrl Pts',(-54.422507019865,31.2224780686858,40.004407552753));
#193035=CARTESIAN_POINT('Ctrl Pts',(-54.4161118092699,31.2138606686949,
39.9953016253715));
#193036=CARTESIAN_POINT('Ctrl Pts',(-54.4091594014078,31.2058737429071,
39.9860353422353));
#193037=CARTESIAN_POINT('Ctrl Pts',(-54.4016713602533,31.1972714816212,
39.9760551582689));
#193038=CARTESIAN_POINT('Ctrl Pts',(-54.393536288055,31.1893995936773,39.965887973815));
#193039=CARTESIAN_POINT('Ctrl Pts',(-54.3848513315119,31.1822725865936,
39.9556174643248));
#193040=CARTESIAN_POINT('Ctrl Pts',(-54.376283651206,31.1752418181691,39.94548564139));
#193041=CARTESIAN_POINT('Ctrl Pts',(-54.3671795569342,31.168935299716,39.9352519465111));
#193042=CARTESIAN_POINT('Ctrl Pts',(-54.3576020372436,31.1634057161445,
39.92499));
#193043=CARTESIAN_POINT('Ctrl Pts',(-51.3783102687782,29.4433108116265,
39.92499));
#193044=CARTESIAN_POINT('Ctrl Pts',(-51.3691445298596,29.4380189697945,
39.9348107241715));
#193045=CARTESIAN_POINT('Ctrl Pts',(-51.3595943606127,29.4334690915866,
39.9446038383154));
#193046=CARTESIAN_POINT('Ctrl Pts',(-51.3497152868792,29.4296781246264,
39.9543158069362));
#193047=CARTESIAN_POINT('Ctrl Pts',(-51.3401761719901,29.4260176124823,
39.9636935671362));
#193048=CARTESIAN_POINT('Ctrl Pts',(-51.3303291924955,29.4230642997994,
39.9729968320954));
#193049=CARTESIAN_POINT('Ctrl Pts',(-51.3202058500938,29.4208754038599,
39.9821731151294));
#193050=CARTESIAN_POINT('Ctrl Pts',(-51.3106361210895,29.4188062116774,
39.9908475764306));
#193051=CARTESIAN_POINT('Ctrl Pts',(-51.3008185461848,29.4174199248374,
39.9994093733795));
#193052=CARTESIAN_POINT('Ctrl Pts',(-51.2907775289415,29.4168067767642,
40.0077966115786));
#193053=CARTESIAN_POINT('Ctrl Pts',(-51.2815299205112,29.416242077675,40.0155211172534));
#193054=CARTESIAN_POINT('Ctrl Pts',(-51.2720922401022,29.4163331870167,
40.0230979940956));
#193055=CARTESIAN_POINT('Ctrl Pts',(-51.2624911797833,29.4171879526237,
40.0304554104678));
#193056=CARTESIAN_POINT('Ctrl Pts',(-51.2596283374029,29.4174428264735,
40.0326492435135));
#193057=CARTESIAN_POINT('Ctrl Pts',(-51.2567510524905,29.4177658668977,
40.0348233715038));
#193058=CARTESIAN_POINT('Ctrl Pts',(-51.2538602864392,29.4181606517646,
40.0369753512356));
#193059=CARTESIAN_POINT('Ctrl Pts',(-51.2509990568965,29.4185514029026,
40.0391053430352));
#193060=CARTESIAN_POINT('Ctrl Pts',(-51.2481275521816,29.4190117629205,
40.041211089324));
#193061=CARTESIAN_POINT('Ctrl Pts',(-51.2452499391937,29.4195444402103,
40.0432881154904));
#193062=CARTESIAN_POINT('Ctrl Pts',(-51.2450498356143,29.4195814815473,
40.043432547828));
#193063=CARTESIAN_POINT('Ctrl Pts',(-51.2448496951981,29.4196188630965,
40.0435768364421));
#193064=CARTESIAN_POINT('Ctrl Pts',(-51.244649518404,29.419656586079,40.0437209807855));
#193065=CARTESIAN_POINT('Ctrl Pts',(-51.2358730344468,29.4213104998205,
40.050040796842));
#193066=CARTESIAN_POINT('Ctrl Pts',(-51.2270453415805,29.4236619033168,
40.0560490279345));
#193067=CARTESIAN_POINT('Ctrl Pts',(-51.2182691329811,29.4267651248012,
40.0616647108615));
#193068=CARTESIAN_POINT('Ctrl Pts',(-51.2100881812716,29.429657866561,40.0668995033487));
#193069=CARTESIAN_POINT('Ctrl Pts',(-51.2019513265387,29.4332044080284,
40.0717933267483));
#193070=CARTESIAN_POINT('Ctrl Pts',(-51.1939656059613,29.4374658604804,
40.0762460303074));
#193071=CARTESIAN_POINT('Ctrl Pts',(-51.1910443260611,29.4390247549187,
40.0778748868749));
#193072=CARTESIAN_POINT('Ctrl Pts',(-51.1881435589218,29.440679457209,40.0794443522248));
#193073=CARTESIAN_POINT('Ctrl Pts',(-51.1852696776791,29.4424334077171,
40.0809482021492));
#193074=CARTESIAN_POINT('Ctrl Pts',(-51.184578605248,29.44285517422,40.0813098278168));
#193075=CARTESIAN_POINT('Ctrl Pts',(-51.1838888551093,29.4432832153792,
40.0816679525672));
#193076=CARTESIAN_POINT('Ctrl Pts',(-51.1832005624686,29.4437175198438,
40.0820224192581));
#193077=CARTESIAN_POINT('Ctrl Pts',(-51.1825337789729,29.4441382522937,
40.0823658088648));
#193078=CARTESIAN_POINT('Ctrl Pts',(-51.181868363317,29.4445648626869,40.0827057654616));
#193079=CARTESIAN_POINT('Ctrl Pts',(-51.1812044402991,29.44499733741,40.0830421470151));
#193080=CARTESIAN_POINT('Ctrl Pts',(-51.1739303963593,29.4497355978007,
40.0867275956806));
#193081=CARTESIAN_POINT('Ctrl Pts',(-51.1668309650356,29.4551812510958,
40.0899823432031));
#193082=CARTESIAN_POINT('Ctrl Pts',(-51.160090071181,29.4612929974523,40.0926299529356));
#193083=CARTESIAN_POINT('Ctrl Pts',(-51.1572944215751,29.4638277208379,
40.0937279956085));
#193084=CARTESIAN_POINT('Ctrl Pts',(-51.1545603804836,29.4664765899958,
40.0947220371803));
#193085=CARTESIAN_POINT('Ctrl Pts',(-51.1519003687088,29.4692349685476,
40.0956014538692));
#193086=CARTESIAN_POINT('Ctrl Pts',(-51.1473634414339,29.473939670611,40.097101390674));
#193087=CARTESIAN_POINT('Ctrl Pts',(-51.1430443628982,29.4789629373386,
40.0982667904316));
#193088=CARTESIAN_POINT('Ctrl Pts',(-51.1390107214363,29.4842777732944,
40.0990539325582));
#193089=CARTESIAN_POINT('Ctrl Pts',(-51.1369939007054,29.4869351912723,
40.0994475036216));
#193090=CARTESIAN_POINT('Ctrl Pts',(-51.1350496570624,29.4896662827386,
40.0997467259952));
#193091=CARTESIAN_POINT('Ctrl Pts',(-51.1331865036876,29.4924676612914,
40.0999473488896));
#193092=CARTESIAN_POINT('Ctrl Pts',(-51.1313233503127,29.4952690398443,
40.100147971784));
#193093=CARTESIAN_POINT('Ctrl Pts',(-51.1295412933643,29.4981406602402,
40.10025));
#193094=CARTESIAN_POINT('Ctrl Pts',(-51.1278468659044,29.5010785149115,
40.10025));
#193095=CARTESIAN_POINT('Origin',(-47.1274239660506,34.2589154226526,39.92499));
#193096=CARTESIAN_POINT('Ctrl Pts',(-50.5784163149354,36.9828414016751,
39.92499));
#193097=CARTESIAN_POINT('Ctrl Pts',(-50.5870002518362,36.9890779968912,
39.9348354642021));
#193098=CARTESIAN_POINT('Ctrl Pts',(-50.5960508068,36.9946187858203,39.9446440828463));
#193099=CARTESIAN_POINT('Ctrl Pts',(-50.6055128591422,36.9994424783908,
39.9543641760339));
#193100=CARTESIAN_POINT('Ctrl Pts',(-50.6146674511261,37.004109429676,39.9637684240722));
#193101=CARTESIAN_POINT('Ctrl Pts',(-50.6242084112814,37.008105653671,39.9730909636407));
#193102=CARTESIAN_POINT('Ctrl Pts',(-50.6341096134637,37.0113722741998,
39.9822808977152));
#193103=CARTESIAN_POINT('Ctrl Pts',(-50.6434755410472,37.0144622960732,
39.9909740094662));
#193104=CARTESIAN_POINT('Ctrl Pts',(-50.6531646927636,37.0168997626768,
39.9995492765014));
#193105=CARTESIAN_POINT('Ctrl Pts',(-50.6631621581243,37.0185933530514,
40.0079462328707));
#193106=CARTESIAN_POINT('Ctrl Pts',(-50.6723705467566,37.0201532722699,
40.0156804369703));
#193107=CARTESIAN_POINT('Ctrl Pts',(-50.6818410607734,37.0210821446115,
40.0232638017436));
#193108=CARTESIAN_POINT('Ctrl Pts',(-50.6915586678655,37.0212705108779,
40.030625726998));
#193109=CARTESIAN_POINT('Ctrl Pts',(-50.6943773762883,37.0213251487714,
40.0327611416661));
#193110=CARTESIAN_POINT('Ctrl Pts',(-50.6972168227826,37.021317219197,40.0348777427276));
#193111=CARTESIAN_POINT('Ctrl Pts',(-50.7000764815584,37.0212433695028,
40.0369733168701));
#193112=CARTESIAN_POINT('Ctrl Pts',(-50.7031765355311,37.0211633116862,
40.039245053974));
#193113=CARTESIAN_POINT('Ctrl Pts',(-50.7062960577319,37.0210069737845,
40.041487875195));
#193114=CARTESIAN_POINT('Ctrl Pts',(-50.7094335311101,37.020770653475,40.0436985701601));
#193115=CARTESIAN_POINT('Ctrl Pts',(-50.7180443514157,37.0201220705313,
40.0497658398386));
#193116=CARTESIAN_POINT('Ctrl Pts',(-50.726776150217,37.0188289150185,40.0555581699984));
#193117=CARTESIAN_POINT('Ctrl Pts',(-50.7355328079486,37.0168522507835,
40.0609828468886));
#193118=CARTESIAN_POINT('Ctrl Pts',(-50.7435446743629,37.0150437103242,
40.0659461317304));
#193119=CARTESIAN_POINT('Ctrl Pts',(-50.7515681793714,37.0126559296153,
40.0706039980705));
#193120=CARTESIAN_POINT('Ctrl Pts',(-50.7595400218642,37.0096268558221,
40.0748843180601));
#193121=CARTESIAN_POINT('Ctrl Pts',(-50.7634557648557,37.0081389846697,
40.0769867972568));
#193122=CARTESIAN_POINT('Ctrl Pts',(-50.7673587034235,37.0064960060563,
40.0789976708174));
#193123=CARTESIAN_POINT('Ctrl Pts',(-50.7712388062147,37.0046883717071,
40.08090504915));
#193124=CARTESIAN_POINT('Ctrl Pts',(-50.7719750179266,37.004345390696,40.0812669556105));
#193125=CARTESIAN_POINT('Ctrl Pts',(-50.7727105984661,37.0039959853419,
40.0816253922033));
#193126=CARTESIAN_POINT('Ctrl Pts',(-50.7734454079406,37.0036401497478,
40.081980198914));
#193127=CARTESIAN_POINT('Ctrl Pts',(-50.7741572546191,37.003295434016,40.0823239179149));
#193128=CARTESIAN_POINT('Ctrl Pts',(-50.7748683776569,37.0029446836757,
40.0826642303498));
#193129=CARTESIAN_POINT('Ctrl Pts',(-50.7755786476299,37.0025878964873,
40.0830009916099));
#193130=CARTESIAN_POINT('Ctrl Pts',(-50.7833190234412,36.9986997032257,
40.0866709464312));
#193131=CARTESIAN_POINT('Ctrl Pts',(-50.790962999314,36.9940916451529,40.0899175831878));
#193132=CARTESIAN_POINT('Ctrl Pts',(-50.7983209798296,36.9887818345685,
40.0925642067062));
#193133=CARTESIAN_POINT('Ctrl Pts',(-50.8014283006921,36.9865394685864,
40.0936818922528));
#193134=CARTESIAN_POINT('Ctrl Pts',(-50.8044846273287,36.9841723869926,
40.0946930094791));
#193135=CARTESIAN_POINT('Ctrl Pts',(-50.8074762285637,36.9816838130238,
40.0955863397546));
#193136=CARTESIAN_POINT('Ctrl Pts',(-50.8125140102916,36.9774931166429,
40.0970906856166));
#193137=CARTESIAN_POINT('Ctrl Pts',(-50.81736572735,36.9729576356985,40.0982599215483));
#193138=CARTESIAN_POINT('Ctrl Pts',(-50.8219595855748,36.9680961762159,
40.0990497370454));
#193139=CARTESIAN_POINT('Ctrl Pts',(-50.823108050131,36.9668808113452,40.0992471909196));
#193140=CARTESIAN_POINT('Ctrl Pts',(-50.8242402182961,36.9656449236014,
40.0994209989363));
#193141=CARTESIAN_POINT('Ctrl Pts',(-50.8253547230709,36.9643886196686,
40.0995705982975));
#193142=CARTESIAN_POINT('Ctrl Pts',(-50.8270264802332,36.9625041637694,
40.0997949973393));
#193143=CARTESIAN_POINT('Ctrl Pts',(-50.8286584747053,36.9605737761781,
40.0999649129781));
#193144=CARTESIAN_POINT('Ctrl Pts',(-50.8302474395911,36.9585988181541,
40.1000786629733));
#193145=CARTESIAN_POINT('Ctrl Pts',(-50.831836404477,36.9566238601302,40.1001924129685));
#193146=CARTESIAN_POINT('Ctrl Pts',(-50.8333823430133,36.9546043428186,
40.10025));
#193147=CARTESIAN_POINT('Ctrl Pts',(-50.8348823336483,36.9525415975216,
40.10025));
#193148=CARTESIAN_POINT('Ctrl Pts',(-47.7461450747862,34.7084426211235,
40.10025));
#193149=CARTESIAN_POINT('Ctrl Pts',(-47.7410693801614,34.7154221779233,
40.10025));
#193150=CARTESIAN_POINT('Ctrl Pts',(-47.7366138137623,34.722760215255,40.099578633424));
#193151=CARTESIAN_POINT('Ctrl Pts',(-47.7327846251238,34.7303057514058,
40.0983063763364));
#193152=CARTESIAN_POINT('Ctrl Pts',(-47.7303113621611,34.7351793935419,
40.097484628799));
#193153=CARTESIAN_POINT('Ctrl Pts',(-47.7280985748132,34.7401391868077,
40.0964130309337));
#193154=CARTESIAN_POINT('Ctrl Pts',(-47.7261394006516,34.7451421370598,
40.0951176960923));
#193155=CARTESIAN_POINT('Ctrl Pts',(-47.7235426275286,34.7517732610328,
40.0934008039614));
#193156=CARTESIAN_POINT('Ctrl Pts',(-47.7213971161177,34.7584811778435,
40.0912909372156));
#193157=CARTESIAN_POINT('Ctrl Pts',(-47.7196932909343,34.7651763312119,
40.0888630467851));
#193158=CARTESIAN_POINT('Ctrl Pts',(-47.7188413783425,34.7685239078962,
40.0876491015698));
#193159=CARTESIAN_POINT('Ctrl Pts',(-47.7180997687559,34.7718684539195,
40.0863558569271));
#193160=CARTESIAN_POINT('Ctrl Pts',(-47.7174664279767,34.7751999143435,
40.0849936342771));
#193161=CARTESIAN_POINT('Ctrl Pts',(-47.7171497575871,34.7768656445556,
40.0843125229521));
#193162=CARTESIAN_POINT('Ctrl Pts',(-47.7168601447018,34.7785281166321,
40.0836141747074));
#193163=CARTESIAN_POINT('Ctrl Pts',(-47.7165972740595,34.7801861569093,
40.0828999161609));
#193164=CARTESIAN_POINT('Ctrl Pts',(-47.7165315563989,34.7806006669786,
40.0827213515243));
#193165=CARTESIAN_POINT('Ctrl Pts',(-47.7164675099214,34.781014900342,40.0825417925841));
#193166=CARTESIAN_POINT('Ctrl Pts',(-47.7164051292831,34.7814288392284,
40.082361260236));
#193167=CARTESIAN_POINT('Ctrl Pts',(-47.7162179873681,34.7826706558878,
40.0818196631917));
#193168=CARTESIAN_POINT('Ctrl Pts',(-47.7160458390452,34.7839098208541,
40.0812693052021));
#193169=CARTESIAN_POINT('Ctrl Pts',(-47.7158885307486,34.785145866835,40.0807107531874));
#193170=CARTESIAN_POINT('Ctrl Pts',(-47.7147804714196,34.7938524151218,
40.076776384918));
#193171=CARTESIAN_POINT('Ctrl Pts',(-47.7143609747535,34.8024290252895,
40.0724140586133));
#193172=CARTESIAN_POINT('Ctrl Pts',(-47.7145286167444,34.8108122146634,
40.0677221223761));
#193173=CARTESIAN_POINT('Ctrl Pts',(-47.7146099229288,34.8148780524502,
40.0654465383716));
#193174=CARTESIAN_POINT('Ctrl Pts',(-47.7148297795037,34.8188987667935,
40.0630928000677));
#193175=CARTESIAN_POINT('Ctrl Pts',(-47.7151790039206,34.8228686918042,
40.0606689262479));
#193176=CARTESIAN_POINT('Ctrl Pts',(-47.7157136421035,34.8289463696256,
40.0569581447805));
#193177=CARTESIAN_POINT('Ctrl Pts',(-47.7165501157949,34.8349017567799,
40.0530843804605));
#193178=CARTESIAN_POINT('Ctrl Pts',(-47.7176563296779,34.8407017446571,
40.0490800251457));
#193179=CARTESIAN_POINT('Ctrl Pts',(-47.718170061128,34.8433952890324,40.0472203818218));
#193180=CARTESIAN_POINT('Ctrl Pts',(-47.7187417155519,34.8460552817722,
40.0453323608818));
#193181=CARTESIAN_POINT('Ctrl Pts',(-47.7193692101068,34.848677918678,40.0434201572162));
#193182=CARTESIAN_POINT('Ctrl Pts',(-47.719417305092,34.8488789334632,40.0432735943397));
#193183=CARTESIAN_POINT('Ctrl Pts',(-47.7194657006753,34.8490797487416,
40.0431268995707));
#193184=CARTESIAN_POINT('Ctrl Pts',(-47.7195143955476,34.8492803638661,
40.0429800745037));
#193185=CARTESIAN_POINT('Ctrl Pts',(-47.7201984116931,34.852098401531,40.0409176249753));
#193186=CARTESIAN_POINT('Ctrl Pts',(-47.7209435418724,34.8548765847939,
40.0388310783333));
#193187=CARTESIAN_POINT('Ctrl Pts',(-47.72174488917,34.8576119849589,40.036725739981));
#193188=CARTESIAN_POINT('Ctrl Pts',(-47.7246183780643,34.8674206434755,
40.0291763710721));
#193189=CARTESIAN_POINT('Ctrl Pts',(-47.7282350429862,34.8767555719415,
40.0213310894601));
#193190=CARTESIAN_POINT('Ctrl Pts',(-47.7324659181288,34.8856231565592,
40.013283755133));
#193191=CARTESIAN_POINT('Ctrl Pts',(-47.7371152248812,34.895367741226,40.0044405431341));
#193192=CARTESIAN_POINT('Ctrl Pts',(-47.7425063743619,34.9045486250982,
39.9953528710623));
#193193=CARTESIAN_POINT('Ctrl Pts',(-47.7485205638392,34.9131661493066,
39.9861103629584));
#193194=CARTESIAN_POINT('Ctrl Pts',(-47.7550143791189,34.922470912748,39.9761307737596));
#193195=CARTESIAN_POINT('Ctrl Pts',(-47.7622350952138,34.9311199163996,
39.9659696936062));
#193196=CARTESIAN_POINT('Ctrl Pts',(-47.7700859102955,34.9390908738006,
39.9557128217568));
#193197=CARTESIAN_POINT('Ctrl Pts',(-47.7778708651077,34.9469949630615,
39.9455419945202));
#193198=CARTESIAN_POINT('Ctrl Pts',(-47.7862765797878,34.9542331399567,
39.9352756289362));
#193199=CARTESIAN_POINT('Ctrl Pts',(-47.7952442955499,34.960748566837,39.92499));
#193200=CARTESIAN_POINT('Origin',(-0.00895784724492722,-0.0123294189942774,
39.92499));
#193201=CARTESIAN_POINT('Ctrl Pts',(-50.8527980281382,36.9278827595331,
40.10025));
#193202=CARTESIAN_POINT('Ctrl Pts',(-50.8578435704955,36.9209320551071,
40.10025));
#193203=CARTESIAN_POINT('Ctrl Pts',(-50.8622636476106,36.9136216385506,
40.0995859581841));
#193204=CARTESIAN_POINT('Ctrl Pts',(-50.8660552387516,36.9061023515948,
40.0983275959619));
#193205=CARTESIAN_POINT('Ctrl Pts',(-50.8684778849907,36.9012978851883,
40.0975235624067));
#193206=CARTESIAN_POINT('Ctrl Pts',(-50.8706447895121,36.8964085464701,
40.096477705949));
#193207=CARTESIAN_POINT('Ctrl Pts',(-50.8725634718543,36.8914758894172,
40.0952149915962));
#193208=CARTESIAN_POINT('Ctrl Pts',(-50.8751820882648,36.8847438022852,
40.0934916398702));
#193209=CARTESIAN_POINT('Ctrl Pts',(-50.8773323251411,36.8779301449088,
40.0913643921631));
#193210=CARTESIAN_POINT('Ctrl Pts',(-50.8790261328802,36.8711298300327,
40.0889118607713));
#193211=CARTESIAN_POINT('Ctrl Pts',(-50.8798730367497,36.8677296725946,
40.0876855950755));
#193212=CARTESIAN_POINT('Ctrl Pts',(-50.8806059576334,36.8643326829604,
40.0863782327527));
#193213=CARTESIAN_POINT('Ctrl Pts',(-50.8812272732512,36.8609495224156,
40.0850006373334));
#193214=CARTESIAN_POINT('Ctrl Pts',(-50.8815379310601,36.8592579421432,
40.0843118396238));
#193215=CARTESIAN_POINT('Ctrl Pts',(-50.881820697829,36.857569805085,40.0836054919165));
#193216=CARTESIAN_POINT('Ctrl Pts',(-50.8820759354566,36.8558863556342,
40.0828829920418));
#193217=CARTESIAN_POINT('Ctrl Pts',(-50.8821397448634,36.8554654932715,
40.0827023670731));
#193218=CARTESIAN_POINT('Ctrl Pts',(-50.8822018339187,36.8550449235853,
40.0825207326933));
#193219=CARTESIAN_POINT('Ctrl Pts',(-50.8822622087208,36.854624665417,40.0823381109276));
#193220=CARTESIAN_POINT('Ctrl Pts',(-50.882443333127,36.8533638909118,40.0817902456304));
#193221=CARTESIAN_POINT('Ctrl Pts',(-50.8826090281503,36.8521059215536,
40.0812334935553));
#193222=CARTESIAN_POINT('Ctrl Pts',(-50.8827594682965,36.8508512527543,
40.0806684524227));
#193223=CARTESIAN_POINT('Ctrl Pts',(-50.8837991030485,36.8421807128858,
40.0767636676135));
#193224=CARTESIAN_POINT('Ctrl Pts',(-50.8841591194358,36.8336410897268,
40.0724404510885));
#193225=CARTESIAN_POINT('Ctrl Pts',(-50.8839416093724,36.8252931160711,
40.0677949937404));
#193226=CARTESIAN_POINT('Ctrl Pts',(-50.883833507468,36.8211441960794,40.0654862141902));
#193227=CARTESIAN_POINT('Ctrl Pts',(-50.8835822787324,36.8170422299139,
40.0630972003214));
#193228=CARTESIAN_POINT('Ctrl Pts',(-50.8831977843863,36.8129929908134,
40.0606363359906));
#193229=CARTESIAN_POINT('Ctrl Pts',(-50.8823495324293,36.8040597645473,
40.0552073017123));
#193230=CARTESIAN_POINT('Ctrl Pts',(-50.880865117541,36.795382949462,40.0494204304519));
#193231=CARTESIAN_POINT('Ctrl Pts',(-50.8788231440728,36.7870848098366,
40.0434049749852));
#193232=CARTESIAN_POINT('Ctrl Pts',(-50.8780771854142,36.7840533947864,
40.0412074532442));
#193233=CARTESIAN_POINT('Ctrl Pts',(-50.8772631333232,36.7810676701181,
40.0389814735788));
#193234=CARTESIAN_POINT('Ctrl Pts',(-50.8763859670022,36.7781294934923,
40.0367321210017));
#193235=CARTESIAN_POINT('Ctrl Pts',(-50.8734396581486,36.7682604691132,
40.0291767837134));
#193236=CARTESIAN_POINT('Ctrl Pts',(-50.8697545265629,36.758867736406,40.0213235332562));
#193237=CARTESIAN_POINT('Ctrl Pts',(-50.865458748795,36.7499455893893,40.0132649215836));
#193238=CARTESIAN_POINT('Ctrl Pts',(-50.8607371801598,36.7401390929203,
40.0044075527503));
#193239=CARTESIAN_POINT('Ctrl Pts',(-50.8552777667754,36.7309004184117,
39.9953016253681));
#193240=CARTESIAN_POINT('Ctrl Pts',(-50.8491983060091,36.7222305213288,
39.9860353422311));
#193241=CARTESIAN_POINT('Ctrl Pts',(-50.8426504662796,36.712892670695,39.9760551582639));
#193242=CARTESIAN_POINT('Ctrl Pts',(-50.835382795207,36.7042135591809,39.965887973809));
#193243=CARTESIAN_POINT('Ctrl Pts',(-50.8274903908619,36.6962177694265,
39.955617464318));
#193244=CARTESIAN_POINT('Ctrl Pts',(-50.8197045606257,36.688329949833,39.9454856413854));
#193245=CARTESIAN_POINT('Ctrl Pts',(-50.8113095502191,36.6811063421661,
39.9352519465088));
#193246=CARTESIAN_POINT('Ctrl Pts',(-50.8023624960588,36.6746059268182,
39.92499));
#193247=CARTESIAN_POINT('Ctrl Pts',(-48.0191904766733,34.6525130919801,
39.92499));
#193248=CARTESIAN_POINT('Ctrl Pts',(-48.010628096725,34.6462921588067,39.9348107241726));
#193249=CARTESIAN_POINT('Ctrl Pts',(-48.0016058360806,34.6407689407917,
39.9446038383178));
#193250=CARTESIAN_POINT('Ctrl Pts',(-47.9921771448961,34.6359660967489,
39.9543158069396));
#193251=CARTESIAN_POINT('Ctrl Pts',(-47.9830729139848,34.6313285282528,
39.9636935671405));
#193252=CARTESIAN_POINT('Ctrl Pts',(-47.9735885825097,34.6273621044913,
39.9729968321003));
#193253=CARTESIAN_POINT('Ctrl Pts',(-47.9637494987646,34.6241270221285,
39.9821731151351));
#193254=CARTESIAN_POINT('Ctrl Pts',(-47.9544484832155,34.6210688561306,
39.9908475764368));
#193255=CARTESIAN_POINT('Ctrl Pts',(-47.9448295964456,34.6186639474974,
39.9994093733862));
#193256=CARTESIAN_POINT('Ctrl Pts',(-47.9349076763704,34.6170045862116,
40.0077966115857));
#193257=CARTESIAN_POINT('Ctrl Pts',(-47.925769754434,34.6154763423054,40.0155211172608));
#193258=CARTESIAN_POINT('Ctrl Pts',(-47.9163742511055,34.614580446311,40.0230979941034));
#193259=CARTESIAN_POINT('Ctrl Pts',(-47.9067364390635,34.6144269453423,
40.0304554104759));
#193260=CARTESIAN_POINT('Ctrl Pts',(-47.9038626380648,34.614381174452,40.0326492435188));
#193261=CARTESIAN_POINT('Ctrl Pts',(-47.9009673483046,34.6144016870568,
40.0348233715064));
#193262=CARTESIAN_POINT('Ctrl Pts',(-47.8980511519203,34.6144921419178,
40.0369753512356));
#193263=CARTESIAN_POINT('Ctrl Pts',(-47.8951647518764,34.614581672553,40.0391053430352));
#193264=CARTESIAN_POINT('Ctrl Pts',(-47.8922608568396,34.6147393566955,
40.041211089324));
#193265=CARTESIAN_POINT('Ctrl Pts',(-47.8893433277782,34.6149683234599,
40.0432881154904));
#193266=CARTESIAN_POINT('Ctrl Pts',(-47.8891404485131,34.6149842453609,
40.043432547828));
#193267=CARTESIAN_POINT('Ctrl Pts',(-47.8889374970512,34.6150005017599,
40.0435768364421));
#193268=CARTESIAN_POINT('Ctrl Pts',(-47.8887344737211,34.6150170939192,
40.0437209807855));
#193269=CARTESIAN_POINT('Ctrl Pts',(-47.8798331871996,34.6157445549673,
40.050040796842));
#193270=CARTESIAN_POINT('Ctrl Pts',(-47.8708080647645,34.6171603320597,
40.0560490279345));
#193271=CARTESIAN_POINT('Ctrl Pts',(-47.8617555581811,34.6193291901739,
40.0616647108615));
#193272=CARTESIAN_POINT('Ctrl Pts',(-47.8533170487303,34.6213509428814,
40.0668995033486));
#193273=CARTESIAN_POINT('Ctrl Pts',(-47.8448540540095,34.6240275231024,
40.0717933267482));
#193274=CARTESIAN_POINT('Ctrl Pts',(-47.836466636969,34.627430895772,40.0762460303073));
#193275=CARTESIAN_POINT('Ctrl Pts',(-47.8333984113056,34.6286758935248,
40.0778748868749));
#193276=CARTESIAN_POINT('Ctrl Pts',(-47.8303405713846,34.6300183184515,
40.0794443522248));
#193277=CARTESIAN_POINT('Ctrl Pts',(-47.8272990958127,34.6314622582452,
40.0809482021492));
#193278=CARTESIAN_POINT('Ctrl Pts',(-47.8265677225444,34.6318094775279,
40.0813098278168));
#193279=CARTESIAN_POINT('Ctrl Pts',(-47.8258370084445,34.6321630753108,
40.0816679525672));
#193280=CARTESIAN_POINT('Ctrl Pts',(-47.8251070891646,34.632523054438,40.082022419258));
#193281=CARTESIAN_POINT('Ctrl Pts',(-47.8243999798623,34.6328717842175,
40.0823658088648));
#193282=CARTESIAN_POINT('Ctrl Pts',(-47.8236936164941,34.6332265027183,
40.0827057654616));
#193283=CARTESIAN_POINT('Ctrl Pts',(-47.8229881245977,34.6335872094468,
40.0830421470151));
#193284=CARTESIAN_POINT('Ctrl Pts',(-47.8152586455543,34.6375391685166,
40.0867275956807));
#193285=CARTESIAN_POINT('Ctrl Pts',(-47.8076288798876,34.642212897307,40.0899823432033));
#193286=CARTESIAN_POINT('Ctrl Pts',(-47.8002860619002,34.647586547602,40.0926299529359));
#193287=CARTESIAN_POINT('Ctrl Pts',(-47.7972407764152,34.6498151605504,
40.0937279956086));
#193288=CARTESIAN_POINT('Ctrl Pts',(-47.7942448304646,34.652163733812,40.0947220371803));
#193289=CARTESIAN_POINT('Ctrl Pts',(-47.7913110614416,34.6546289547342,
40.0956014538692));
#193290=CARTESIAN_POINT('Ctrl Pts',(-47.7863072126523,34.6588336459114,
40.097101390674));
#193291=CARTESIAN_POINT('Ctrl Pts',(-47.7814867201291,34.6633779280163,
40.0982667904316));
#193292=CARTESIAN_POINT('Ctrl Pts',(-47.7769196237422,34.6682420184012,
40.0990539325583));
#193293=CARTESIAN_POINT('Ctrl Pts',(-47.7746360755488,34.6706740635937,
40.0994475036216));
#193294=CARTESIAN_POINT('Ctrl Pts',(-47.7724170058819,34.6731869650549,
40.0997467259952));
#193295=CARTESIAN_POINT('Ctrl Pts',(-47.770271235261,34.6757782448038,40.0999473488896));
#193296=CARTESIAN_POINT('Ctrl Pts',(-47.7681254646401,34.6783695245527,
40.100147971784));
#193297=CARTESIAN_POINT('Ctrl Pts',(-47.7660530039191,34.6810391382374,
40.10025));
#193298=CARTESIAN_POINT('Ctrl Pts',(-47.764060769276,34.683783783135,40.10025));
#193299=CARTESIAN_POINT('Origin',(-43.2882232241945,38.9973987043323,39.92499));
#193300=CARTESIAN_POINT('Ctrl Pts',(-46.4355828792667,42.06712965881,39.92499));
#193301=CARTESIAN_POINT('Ctrl Pts',(-46.443467890749,42.074229355038,39.934835464202));
#193302=CARTESIAN_POINT('Ctrl Pts',(-46.4518896956737,42.0806858315476,
39.9446440828461));
#193303=CARTESIAN_POINT('Ctrl Pts',(-46.4607957007314,42.0864721532162,
39.9543641760336));
#193304=CARTESIAN_POINT('Ctrl Pts',(-46.4694123136565,42.0920704538858,
39.9637684240718));
#193305=CARTESIAN_POINT('Ctrl Pts',(-46.4784832882807,42.0970420880509,
39.9730909636402));
#193306=CARTESIAN_POINT('Ctrl Pts',(-46.4879887958175,42.1013257711392,
39.9822808977148));
#193307=CARTESIAN_POINT('Ctrl Pts',(-46.4969804206318,42.1053778715668,
39.9909740094658));
#193308=CARTESIAN_POINT('Ctrl Pts',(-46.5063617095229,42.1088147776126,
39.999549276501));
#193309=CARTESIAN_POINT('Ctrl Pts',(-46.516127379323,42.1115441100126,40.0079462328704));
#193310=CARTESIAN_POINT('Ctrl Pts',(-46.5251222674801,42.1140580225433,
40.01568043697));
#193311=CARTESIAN_POINT('Ctrl Pts',(-46.5344438074317,42.1159717447016,
40.0232638017433));
#193312=CARTESIAN_POINT('Ctrl Pts',(-46.544088490819,42.1171748456138,40.0306257269978));
#193313=CARTESIAN_POINT('Ctrl Pts',(-46.5468860468472,42.1175238194551,
40.0327611416659));
#193314=CARTESIAN_POINT('Ctrl Pts',(-46.5497107674229,42.1178127362983,
40.0348777427275));
#193315=CARTESIAN_POINT('Ctrl Pts',(-46.5525624800839,42.1180382068978,
40.0369733168701));
#193316=CARTESIAN_POINT('Ctrl Pts',(-46.5556539199571,42.1182826315242,
40.039245053974));
#193317=CARTESIAN_POINT('Ctrl Pts',(-46.5587726948496,42.1184532289196,
40.041487875195));
#193318=CARTESIAN_POINT('Ctrl Pts',(-46.5619176830191,42.1185461584682,
40.0436985701601));
#193319=CARTESIAN_POINT('Ctrl Pts',(-46.5705491277285,42.1188012043438,
40.0497658398386));
#193320=CARTESIAN_POINT('Ctrl Pts',(-46.5793682643808,42.1184278543824,
40.0555581699984));
#193321=CARTESIAN_POINT('Ctrl Pts',(-46.5882835699001,42.117377338497,40.0609828468885));
#193322=CARTESIAN_POINT('Ctrl Pts',(-46.596440590427,42.1164161734957,40.0659461317304));
#193323=CARTESIAN_POINT('Ctrl Pts',(-46.6046697328837,42.114880157948,40.0706039980706));
#193324=CARTESIAN_POINT('Ctrl Pts',(-46.6129145292181,42.1127009621831,
40.0748843180603));
#193325=CARTESIAN_POINT('Ctrl Pts',(-46.6169643462448,42.111630548342,40.076986797257));
#193326=CARTESIAN_POINT('Ctrl Pts',(-46.6210176421362,42.1104045383081,
40.0789976708175));
#193327=CARTESIAN_POINT('Ctrl Pts',(-46.6250654385589,42.1090123875511,
40.08090504915));
#193328=CARTESIAN_POINT('Ctrl Pts',(-46.6258334685041,42.1087482405047,
40.0812669556105));
#193329=CARTESIAN_POINT('Ctrl Pts',(-46.6266015422611,42.1084776383331,
40.0816253922033));
#193330=CARTESIAN_POINT('Ctrl Pts',(-46.6273695213203,42.1082005605488,
40.0819801989139));
#193331=CARTESIAN_POINT('Ctrl Pts',(-46.6281135010338,42.1079321414453,
40.0823239179149));
#193332=CARTESIAN_POINT('Ctrl Pts',(-46.6288573918593,42.1076576451504,
40.0826642303498));
#193333=CARTESIAN_POINT('Ctrl Pts',(-46.6296010653156,42.1073770559083,
40.0830009916099));
#193334=CARTESIAN_POINT('Ctrl Pts',(-46.6377054654047,42.1043192521649,
40.0866709464311));
#193335=CARTESIAN_POINT('Ctrl Pts',(-46.6457892400066,42.1005354505678,
40.0899175831876));
#193336=CARTESIAN_POINT('Ctrl Pts',(-46.6536619390755,42.0960238460775,
40.092564206706));
#193337=CARTESIAN_POINT('Ctrl Pts',(-46.6569866287796,42.0941185674854,
40.0936818922527));
#193338=CARTESIAN_POINT('Ctrl Pts',(-46.6602736399407,42.0920839261387,
40.094693009479));
#193339=CARTESIAN_POINT('Ctrl Pts',(-46.663508979684,42.0899216923182,40.0955863397546));
#193340=CARTESIAN_POINT('Ctrl Pts',(-46.6689572109691,42.0862805445929,
40.0970906856166));
#193341=CARTESIAN_POINT('Ctrl Pts',(-46.6742564366672,42.082277052016,40.0982599215483));
#193342=CARTESIAN_POINT('Ctrl Pts',(-46.6793332901452,42.0779224130581,
40.0990497370454));
#193343=CARTESIAN_POINT('Ctrl Pts',(-46.6806025035147,42.0768337533186,
40.0992471909196));
#193344=CARTESIAN_POINT('Ctrl Pts',(-46.6818576549908,42.0757229796955,
40.0994209989363));
#193345=CARTESIAN_POINT('Ctrl Pts',(-46.6830973739113,42.0745900553985,
40.0995705982975));
#193346=CARTESIAN_POINT('Ctrl Pts',(-46.6849569522921,42.0728906689529,
40.0997949973393));
#193347=CARTESIAN_POINT('Ctrl Pts',(-46.6867817869761,42.0711414461011,
40.0999649129781));
#193348=CARTESIAN_POINT('Ctrl Pts',(-46.6885684866733,42.0693433991615,
40.1000786629733));
#193349=CARTESIAN_POINT('Ctrl Pts',(-46.6903551863704,42.0675453522219,
40.1001924129685));
#193350=CARTESIAN_POINT('Ctrl Pts',(-46.692103753136,42.065698492618,40.10025));
#193351=CARTESIAN_POINT('Ctrl Pts',(-46.6938111422614,42.0638038389716,
40.10025));
#193352=CARTESIAN_POINT('Ctrl Pts',(-43.8565665267053,39.5091373124626,
40.10025));
#193353=CARTESIAN_POINT('Ctrl Pts',(-43.8507890749205,39.5155480799605,
40.10025));
#193354=CARTESIAN_POINT('Ctrl Pts',(-43.8455908828149,39.5223801852468,
40.0995786334241));
#193355=CARTESIAN_POINT('Ctrl Pts',(-43.8409939475741,39.5294841269568,
40.0983063763366));
#193356=CARTESIAN_POINT('Ctrl Pts',(-43.8380247990815,39.5340725443949,
40.0974846287992));
#193357=CARTESIAN_POINT('Ctrl Pts',(-43.8353056940458,39.5387738681335,
40.0964130309338));
#193358=CARTESIAN_POINT('Ctrl Pts',(-43.8328343017434,39.5435446222366,
40.0951176960924));
#193359=CARTESIAN_POINT('Ctrl Pts',(-43.8295586128166,39.5498679835147,
40.0934008039614));
#193360=CARTESIAN_POINT('Ctrl Pts',(-43.8267236865058,39.5563148866446,
40.0912909372157));
#193361=CARTESIAN_POINT('Ctrl Pts',(-43.824329360962,39.5627952650343,40.0888630467851));
#193362=CARTESIAN_POINT('Ctrl Pts',(-43.8231321981901,39.5660354542291,
40.0876491015699));
#193363=CARTESIAN_POINT('Ctrl Pts',(-43.8220450509623,39.5692841591689,
40.0863558569271));
#193364=CARTESIAN_POINT('Ctrl Pts',(-43.8210669472515,39.5725311673658,
40.0849936342771));
#193365=CARTESIAN_POINT('Ctrl Pts',(-43.8205778953961,39.5741546714643,
40.0843125229521));
#193366=CARTESIAN_POINT('Ctrl Pts',(-43.8201160933892,39.575777763555,40.0836141747074));
#193367=CARTESIAN_POINT('Ctrl Pts',(-43.8196813503776,39.5773992434498,
40.0828999161609));
#193368=CARTESIAN_POINT('Ctrl Pts',(-43.8195726646246,39.5778046134235,
40.0827213515243));
#193369=CARTESIAN_POINT('Ctrl Pts',(-43.8194656698236,39.5782098828933,
40.0825417925842));
#193370=CARTESIAN_POINT('Ctrl Pts',(-43.8193603625172,39.578615033627,40.0823612602361));
#193371=CARTESIAN_POINT('Ctrl Pts',(-43.8190444405982,39.5798304858279,
40.0818196631917));
#193372=CARTESIAN_POINT('Ctrl Pts',(-43.8187437073121,39.5810448681193,
40.0812693052022));
#193373=CARTESIAN_POINT('Ctrl Pts',(-43.8184580587799,39.5822576997164,
40.0807107531875));
#193374=CARTESIAN_POINT('Ctrl Pts',(-43.8164459874032,39.5908007288814,
40.0767763849182));
#193375=CARTESIAN_POINT('Ctrl Pts',(-43.8151322889029,39.5992865061389,
40.0724140586138));
#193376=CARTESIAN_POINT('Ctrl Pts',(-43.8144227306309,39.6076412948835,
40.067722122377));
#193377=CARTESIAN_POINT('Ctrl Pts',(-43.8140785956357,39.6116933583964,
40.0654465383722));
#193378=CARTESIAN_POINT('Ctrl Pts',(-43.8138769687216,39.6157150281163,
40.063092800068));
#193379=CARTESIAN_POINT('Ctrl Pts',(-43.81380930989,39.6196997093545,40.0606689262479));
#193380=CARTESIAN_POINT('Ctrl Pts',(-43.8137057289461,39.6257999779285,
40.0569581447806));
#193381=CARTESIAN_POINT('Ctrl Pts',(-43.8139151128796,39.6318101761584,
40.0530843804606));
#193382=CARTESIAN_POINT('Ctrl Pts',(-43.8144090029875,39.6376940219324,
40.0490800251458));
#193383=CARTESIAN_POINT('Ctrl Pts',(-43.8146383681086,39.6404265103488,
40.0472203818218));
#193384=CARTESIAN_POINT('Ctrl Pts',(-43.8149288459964,39.6431316855285,
40.0453323608818));
#193385=CARTESIAN_POINT('Ctrl Pts',(-43.815278762865,39.6458055463964,40.0434201572162));
#193386=CARTESIAN_POINT('Ctrl Pts',(-43.8153055826142,39.6460104872964,
40.0432735943397));
#193387=CARTESIAN_POINT('Ctrl Pts',(-43.8153327221691,39.6462152612037,
40.0431268995707));
#193388=CARTESIAN_POINT('Ctrl Pts',(-43.8153601802951,39.6464198673378,
40.0429800745037));
#193389=CARTESIAN_POINT('Ctrl Pts',(-43.815745884182,39.649293966654,40.0409176249753));
#193390=CARTESIAN_POINT('Ctrl Pts',(-43.8161965332331,39.6521348180509,
40.0388310783332));
#193391=CARTESIAN_POINT('Ctrl Pts',(-43.8167075634907,39.6549389970091,
40.036725739981));
#193392=CARTESIAN_POINT('Ctrl Pts',(-43.8185400271108,39.664994284047,40.0291763710717));
#193393=CARTESIAN_POINT('Ctrl Pts',(-43.8211611138367,39.6746561192251,
40.0213310894592));
#193394=CARTESIAN_POINT('Ctrl Pts',(-43.8244418968098,39.6839173731639,
40.0132837551316));
#193395=CARTESIAN_POINT('Ctrl Pts',(-43.8280471477135,39.6940945608674,
40.0044405431319));
#193396=CARTESIAN_POINT('Ctrl Pts',(-43.8324491002312,39.7037886794685,
39.9953528710591));
#193397=CARTESIAN_POINT('Ctrl Pts',(-43.8375295667874,39.7129876499623,
39.9861103629542));
#193398=CARTESIAN_POINT('Ctrl Pts',(-43.8430151956451,39.7229202294695,
39.9761307737535));
#193399=CARTESIAN_POINT('Ctrl Pts',(-43.8492922888428,39.7322766233327,
39.9659696935982));
#193400=CARTESIAN_POINT('Ctrl Pts',(-43.8562669044119,39.7410245486321,
39.9557128217468));
#193401=CARTESIAN_POINT('Ctrl Pts',(-43.8631830101213,39.7496990878249,
39.9455419945135));
#193402=CARTESIAN_POINT('Ctrl Pts',(-43.8707860819068,39.757776249665,39.9352756289328));
#193403=CARTESIAN_POINT('Ctrl Pts',(-43.8790236240217,39.7651933659002,
39.92499));
#193404=CARTESIAN_POINT('Origin',(-0.0101975504408993,-0.0113255271402792,
39.92499));
#193405=CARTESIAN_POINT('Ctrl Pts',(-46.7142062431419,42.0411527846899,
40.10025));
#193406=CARTESIAN_POINT('Ctrl Pts',(-46.7199506919431,42.0347675597384,
40.10025));
#193407=CARTESIAN_POINT('Ctrl Pts',(-46.7251107020222,42.0279592142763,
40.099585958184));
#193408=CARTESIAN_POINT('Ctrl Pts',(-46.7296675019408,42.0208774479559,
40.0983275959616));
#193409=CARTESIAN_POINT('Ctrl Pts',(-46.7325790801602,42.0163525364081,
40.0975235624064));
#193410=CARTESIAN_POINT('Ctrl Pts',(-46.7352451892141,42.0117164851992,
40.0964777059487));
#193411=CARTESIAN_POINT('Ctrl Pts',(-46.737668963875,42.007011406675,40.0952149915961));
#193412=CARTESIAN_POINT('Ctrl Pts',(-46.7409769299532,42.00058991857,40.09349163987));
#193413=CARTESIAN_POINT('Ctrl Pts',(-46.7438276087417,41.9940383480781,
40.091364392163));
#193414=CARTESIAN_POINT('Ctrl Pts',(-46.7462229640885,41.9874523371584,
40.0889118607712));
#193415=CARTESIAN_POINT('Ctrl Pts',(-46.7474206417619,41.9841593316986,
40.0876855950754));
#193416=CARTESIAN_POINT('Ctrl Pts',(-46.7485046297344,41.9808575622227,
40.0863782327526));
#193417=CARTESIAN_POINT('Ctrl Pts',(-46.749476178293,41.9775578801521,40.0850006373333));
#193418=CARTESIAN_POINT('Ctrl Pts',(-46.7499619525723,41.9759080391169,
40.0843118396237));
#193419=CARTESIAN_POINT('Ctrl Pts',(-46.7504196286878,41.9742587070259,
40.0836054919164));
#193420=CARTESIAN_POINT('Ctrl Pts',(-46.7508494364809,41.9726111592843,
40.0828829920417));
#193421=CARTESIAN_POINT('Ctrl Pts',(-46.7509568884292,41.9721992723489,
40.082702367073));
#193422=CARTESIAN_POINT('Ctrl Pts',(-46.7510625988572,41.9717874966611,
40.0825207326932));
#193423=CARTESIAN_POINT('Ctrl Pts',(-46.7511665718603,41.9713758515962,
40.0823381109275));
#193424=CARTESIAN_POINT('Ctrl Pts',(-46.7514784908696,41.9701409164016,
40.0817902456303));
#193425=CARTESIAN_POINT('Ctrl Pts',(-46.751774771802,41.9689071581772,40.0812334935553));
#193426=CARTESIAN_POINT('Ctrl Pts',(-46.7520555364229,41.9676750878623,
40.0806684524226));
#193427=CARTESIAN_POINT('Ctrl Pts',(-46.753995794155,41.9591607175415,40.0767636676136));
#193428=CARTESIAN_POINT('Ctrl Pts',(-46.7552464720206,41.9507055072916,
40.0724404510887));
#193429=CARTESIAN_POINT('Ctrl Pts',(-46.7559027543577,41.9423805287165,
40.0677949937407));
#193430=CARTESIAN_POINT('Ctrl Pts',(-46.7562289248778,41.9382430372166,
40.0654862141904));
#193431=CARTESIAN_POINT('Ctrl Pts',(-46.7564078446192,41.934137281497,40.0630972003215));
#193432=CARTESIAN_POINT('Ctrl Pts',(-46.756448717314,41.9300700339487,40.0606363359906));
#193433=CARTESIAN_POINT('Ctrl Pts',(-46.7565388885835,41.9210970783572,
40.0552073017123));
#193434=CARTESIAN_POINT('Ctrl Pts',(-46.7559695796222,41.9123126321657,
40.0494204304519));
#193435=CARTESIAN_POINT('Ctrl Pts',(-46.7548061840814,41.9038465062688,
40.0434049749851));
#193436=CARTESIAN_POINT('Ctrl Pts',(-46.7543811810191,41.9007537237152,
40.0412074532442));
#193437=CARTESIAN_POINT('Ctrl Pts',(-46.753883681602,41.8976992635449,40.0389814735788));
#193438=CARTESIAN_POINT('Ctrl Pts',(-46.7533184435774,41.8946854937105,
40.0367321210017));
#193439=CARTESIAN_POINT('Ctrl Pts',(-46.7514198688646,41.8845625597445,
40.0291767837145));
#193440=CARTESIAN_POINT('Ctrl Pts',(-46.7487367327317,41.8748360802697,
40.0213235332586));
#193441=CARTESIAN_POINT('Ctrl Pts',(-46.7453971060013,41.8655137786607,
40.0132649215873));
#193442=CARTESIAN_POINT('Ctrl Pts',(-46.7417264606198,41.855267464893,40.0044075527552));
#193443=CARTESIAN_POINT('Ctrl Pts',(-46.737262658923,41.8455087367198,39.9953016253744));
#193444=CARTESIAN_POINT('Ctrl Pts',(-46.7321227530987,41.8362508575498,
39.9860353422388));
#193445=CARTESIAN_POINT('Ctrl Pts',(-46.7265868542985,41.8262797250152,
39.9760551582731));
#193446=CARTESIAN_POINT('Ctrl Pts',(-46.7202662104789,41.8168884800942,
39.9658879738197));
#193447=CARTESIAN_POINT('Ctrl Pts',(-46.7132528291677,41.8081115112156,
39.9556174643302));
#193448=CARTESIAN_POINT('Ctrl Pts',(-46.7063341521825,41.7994530610494,
39.9454856413937));
#193449=CARTESIAN_POINT('Ctrl Pts',(-46.6987402031273,41.7913915075206,
39.9352519465129));
#193450=CARTESIAN_POINT('Ctrl Pts',(-46.6905216402894,41.7839914803031,
39.92499));
#193451=CARTESIAN_POINT('Ctrl Pts',(-44.1339623850444,39.4820551873934,
39.92499));
#193452=CARTESIAN_POINT('Ctrl Pts',(-44.1260971752947,39.4749733207255,
39.9348107241718));
#193453=CARTESIAN_POINT('Ctrl Pts',(-44.1177016730302,39.4685372764368,
39.9446038383161));
#193454=CARTESIAN_POINT('Ctrl Pts',(-44.1088266671104,39.4627751762764,
39.9543158069372));
#193455=CARTESIAN_POINT('Ctrl Pts',(-44.1002570680373,39.4572113615995,
39.9636935671376));
#193456=CARTESIAN_POINT('Ctrl Pts',(-44.0912392969033,39.4522752837282,
39.9729968320971));
#193457=CARTESIAN_POINT('Ctrl Pts',(-44.0817922708769,39.4480294591813,
39.9821731151315));
#193458=CARTESIAN_POINT('Ctrl Pts',(-44.0728618726566,39.4440158252744,
39.9908475764331));
#193459=CARTESIAN_POINT('Ctrl Pts',(-44.0635470605588,39.4406186435298,
39.9994093733824));
#193460=CARTESIAN_POINT('Ctrl Pts',(-44.0538529442853,39.4379312493405,
40.0077966115819));
#193461=CARTESIAN_POINT('Ctrl Pts',(-44.0449248258284,39.4354562043765,
40.0155211172573));
#193462=CARTESIAN_POINT('Ctrl Pts',(-44.0356744386817,39.4335831186693,
40.0230979941));
#193463=CARTESIAN_POINT('Ctrl Pts',(-44.0261054688028,39.4324230329128,
40.0304554104726));
#193464=CARTESIAN_POINT('Ctrl Pts',(-44.0232521951461,39.4320771187579,
40.0326492435167));
#193465=CARTESIAN_POINT('Ctrl Pts',(-44.0203706219338,39.4317948788029,
40.0348233715053));
#193466=CARTESIAN_POINT('Ctrl Pts',(-44.0174609456693,39.431580012616,40.0369753512356));
#193467=CARTESIAN_POINT('Ctrl Pts',(-44.0145809991271,39.4313673418321,
40.0391053430352));
#193468=CARTESIAN_POINT('Ctrl Pts',(-44.0116765294501,39.4312206224786,
40.041211089324));
#193469=CARTESIAN_POINT('Ctrl Pts',(-44.0087510493742,39.4311433701098,
40.0432881154904));
#193470=CARTESIAN_POINT('Ctrl Pts',(-44.0085476172111,39.4311379981311,
40.043432547828));
#193471=CARTESIAN_POINT('Ctrl Pts',(-44.0083440782821,39.4311329512714,
40.0435768364421));
#193472=CARTESIAN_POINT('Ctrl Pts',(-44.0081404327822,39.4311282308205,
40.0437209807855));
#193473=CARTESIAN_POINT('Ctrl Pts',(-43.999211868054,39.4309212689597,40.0500407968421));
#193474=CARTESIAN_POINT('Ctrl Pts',(-43.9900881971801,39.431385908098,40.0560490279346));
#193475=CARTESIAN_POINT('Ctrl Pts',(-43.9808585737691,39.4325966403787,
40.0616647108616));
#193476=CARTESIAN_POINT('Ctrl Pts',(-43.9722549606523,39.4337252532882,
40.0668995033489));
#193477=CARTESIAN_POINT('Ctrl Pts',(-43.9635585482845,39.43550254709,40.0717933267486));
#193478=CARTESIAN_POINT('Ctrl Pts',(-43.9548613290768,39.4380105519141,
40.0762460303077));
#193479=CARTESIAN_POINT('Ctrl Pts',(-43.9516797737731,39.4389280125252,
40.0778748868751));
#193480=CARTESIAN_POINT('Ctrl Pts',(-43.9484983634048,39.4399434521998,
40.0794443522249));
#193481=CARTESIAN_POINT('Ctrl Pts',(-43.9453226165469,39.4410615611726,
40.0809482021492));
#193482=CARTESIAN_POINT('Ctrl Pts',(-43.9445589555198,39.4413304290279,
40.0813098278168));
#193483=CARTESIAN_POINT('Ctrl Pts',(-43.9437952833153,39.4416057093431,
40.0816679525672));
#193484=CARTESIAN_POINT('Ctrl Pts',(-43.9430317345447,39.4418874191264,
40.082022419258));
#193485=CARTESIAN_POINT('Ctrl Pts',(-43.9422920466731,39.4421603254789,
40.0823658088648));
#193486=CARTESIAN_POINT('Ctrl Pts',(-43.9415524746576,39.4424392657174,
40.0827057654617));
#193487=CARTESIAN_POINT('Ctrl Pts',(-43.9408131433996,39.4427242524729,
40.0830421470151));
#193488=CARTESIAN_POINT('Ctrl Pts',(-43.9327129150431,39.445846611731,40.0867275956806));
#193489=CARTESIAN_POINT('Ctrl Pts',(-43.9246364083432,39.4496972096656,
40.089982343203));
#193490=CARTESIAN_POINT('Ctrl Pts',(-43.9167721156739,39.4542738890614,
40.0926299529355));
#193491=CARTESIAN_POINT('Ctrl Pts',(-43.9135105590943,39.4561719744232,
40.0937279956084));
#193492=CARTESIAN_POINT('Ctrl Pts',(-43.9102855324948,39.4581945203286,
40.0947220371802));
#193493=CARTESIAN_POINT('Ctrl Pts',(-43.9071101492106,39.4603395741454,
40.0956014538692));
#193494=CARTESIAN_POINT('Ctrl Pts',(-43.9016942021212,39.46399818696,40.097101390674));
#193495=CARTESIAN_POINT('Ctrl Pts',(-43.8964251099353,39.4680136963364,
40.0982667904316));
#193496=CARTESIAN_POINT('Ctrl Pts',(-43.8913745966873,39.4723737491584,
40.0990539325583));
#193497=CARTESIAN_POINT('Ctrl Pts',(-43.8888493400632,39.4745537755694,
40.0994475036216));
#193498=CARTESIAN_POINT('Ctrl Pts',(-43.8863797569641,39.4768209551514,
40.0997467259952));
#193499=CARTESIAN_POINT('Ctrl Pts',(-43.8839748786091,39.4791737454931,
40.0999473488896));
#193500=CARTESIAN_POINT('Ctrl Pts',(-43.8815700002541,39.4815265358349,
40.100147971784));
#193501=CARTESIAN_POINT('Ctrl Pts',(-43.8792298420738,39.4839648939621,
40.10025));
#193502=CARTESIAN_POINT('Ctrl Pts',(-43.8769616275871,39.486486258182,40.10025));
#193503=CARTESIAN_POINT('Origin',(-38.974747650051,43.308618325077,39.92499));
#193504=CARTESIAN_POINT('Ctrl Pts',(-41.7839914803023,46.6905216402901,
39.92499));
#193505=CARTESIAN_POINT('Ctrl Pts',(-41.7910911765302,46.6984066517723,
39.9348354642018));
#193506=CARTESIAN_POINT('Ctrl Pts',(-41.7987919603585,46.7057080773547,
39.9446440828458));
#193507=CARTESIAN_POINT('Ctrl Pts',(-41.8070443420765,46.7123936319702,
39.9543641760331));
#193508=CARTESIAN_POINT('Ctrl Pts',(-41.8150285705285,46.7188619458705,
39.9637684240712));
#193509=CARTESIAN_POINT('Ctrl Pts',(-41.8235301761253,46.7247545199412,
39.9730909636396));
#193510=CARTESIAN_POINT('Ctrl Pts',(-41.8325358446866,46.7300083326607,
39.982280897714));
#193511=CARTESIAN_POINT('Ctrl Pts',(-41.8410546526086,46.7349781159823,
39.9909740094649));
#193512=CARTESIAN_POINT('Ctrl Pts',(-41.85002529531,46.7393768060084,39.9995492765));
#193513=CARTESIAN_POINT('Ctrl Pts',(-41.8594521748275,46.7431119772969,
40.0079462328693));
#193514=CARTESIAN_POINT('Ctrl Pts',(-41.8681350126323,46.7465523401881,
40.0156804369688));
#193515=CARTESIAN_POINT('Ctrl Pts',(-41.8772054497763,46.7494299450226,
40.023263801742));
#193516=CARTESIAN_POINT('Ctrl Pts',(-41.8866715402891,46.7516345991555,
40.0306257269964));
#193517=CARTESIAN_POINT('Ctrl Pts',(-41.8894172933139,46.7522740855142,
40.032761141665));
#193518=CARTESIAN_POINT('Ctrl Pts',(-41.8921963397416,46.7528566833418,
40.034877742727));
#193519=CARTESIAN_POINT('Ctrl Pts',(-41.8950088623276,46.753379003932,40.0369733168701));
#193520=CARTESIAN_POINT('Ctrl Pts',(-41.8980578176392,46.7539452330339,
40.039245053974));
#193521=CARTESIAN_POINT('Ctrl Pts',(-41.9011416752729,46.7544408966257,
40.041487875195));
#193522=CARTESIAN_POINT('Ctrl Pts',(-41.9042597210852,46.7548620578769,
40.0436985701601));
#193523=CARTESIAN_POINT('Ctrl Pts',(-41.912817222284,46.7560179382357,40.0497658398386));
#193524=CARTESIAN_POINT('Ctrl Pts',(-41.9216270724807,46.7565684843261,
40.0555581699984));
#193525=CARTESIAN_POINT('Ctrl Pts',(-41.9306033478346,46.7564556264622,
40.0609828468885));
#193526=CARTESIAN_POINT('Ctrl Pts',(-41.93881615245,46.7563523676438,40.0659461317303));
#193527=CARTESIAN_POINT('Ctrl Pts',(-41.947160772148,46.755684946165,40.0706039980704));
#193528=CARTESIAN_POINT('Ctrl Pts',(-41.9555881906097,46.7543795041533,
40.0748843180601));
#193529=CARTESIAN_POINT('Ctrl Pts',(-41.959727711029,46.7537382753016,40.0769867972568));
#193530=CARTESIAN_POINT('Ctrl Pts',(-41.9638869554863,46.7529426662696,
40.0789976708174));
#193531=CARTESIAN_POINT('Ctrl Pts',(-41.9680580970361,46.7519812517998,
40.08090504915));
#193532=CARTESIAN_POINT('Ctrl Pts',(-41.9688495305177,46.7517988327685,
40.0812669556104));
#193533=CARTESIAN_POINT('Ctrl Pts',(-41.9696416823154,46.7516099985534,
40.0816253922032));
#193534=CARTESIAN_POINT('Ctrl Pts',(-41.97043441682,46.7514147143011,40.0819801989139));
#193535=CARTESIAN_POINT('Ctrl Pts',(-41.9712023783712,46.7512255326816,
40.0823239179149));
#193536=CARTESIAN_POINT('Ctrl Pts',(-41.9719708867608,46.7510302978709,
40.0826642303498));
#193537=CARTESIAN_POINT('Ctrl Pts',(-41.9727398158584,46.7508289807696,
40.0830009916099));
#193538=CARTESIAN_POINT('Ctrl Pts',(-41.9811194467224,46.7486350684821,
40.0866709464312));
#193539=CARTESIAN_POINT('Ctrl Pts',(-41.9895544525278,46.7457169794824,
40.0899175831878));
#193540=CARTESIAN_POINT('Ctrl Pts',(-41.9978556152119,46.7420530111689,
40.0925642067063));
#193541=CARTESIAN_POINT('Ctrl Pts',(-42.001361247761,46.740505694598,40.0936818922528));
#193542=CARTESIAN_POINT('Ctrl Pts',(-42.004842930264,46.738825785455,40.0946930094791));
#193543=CARTESIAN_POINT('Ctrl Pts',(-42.0082865614559,46.7370135816692,
40.0955863397546));
#193544=CARTESIAN_POINT('Ctrl Pts',(-42.0140855503362,46.7339618757759,
40.0970906856166));
#193545=CARTESIAN_POINT('Ctrl Pts',(-42.0197742252482,46.730534234669,40.0982599215483));
#193546=CARTESIAN_POINT('Ctrl Pts',(-42.0252784509101,46.7267341265712,
40.0990497370454));
#193547=CARTESIAN_POINT('Ctrl Pts',(-42.0266545073256,46.7257840995468,
40.0992471909196));
#193548=CARTESIAN_POINT('Ctrl Pts',(-42.0280188904104,46.7248106099129,
40.0994209989363));
#193549=CARTESIAN_POINT('Ctrl Pts',(-42.0293702408567,46.7238134778073,
40.0995705982975));
#193550=CARTESIAN_POINT('Ctrl Pts',(-42.0313972665262,46.722317779649,40.0997949973393));
#193551=CARTESIAN_POINT('Ctrl Pts',(-42.0333949481515,46.7207688863881,
40.0999649129781));
#193552=CARTESIAN_POINT('Ctrl Pts',(-42.0353598072042,46.7191674503114,
40.1000786629733));
#193553=CARTESIAN_POINT('Ctrl Pts',(-42.037324666257,46.7175660142347,40.1001924129685));
#193554=CARTESIAN_POINT('Ctrl Pts',(-42.0392567035859,46.7159120469166,
40.10025));
#193555=CARTESIAN_POINT('Ctrl Pts',(-42.0411527846891,46.7142062431426,
40.10025));
#193556=CARTESIAN_POINT('Ctrl Pts',(-39.4864862581813,43.8769616275878,
40.10025));
#193557=CARTESIAN_POINT('Ctrl Pts',(-39.4800703482072,43.8827333680737,
40.10025));
#193558=CARTESIAN_POINT('Ctrl Pts',(-39.4741864828755,43.8889846873396,
40.0995786334241));
#193559=CARTESIAN_POINT('Ctrl Pts',(-39.4688721660171,43.8955692023369,
40.0983063763367));
#193560=CARTESIAN_POINT('Ctrl Pts',(-39.4654396626067,43.8998221234152,
40.0974846287993));
#193561=CARTESIAN_POINT('Ctrl Pts',(-39.4622440309669,43.9042134689399,
40.0964130309338));
#193562=CARTESIAN_POINT('Ctrl Pts',(-39.459287497615,43.9086997575136,40.0951176960923));
#193563=CARTESIAN_POINT('Ctrl Pts',(-39.4553687820178,43.9146460760273,
40.0934008039614));
#193564=CARTESIAN_POINT('Ctrl Pts',(-39.451875500853,43.9207613318566,40.0912909372156));
#193565=CARTESIAN_POINT('Ctrl Pts',(-39.4488169076806,43.9269559348857,
40.0888630467851));
#193566=CARTESIAN_POINT('Ctrl Pts',(-39.4472876110944,43.9300532364003,
40.0876491015699));
#193567=CARTESIAN_POINT('Ctrl Pts',(-39.4458668372378,43.9331705067655,
40.0863558569271));
#193568=CARTESIAN_POINT('Ctrl Pts',(-39.4445546869045,43.9362974878339,
40.0849936342771));
#193569=CARTESIAN_POINT('Ctrl Pts',(-39.4438986117379,43.9378609783681,
40.0843125229521));
#193570=CARTESIAN_POINT('Ctrl Pts',(-39.4432696802086,43.9394269075364,
40.0836141747074));
#193571=CARTESIAN_POINT('Ctrl Pts',(-39.4426678279631,43.9409940617758,
40.0828999161609));
#193572=CARTESIAN_POINT('Ctrl Pts',(-39.4425173649017,43.9413858503356,
40.0827213515243));
#193573=CARTESIAN_POINT('Ctrl Pts',(-39.4423685940344,43.9417777156947,
40.0825417925842));
#193574=CARTESIAN_POINT('Ctrl Pts',(-39.4422215138289,43.9421696393594,
40.082361260236));
#193575=CARTESIAN_POINT('Ctrl Pts',(-39.4417802732125,43.9433454103533,
40.0818196631917));
#193576=CARTESIAN_POINT('Ctrl Pts',(-39.44135424986,43.9445217049432,40.0812693052021));
#193577=CARTESIAN_POINT('Ctrl Pts',(-39.4409433907174,43.9456980341198,
40.0807107531874));
#193578=CARTESIAN_POINT('Ctrl Pts',(-39.4380493519679,43.953983944948,40.0767763849182));
#193579=CARTESIAN_POINT('Ctrl Pts',(-39.4358558447891,43.9622859173442,
40.0724140586139));
#193580=CARTESIAN_POINT('Ctrl Pts',(-39.4342768603232,43.970520768646,40.0677221223771));
#193581=CARTESIAN_POINT('Ctrl Pts',(-39.4335110545634,43.974514662629,40.0654465383723));
#193582=CARTESIAN_POINT('Ctrl Pts',(-39.4328901532271,43.97849322547,40.063092800068));
#193583=CARTESIAN_POINT('Ctrl Pts',(-39.4324063524312,43.9824490059339,
40.0606689262479));
#193584=CARTESIAN_POINT('Ctrl Pts',(-39.4316656872149,43.9885050294414,
40.0569581447805));
#193585=CARTESIAN_POINT('Ctrl Pts',(-39.4312456873365,43.9945041897574,
40.0530843804606));
#193586=CARTESIAN_POINT('Ctrl Pts',(-39.4311218425058,44.0004074287826,
40.0490800251458));
#193587=CARTESIAN_POINT('Ctrl Pts',(-39.4310643283257,44.0031489235252,
40.0472203818218));
#193588=CARTESIAN_POINT('Ctrl Pts',(-39.4310704471408,44.0058696426794,
40.0453323608819));
#193589=CARTESIAN_POINT('Ctrl Pts',(-39.4311389525607,44.0085654321303,
40.0434201572162));
#193590=CARTESIAN_POINT('Ctrl Pts',(-39.4311442032312,44.0087720537698,
40.0432735943397));
#193591=CARTESIAN_POINT('Ctrl Pts',(-39.4311497894109,44.0089785427601,
40.0431268995708));
#193592=CARTESIAN_POINT('Ctrl Pts',(-39.4311557099537,44.0091848981961,
40.0429800745037));
#193593=CARTESIAN_POINT('Ctrl Pts',(-39.4312388757296,44.0120835699301,
40.0409176249753));
#193594=CARTESIAN_POINT('Ctrl Pts',(-39.4313901062471,44.0149559644986,
40.0388310783332));
#193595=CARTESIAN_POINT('Ctrl Pts',(-39.4316052205102,44.0177981990786,
40.036725739981));
#193596=CARTESIAN_POINT('Ctrl Pts',(-39.432376582001,44.0279899468076,40.0291763710721));
#193597=CARTESIAN_POINT('Ctrl Pts',(-39.433973373356,44.0378728316087,40.0213310894601));
#193598=CARTESIAN_POINT('Ctrl Pts',(-39.4362681192144,44.0474262866314,
40.0132837551329));
#193599=CARTESIAN_POINT('Ctrl Pts',(-39.438789814385,44.0579245739714,40.0044405431341));
#193600=CARTESIAN_POINT('Ctrl Pts',(-39.4421543412256,44.0680257165074,
39.9953528710623));
#193601=CARTESIAN_POINT('Ctrl Pts',(-39.4462454222044,44.0777053474392,
39.9861103629585));
#193602=CARTESIAN_POINT('Ctrl Pts',(-39.4506627629399,44.0881569195892,
39.9761307737599));
#193603=CARTESIAN_POINT('Ctrl Pts',(-39.4559274600905,44.0981181930518,
39.9659696936068));
#193604=CARTESIAN_POINT('Ctrl Pts',(-39.4619494607956,44.1075472421469,
39.9557128217576));
#193605=CARTESIAN_POINT('Ctrl Pts',(-39.4679209431045,44.1168971912117,
39.9455419945208));
#193606=CARTESIAN_POINT('Ctrl Pts',(-39.4746380711547,44.1257248429273,
39.9352756289364));
#193607=CARTESIAN_POINT('Ctrl Pts',(-39.4820551873926,44.1339623850451,
39.92499));
#193608=CARTESIAN_POINT('Origin',(-0.0113255271402662,-0.0101975504409131,
39.92499));
#193609=CARTESIAN_POINT('Ctrl Pts',(-42.0638038389696,46.6938111422608,
40.10025));
#193610=CARTESIAN_POINT('Ctrl Pts',(-42.07018425683,46.6880613546461,40.10025));
#193611=CARTESIAN_POINT('Ctrl Pts',(-42.0760276657216,46.681829673938,40.0995859581842));
#193612=CARTESIAN_POINT('Ctrl Pts',(-42.0812997491636,46.6752630175686,
40.0983275959622));
#193613=CARTESIAN_POINT('Ctrl Pts',(-42.0846683595043,46.6710672367555,
40.0975235624069));
#193614=CARTESIAN_POINT('Ctrl Pts',(-42.0878044626433,46.6667352666015,
40.0964777059491));
#193615=CARTESIAN_POINT('Ctrl Pts',(-42.0907067742414,46.6623093164292,
40.0952149915961));
#193616=CARTESIAN_POINT('Ctrl Pts',(-42.0946678472188,46.6562687825187,
40.0934916398701));
#193617=CARTESIAN_POINT('Ctrl Pts',(-42.0981877352862,46.6500510792884,
40.0913643921631));
#193618=CARTESIAN_POINT('Ctrl Pts',(-42.1012583942262,46.6437515300391,
40.0889118607713));
#193619=CARTESIAN_POINT('Ctrl Pts',(-42.1027937236962,46.6406017554144,
40.0876855950755));
#193620=CARTESIAN_POINT('Ctrl Pts',(-42.1042169023586,46.6374313809741,
40.0863782327527));
#193621=CARTESIAN_POINT('Ctrl Pts',(-42.1055280393686,46.634251329385,40.0850006373334));
#193622=CARTESIAN_POINT('Ctrl Pts',(-42.1061836078736,46.6326613035905,
40.0843118396238));
#193623=CARTESIAN_POINT('Ctrl Pts',(-42.1068111789404,46.6310688468943,
40.0836054919165));
#193624=CARTESIAN_POINT('Ctrl Pts',(-42.1074108478351,46.6294752517397,
40.0828829920418));
#193625=CARTESIAN_POINT('Ctrl Pts',(-42.1075607650587,46.6290768529511,
40.0827023670731));
#193626=CARTESIAN_POINT('Ctrl Pts',(-42.1077089386738,46.6286783827621,
40.0825207326933));
#193627=CARTESIAN_POINT('Ctrl Pts',(-42.1078553707279,46.6282798608702,
40.0823381109276));
#193628=CARTESIAN_POINT('Ctrl Pts',(-42.1082946668904,46.6270842951945,
40.0817902456304));
#193629=CARTESIAN_POINT('Ctrl Pts',(-42.1087182876161,46.6258882654174,
40.0812334935554));
#193630=CARTESIAN_POINT('Ctrl Pts',(-42.1091263005957,46.6246922924069,
40.0806684524227));
#193631=CARTESIAN_POINT('Ctrl Pts',(-42.1119459234382,46.6164273768569,
40.0767636676138));
#193632=CARTESIAN_POINT('Ctrl Pts',(-42.1140735600935,46.608149216569,40.072440451089));
#193633=CARTESIAN_POINT('Ctrl Pts',(-42.1155964444645,46.599938443282,40.0677949937411));
#193634=CARTESIAN_POINT('Ctrl Pts',(-42.1163533138167,46.5958577114964,
40.0654862141907));
#193635=CARTESIAN_POINT('Ctrl Pts',(-42.116960421753,46.5917931497417,40.0630972003216));
#193636=CARTESIAN_POINT('Ctrl Pts',(-42.1174262136788,46.5877524553608,
40.0606363359906));
#193637=CARTESIAN_POINT('Ctrl Pts',(-42.1184538202397,46.5788380800231,
40.0552073017124));
#193638=CARTESIAN_POINT('Ctrl Pts',(-42.1188058546734,46.5700422469561,
40.0494204304519));
#193639=CARTESIAN_POINT('Ctrl Pts',(-42.118533783465,46.5615008914347,40.0434049749851));
#193640=CARTESIAN_POINT('Ctrl Pts',(-42.1184343924215,46.5583806265505,
40.0412074532442));
#193641=CARTESIAN_POINT('Ctrl Pts',(-42.118258896386,46.5552908961831,40.0389814735788));
#193642=CARTESIAN_POINT('Ctrl Pts',(-42.1180117795239,46.5522345526331,
40.0367321210016));
#193643=CARTESIAN_POINT('Ctrl Pts',(-42.1171817401332,46.5419686180606,
40.029176783714));
#193644=CARTESIAN_POINT('Ctrl Pts',(-42.1155299964531,46.5320149571607,
40.0213235332574));
#193645=CARTESIAN_POINT('Ctrl Pts',(-42.1131831104084,46.5223946380446,
40.0132649215855));
#193646=CARTESIAN_POINT('Ctrl Pts',(-42.1106036046384,46.5118207677343,
40.0044075527528));
#193647=CARTESIAN_POINT('Ctrl Pts',(-42.1071843209734,46.5016489045629,
39.9953016253713));
#193648=CARTESIAN_POINT('Ctrl Pts',(-42.1030402839734,46.491904474566,39.986035342235));
#193649=CARTESIAN_POINT('Ctrl Pts',(-42.0985769785664,46.4814093059437,
39.9760551582686));
#193650=CARTESIAN_POINT('Ctrl Pts',(-42.0932726122941,46.4714088200593,
39.9658879738145));
#193651=CARTESIAN_POINT('Ctrl Pts',(-42.0872150940878,46.4619468343633,
39.9556174643243));
#193652=CARTESIAN_POINT('Ctrl Pts',(-42.0812393728301,46.4526126174219,
39.9454856413897));
#193653=CARTESIAN_POINT('Ctrl Pts',(-42.0745296860254,46.4438014421037,
39.9352519465109));
#193654=CARTESIAN_POINT('Ctrl Pts',(-42.0671296588092,46.4355828792674,
39.92499));
#193655=CARTESIAN_POINT('Ctrl Pts',(-39.7651933658995,43.8790236240223,
39.92499));
#193656=CARTESIAN_POINT('Ctrl Pts',(-39.7581114992309,43.8711584142718,
39.9348107241729));
#193657=CARTESIAN_POINT('Ctrl Pts',(-39.7504347382243,43.8638800583564,
39.9446038383182));
#193658=CARTESIAN_POINT('Ctrl Pts',(-39.7422106539896,43.8572218328526,
39.9543158069403));
#193659=CARTESIAN_POINT('Ctrl Pts',(-39.7342695770743,43.8507927303124,
39.9636935671414));
#193660=CARTESIAN_POINT('Ctrl Pts',(-39.7258171668678,43.8449410790332,
39.9729968321016));
#193661=CARTESIAN_POINT('Ctrl Pts',(-39.7168657021529,43.8397310304442,
39.9821731151366));
#193662=CARTESIAN_POINT('Ctrl Pts',(-39.7084037645721,43.8348059028415,
39.9908475764386));
#193663=CARTESIAN_POINT('Ctrl Pts',(-39.6994950821762,43.8304536682197,
39.9994093733883));
#193664=CARTESIAN_POINT('Ctrl Pts',(-39.6901349804701,43.8267676847803,
40.0077966115881));
#193665=CARTESIAN_POINT('Ctrl Pts',(-39.6815144838262,43.8233729558697,
40.0155211172637));
#193666=CARTESIAN_POINT('Ctrl Pts',(-39.6725105620382,43.8205432023691,
40.0230979941066));
#193667=CARTESIAN_POINT('Ctrl Pts',(-39.6631152739582,43.8183892419676,
40.0304554104794));
#193668=CARTESIAN_POINT('Ctrl Pts',(-39.660313788711,43.8177469744568,40.0326492435211));
#193669=CARTESIAN_POINT('Ctrl Pts',(-39.6574775031699,43.8171650742228,
40.0348233715075));
#193670=CARTESIAN_POINT('Ctrl Pts',(-39.6546062260517,43.8166472411073,
40.0369753512356));
#193671=CARTESIAN_POINT('Ctrl Pts',(-39.6517642863083,43.8161346989699,
40.0391053430352));
#193672=CARTESIAN_POINT('Ctrl Pts',(-39.6488910639686,43.8156851836085,
40.041211089324));
#193673=CARTESIAN_POINT('Ctrl Pts',(-39.64598968505,43.8153025584995,40.0432881154904));
#193674=CARTESIAN_POINT('Ctrl Pts',(-39.6457879288342,43.8152759514977,
40.043432547828));
#193675=CARTESIAN_POINT('Ctrl Pts',(-39.6455860324533,43.8152496566738,
40.0435768364421));
#193676=CARTESIAN_POINT('Ctrl Pts',(-39.6453839959662,43.8152236753309,
40.0437209807855));
#193677=CARTESIAN_POINT('Ctrl Pts',(-39.6365259762552,43.8140845580785,
40.050040796842));
#193678=CARTESIAN_POINT('Ctrl Pts',(-39.6274037177901,43.8135929685793,
40.0560490279344));
#193679=CARTESIAN_POINT('Ctrl Pts',(-39.6180980992373,43.8138323099901,
40.0616647108614));
#193680=CARTESIAN_POINT('Ctrl Pts',(-39.6094236454406,43.8140554177823,
40.0668995033484));
#193681=CARTESIAN_POINT('Ctrl Pts',(-39.6005890951403,43.8149139527619,
40.0717933267479));
#193682=CARTESIAN_POINT('Ctrl Pts',(-39.5916773623197,43.8164991115145,
40.0762460303069));
#193683=CARTESIAN_POINT('Ctrl Pts',(-39.5884173351605,43.8170789830938,
40.0778748868746));
#193684=CARTESIAN_POINT('Ctrl Pts',(-39.5851472105417,43.8177563121468,
40.0794443522247));
#193685=CARTESIAN_POINT('Ctrl Pts',(-39.5818719865441,43.818536340063,40.0809482021492));
#193686=CARTESIAN_POINT('Ctrl Pts',(-39.5810844045883,43.8187239107184,
40.0813098278169));
#193687=CARTESIAN_POINT('Ctrl Pts',(-39.5802961412317,43.8189178575374,
40.0816679525672));
#193688=CARTESIAN_POINT('Ctrl Pts',(-39.5795073285704,43.8191182115053,
40.0820224192581));
#193689=CARTESIAN_POINT('Ctrl Pts',(-39.5787431663048,43.8193123044118,
40.0823658088648));
#193690=CARTESIAN_POINT('Ctrl Pts',(-39.5779784885477,43.8195124102602,
40.0827057654617));
#193691=CARTESIAN_POINT('Ctrl Pts',(-39.5772134181961,43.8197185546681,
40.0830421470151));
#193692=CARTESIAN_POINT('Ctrl Pts',(-39.568831188323,43.8219771048933,40.0867275956806));
#193693=CARTESIAN_POINT('Ctrl Pts',(-39.5603964284872,43.8249623840156,
40.089982343203));
#193694=CARTESIAN_POINT('Ctrl Pts',(-39.5520968239719,43.8286919494554,
40.0926299529355));
#193695=CARTESIAN_POINT('Ctrl Pts',(-39.5486547305945,43.8302387114099,
40.0937279956084));
#193696=CARTESIAN_POINT('Ctrl Pts',(-39.5452359574127,43.8319130705228,
40.0947220371802));
#193697=CARTESIAN_POINT('Ctrl Pts',(-39.5418537500313,43.8337144555753,
40.0956014538693));
#193698=CARTESIAN_POINT('Ctrl Pts',(-39.5360850428915,43.8367869054998,
40.097101390674));
#193699=CARTESIAN_POINT('Ctrl Pts',(-39.5304250803196,43.8402296473866,
40.0982667904316));
#193700=CARTESIAN_POINT('Ctrl Pts',(-39.5249464846901,43.8440378929943,
40.0990539325583));
#193701=CARTESIAN_POINT('Ctrl Pts',(-39.5222071868753,43.8459420157981,
40.0994475036216));
#193702=CARTESIAN_POINT('Ctrl Pts',(-39.5195141476131,43.8479386338069,
40.0997467259952));
#193703=CARTESIAN_POINT('Ctrl Pts',(-39.5168765098747,43.8500271570783,
40.0999473488896));
#193704=CARTESIAN_POINT('Ctrl Pts',(-39.5142388721362,43.8521156803497,
40.100147971784));
#193705=CARTESIAN_POINT('Ctrl Pts',(-39.5116566557594,43.8542960677577,
40.10025));
#193706=CARTESIAN_POINT('Ctrl Pts',(-39.5091373124618,43.856566526706,40.10025));
#193707=CARTESIAN_POINT('Origin',(-34.2342565846632,47.1453396605411,39.92499));
#193708=CARTESIAN_POINT('Ctrl Pts',(-36.6746059268174,50.8023624960594,
39.92499));
#193709=CARTESIAN_POINT('Ctrl Pts',(-36.6808425220335,50.8109464329603,
39.9348354642022));
#193710=CARTESIAN_POINT('Ctrl Pts',(-36.6877379133667,50.819012811669,39.9446440828465));
#193711=CARTESIAN_POINT('Ctrl Pts',(-36.6952462569244,50.8265243508963,
39.9543641760341));
#193712=CARTESIAN_POINT('Ctrl Pts',(-36.7025106240257,50.8337918098269,
39.9637684240725));
#193713=CARTESIAN_POINT('Ctrl Pts',(-36.7103497152254,50.8405407635287,
39.973090963641));
#193714=CARTESIAN_POINT('Ctrl Pts',(-36.7187568768225,50.8467071440079,
39.9822808977156));
#193715=CARTESIAN_POINT('Ctrl Pts',(-36.7267095340102,50.8525401602375,
39.9909740094666));
#193716=CARTESIAN_POINT('Ctrl Pts',(-36.7351712462837,50.8578524412756,
39.9995492765018));
#193717=CARTESIAN_POINT('Ctrl Pts',(-36.7441560526543,50.8625525281344,
40.0079462328713));
#193718=CARTESIAN_POINT('Ctrl Pts',(-36.7524317091193,50.8668816480503,
40.0156804369708));
#193719=CARTESIAN_POINT('Ctrl Pts',(-36.7611516658486,50.8706916079202,
40.0232638017442));
#193720=CARTESIAN_POINT('Ctrl Pts',(-36.7703354510189,50.8738736606214,
40.0306257269987));
#193721=CARTESIAN_POINT('Ctrl Pts',(-36.772999317994,50.8747966531508,40.0327611416665));
#193722=CARTESIAN_POINT('Ctrl Pts',(-36.7757022424581,50.8756665488987,
40.0348777427278));
#193723=CARTESIAN_POINT('Ctrl Pts',(-36.7784447603815,50.8764799968256,
40.0369733168701));
#193724=CARTESIAN_POINT('Ctrl Pts',(-36.7814178261389,50.8773618266785,
40.039245053974));
#193725=CARTESIAN_POINT('Ctrl Pts',(-36.7844329791243,50.8781771258726,
40.041487875195));
#193726=CARTESIAN_POINT('Ctrl Pts',(-36.7874899206171,50.8789219044956,
40.0436985701601));
#193727=CARTESIAN_POINT('Ctrl Pts',(-36.7958797205313,50.8809659552706,
40.0497658398386));
#193728=CARTESIAN_POINT('Ctrl Pts',(-36.80458376171,50.8824343655146,40.0555581699984));
#193729=CARTESIAN_POINT('Ctrl Pts',(-36.8135226609474,50.8832604021664,
40.0609828468886));
#193730=CARTESIAN_POINT('Ctrl Pts',(-36.8217012684457,50.8840161808563,
40.0659461317305));
#193731=CARTESIAN_POINT('Ctrl Pts',(-36.8300699399857,50.8842246658557,
40.0706039980708));
#193732=CARTESIAN_POINT('Ctrl Pts',(-36.8385876480149,50.8838072802931,
40.0748843180605));
#193733=CARTESIAN_POINT('Ctrl Pts',(-36.8427715183744,50.8836022618681,
40.0769867972571));
#193734=CARTESIAN_POINT('Ctrl Pts',(-36.8469911418446,50.8832457706972,
40.0789976708176));
#193735=CARTESIAN_POINT('Ctrl Pts',(-36.8512399286213,50.8827256259728,
40.08090504915));
#193736=CARTESIAN_POINT('Ctrl Pts',(-36.8520460945285,50.8826269335776,
40.0812669556105));
#193737=CARTESIAN_POINT('Ctrl Pts',(-36.8528536453862,50.8825219362262,
40.0816253922033));
#193738=CARTESIAN_POINT('Ctrl Pts',(-36.8536624499709,50.8824105850809,
40.0819801989139));
#193739=CARTESIAN_POINT('Ctrl Pts',(-36.8544459794124,50.882302713659,40.0823239179149));
#193740=CARTESIAN_POINT('Ctrl Pts',(-36.8552306854274,50.882188879366,40.0826642303499));
#193741=CARTESIAN_POINT('Ctrl Pts',(-36.8560164456182,50.8820690400778,
40.08300099161));
#193742=CARTESIAN_POINT('Ctrl Pts',(-36.8645794982669,50.8807630562083,
40.0866709464311));
#193743=CARTESIAN_POINT('Ctrl Pts',(-36.8732733195863,50.8787426510002,
40.0899175831875));
#193744=CARTESIAN_POINT('Ctrl Pts',(-36.8819119966095,50.8759664620674,
40.0925642067059));
#193745=CARTESIAN_POINT('Ctrl Pts',(-36.8855601635605,50.8747940602416,
40.0936818922526));
#193746=CARTESIAN_POINT('Ctrl Pts',(-36.8891983713641,50.8734872887381,
40.094693009479));
#193747=CARTESIAN_POINT('Ctrl Pts',(-36.8928125648613,50.8720449698707,
40.0955863397546));
#193748=CARTESIAN_POINT('Ctrl Pts',(-36.8988987764012,50.8696161409377,
40.0970906856166));
#193749=CARTESIAN_POINT('Ctrl Pts',(-36.9049145742144,50.8668019052539,
40.0982599215483));
#193750=CARTESIAN_POINT('Ctrl Pts',(-36.9107858666115,50.8635979627953,
40.0990497370454));
#193751=CARTESIAN_POINT('Ctrl Pts',(-36.9122536897107,50.8627969771806,
40.0992471909196));
#193752=CARTESIAN_POINT('Ctrl Pts',(-36.9137123559377,50.861971437292,40.0994209989363));
#193753=CARTESIAN_POINT('Ctrl Pts',(-36.9151605322316,50.861121022166,40.0995705982975));
#193754=CARTESIAN_POINT('Ctrl Pts',(-36.9173327966724,50.8598453994769,
40.0997949973393));
#193755=CARTESIAN_POINT('Ctrl Pts',(-36.9194814382212,50.8585138058059,
40.0999649129781));
#193756=CARTESIAN_POINT('Ctrl Pts',(-36.9216029292226,50.8571265262611,
40.1000786629733));
#193757=CARTESIAN_POINT('Ctrl Pts',(-36.923724420224,50.8557392467162,40.1001924129685));
#193758=CARTESIAN_POINT('Ctrl Pts',(-36.9258187603126,50.8542962928973,
40.10025));
#193759=CARTESIAN_POINT('Ctrl Pts',(-36.9278827595322,50.8527980281388,
40.10025));
#193760=CARTESIAN_POINT('Ctrl Pts',(-34.6837837831342,47.7640607692766,
40.10025));
#193761=CARTESIAN_POINT('Ctrl Pts',(-34.6767997090225,47.7691302463545,
40.10025));
#193762=CARTESIAN_POINT('Ctrl Pts',(-34.6702946353241,47.7747322888385,
40.0995786334241));
#193763=CARTESIAN_POINT('Ctrl Pts',(-34.6643211616152,47.7807252357995,
40.0983063763365));
#193764=CARTESIAN_POINT('Ctrl Pts',(-34.6604629105133,47.7845960646243,
40.0974846287992));
#193765=CARTESIAN_POINT('Ctrl Pts',(-34.6568257642789,47.7886293194339,
40.0964130309337));
#193766=CARTESIAN_POINT('Ctrl Pts',(-34.6534164822759,47.7927819897612,
40.0951176960923));
#193767=CARTESIAN_POINT('Ctrl Pts',(-34.6488976742765,47.7982861164005,
40.0934008039614));
#193768=CARTESIAN_POINT('Ctrl Pts',(-34.6447843113771,47.8040027249066,
40.0912909372156));
#193769=CARTESIAN_POINT('Ctrl Pts',(-34.6410949611629,47.8098436832081,
40.0888630467851));
#193770=CARTESIAN_POINT('Ctrl Pts',(-34.6392502860559,47.8127641623588,
40.0876491015699));
#193771=CARTESIAN_POINT('Ctrl Pts',(-34.6375114518663,47.8157158446829,
40.0863558569271));
#193772=CARTESIAN_POINT('Ctrl Pts',(-34.635879631104,47.818688538764,40.0849936342771));
#193773=CARTESIAN_POINT('Ctrl Pts',(-34.6350637207229,47.8201748858045,
40.0843125229521));
#193774=CARTESIAN_POINT('Ctrl Pts',(-34.6342745503769,47.8216664954027,
40.0836141747074));
#193775=CARTESIAN_POINT('Ctrl Pts',(-34.6335121829165,47.8231621539168,
40.0828999161609));
#193776=CARTESIAN_POINT('Ctrl Pts',(-34.6333215910514,47.8235360685453,
40.0827213515243));
#193777=CARTESIAN_POINT('Ctrl Pts',(-34.6331326740828,47.8239102364349,
40.0825417925842));
#193778=CARTESIAN_POINT('Ctrl Pts',(-34.6329454324196,47.8242846390328,
40.0823612602361));
#193779=CARTESIAN_POINT('Ctrl Pts',(-34.6323837074303,47.8254078468266,
40.0818196631917));
#193780=CARTESIAN_POINT('Ctrl Pts',(-34.6318370616126,47.8265331659853,
40.0812693052022));
#193781=CARTESIAN_POINT('Ctrl Pts',(-34.6313054933181,47.8276601046328,
40.0807107531875));
#193782=CARTESIAN_POINT('Ctrl Pts',(-34.6275611948899,47.8355981149519,
40.0767763849181));
#193783=CARTESIAN_POINT('Ctrl Pts',(-34.6245119115562,47.8436253243405,
40.0724140586135));
#193784=CARTESIAN_POINT('Ctrl Pts',(-34.6220808005805,47.8516500154458,
40.0677221223765));
#193785=CARTESIAN_POINT('Ctrl Pts',(-34.6209017143844,47.8555419819601,
40.0654465383718));
#193786=CARTESIAN_POINT('Ctrl Pts',(-34.6198683413509,47.8594338479546,
40.0630928000678));
#193787=CARTESIAN_POINT('Ctrl Pts',(-34.6189736992136,47.8633173872851,
40.0606689262479));
#193788=CARTESIAN_POINT('Ctrl Pts',(-34.6176040646081,47.8692628146654,
40.0569581447806));
#193789=CARTESIAN_POINT('Ctrl Pts',(-34.6165592825243,47.8751852090116,
40.0530843804606));
#193790=CARTESIAN_POINT('Ctrl Pts',(-34.6158190596249,47.8810431641658,
40.0490800251458));
#193791=CARTESIAN_POINT('Ctrl Pts',(-34.6154752962811,47.8837636288445,
40.0472203818218));
#193792=CARTESIAN_POINT('Ctrl Pts',(-34.6151969889845,47.8864700832049,
40.0453323608819));
#193793=CARTESIAN_POINT('Ctrl Pts',(-34.6149833323959,47.8891582656054,
40.0434201572162));
#193794=CARTESIAN_POINT('Ctrl Pts',(-34.6149669564602,47.8893643041944,
40.0432735943397));
#193795=CARTESIAN_POINT('Ctrl Pts',(-34.6149509280614,47.8895702459313,
40.0431268995707));
#193796=CARTESIAN_POINT('Ctrl Pts',(-34.6149352461542,47.8897760897958,
40.0429800745037));
#193797=CARTESIAN_POINT('Ctrl Pts',(-34.6147149626374,47.8926675754935,
40.0409176249753));
#193798=CARTESIAN_POINT('Ctrl Pts',(-34.6145651177081,47.8955400426777,
40.0388310783332));
#193799=CARTESIAN_POINT('Ctrl Pts',(-34.6144819591399,47.8983891927626,
40.036725739981));
#193800=CARTESIAN_POINT('Ctrl Pts',(-34.6141837673037,47.908605738263,40.0291763710716));
#193801=CARTESIAN_POINT('Ctrl Pts',(-34.6147387685077,47.9186013937342,
40.0213310894592));
#193802=CARTESIAN_POINT('Ctrl Pts',(-34.6160223355359,47.9283423801894,
40.0132837551316));
#193803=CARTESIAN_POINT('Ctrl Pts',(-34.6174328467541,47.9390467457347,
40.0044405431319));
#193804=CARTESIAN_POINT('Ctrl Pts',(-34.6197230854584,47.9494442419762,
39.9953528710594));
#193805=CARTESIAN_POINT('Ctrl Pts',(-34.6227799581217,47.9594984812856,
39.9861103629547));
#193806=CARTESIAN_POINT('Ctrl Pts',(-34.6260806134277,47.97035453647,39.9761307737546));
#193807=CARTESIAN_POINT('Ctrl Pts',(-34.6302752334102,47.9808115517384,
39.9659696935999));
#193808=CARTESIAN_POINT('Ctrl Pts',(-34.6352786409545,47.9908184179967,
39.9557128217491));
#193809=CARTESIAN_POINT('Ctrl Pts',(-34.6402400750502,48.0007413369283,
39.9455419945151));
#193810=CARTESIAN_POINT('Ctrl Pts',(-34.6459976651007,48.010222760914,39.9352756289336));
#193811=CARTESIAN_POINT('Ctrl Pts',(-34.6525130919793,48.0191904766739,
39.92499));
#193812=CARTESIAN_POINT('Origin',(-0.0123294189942654,-0.00895784724494174,
39.92499));
#193813=CARTESIAN_POINT('Ctrl Pts',(-36.9525415975208,50.8348823336489,
40.10025));
#193814=CARTESIAN_POINT('Ctrl Pts',(-36.9594880792485,50.829830979246,40.10025));
#193815=CARTESIAN_POINT('Ctrl Pts',(-36.9659508653433,50.824244238888,40.0995859581841));
#193816=CARTESIAN_POINT('Ctrl Pts',(-36.97188047026,50.8182646381292,40.0983275959619));
#193817=CARTESIAN_POINT('Ctrl Pts',(-36.9756692055208,50.8144439579052,
40.0975235624067));
#193818=CARTESIAN_POINT('Ctrl Pts',(-36.9792409429413,50.8104635307792,
40.0964777059489));
#193819=CARTESIAN_POINT('Ctrl Pts',(-36.9825899931423,50.8063652005969,
40.0952149915961));
#193820=CARTESIAN_POINT('Ctrl Pts',(-36.9871607746745,50.8007718022344,
40.0934916398701));
#193821=CARTESIAN_POINT('Ctrl Pts',(-36.9913113073905,50.7949560887235,
40.0913643921631));
#193822=CARTESIAN_POINT('Ctrl Pts',(-36.9950236271419,50.7890120203242,
40.0889118607713));
#193823=CARTESIAN_POINT('Ctrl Pts',(-36.9968797870176,50.7860399861246,
40.0876855950754));
#193824=CARTESIAN_POINT('Ctrl Pts',(-36.9986265637266,50.7830357420058,
40.0863782327526));
#193825=CARTESIAN_POINT('Ctrl Pts',(-37.0002629240967,50.7800101622088,
40.0850006373334));
#193826=CARTESIAN_POINT('Ctrl Pts',(-37.0010811042817,50.7784973723103,
40.0843118396237));
#193827=CARTESIAN_POINT('Ctrl Pts',(-37.0018716944997,50.7769792382977,
40.0836054919164));
#193828=CARTESIAN_POINT('Ctrl Pts',(-37.002634654398,50.7754570554922,40.0828829920417));
#193829=CARTESIAN_POINT('Ctrl Pts',(-37.0028253943726,50.7750765097908,
40.0827023670731));
#193830=CARTESIAN_POINT('Ctrl Pts',(-37.0030144077536,50.7746957108235,
40.0825207326932));
#193831=CARTESIAN_POINT('Ctrl Pts',(-37.0032016945186,50.7743146783938,
40.0823381109275));
#193832=CARTESIAN_POINT('Ctrl Pts',(-37.0037635548135,50.7731715811047,
40.0817902456303));
#193833=CARTESIAN_POINT('Ctrl Pts',(-37.0043098740552,50.7720263837273,
40.0812334935553));
#193834=CARTESIAN_POINT('Ctrl Pts',(-37.0048406651179,50.7708796113519,
40.0806684524227));
#193835=CARTESIAN_POINT('Ctrl Pts',(-37.0085087606929,50.7629547027167,
40.0767636676137));
#193836=CARTESIAN_POINT('Ctrl Pts',(-37.0114900453056,50.7549442896469,
40.0724404510888));
#193837=CARTESIAN_POINT('Ctrl Pts',(-37.0138628466707,50.7469376805981,
40.067794993741));
#193838=CARTESIAN_POINT('Ctrl Pts',(-37.0150421224359,50.7429584178785,
40.0654862141906));
#193839=CARTESIAN_POINT('Ctrl Pts',(-37.0160707669654,50.738979582278,40.0630972003216));
#193840=CARTESIAN_POINT('Ctrl Pts',(-37.0169563748085,50.735009711758,40.0606363359906));
#193841=CARTESIAN_POINT('Ctrl Pts',(-37.0189101579882,50.7262515844358,
40.0552073017123));
#193842=CARTESIAN_POINT('Ctrl Pts',(-37.0201796788542,50.7175407334811,
40.0494204304519));
#193843=CARTESIAN_POINT('Ctrl Pts',(-37.0208019128471,50.7090177292135,
40.0434049749852));
#193844=CARTESIAN_POINT('Ctrl Pts',(-37.0210292227715,50.7059041682738,
40.0412074532443));
#193845=CARTESIAN_POINT('Ctrl Pts',(-37.0211776528887,50.7028130194417,
40.0389814735788));
#193846=CARTESIAN_POINT('Ctrl Pts',(-37.0212513646531,50.6997475881155,
40.0367321210017));
#193847=CARTESIAN_POINT('Ctrl Pts',(-37.0214989546698,50.6894511286642,
40.0291767837136));
#193848=CARTESIAN_POINT('Ctrl Pts',(-37.0208967002921,50.6793793407311,
40.0213235332566));
#193849=CARTESIAN_POINT('Ctrl Pts',(-37.0195682679079,50.6695664063375,
40.0132649215843));
#193850=CARTESIAN_POINT('Ctrl Pts',(-37.0181081633546,50.6587808290205,
40.0044075527512));
#193851=CARTESIAN_POINT('Ctrl Pts',(-37.015770860109,50.6483072759125,39.9953016253693));
#193852=CARTESIAN_POINT('Ctrl Pts',(-37.01266809487,50.638183057103,39.9860353422325));
#193853=CARTESIAN_POINT('Ctrl Pts',(-37.0093262837647,50.6272788396571,
39.9760551582657));
#193854=CARTESIAN_POINT('Ctrl Pts',(-37.005096310787,50.6167786802254,39.9658879738112));
#193855=CARTESIAN_POINT('Ctrl Pts',(-37.0000610231232,50.6067353452076,
39.9556174643206));
#193856=CARTESIAN_POINT('Ctrl Pts',(-36.9950937288449,50.5968276291246,
39.9454856413871));
#193857=CARTESIAN_POINT('Ctrl Pts',(-36.9893418170227,50.5873633690972,
39.9352519465096));
#193858=CARTESIAN_POINT('Ctrl Pts',(-36.9828414016742,50.578416314936,39.92499));
#193859=CARTESIAN_POINT('Ctrl Pts',(-34.9607485668361,47.7952442955505,
39.92499));
#193860=CARTESIAN_POINT('Ctrl Pts',(-34.9545276336625,47.7866819156019,
39.934810724173));
#193861=CARTESIAN_POINT('Ctrl Pts',(-34.9476537221149,47.7786409912507,
39.9446038383184));
#193862=CARTESIAN_POINT('Ctrl Pts',(-34.940170664354,47.7711595893161,39.9543158069406));
#193863=CARTESIAN_POINT('Ctrl Pts',(-34.9329451136977,47.7639356375057,
39.9636935671417));
#193864=CARTESIAN_POINT('Ctrl Pts',(-34.9251506707945,47.7572325247346,
39.9729968321018));
#193865=CARTESIAN_POINT('Ctrl Pts',(-34.9167928415125,47.7511153344864,
39.9821731151368));
#193866=CARTESIAN_POINT('Ctrl Pts',(-34.908892075331,47.7453326739166,39.9908475764386));
#193867=CARTESIAN_POINT('Ctrl Pts',(-34.9004871280263,47.7400730704109,
39.9994093733882));
#193868=CARTESIAN_POINT('Ctrl Pts',(-34.8915635921215,47.7354288821272,
40.0077966115878));
#193869=CARTESIAN_POINT('Ctrl Pts',(-34.8833451652567,47.73115166263,40.0155211172631));
#193870=CARTESIAN_POINT('Ctrl Pts',(-34.8746863576795,47.7273962447075,
40.0230979941058));
#193871=CARTESIAN_POINT('Ctrl Pts',(-34.8655676881418,47.7242720089015,
40.0304554104784));
#193872=CARTESIAN_POINT('Ctrl Pts',(-34.8628486849594,47.7233404248514,
40.0326492435204));
#193873=CARTESIAN_POINT('Ctrl Pts',(-34.860088762024,47.7224652397586,40.0348233715072));
#193874=CARTESIAN_POINT('Ctrl Pts',(-34.8572873423617,47.7216501132022,
40.0369753512356));
#193875=CARTESIAN_POINT('Ctrl Pts',(-34.8545145463035,47.7208433152301,
40.0391053430352));
#193876=CARTESIAN_POINT('Ctrl Pts',(-34.8517040509264,47.7200959288451,
40.041211089324));
#193877=CARTESIAN_POINT('Ctrl Pts',(-34.8488585612797,47.7194121231168,
40.0432881154904));
#193878=CARTESIAN_POINT('Ctrl Pts',(-34.8486606914946,47.7193645726038,
40.043432547828));
#193879=CARTESIAN_POINT('Ctrl Pts',(-34.8484626496807,47.7193173179073,
40.0435768364421));
#193880=CARTESIAN_POINT('Ctrl Pts',(-34.8482644357605,47.7192703603293,
40.0437209807855));
#193881=CARTESIAN_POINT('Ctrl Pts',(-34.8395740113842,47.7172115680925,
40.050040796842));
#193882=CARTESIAN_POINT('Ctrl Pts',(-34.8305531107003,47.715769135913,40.0560490279343));
#193883=CARTESIAN_POINT('Ctrl Pts',(-34.8212734513098,47.7150344641795,
40.0616647108613));
#193884=CARTESIAN_POINT('Ctrl Pts',(-34.8126231959637,47.7143496224388,
40.0668995033484));
#193885=CARTESIAN_POINT('Ctrl Pts',(-34.8037473009119,47.7142799923074,
40.0717933267481));
#193886=CARTESIAN_POINT('Ctrl Pts',(-34.7947186932874,47.7149249376578,
40.0762460303072));
#193887=CARTESIAN_POINT('Ctrl Pts',(-34.7914159118133,47.7151608670107,
40.0778748868748));
#193888=CARTESIAN_POINT('Ctrl Pts',(-34.7880929011146,47.7154926644832,
40.0794443522247));
#193889=CARTESIAN_POINT('Ctrl Pts',(-34.7847540840176,47.7159260651935,
40.0809482021491));
#193890=CARTESIAN_POINT('Ctrl Pts',(-34.7839512100458,47.7160302835857,
40.0813098278168));
#193891=CARTESIAN_POINT('Ctrl Pts',(-34.7831469919154,47.7161407719864,
40.0816679525672));
#193892=CARTESIAN_POINT('Ctrl Pts',(-34.78234155776,47.716257575019,40.082022419258));
#193893=CARTESIAN_POINT('Ctrl Pts',(-34.781561293422,47.7163707279569,40.0823658088648));
#193894=CARTESIAN_POINT('Ctrl Pts',(-34.7807798878928,47.7164898070137,
40.0827057654616));
#193895=CARTESIAN_POINT('Ctrl Pts',(-34.7799974607185,47.7166148505129,
40.083042147015));
#193896=CARTESIAN_POINT('Ctrl Pts',(-34.7714250667933,47.7179848465562,
40.0867275956806));
#193897=CARTESIAN_POINT('Ctrl Pts',(-34.7627244668151,47.7200720995235,
40.0899823432031));
#193898=CARTESIAN_POINT('Ctrl Pts',(-34.7540804826574,47.722913689108,40.0926299529356));
#193899=CARTESIAN_POINT('Ctrl Pts',(-34.7504955647778,47.7240921810074,
40.0937279956084));
#193900=CARTESIAN_POINT('Ctrl Pts',(-34.7469205018084,47.7254000086989,
40.0947220371802));
#193901=CARTESIAN_POINT('Ctrl Pts',(-34.7433685265017,47.7268379886355,
40.0956014538692));
#193902=CARTESIAN_POINT('Ctrl Pts',(-34.7373102624742,47.7292906132654,
40.097101390674));
#193903=CARTESIAN_POINT('Ctrl Pts',(-34.7313214412506,47.7321228682622,
40.0982667904316));
#193904=CARTESIAN_POINT('Ctrl Pts',(-34.7254747878803,47.7353375827203,
40.0990539325582));
#193905=CARTESIAN_POINT('Ctrl Pts',(-34.7225514611951,47.7369449399494,
40.0994475036216));
#193906=CARTESIAN_POINT('Ctrl Pts',(-34.7196644712716,47.7386491210201,
40.0997467259952));
#193907=CARTESIAN_POINT('Ctrl Pts',(-34.7168229726605,47.7404504949229,
40.0999473488896));
#193908=CARTESIAN_POINT('Ctrl Pts',(-34.7139814740494,47.7422518688257,
40.100147971784));
#193909=CARTESIAN_POINT('Ctrl Pts',(-34.7111854907789,47.7441503967335,
40.10025));
#193910=CARTESIAN_POINT('Ctrl Pts',(-34.7084426211227,47.7461450747867,
40.10025));
#193911=CARTESIAN_POINT('Origin',(-29.1186878401551,50.4655267888878,39.92499));
#193912=CARTESIAN_POINT('Ctrl Pts',(-31.1634057161435,54.3576020372441,
39.92499));
#193913=CARTESIAN_POINT('Ctrl Pts',(-31.1687108809055,54.3667908521544,
39.9348354642014));
#193914=CARTESIAN_POINT('Ctrl Pts',(-31.1747253323927,54.3755338070562,
39.9446440828452));
#193915=CARTESIAN_POINT('Ctrl Pts',(-31.1814073748063,54.3837890328991,
39.9543641760323));
#193916=CARTESIAN_POINT('Ctrl Pts',(-31.1878722906305,54.3917760130589,
39.9637684240703));
#193917=CARTESIAN_POINT('Ctrl Pts',(-31.194962980709,54.3993074034425,39.9730909636386));
#193918=CARTESIAN_POINT('Ctrl Pts',(-31.2026795247194,54.4063187915262,
39.982280897713));
#193919=CARTESIAN_POINT('Ctrl Pts',(-31.2099789001959,54.4129511329171,
39.9909740094639));
#193920=CARTESIAN_POINT('Ctrl Pts',(-31.2178389737506,54.4191188025042,
39.999549276499));
#193921=CARTESIAN_POINT('Ctrl Pts',(-31.2262832675547,54.4247323097979,
40.0079462328684));
#193922=CARTESIAN_POINT('Ctrl Pts',(-31.2340610728553,54.4299027559947,
40.0156804369679));
#193923=CARTESIAN_POINT('Ctrl Pts',(-31.2423350114985,54.4346033281824,
40.0232638017412));
#193924=CARTESIAN_POINT('Ctrl Pts',(-31.2511358718535,54.4387279162168,
40.0306257269957));
#193925=CARTESIAN_POINT('Ctrl Pts',(-31.2536886668971,54.4399243024184,
40.0327611416645));
#193926=CARTESIAN_POINT('Ctrl Pts',(-31.2562858555935,54.4410719653274,
40.0348777427268));
#193927=CARTESIAN_POINT('Ctrl Pts',(-31.2589283212562,54.442167628286,40.03697331687));
#193928=CARTESIAN_POINT('Ctrl Pts',(-31.261792923929,54.4433553973775,40.039245053974));
#193929=CARTESIAN_POINT('Ctrl Pts',(-31.264706337619,54.4444813995855,40.041487875195));
#193930=CARTESIAN_POINT('Ctrl Pts',(-31.2676686823014,54.4455416356298,
40.0436985701601));
#193931=CARTESIAN_POINT('Ctrl Pts',(-31.2757988605275,54.4484514617729,
40.0497658398386));
#193932=CARTESIAN_POINT('Ctrl Pts',(-31.2843017293917,54.4508216479606,
40.0555581699984));
#193933=CARTESIAN_POINT('Ctrl Pts',(-31.293105316062,54.4525775288978,40.0609828468885));
#193934=CARTESIAN_POINT('Ctrl Pts',(-31.3011601199074,54.4541840646263,
40.0659461317304));
#193935=CARTESIAN_POINT('Ctrl Pts',(-31.3094611543724,54.4552661718987,
40.0706039980706));
#193936=CARTESIAN_POINT('Ctrl Pts',(-31.3179758301772,54.4557414157487,
40.0748843180603));
#193937=CARTESIAN_POINT('Ctrl Pts',(-31.3221582111181,54.4559748539754,
40.076986797257));
#193938=CARTESIAN_POINT('Ctrl Pts',(-31.3263919825238,54.4560613864573,
40.0789976708175));
#193939=CARTESIAN_POINT('Ctrl Pts',(-31.3306718639309,54.4559882102926,
40.08090504915));
#193940=CARTESIAN_POINT('Ctrl Pts',(-31.3314839297413,54.4559743258281,
40.0812669556105));
#193941=CARTESIAN_POINT('Ctrl Pts',(-31.3322980319626,54.4559543157133,
40.0816253922033));
#193942=CARTESIAN_POINT('Ctrl Pts',(-31.3331140451953,54.4559281176617,
40.0819801989139));
#193943=CARTESIAN_POINT('Ctrl Pts',(-31.3339045580145,54.4559027382991,
40.0823239179149));
#193944=CARTESIAN_POINT('Ctrl Pts',(-31.3346968642515,54.4558715517162,
40.0826642303498));
#193945=CARTESIAN_POINT('Ctrl Pts',(-31.3354908465824,54.4558345032253,
40.0830009916099));
#193946=CARTESIAN_POINT('Ctrl Pts',(-31.3441435024199,54.4554307564064,
40.0866709464312));
#193947=CARTESIAN_POINT('Ctrl Pts',(-31.3530008879283,54.4543301709717,
40.0899175831877));
#193948=CARTESIAN_POINT('Ctrl Pts',(-31.3618824321381,54.4524721779262,
40.0925642067061));
#193949=CARTESIAN_POINT('Ctrl Pts',(-31.3656331634097,54.4516875359255,
40.0936818922527));
#193950=CARTESIAN_POINT('Ctrl Pts',(-31.3693880355472,54.4507682193238,
40.094693009479));
#193951=CARTESIAN_POINT('Ctrl Pts',(-31.3731331934888,54.4497115877223,
40.0955863397546));
#193952=CARTESIAN_POINT('Ctrl Pts',(-31.3794399458809,54.4479322465077,
40.0970906856167));
#193953=CARTESIAN_POINT('Ctrl Pts',(-31.3857169562555,54.4457622496023,
40.0982599215483));
#193954=CARTESIAN_POINT('Ctrl Pts',(-31.3918909882804,54.4431895758479,
40.0990497370454));
#193955=CARTESIAN_POINT('Ctrl Pts',(-31.3934344962867,54.4425464074094,
40.0992471909196));
#193956=CARTESIAN_POINT('Ctrl Pts',(-31.3949714642034,54.4418778620537,
40.0994209989363));
#193957=CARTESIAN_POINT('Ctrl Pts',(-31.3965005998222,54.4411834812332,
40.0995705982975));
#193958=CARTESIAN_POINT('Ctrl Pts',(-31.3987943032505,54.4401419100025,
40.0997949973393));
#193959=CARTESIAN_POINT('Ctrl Pts',(-31.4010703637561,54.43904220514,40.0999649129781));
#193960=CARTESIAN_POINT('Ctrl Pts',(-31.4033252432067,54.4378842814518,
40.1000786629733));
#193961=CARTESIAN_POINT('Ctrl Pts',(-31.4055801226574,54.4367263577635,
40.1001924129685));
#193962=CARTESIAN_POINT('Ctrl Pts',(-31.4078138194769,54.4355102267474,
40.10025));
#193963=CARTESIAN_POINT('Ctrl Pts',(-31.4100231232056,54.4342359163066,
40.10025));
#193964=CARTESIAN_POINT('Ctrl Pts',(-29.5010785149107,51.127846865905,40.10025));
#193965=CARTESIAN_POINT('Ctrl Pts',(-29.4936027956391,51.1321585373228,
40.10025));
#193966=CARTESIAN_POINT('Ctrl Pts',(-29.486547784523,51.1370499258748,40.099578633424));
#193967=CARTESIAN_POINT('Ctrl Pts',(-29.4799806005917,51.1423856448183,
40.0983063763365));
#193968=CARTESIAN_POINT('Ctrl Pts',(-29.4757388736045,51.145831971779,40.0974846287991));
#193969=CARTESIAN_POINT('Ctrl Pts',(-29.4717000621107,51.1494629466902,
40.0964130309337));
#193970=CARTESIAN_POINT('Ctrl Pts',(-29.4678753842635,51.1532365012462,
40.0951176960923));
#193971=CARTESIAN_POINT('Ctrl Pts',(-29.4628059928679,51.158238131648,40.0934008039614));
#193972=CARTESIAN_POINT('Ctrl Pts',(-29.4581176150985,51.1634934604718,
40.0912909372156));
#193973=CARTESIAN_POINT('Ctrl Pts',(-29.4538379291356,51.1689167792842,
40.0888630467851));
#193974=CARTESIAN_POINT('Ctrl Pts',(-29.4516980861541,51.1716284386904,
40.0876491015699));
#193975=CARTESIAN_POINT('Ctrl Pts',(-29.4496602426628,51.1743821937242,
40.0863558569271));
#193976=CARTESIAN_POINT('Ctrl Pts',(-29.4477266300414,51.1771680313594,
40.0849936342771));
#193977=CARTESIAN_POINT('Ctrl Pts',(-29.4467598237307,51.178560950177,40.0843125229521));
#193978=CARTESIAN_POINT('Ctrl Pts',(-29.4458190608832,51.1799618978182,
40.0836141747074));
#193979=CARTESIAN_POINT('Ctrl Pts',(-29.4449045308656,51.1813696738594,
40.0828999161609));
#193980=CARTESIAN_POINT('Ctrl Pts',(-29.4446758983612,51.1817216178698,
40.0827213515243));
#193981=CARTESIAN_POINT('Ctrl Pts',(-29.4444489051049,51.182073988828,40.0825417925842));
#193982=CARTESIAN_POINT('Ctrl Pts',(-29.444223553443,51.1824267683261,40.082361260236));
#193983=CARTESIAN_POINT('Ctrl Pts',(-29.4435474984573,51.1834851068201,
40.0818196631917));
#193984=CARTESIAN_POINT('Ctrl Pts',(-29.4428862193402,51.1845471213154,
40.0812693052022));
#193985=CARTESIAN_POINT('Ctrl Pts',(-29.4422397658675,51.1856123224582,
40.0807107531875));
#193986=CARTESIAN_POINT('Ctrl Pts',(-29.4376862310779,51.1931154617653,
40.0767763849181));
#193987=CARTESIAN_POINT('Ctrl Pts',(-29.4338145801756,51.20077996036,40.0724140586136));
#193988=CARTESIAN_POINT('Ctrl Pts',(-29.4305579784508,51.2085065710734,
40.0677221223766));
#193989=CARTESIAN_POINT('Ctrl Pts',(-29.4289785301334,51.2122539689198,
40.0654465383719));
#193990=CARTESIAN_POINT('Ctrl Pts',(-29.4275440072538,51.2160164979701,
40.0630928000679));
#193991=CARTESIAN_POINT('Ctrl Pts',(-29.4262483256614,51.2197852472981,
40.0606689262479));
#193992=CARTESIAN_POINT('Ctrl Pts',(-29.4242647276701,51.2255549392046,
40.0569581447806));
#193993=CARTESIAN_POINT('Ctrl Pts',(-29.4226066102319,51.2313356805892,
40.0530843804606));
#193994=CARTESIAN_POINT('Ctrl Pts',(-29.4212581193009,51.2370841708901,
40.0490800251458));
#193995=CARTESIAN_POINT('Ctrl Pts',(-29.4206318731364,51.2397537995246,
40.0472203818218));
#193996=CARTESIAN_POINT('Ctrl Pts',(-29.4200721889211,51.2424163366107,
40.0453323608818));
#193997=CARTESIAN_POINT('Ctrl Pts',(-29.4195787111903,51.2450674596719,
40.0434201572162));
#193998=CARTESIAN_POINT('Ctrl Pts',(-29.4195408880667,51.2452706578086,
40.0432735943397));
#193999=CARTESIAN_POINT('Ctrl Pts',(-29.4195034206998,51.2454737959511,
40.0431268995707));
#194000=CARTESIAN_POINT('Ctrl Pts',(-29.4194663081569,51.2456768729758,
40.0429800745037));
#194001=CARTESIAN_POINT('Ctrl Pts',(-29.4189449888197,51.2485294929148,
40.0409176249753));
#194002=CARTESIAN_POINT('Ctrl Pts',(-29.4184957101761,51.251370561363,40.0388310783332));
#194003=CARTESIAN_POINT('Ctrl Pts',(-29.4181151898793,51.2541954110683,
40.036725739981));
#194004=CARTESIAN_POINT('Ctrl Pts',(-29.416750711768,51.2643248197292,40.0291763710715));
#194005=CARTESIAN_POINT('Ctrl Pts',(-29.4162578421116,51.2743237313769,
40.0213310894589));
#194006=CARTESIAN_POINT('Ctrl Pts',(-29.4165161672804,51.2841455249782,
40.0132837551312));
#194007=CARTESIAN_POINT('Ctrl Pts',(-29.4168000406899,51.2949386894592,
40.0044405431316));
#194008=CARTESIAN_POINT('Ctrl Pts',(-29.4179908989231,51.3055186222606,
39.995352871059));
#194009=CARTESIAN_POINT('Ctrl Pts',(-29.4199800715338,51.315837313597,39.9861103629543));
#194010=CARTESIAN_POINT('Ctrl Pts',(-29.422127878739,51.3269789106019,39.9761307737543));
#194011=CARTESIAN_POINT('Ctrl Pts',(-29.4252064644179,51.3378170984271,
39.9659696935998));
#194012=CARTESIAN_POINT('Ctrl Pts',(-29.4291364604201,51.3482921445265,
39.9557128217493));
#194013=CARTESIAN_POINT('Ctrl Pts',(-29.4330334877936,51.3586793157517,
39.9455419945152));
#194014=CARTESIAN_POINT('Ctrl Pts',(-29.4377684584846,51.3687106315449,
39.9352756289336));
#194015=CARTESIAN_POINT('Ctrl Pts',(-29.4433108116256,51.3783102687788,
39.92499));
#194016=CARTESIAN_POINT('Origin',(-0.0131982271536665,-0.00762000000000475,
39.92499));
#194017=CARTESIAN_POINT('Ctrl Pts',(-31.436419577513,54.4189959163066,40.10025));
#194018=CARTESIAN_POINT('Ctrl Pts',(-31.4438560159996,54.414698338812,40.10025));
#194019=CARTESIAN_POINT('Ctrl Pts',(-31.4508673716598,54.4098177483016,
40.0995859581842));
#194020=CARTESIAN_POINT('Ctrl Pts',(-31.4573895320582,54.4044907169115,
40.0983275959622));
#194021=CARTESIAN_POINT('Ctrl Pts',(-31.4615568820638,54.4010869974478,
40.0975235624069));
#194022=CARTESIAN_POINT('Ctrl Pts',(-31.4655251210641,54.3975017237414,
40.0964777059491));
#194023=CARTESIAN_POINT('Ctrl Pts',(-31.469284216974,54.3937759157112,40.0952149915962));
#194024=CARTESIAN_POINT('Ctrl Pts',(-31.474414628622,54.3886909353396,40.0934916398702));
#194025=CARTESIAN_POINT('Ctrl Pts',(-31.4791503318816,54.3833409297224,
40.0913643921631));
#194026=CARTESIAN_POINT('Ctrl Pts',(-31.4834636394924,54.3778174666306,
40.0889118607713));
#194027=CARTESIAN_POINT('Ctrl Pts',(-31.4856202932977,54.3750557350847,
40.0876855950755));
#194028=CARTESIAN_POINT('Ctrl Pts',(-31.4876715300021,54.3722505364145,
40.0863782327527));
#194029=CARTESIAN_POINT('Ctrl Pts',(-31.4896151854255,54.369412577295,40.0850006373334));
#194030=CARTESIAN_POINT('Ctrl Pts',(-31.4905870131372,54.3679935977353,
40.0843118396238));
#194031=CARTESIAN_POINT('Ctrl Pts',(-31.4915319606347,54.3665664194002,
40.0836054919165));
#194032=CARTESIAN_POINT('Ctrl Pts',(-31.4924498523883,54.3651323262971,
40.0828829920418));
#194033=CARTESIAN_POINT('Ctrl Pts',(-31.4926793253267,54.3647738030213,
40.0827023670731));
#194034=CARTESIAN_POINT('Ctrl Pts',(-31.4929071076035,54.3644148473888,
40.0825207326933));
#194035=CARTESIAN_POINT('Ctrl Pts',(-31.4931331971263,54.3640554790924,
40.0823381109276));
#194036=CARTESIAN_POINT('Ctrl Pts',(-31.4938114656948,54.3629773742031,
40.0817902456304));
#194037=CARTESIAN_POINT('Ctrl Pts',(-31.4944744978645,54.3618955562475,
40.0812334935553));
#194038=CARTESIAN_POINT('Ctrl Pts',(-31.4951222515523,54.3608105487852,
40.0806684524227));
#194039=CARTESIAN_POINT('Ctrl Pts',(-31.499598631437,54.3533124740227,40.0767636676139));
#194040=CARTESIAN_POINT('Ctrl Pts',(-31.5034009004289,54.3456575719332,
40.0724404510892));
#194041=CARTESIAN_POINT('Ctrl Pts',(-31.5065976218795,54.3379428492072,
40.0677949937415));
#194042=CARTESIAN_POINT('Ctrl Pts',(-31.5081863836659,54.3341086531883,
40.065486214191));
#194043=CARTESIAN_POINT('Ctrl Pts',(-31.5096252947441,54.3302591366972,
40.0630972003218));
#194044=CARTESIAN_POINT('Ctrl Pts',(-31.5109210155997,54.3264035847699,
40.0606363359906));
#194045=CARTESIAN_POINT('Ctrl Pts',(-31.5137795693407,54.3178976613389,
40.0552073017124));
#194046=CARTESIAN_POINT('Ctrl Pts',(-31.5159526675026,54.3093672304022,
40.0494204304519));
#194047=CARTESIAN_POINT('Ctrl Pts',(-31.5174623893712,54.3009559572069,
40.0434049749851));
#194048=CARTESIAN_POINT('Ctrl Pts',(-31.5180139098083,54.2978832130369,
40.0412074532442));
#194049=CARTESIAN_POINT('Ctrl Pts',(-31.5184846398471,54.2948245130136,
40.0389814735788));
#194050=CARTESIAN_POINT('Ctrl Pts',(-31.5188783726365,54.2917835794185,
40.0367321210017));
#194051=CARTESIAN_POINT('Ctrl Pts',(-31.5202008794128,54.2815694052538,
40.0291767837139));
#194052=CARTESIAN_POINT('Ctrl Pts',(-31.5206547127625,54.2714898389046,
40.0213235332572));
#194053=CARTESIAN_POINT('Ctrl Pts',(-31.5203592886224,54.261591801797,40.0132649215852));
#194054=CARTESIAN_POINT('Ctrl Pts',(-31.520034582497,54.2507126865162,40.0044075527524));
#194055=CARTESIAN_POINT('Ctrl Pts',(-31.5188048676546,54.2400521939118,
39.9953016253709));
#194056=CARTESIAN_POINT('Ctrl Pts',(-31.5167773687222,54.2296591093502,
39.9860353422345));
#194057=CARTESIAN_POINT('Ctrl Pts',(-31.5145936655006,54.2184653119691,
39.9760551582679));
#194058=CARTESIAN_POINT('Ctrl Pts',(-31.5114844302871,54.2075805209345,
39.9658879738137));
#194059=CARTESIAN_POINT('Ctrl Pts',(-31.5075265408317,54.1970658734753,
39.9556174643232));
#194060=CARTESIAN_POINT('Ctrl Pts',(-31.5036220962477,54.1866932092592,
39.945485641389));
#194061=CARTESIAN_POINT('Ctrl Pts',(-31.4988909785566,54.1766795569341,
39.9352519465106));
#194062=CARTESIAN_POINT('Ctrl Pts',(-31.4933613949854,54.1671020372441,
39.92499));
#194063=CARTESIAN_POINT('Ctrl Pts',(-29.7732664904675,51.1878102687788,
39.92499));
#194064=CARTESIAN_POINT('Ctrl Pts',(-29.767974648635,51.1786445298592,39.9348107241724));
#194065=CARTESIAN_POINT('Ctrl Pts',(-29.7619788985601,51.1699291351227,
39.9446038383174));
#194066=CARTESIAN_POINT('Ctrl Pts',(-29.7553188532203,51.1617065245628,
39.9543158069391));
#194067=CARTESIAN_POINT('Ctrl Pts',(-29.7488879934682,51.1537668706101,
39.9636935671398));
#194068=CARTESIAN_POINT('Ctrl Pts',(-29.7418369154162,51.1462857370536,
39.9729968320996));
#194069=CARTESIAN_POINT('Ctrl Pts',(-29.734164291694,51.1393284263626,39.9821731151343));
#194070=CARTESIAN_POINT('Ctrl Pts',(-29.7269112593595,51.1327515888649,
39.990847576436));
#194071=CARTESIAN_POINT('Ctrl Pts',(-29.7191021335077,51.126642241792,39.9994093733854));
#194072=CARTESIAN_POINT('Ctrl Pts',(-29.7107129315309,51.1210907313625,
40.007796611585));
#194073=CARTESIAN_POINT('Ctrl Pts',(-29.7029866172497,51.1159778833906,
40.0155211172603));
#194074=CARTESIAN_POINT('Ctrl Pts',(-29.694767791591,51.1113379461905,40.0230979941029));
#194075=CARTESIAN_POINT('Ctrl Pts',(-29.686025646647,51.1072776647611,40.0304554104755));
#194076=CARTESIAN_POINT('Ctrl Pts',(-29.6834189154966,51.1060669708011,
40.0326492435186));
#194077=CARTESIAN_POINT('Ctrl Pts',(-29.6807655934595,51.1049080895602,
40.0348233715063));
#194078=CARTESIAN_POINT('Ctrl Pts',(-29.6780647241923,51.1038046002596,
40.0369753512356));
#194079=CARTESIAN_POINT('Ctrl Pts',(-29.6753914511533,51.1027123859003,
40.0391053430352));
#194080=CARTESIAN_POINT('Ctrl Pts',(-29.6726744751142,51.1016753170132,
40.041211089324));
#194081=CARTESIAN_POINT('Ctrl Pts',(-29.6699160505195,51.1006978225843,
40.0432881154904));
#194082=CARTESIAN_POINT('Ctrl Pts',(-29.6697242350678,51.1006298495334,
40.043432547828));
#194083=CARTESIAN_POINT('Ctrl Pts',(-29.6695322176085,51.1005621526965,
40.0435768364421));
#194084=CARTESIAN_POINT('Ctrl Pts',(-29.6693399979284,51.1004947333606,
40.0437209807855));
#194085=CARTESIAN_POINT('Ctrl Pts',(-29.6609123829948,51.0975388226979,
40.050040796842));
#194086=CARTESIAN_POINT('Ctrl Pts',(-29.6520916749677,51.0951613514271,
40.0560490279344));
#194087=CARTESIAN_POINT('Ctrl Pts',(-29.6429396446295,51.0934607157664,
40.0616647108614));
#194088=CARTESIAN_POINT('Ctrl Pts',(-29.6344083617421,51.0918754277623,
40.0668995033485));
#194089=CARTESIAN_POINT('Ctrl Pts',(-29.6255883681029,51.0908783954021,
40.0717933267481));
#194090=CARTESIAN_POINT('Ctrl Pts',(-29.6165418049893,51.0905760611939,
40.0762460303072));
#194091=CARTESIAN_POINT('Ctrl Pts',(-29.6132324551649,51.0904654634292,
40.0778748868748));
#194092=CARTESIAN_POINT('Ctrl Pts',(-29.6098929659866,51.0904480940786,
40.0794443522247));
#194093=CARTESIAN_POINT('Ctrl Pts',(-29.6065271365688,51.0905301191542,
40.0809482021492));
#194094=CARTESIAN_POINT('Ctrl Pts',(-29.6057177670362,51.0905498434447,
40.0813098278168));
#194095=CARTESIAN_POINT('Ctrl Pts',(-29.6049064053142,51.0905756628931,
40.0816679525672));
#194096=CARTESIAN_POINT('Ctrl Pts',(-29.6040931741699,51.090607635272,40.082022419258));
#194097=CARTESIAN_POINT('Ctrl Pts',(-29.6033053564988,51.090638608514,40.0823658088648));
#194098=CARTESIAN_POINT('Ctrl Pts',(-29.60251578444,51.0906753561241,40.0827057654616));
#194099=CARTESIAN_POINT('Ctrl Pts',(-29.6017245728788,51.0907179287118,
40.0830421470151));
#194100=CARTESIAN_POINT('Ctrl Pts',(-29.5930559358432,51.0911843606099,
40.0867275956807));
#194101=CARTESIAN_POINT('Ctrl Pts',(-29.5841848213168,51.0923507190419,
40.0899823432032));
#194102=CARTESIAN_POINT('Ctrl Pts',(-29.5752911628161,51.0942731997209,
40.0926299529358));
#194103=CARTESIAN_POINT('Ctrl Pts',(-29.5716026975446,51.0950705097614,
40.0937279956086));
#194104=CARTESIAN_POINT('Ctrl Pts',(-29.5679105139256,51.0959974771977,
40.0947220371803));
#194105=CARTESIAN_POINT('Ctrl Pts',(-29.5642276868785,51.0970562972093,
40.0956014538692));
#194106=CARTESIAN_POINT('Ctrl Pts',(-29.5579462415717,51.098862225076,40.097101390674));
#194107=CARTESIAN_POINT('Ctrl Pts',(-29.551694176475,51.1010529624043,40.0982667904316));
#194108=CARTESIAN_POINT('Ctrl Pts',(-29.5455435225214,51.103638924628,40.0990539325582));
#194109=CARTESIAN_POINT('Ctrl Pts',(-29.5424681955445,51.1049319057399,
40.0994475036216));
#194110=CARTESIAN_POINT('Ctrl Pts',(-29.5394188854254,51.1063249785082,
40.0997467259952));
#194111=CARTESIAN_POINT('Ctrl Pts',(-29.5364046579953,51.1078194668132,
40.0999473488896));
#194112=CARTESIAN_POINT('Ctrl Pts',(-29.5333904305651,51.1093139551182,
40.100147971784));
#194113=CARTESIAN_POINT('Ctrl Pts',(-29.5304113137788,51.1109098228569,
40.10025));
#194114=CARTESIAN_POINT('Ctrl Pts',(-29.527474969218,51.112606865905,40.10025));
#194115=CARTESIAN_POINT('Origin',(-23.6840886581931,53.232803045145,39.92499));
#194116=CARTESIAN_POINT('Ctrl Pts',(-25.3107727110817,57.3172883154492,
39.92499));
#194117=CARTESIAN_POINT('Ctrl Pts',(-25.3150883208942,57.3269813337898,
39.9348354642014));
#194118=CARTESIAN_POINT('Ctrl Pts',(-25.3201559369465,57.336305075241,39.9446440828451));
#194119=CARTESIAN_POINT('Ctrl Pts',(-25.3259384683613,57.345213541718,39.9543641760322));
#194120=CARTESIAN_POINT('Ctrl Pts',(-25.3315331019378,57.3538325360809,
39.9637684240701));
#194121=CARTESIAN_POINT('Ctrl Pts',(-25.337797703811,57.3620638476573,39.9730909636383));
#194122=CARTESIAN_POINT('Ctrl Pts',(-25.3447390861641,57.3698434251107,
39.9822808977126));
#194123=CARTESIAN_POINT('Ctrl Pts',(-25.3513052064445,57.3772024263428,
39.9909740094634));
#194124=CARTESIAN_POINT('Ctrl Pts',(-25.3584775246698,57.3841579102004,
39.9995492764985));
#194125=CARTESIAN_POINT('Ctrl Pts',(-25.3662887884579,57.3906233351685,
40.0079462328677));
#194126=CARTESIAN_POINT('Ctrl Pts',(-25.3734835273317,57.3965784591556,
40.0156804369671));
#194127=CARTESIAN_POINT('Ctrl Pts',(-25.3812207968859,57.4021181432086,
40.0232638017402));
#194128=CARTESIAN_POINT('Ctrl Pts',(-25.3895423083579,57.4071400767265,
40.0306257269946));
#194129=CARTESIAN_POINT('Ctrl Pts',(-25.3919560625124,57.4085967487425,
40.0327611416638));
#194130=CARTESIAN_POINT('Ctrl Pts',(-25.3944190600976,57.4100096047775,
40.0348777427264));
#194131=CARTESIAN_POINT('Ctrl Pts',(-25.396932522092,57.4113754784549,40.0369733168701));
#194132=CARTESIAN_POINT('Ctrl Pts',(-25.3996572764938,57.4128561733383,
40.039245053974));
#194133=CARTESIAN_POINT('Ctrl Pts',(-25.4024370309183,57.4142805418442,
40.041487875195));
#194134=CARTESIAN_POINT('Ctrl Pts',(-25.4052723227222,57.4156446191419,
40.0436985701601));
#194135=CARTESIAN_POINT('Ctrl Pts',(-25.4130538033262,57.419388339989,40.0497658398386));
#194136=CARTESIAN_POINT('Ctrl Pts',(-25.4212623406652,57.4226343338644,
40.0555581699984));
#194137=CARTESIAN_POINT('Ctrl Pts',(-25.4298341608305,57.425300821288,40.0609828468886));
#194138=CARTESIAN_POINT('Ctrl Pts',(-25.4376769109072,57.4277405125137,
40.0659461317306));
#194139=CARTESIAN_POINT('Ctrl Pts',(-25.4458193604268,57.4296843862656,
40.070603998071));
#194140=CARTESIAN_POINT('Ctrl Pts',(-25.4542377154376,57.4310470526571,
40.0748843180608));
#194141=CARTESIAN_POINT('Ctrl Pts',(-25.4583727839187,57.4317163899372,
40.0769867972573));
#194142=CARTESIAN_POINT('Ctrl Pts',(-25.462574317174,57.432244998004,40.0789976708176));
#194143=CARTESIAN_POINT('Ctrl Pts',(-25.4668384019346,57.4326195921324,
40.08090504915));
#194144=CARTESIAN_POINT('Ctrl Pts',(-25.4676474704853,57.4326906677196,
40.0812669556105));
#194145=CARTESIAN_POINT('Ctrl Pts',(-25.4684592045961,57.4327558640765,
40.0816253922033));
#194146=CARTESIAN_POINT('Ctrl Pts',(-25.469273486065,57.4328151061498,40.0819801989139));
#194147=CARTESIAN_POINT('Ctrl Pts',(-25.470062321238,57.4328724969082,40.0823239179149));
#194148=CARTESIAN_POINT('Ctrl Pts',(-25.4708535470242,57.432924299722,40.0826642303498));
#194149=CARTESIAN_POINT('Ctrl Pts',(-25.4716470524585,57.4329704479396,
40.0830009916099));
#194150=CARTESIAN_POINT('Ctrl Pts',(-25.4802945111763,57.4334733617058,
40.086670946431));
#194151=CARTESIAN_POINT('Ctrl Pts',(-25.4892184175041,57.4333046542891,
40.0899175831875));
#194152=CARTESIAN_POINT('Ctrl Pts',(-25.4982455208428,57.4323852136917,
40.0925642067058));
#194153=CARTESIAN_POINT('Ctrl Pts',(-25.502057722639,57.4319969282178,40.0936818922525));
#194154=CARTESIAN_POINT('Ctrl Pts',(-25.5058881199459,57.431475138743,40.094693009479));
#194155=CARTESIAN_POINT('Ctrl Pts',(-25.5097232095982,57.4308157710843,
40.0955863397546));
#194156=CARTESIAN_POINT('Ctrl Pts',(-25.5161814047437,57.4297054124228,
40.0970906856166));
#194157=CARTESIAN_POINT('Ctrl Pts',(-25.5226508554405,57.4282034292358,
40.0982599215483));
#194158=CARTESIAN_POINT('Ctrl Pts',(-25.5290599831058,57.4262902109365,
40.0990497370454));
#194159=CARTESIAN_POINT('Ctrl Pts',(-25.5306622650221,57.4258119063617,
40.0992471909196));
#194160=CARTESIAN_POINT('Ctrl Pts',(-25.5322606952864,57.4253076802619,
40.0994209989363));
#194161=CARTESIAN_POINT('Ctrl Pts',(-25.5338540367004,57.4247769415286,
40.0995705982975));
#194162=CARTESIAN_POINT('Ctrl Pts',(-25.5362440488215,57.4239808334287,
40.0997949973393));
#194163=CARTESIAN_POINT('Ctrl Pts',(-25.5386225912888,57.4231250659716,
40.0999649129781));
#194164=CARTESIAN_POINT('Ctrl Pts',(-25.5409861542577,57.4222091845945,
40.1000786629733));
#194165=CARTESIAN_POINT('Ctrl Pts',(-25.5433497172265,57.4212933032173,
40.1001924129685));
#194166=CARTESIAN_POINT('Ctrl Pts',(-25.5456982979275,57.4203173191903,
40.10025));
#194167=CARTESIAN_POINT('Ctrl Pts',(-25.5480287005713,57.4192809246791,
40.10025));
#194168=CARTESIAN_POINT('Ctrl Pts',(-23.9951532569802,53.9314655730806,
40.10025));
#194169=CARTESIAN_POINT('Ctrl Pts',(-23.9872677980933,53.9349721992642,
40.10025));
#194170=CARTESIAN_POINT('Ctrl Pts',(-23.9797401457373,53.9390993428078,
40.099578633424));
#194171=CARTESIAN_POINT('Ctrl Pts',(-23.9726512030249,53.9437193744806,
40.0983063763363));
#194172=CARTESIAN_POINT('Ctrl Pts',(-23.9680724734011,53.9467034408979,
40.097484628799));
#194173=CARTESIAN_POINT('Ctrl Pts',(-23.9636762467119,53.9498923541895,
40.0964130309336));
#194174=CARTESIAN_POINT('Ctrl Pts',(-23.9594780769917,53.9532454491207,
40.0951176960923));
#194175=CARTESIAN_POINT('Ctrl Pts',(-23.9539136435128,53.9576897843755,
40.0934008039614));
#194176=CARTESIAN_POINT('Ctrl Pts',(-23.9487016177215,53.9624262550347,
40.0912909372156));
#194177=CARTESIAN_POINT('Ctrl Pts',(-23.9438784851449,53.9673725153422,
40.0888630467851));
#194178=CARTESIAN_POINT('Ctrl Pts',(-23.9414669188565,53.969845645496,40.0876491015699));
#194179=CARTESIAN_POINT('Ctrl Pts',(-23.9391523931032,53.972371302523,40.0863558569271));
#194180=CARTESIAN_POINT('Ctrl Pts',(-23.9369381736871,53.9749397614923,
40.0849936342771));
#194181=CARTESIAN_POINT('Ctrl Pts',(-23.935831063979,53.976223990977,40.0843125229521));
#194182=CARTESIAN_POINT('Ctrl Pts',(-23.9347490158249,53.9775189275857,
40.0836141747074));
#194183=CARTESIAN_POINT('Ctrl Pts',(-23.9336923430321,53.9788233972651,
40.0828999161609));
#194184=CARTESIAN_POINT('Ctrl Pts',(-23.9334281748339,53.9791495146849,
40.0827213515243));
#194185=CARTESIAN_POINT('Ctrl Pts',(-23.9331655922757,53.979476228062,40.0825417925842));
#194186=CARTESIAN_POINT('Ctrl Pts',(-23.932904599615,53.9798035193341,40.0823612602361));
#194187=CARTESIAN_POINT('Ctrl Pts',(-23.9321216216328,53.9807853931505,
40.0818196631917));
#194188=CARTESIAN_POINT('Ctrl Pts',(-23.9313529543287,53.9817724673293,
40.0812693052022));
#194189=CARTESIAN_POINT('Ctrl Pts',(-23.9305986983573,53.9827642604007,
40.0807107531875));
#194190=CARTESIAN_POINT('Ctrl Pts',(-23.925285816686,53.9897503227319,40.076776384918));
#194191=CARTESIAN_POINT('Ctrl Pts',(-23.9206342168325,53.9969681366825,
40.0724140586132));
#194192=CARTESIAN_POINT('Ctrl Pts',(-23.9165878043684,54.0043120126406,
40.067722122376));
#194193=CARTESIAN_POINT('Ctrl Pts',(-23.9146252986962,54.0078737845438,
40.0654465383715));
#194194=CARTESIAN_POINT('Ctrl Pts',(-23.9128053429036,54.0114657535938,
40.0630928000676));
#194195=CARTESIAN_POINT('Ctrl Pts',(-23.911122817615,54.0150784217126,40.0606689262479));
#194196=CARTESIAN_POINT('Ctrl Pts',(-23.9085469889525,54.0206091641934,
40.0569581447805));
#194197=CARTESIAN_POINT('Ctrl Pts',(-23.9062937028417,54.0261849176041,
40.0530843804606));
#194198=CARTESIAN_POINT('Ctrl Pts',(-23.9043517182278,54.0317609613889,
40.0490800251458));
#194199=CARTESIAN_POINT('Ctrl Pts',(-23.9034498505266,54.0343505049692,
40.0472203818218));
#194200=CARTESIAN_POINT('Ctrl Pts',(-23.90261492141,54.0369399534676,40.0453323608819));
#194201=CARTESIAN_POINT('Ctrl Pts',(-23.9018470291824,54.0395249709304,
40.0434201572162));
#194202=CARTESIAN_POINT('Ctrl Pts',(-23.9017881732688,54.0397231023335,
40.0432735943397));
#194203=CARTESIAN_POINT('Ctrl Pts',(-23.9017296774342,54.0399212112578,
40.0431268995707));
#194204=CARTESIAN_POINT('Ctrl Pts',(-23.9016715408684,54.0401192964882,
40.0429800745037));
#194205=CARTESIAN_POINT('Ctrl Pts',(-23.9008548973946,54.0429017967675,
40.0409176249753));
#194206=CARTESIAN_POINT('Ctrl Pts',(-23.9001111074275,54.0456803391392,
40.0388310783332));
#194207=CARTESIAN_POINT('Ctrl Pts',(-23.899437394462,54.0484499388204,40.036725739981));
#194208=CARTESIAN_POINT('Ctrl Pts',(-23.8970215795833,54.0583812307209,
40.0291763710714));
#194209=CARTESIAN_POINT('Ctrl Pts',(-23.8954862390496,54.0682738483768,
40.0213310894587));
#194210=CARTESIAN_POINT('Ctrl Pts',(-23.8947164920945,54.0780688394982,
40.0132837551308));
#194211=CARTESIAN_POINT('Ctrl Pts',(-23.8938706175187,54.0888325507465,
40.0044405431308));
#194212=CARTESIAN_POINT('Ctrl Pts',(-23.8939490479888,54.0994790041506,
39.9953528710578));
#194213=CARTESIAN_POINT('Ctrl Pts',(-23.8948487267555,54.1099490937727,
39.9861103629527));
#194214=CARTESIAN_POINT('Ctrl Pts',(-23.8958201540351,54.1212541629309,
39.976130773752));
#194215=CARTESIAN_POINT('Ctrl Pts',(-23.8977489757819,54.13235477786,39.9659696935967));
#194216=CARTESIAN_POINT('Ctrl Pts',(-23.9005625023837,54.1431832370043,
39.9557128217453));
#194217=CARTESIAN_POINT('Ctrl Pts',(-23.9033524263876,54.1539208564999,
39.9455419945125));
#194218=CARTESIAN_POINT('Ctrl Pts',(-23.9070129003889,54.1643921589041,
39.9352756289323));
#194219=CARTESIAN_POINT('Ctrl Pts',(-23.911521456611,54.1745185419761,39.92499));
#194220=CARTESIAN_POINT('Origin',(-0.0139224327744654,-0.0061986664404802,
39.92499));
#194221=CARTESIAN_POINT('Ctrl Pts',(-25.5758735661203,57.4068835917982,
40.10025));
#194222=CARTESIAN_POINT('Ctrl Pts',(-25.5837184861901,57.4033868763699,
40.10025));
#194223=CARTESIAN_POINT('Ctrl Pts',(-25.5912015935364,57.3992659084775,
40.0995859581842));
#194224=CARTESIAN_POINT('Ctrl Pts',(-25.5982448512627,57.3946498105263,
40.0983275959621));
#194225=CARTESIAN_POINT('Ctrl Pts',(-25.6027451576539,57.3917003436859,
40.0975235624068));
#194226=CARTESIAN_POINT('Ctrl Pts',(-25.6070664213767,57.3885495044087,
40.0964777059491));
#194227=CARTESIAN_POINT('Ctrl Pts',(-25.6111943775537,57.3852370392634,
40.0952149915961));
#194228=CARTESIAN_POINT('Ctrl Pts',(-25.6168282094538,57.3807161889918,
40.0934916398701));
#194229=CARTESIAN_POINT('Ctrl Pts',(-25.6220971979011,57.3758905070494,
40.091364392163));
#194230=CARTESIAN_POINT('Ctrl Pts',(-25.6269642358703,57.3708481654825,
40.0889118607713));
#194231=CARTESIAN_POINT('Ctrl Pts',(-25.6293977548549,57.3683269946991,
40.0876855950754));
#194232=CARTESIAN_POINT('Ctrl Pts',(-25.6317309777762,57.3657515758212,
40.0863782327526));
#194233=CARTESIAN_POINT('Ctrl Pts',(-25.6339606331573,57.3631323306533,
40.0850006373334));
#194234=CARTESIAN_POINT('Ctrl Pts',(-25.6350754608479,57.3618227080694,
40.0843118396237));
#194235=CARTESIAN_POINT('Ctrl Pts',(-25.6361644125823,57.3605021218764,
40.0836054919164));
#194236=CARTESIAN_POINT('Ctrl Pts',(-25.6372271795771,57.3591718306997,
40.0828829920418));
#194237=CARTESIAN_POINT('Ctrl Pts',(-25.6374928713258,57.3588392579056,
40.0827023670731));
#194238=CARTESIAN_POINT('Ctrl Pts',(-25.6377569268681,57.358506078401,40.0825207326933));
#194239=CARTESIAN_POINT('Ctrl Pts',(-25.6380193420646,57.358172311552,40.0823381109275));
#194240=CARTESIAN_POINT('Ctrl Pts',(-25.6388065876542,57.3571710110053,
40.0817902456303));
#194241=CARTESIAN_POINT('Ctrl Pts',(-25.6395790684327,57.3561644250955,
40.0812334935553));
#194242=CARTESIAN_POINT('Ctrl Pts',(-25.6403366878207,57.3551530701152,
40.0806684524227));
#194243=CARTESIAN_POINT('Ctrl Pts',(-25.6455723078606,57.3481639797008,
40.0767636676137));
#194244=CARTESIAN_POINT('Ctrl Pts',(-25.6501539027771,57.3409484573004,
40.0724404510889));
#194245=CARTESIAN_POINT('Ctrl Pts',(-25.6541395203643,57.3336101450131,
40.0677949937411));
#194246=CARTESIAN_POINT('Ctrl Pts',(-25.656120361365,57.3299630239495,40.0654862141907));
#194247=CARTESIAN_POINT('Ctrl Pts',(-25.6579537739808,57.3262850026765,
40.0630972003217));
#194248=CARTESIAN_POINT('Ctrl Pts',(-25.6596454116599,57.3225860115761,
40.0606363359906));
#194249=CARTESIAN_POINT('Ctrl Pts',(-25.6633774170493,57.3144254847134,
40.0552073017124));
#194250=CARTESIAN_POINT('Ctrl Pts',(-25.6664302835889,57.3061689349814,
40.0494204304519));
#194251=CARTESIAN_POINT('Ctrl Pts',(-25.6688109525044,57.2979615485276,
40.0434049749851));
#194252=CARTESIAN_POINT('Ctrl Pts',(-25.669680640881,57.2949632867554,40.0412074532442));
#194253=CARTESIAN_POINT('Ctrl Pts',(-25.6704685134244,57.2919705472985,
40.0389814735788));
#194254=CARTESIAN_POINT('Ctrl Pts',(-25.67117795342,57.2889874285393,40.0367321210017));
#194255=CARTESIAN_POINT('Ctrl Pts',(-25.6735608872945,57.2789674482913,
40.0291767837146));
#194256=CARTESIAN_POINT('Ctrl Pts',(-25.6750658360785,57.2689905373647,
40.0213235332587));
#194257=CARTESIAN_POINT('Ctrl Pts',(-25.675806656911,57.2591158425095,40.0132649215875));
#194258=CARTESIAN_POINT('Ctrl Pts',(-25.6766209067618,57.248262383129,40.0044075527555));
#194259=CARTESIAN_POINT('Ctrl Pts',(-25.6765122533358,57.2375317496164,
39.9953016253747));
#194260=CARTESIAN_POINT('Ctrl Pts',(-25.6755822344128,57.2269836681125,
39.9860353422391));
#194261=CARTESIAN_POINT('Ctrl Pts',(-25.6745805641847,57.2156229323833,
39.9760551582733));
#194262=CARTESIAN_POINT('Ctrl Pts',(-25.6726261321672,57.2044727657947,
39.9658879738199));
#194263=CARTESIAN_POINT('Ctrl Pts',(-25.6697890043857,57.1936020065725,
39.9556174643302));
#194264=CARTESIAN_POINT('Ctrl Pts',(-25.6669901874079,57.1828780393016,
39.9454856413937));
#194265=CARTESIAN_POINT('Ctrl Pts',(-25.6633316989632,57.1724247063476,
39.935251946513));
#194266=CARTESIAN_POINT('Ctrl Pts',(-25.6588335304436,57.1623216544373,
39.92499));
#194267=CARTESIAN_POINT('Ctrl Pts',(-24.2595822759728,54.0195518809643,
39.92499));
#194268=CARTESIAN_POINT('Ctrl Pts',(-24.2552775040072,54.0098832048262,
39.9348107241732));
#194269=CARTESIAN_POINT('Ctrl Pts',(-24.2502256060967,54.0005888273918,
39.9446038383189));
#194270=CARTESIAN_POINT('Ctrl Pts',(-24.2444615420275,53.9917150968476,
39.9543158069413));
#194271=CARTESIAN_POINT('Ctrl Pts',(-24.2388958310241,53.9831467292621,
39.9636935671426));
#194272=CARTESIAN_POINT('Ctrl Pts',(-24.232665370909,53.9749695397845,39.972996832103));
#194273=CARTESIAN_POINT('Ctrl Pts',(-24.2257620156167,53.9672483344021,
39.9821731151383));
#194274=CARTESIAN_POINT('Ctrl Pts',(-24.2192361828685,53.959949377184,39.9908475764405));
#194275=CARTESIAN_POINT('Ctrl Pts',(-24.2121084368856,53.9530572218286,
39.9994093733904));
#194276=CARTESIAN_POINT('Ctrl Pts',(-24.2043454826882,53.9466592127632,
40.0077966115905));
#194277=CARTESIAN_POINT('Ctrl Pts',(-24.1971959321057,53.9407667537486,
40.0155211172663));
#194278=CARTESIAN_POINT('Ctrl Pts',(-24.1895071355381,53.9352931333939,
40.0230979941094));
#194279=CARTESIAN_POINT('Ctrl Pts',(-24.181237295956,53.9303412916343,40.0304554104825));
#194280=CARTESIAN_POINT('Ctrl Pts',(-24.1787713967332,53.9288647523828,
40.0326492435231));
#194281=CARTESIAN_POINT('Ctrl Pts',(-24.1762537459497,53.9274348719411,
40.0348233715086));
#194282=CARTESIAN_POINT('Ctrl Pts',(-24.1736830183705,53.9260551099578,
40.0369753512356));
#194283=CARTESIAN_POINT('Ctrl Pts',(-24.1711385572894,53.9246894457404,
40.0391053430352));
#194284=CARTESIAN_POINT('Ctrl Pts',(-24.1685448683464,53.9233740566951,
40.041211089324));
#194285=CARTESIAN_POINT('Ctrl Pts',(-24.1659037306808,53.922113583199,40.0432881154904));
#194286=CARTESIAN_POINT('Ctrl Pts',(-24.1657200711328,53.9220259323371,
40.0434325478279));
#194287=CARTESIAN_POINT('Ctrl Pts',(-24.1655361818115,53.9219385350607,
40.0435768364421));
#194288=CARTESIAN_POINT('Ctrl Pts',(-24.1653520623704,53.9218513926272,
40.0437209807855));
#194289=CARTESIAN_POINT('Ctrl Pts',(-24.1572795915922,53.9180307491142,
40.0500407968422));
#194290=CARTESIAN_POINT('Ctrl Pts',(-24.1487557177448,53.9147442868247,
40.0560490279348));
#194291=CARTESIAN_POINT('Ctrl Pts',(-24.1398315880183,53.9120963197571,
40.0616647108619));
#194292=CARTESIAN_POINT('Ctrl Pts',(-24.1315127481097,53.9096279542365,
40.0668995033492));
#194293=CARTESIAN_POINT('Ctrl Pts',(-24.1228452895785,53.9077144433428,
40.071793326749));
#194294=CARTESIAN_POINT('Ctrl Pts',(-24.113879887014,53.906468142013,40.0762460303083));
#194295=CARTESIAN_POINT('Ctrl Pts',(-24.1106002267692,53.9060122288629,
40.0778748868755));
#194296=CARTESIAN_POINT('Ctrl Pts',(-24.1072808472542,53.9056458829917,
40.0794443522251));
#194297=CARTESIAN_POINT('Ctrl Pts',(-24.1039248822477,53.9053756337488,
40.0809482021492));
#194298=CARTESIAN_POINT('Ctrl Pts',(-24.1031178847763,53.9053106478341,
40.0813098278169));
#194299=CARTESIAN_POINT('Ctrl Pts',(-24.1023082689114,53.9052515154468,
40.0816679525672));
#194300=CARTESIAN_POINT('Ctrl Pts',(-24.1014961507088,53.9051983068758,
40.0820224192581));
#194301=CARTESIAN_POINT('Ctrl Pts',(-24.1007094112,53.9051467610727,40.0823658088648));
#194302=CARTESIAN_POINT('Ctrl Pts',(-24.0999203233284,53.9051007746216,
40.0827057654617));
#194303=CARTESIAN_POINT('Ctrl Pts',(-24.0991289960597,53.9050604098636,
40.0830421470151));
#194304=CARTESIAN_POINT('Ctrl Pts',(-24.0904590913156,53.9046181672911,
40.0867275956806));
#194305=CARTESIAN_POINT('Ctrl Pts',(-24.0815146560285,53.9048508523206,
40.089982343203));
#194306=CARTESIAN_POINT('Ctrl Pts',(-24.072468763969,53.9058331609933,40.0926299529355));
#194307=CARTESIAN_POINT('Ctrl Pts',(-24.0687171629026,53.9062405536793,
40.0937279956084));
#194308=CARTESIAN_POINT('Ctrl Pts',(-24.0649483109698,53.9067765048112,
40.0947220371802));
#194309=CARTESIAN_POINT('Ctrl Pts',(-24.0611749820056,53.9074445642444,
40.0956014538693));
#194310=CARTESIAN_POINT('Ctrl Pts',(-24.0547391762487,53.9085840092243,
40.097101390674));
#194311=CARTESIAN_POINT('Ctrl Pts',(-24.0482923662124,53.9101092267075,
40.0982667904316));
#194312=CARTESIAN_POINT('Ctrl Pts',(-24.0419050995275,53.9120381043539,
40.0990539325583));
#194313=CARTESIAN_POINT('Ctrl Pts',(-24.038711466185,53.9130025431771,40.0994475036216));
#194314=CARTESIAN_POINT('Ctrl Pts',(-24.03553324475,53.9140692448462,40.0997467259952));
#194315=CARTESIAN_POINT('Ctrl Pts',(-24.0323793130072,53.9152404736266,
40.0999473488896));
#194316=CARTESIAN_POINT('Ctrl Pts',(-24.0292253812643,53.916411702407,40.100147971784));
#194317=CARTESIAN_POINT('Ctrl Pts',(-24.0260957707892,53.9176874253155,
40.10025));
#194318=CARTESIAN_POINT('Ctrl Pts',(-24.0229981225292,53.9190682401997,
40.10025));
#194319=CARTESIAN_POINT('Origin',(-17.9900016446778,55.4168495715594,39.92499));
#194320=CARTESIAN_POINT('Ctrl Pts',(-19.1808295835776,59.6489943884566,
39.92499));
#194321=CARTESIAN_POINT('Ctrl Pts',(-19.1841083557164,59.6590854114903,
39.9348354642017));
#194322=CARTESIAN_POINT('Ctrl Pts',(-19.188173614472,59.6688877866287,39.9446440828455));
#194323=CARTESIAN_POINT('Ctrl Pts',(-19.1929932802638,59.6783518907168,
39.9543641760327));
#194324=CARTESIAN_POINT('Ctrl Pts',(-19.1976563356165,59.6875084677772,
39.9637684240707));
#194325=CARTESIAN_POINT('Ctrl Pts',(-19.2030262129955,59.6963495165744,
39.973090963639));
#194326=CARTESIAN_POINT('Ctrl Pts',(-19.2091163824538,59.7048120487189,
39.9822808977133));
#194327=CARTESIAN_POINT('Ctrl Pts',(-19.2148773077503,59.7128170830349,
39.9909740094641));
#194328=CARTESIAN_POINT('Ctrl Pts',(-19.2212832892271,59.7204841754264,
39.9995492764992));
#194329=CARTESIAN_POINT('Ctrl Pts',(-19.2283759411587,59.72773068152,40.0079462328684));
#194330=CARTESIAN_POINT('Ctrl Pts',(-19.2349087865413,59.7344052377129,
40.0156804369678));
#194331=CARTESIAN_POINT('Ctrl Pts',(-19.2420246158623,59.7407233396934,
40.0232638017409));
#194332=CARTESIAN_POINT('Ctrl Pts',(-19.2497756062306,59.7465875973403,
40.0306257269953));
#194333=CARTESIAN_POINT('Ctrl Pts',(-19.2520238738997,59.7482885955669,
40.0327611416643));
#194334=CARTESIAN_POINT('Ctrl Pts',(-19.2543256952561,59.7499511651811,
40.0348777427266));
#194335=CARTESIAN_POINT('Ctrl Pts',(-19.2566826155659,59.7515722847792,
40.03697331687));
#194336=CARTESIAN_POINT('Ctrl Pts',(-19.2592376687173,59.7533296826515,
40.039245053974));
#194337=CARTESIAN_POINT('Ctrl Pts',(-19.2618533083051,59.7550368117759,
40.041487875195));
#194338=CARTESIAN_POINT('Ctrl Pts',(-19.2645304831802,59.7566897852106,
40.0436985701601));
#194339=CARTESIAN_POINT('Ctrl Pts',(-19.2718780106322,59.7612263837726,
40.0497658398386));
#194340=CARTESIAN_POINT('Ctrl Pts',(-19.2797022819932,59.7653126215478,
40.0555581699984));
#194341=CARTESIAN_POINT('Ctrl Pts',(-19.2879484209981,59.7688605008636,
40.0609828468886));
#194342=CARTESIAN_POINT('Ctrl Pts',(-19.2954931904943,59.7721066178187,
40.0659461317305));
#194343=CARTESIAN_POINT('Ctrl Pts',(-19.3033878446872,59.7748909605621,
40.0706039980708));
#194344=CARTESIAN_POINT('Ctrl Pts',(-19.3116176456444,59.7771261198371,
40.0748843180605));
#194345=CARTESIAN_POINT('Ctrl Pts',(-19.3156600969906,59.7782240227715,
40.0769867972571));
#194346=CARTESIAN_POINT('Ctrl Pts',(-19.3197833592184,59.7791889148825,
40.0789976708176));
#194347=CARTESIAN_POINT('Ctrl Pts',(-19.3239849291282,59.7800071751724,
40.08090504915));
#194348=CARTESIAN_POINT('Ctrl Pts',(-19.3247821360948,59.7801624320925,
40.0812669556105));
#194349=CARTESIAN_POINT('Ctrl Pts',(-19.3255826085661,59.7803121206161,
40.0816253922033));
#194350=CARTESIAN_POINT('Ctrl Pts',(-19.3263862368331,59.7804561537456,
40.081980198914));
#194351=CARTESIAN_POINT('Ctrl Pts',(-19.3271647517167,59.7805956858399,
40.0823239179149));
#194352=CARTESIAN_POINT('Ctrl Pts',(-19.3279462282167,59.780729910488,40.0826642303499));
#194353=CARTESIAN_POINT('Ctrl Pts',(-19.328730562943,59.7808587498045,40.08300099161));
#194354=CARTESIAN_POINT('Ctrl Pts',(-19.3372780811743,59.7822628141275,
40.0866709464312));
#194355=CARTESIAN_POINT('Ctrl Pts',(-19.3461707361367,59.7830278331224,
40.0899175831877));
#194356=CARTESIAN_POINT('Ctrl Pts',(-19.3552444957718,59.7830570185564,
40.0925642067061));
#194357=CARTESIAN_POINT('Ctrl Pts',(-19.3590764008113,59.7830693437465,
40.0936818922527));
#194358=CARTESIAN_POINT('Ctrl Pts',(-19.3629403566526,59.7829507982332,
40.094693009479));
#194359=CARTESIAN_POINT('Ctrl Pts',(-19.3668233599705,59.7826959186873,
40.0955863397546));
#194360=CARTESIAN_POINT('Ctrl Pts',(-19.3733622405317,59.7822667079008,
40.0970906856167));
#194361=CARTESIAN_POINT('Ctrl Pts',(-19.3799532508951,59.7814491944744,
40.0982599215483));
#194362=CARTESIAN_POINT('Ctrl Pts',(-19.3865272544572,59.780216393251,40.0990497370454));
#194363=CARTESIAN_POINT('Ctrl Pts',(-19.3881707553477,59.7799081929452,
40.0992471909196));
#194364=CARTESIAN_POINT('Ctrl Pts',(-19.3898131352231,59.7795738105079,
40.0994209989363));
#194365=CARTESIAN_POINT('Ctrl Pts',(-19.3914532254504,59.7792125287464,
40.0995705982975));
#194366=CARTESIAN_POINT('Ctrl Pts',(-19.3939133607912,59.7786706061041,
40.0997949973393));
#194367=CARTESIAN_POINT('Ctrl Pts',(-19.3963683254113,59.7780681520196,
40.0999649129781));
#194368=CARTESIAN_POINT('Ctrl Pts',(-19.3988146762078,59.7774043475414,
40.1000786629733));
#194369=CARTESIAN_POINT('Ctrl Pts',(-19.4012610270042,59.7767405430632,
40.1001924129685));
#194370=CARTESIAN_POINT('Ctrl Pts',(-19.4036987600454,59.7760153991119,
40.10025));
#194371=CARTESIAN_POINT('Ctrl Pts',(-19.4061247292253,59.7752282754855,
40.10025));
#194372=CARTESIAN_POINT('Ctrl Pts',(-18.2263320786577,56.1441998575529,
40.10025));
#194373=CARTESIAN_POINT('Ctrl Pts',(-18.2181232748938,56.1468630191715,
40.10025));
#194374=CARTESIAN_POINT('Ctrl Pts',(-18.2102054558333,56.150180699858,40.0995786334241));
#194375=CARTESIAN_POINT('Ctrl Pts',(-18.2026724222802,56.1540344262256,
40.0983063763366));
#194376=CARTESIAN_POINT('Ctrl Pts',(-18.1978068555391,56.1565235380438,
40.0974846287992));
#194377=CARTESIAN_POINT('Ctrl Pts',(-18.1931013796334,56.1592354513149,
40.0964130309338));
#194378=CARTESIAN_POINT('Ctrl Pts',(-18.1885757140654,56.1621313494121,
40.0951176960924));
#194379=CARTESIAN_POINT('Ctrl Pts',(-18.1825772036009,56.1659696964529,
40.0934008039615));
#194380=CARTESIAN_POINT('Ctrl Pts',(-18.1768986338329,56.1701354151837,
40.0912909372157));
#194381=CARTESIAN_POINT('Ctrl Pts',(-18.1715848978922,56.1745504247234,
40.0888630467852));
#194382=CARTESIAN_POINT('Ctrl Pts',(-18.1689280299218,56.1767579294932,
40.0876491015699));
#194383=CARTESIAN_POINT('Ctrl Pts',(-18.1663621803349,56.1790278168866,
40.0863558569272));
#194384=CARTESIAN_POINT('Ctrl Pts',(-18.1638916135754,56.1813507566161,
40.0849936342771));
#194385=CARTESIAN_POINT('Ctrl Pts',(-18.1626563301957,56.1825122264808,
40.0843125229521));
#194386=CARTESIAN_POINT('Ctrl Pts',(-18.1614448518808,56.1836869644605,
40.0836141747075));
#194387=CARTESIAN_POINT('Ctrl Pts',(-18.1602576134412,56.1848738357354,
40.082899916161));
#194388=CARTESIAN_POINT('Ctrl Pts',(-18.1599608038313,56.1851705535541,
40.0827213515244));
#194389=CARTESIAN_POINT('Ctrl Pts',(-18.1596655088806,56.1854680298098,
40.0825417925842));
#194390=CARTESIAN_POINT('Ctrl Pts',(-18.1593717347113,56.1857662469843,
40.0823612602361));
#194391=CARTESIAN_POINT('Ctrl Pts',(-18.1584904122033,56.1866608985079,
40.0818196631918));
#194392=CARTESIAN_POINT('Ctrl Pts',(-18.157622778392,56.1875622177791,40.0812693052022));
#194393=CARTESIAN_POINT('Ctrl Pts',(-18.156768983708,56.1884697364866,40.0807107531875));
#194394=CARTESIAN_POINT('Ctrl Pts',(-18.1507549641989,56.1948621810806,
40.0767763849181));
#194395=CARTESIAN_POINT('Ctrl Pts',(-18.1453743792958,56.2015542305065,
40.0724140586135));
#194396=CARTESIAN_POINT('Ctrl Pts',(-18.1405824894343,56.2084349106669,
40.0677221223765));
#194397=CARTESIAN_POINT('Ctrl Pts',(-18.1382584280299,56.211772033109,40.0654465383718));
#194398=CARTESIAN_POINT('Ctrl Pts',(-18.1360729791405,56.2151540877948,
40.0630928000678));
#194399=CARTESIAN_POINT('Ctrl Pts',(-18.1340220442546,56.218571093557,40.0606689262479));
#194400=CARTESIAN_POINT('Ctrl Pts',(-18.1308822062388,56.22380229064,40.0569581447806));
#194401=CARTESIAN_POINT('Ctrl Pts',(-18.1280584389294,56.2291119669557,
40.0530843804606));
#194402=CARTESIAN_POINT('Ctrl Pts',(-18.1255442374226,56.2344544719218,
40.0490800251458));
#194403=CARTESIAN_POINT('Ctrl Pts',(-18.124376629236,56.2369355588665,40.0472203818218));
#194404=CARTESIAN_POINT('Ctrl Pts',(-18.1232756028762,56.2394235482377,
40.0453323608819));
#194405=CARTESIAN_POINT('Ctrl Pts',(-18.1222417093396,56.2419141381098,
40.0434201572162));
#194406=CARTESIAN_POINT('Ctrl Pts',(-18.1221624654738,56.2421050320101,
40.0432735943397));
#194407=CARTESIAN_POINT('Ctrl Pts',(-18.1220835820641,56.2422959411933,
40.0431268995708));
#194408=CARTESIAN_POINT('Ctrl Pts',(-18.1220050584317,56.2424868643661,
40.0429800745037));
#194409=CARTESIAN_POINT('Ctrl Pts',(-18.1209020381381,56.2451687593305,
40.0409176249753));
#194410=CARTESIAN_POINT('Ctrl Pts',(-18.119871885966,56.2478543333341,40.0388310783333));
#194411=CARTESIAN_POINT('Ctrl Pts',(-18.1189123616721,56.2505383386775,
40.036725739981));
#194412=CARTESIAN_POINT('Ctrl Pts',(-18.1154716782,56.2601627045038,40.0291763710724));
#194413=CARTESIAN_POINT('Ctrl Pts',(-18.1129106883013,56.2698406425772,
40.0213310894607));
#194414=CARTESIAN_POINT('Ctrl Pts',(-18.111121302731,56.2795015152448,40.0132837551339));
#194415=CARTESIAN_POINT('Ctrl Pts',(-18.1091549477489,56.2901178437856,
40.0044405431352));
#194416=CARTESIAN_POINT('Ctrl Pts',(-18.1081200911549,56.300714173019,39.9953528710635));
#194417=CARTESIAN_POINT('Ctrl Pts',(-18.1079204190083,56.3112209484322,
39.9861103629598));
#194418=CARTESIAN_POINT('Ctrl Pts',(-18.1077048232009,56.3225656290374,
39.976130773761));
#194419=CARTESIAN_POINT('Ctrl Pts',(-18.1084627484397,56.3338070504076,
39.9659696936077));
#194420=CARTESIAN_POINT('Ctrl Pts',(-18.1101289800535,56.3448702837299,
39.9557128217582));
#194421=CARTESIAN_POINT('Ctrl Pts',(-18.1117812336966,56.355840707896,39.9455419945212));
#194422=CARTESIAN_POINT('Ctrl Pts',(-18.1143271060902,56.3666372711369,
39.9352756289366));
#194423=CARTESIAN_POINT('Ctrl Pts',(-18.1177524687101,56.3771794532809,
39.92499));
#194424=CARTESIAN_POINT('Origin',(-0.0144941013083308,-0.0047094189942794,
39.92499));
#194425=CARTESIAN_POINT('Ctrl Pts',(-19.4351129318415,59.7658094374953,
40.10025));
#194426=CARTESIAN_POINT('Ctrl Pts',(-19.4432803829089,59.7631518948793,
40.10025));
#194427=CARTESIAN_POINT('Ctrl Pts',(-19.4511532554514,59.7598356997914,
40.0995859581841));
#194428=CARTESIAN_POINT('Ctrl Pts',(-19.4586404431004,59.7559811102141,
40.098327595962));
#194429=CARTESIAN_POINT('Ctrl Pts',(-19.4634243995782,59.7535182109732,
40.0975235624067));
#194430=CARTESIAN_POINT('Ctrl Pts',(-19.4680513433534,59.7508363273796,
40.096477705949));
#194431=CARTESIAN_POINT('Ctrl Pts',(-19.4725029330456,59.7479734971808,
40.0952149915961));
#194432=CARTESIAN_POINT('Ctrl Pts',(-19.4785784597567,59.7440663083909,
40.0934916398701));
#194433=CARTESIAN_POINT('Ctrl Pts',(-19.4843230052516,59.7398178213044,
40.091364392163));
#194434=CARTESIAN_POINT('Ctrl Pts',(-19.4896904492928,59.7353118462118,
40.0889118607713));
#194435=CARTESIAN_POINT('Ctrl Pts',(-19.4923741713134,59.7330588586655,
40.0876855950754));
#194436=CARTESIAN_POINT('Ctrl Pts',(-19.494963817173,59.7307414364082,40.0863782327526));
#194437=CARTESIAN_POINT('Ctrl Pts',(-19.497455043941,59.72836960219,40.0850006373333));
#194438=CARTESIAN_POINT('Ctrl Pts',(-19.498700657325,59.7271836850808,40.0843118396237));
#194439=CARTESIAN_POINT('Ctrl Pts',(-19.4999216825132,59.7259841596485,
40.0836054919164));
#194440=CARTESIAN_POINT('Ctrl Pts',(-19.5011176808517,59.7247722453469,
40.0828829920417));
#194441=CARTESIAN_POINT('Ctrl Pts',(-19.5014166804363,59.7244692667715,
40.082702367073));
#194442=CARTESIAN_POINT('Ctrl Pts',(-19.5017141161962,59.7241655137792,
40.0825207326932));
#194443=CARTESIAN_POINT('Ctrl Pts',(-19.5020099819907,59.7238610051972,
40.0823381109275));
#194444=CARTESIAN_POINT('Ctrl Pts',(-19.502897579374,59.7229474794513,40.0817902456303));
#194445=CARTESIAN_POINT('Ctrl Pts',(-19.5037710453003,59.7220271539531,
40.0812334935553));
#194446=CARTESIAN_POINT('Ctrl Pts',(-19.5046302297519,59.7211005320715,
40.0806684524226));
#194447=CARTESIAN_POINT('Ctrl Pts',(-19.5105677273981,59.7146969999428,
40.0767636676137));
#194448=CARTESIAN_POINT('Ctrl Pts',(-19.5158784513264,59.707999912005,40.0724404510889));
#194449=CARTESIAN_POINT('Ctrl Pts',(-19.5206092977898,59.7011184102419,
40.0677949937411));
#194450=CARTESIAN_POINT('Ctrl Pts',(-19.5229605154963,59.6976983227548,
40.0654862141907));
#194451=CARTESIAN_POINT('Ctrl Pts',(-19.5251683423975,59.6942320938704,
40.0630972003217));
#194452=CARTESIAN_POINT('Ctrl Pts',(-19.5272373629638,59.6907301905173,
40.0606363359906));
#194453=CARTESIAN_POINT('Ctrl Pts',(-19.5318019313697,59.6830044686628,
40.0552073017123));
#194454=CARTESIAN_POINT('Ctrl Pts',(-19.5357011184423,59.6751122606221,
40.0494204304519));
#194455=CARTESIAN_POINT('Ctrl Pts',(-19.5389266512978,59.6671986827533,
40.0434049749851));
#194456=CARTESIAN_POINT('Ctrl Pts',(-19.540104979126,59.6643077529624,40.0412074532442));
#194457=CARTESIAN_POINT('Ctrl Pts',(-19.5412013620775,59.6614137631515,
40.0389814735788));
#194458=CARTESIAN_POINT('Ctrl Pts',(-19.5422187365062,59.6585211429014,
40.0367321210017));
#194459=CARTESIAN_POINT('Ctrl Pts',(-19.5456359895572,59.6488051375689,
40.0291767837141));
#194460=CARTESIAN_POINT('Ctrl Pts',(-19.5481755652417,59.6390401911873,
40.0213235332577));
#194461=CARTESIAN_POINT('Ctrl Pts',(-19.5499445144585,59.6292970278063,
40.013264921586));
#194462=CARTESIAN_POINT('Ctrl Pts',(-19.5518887991937,59.6185881370969,
40.0044075527534));
#194463=CARTESIAN_POINT('Ctrl Pts',(-19.5529023976133,59.6079049297412,
39.9953016253721));
#194464=CARTESIAN_POINT('Ctrl Pts',(-19.5530800481813,59.5973174182821,
39.9860353422359));
#194465=CARTESIAN_POINT('Ctrl Pts',(-19.5532713854546,59.5859142148018,
39.9760551582696));
#194466=CARTESIAN_POINT('Ctrl Pts',(-19.5524931697987,59.5746208362166,
39.9658879738156));
#194467=CARTESIAN_POINT('Ctrl Pts',(-19.5508078878557,59.5635130675434,
39.9556174643253));
#194468=CARTESIAN_POINT('Ctrl Pts',(-19.5491453629091,59.5525552912514,
39.9454856413904));
#194469=CARTESIAN_POINT('Ctrl Pts',(-19.5465995868769,59.5417768065758,
39.9352519465114));
#194470=CARTESIAN_POINT('Ctrl Pts',(-19.5431821162861,59.5312589135997,
39.92499));
#194471=CARTESIAN_POINT('Ctrl Pts',(-18.4801050014185,56.259443978424,39.92499));
#194472=CARTESIAN_POINT('Ctrl Pts',(-18.4768344633031,56.2493782971084,
39.934810724172));
#194473=CARTESIAN_POINT('Ctrl Pts',(-18.4727817672087,56.239606768122,39.9446038383166));
#194474=CARTESIAN_POINT('Ctrl Pts',(-18.4679768367035,56.2301791400439,
39.9543158069379));
#194475=CARTESIAN_POINT('Ctrl Pts',(-18.4633372535444,56.2210759356552,
39.9636935671383));
#194476=CARTESIAN_POINT('Ctrl Pts',(-18.4579956735924,56.2122922812566,
39.9729968320978));
#194477=CARTESIAN_POINT('Ctrl Pts',(-18.4519372213368,56.2038917763258,
39.9821731151322));
#194478=CARTESIAN_POINT('Ctrl Pts',(-18.4462100865656,56.195950668291,39.9908475764336));
#194479=CARTESIAN_POINT('Ctrl Pts',(-18.4398418135299,56.1883512165501,
39.9994093733827));
#194480=CARTESIAN_POINT('Ctrl Pts',(-18.4327901596646,56.1811768067756,
40.007796611582));
#194481=CARTESIAN_POINT('Ctrl Pts',(-18.4262957047551,56.1745692957332,
40.015521117257));
#194482=CARTESIAN_POINT('Ctrl Pts',(-18.4192211773452,56.1683219623542,
40.0230979940993));
#194483=CARTESIAN_POINT('Ctrl Pts',(-18.4115142492208,56.1625328136792,
40.0304554104717));
#194484=CARTESIAN_POINT('Ctrl Pts',(-18.4092161988273,56.160806606405,40.032649243516));
#194485=CARTESIAN_POINT('Ctrl Pts',(-18.4068618031996,56.1591213928276,
40.034823371505));
#194486=CARTESIAN_POINT('Ctrl Pts',(-18.4044493827309,56.1574804751188,
40.0369753512355));
#194487=CARTESIAN_POINT('Ctrl Pts',(-18.4020616112559,56.1558563235462,
40.0391053430352));
#194488=CARTESIAN_POINT('Ctrl Pts',(-18.3996196264078,56.1542770260204,
40.041211089324));
#194489=CARTESIAN_POINT('Ctrl Pts',(-18.3971247125282,56.1527473834685,
40.0432881154904));
#194490=CARTESIAN_POINT('Ctrl Pts',(-18.3969512210963,56.152641015117,40.043432547828));
#194491=CARTESIAN_POINT('Ctrl Pts',(-18.3967774746429,56.1525348749438,
40.0435768364421));
#194492=CARTESIAN_POINT('Ctrl Pts',(-18.3966034726921,56.1524289641634,
40.0437209807855));
#194493=CARTESIAN_POINT('Ctrl Pts',(-18.3889745897489,56.1477854475704,
40.0500407968419));
#194494=CARTESIAN_POINT('Ctrl Pts',(-18.3808409394273,56.143626001431,40.0560490279342));
#194495=CARTESIAN_POINT('Ctrl Pts',(-18.372242484946,56.1400597146378,40.0616647108612));
#194496=CARTESIAN_POINT('Ctrl Pts',(-18.3642272309682,56.1367353155302,
40.066899503348));
#194497=CARTESIAN_POINT('Ctrl Pts',(-18.3558072700357,56.1339262909288,
40.0717933267475));
#194498=CARTESIAN_POINT('Ctrl Pts',(-18.3470212548482,56.1317496772155,
40.0762460303064));
#194499=CARTESIAN_POINT('Ctrl Pts',(-18.3438072168252,56.1309534437596,
40.0778748868742));
#194500=CARTESIAN_POINT('Ctrl Pts',(-18.3405443147883,56.1302421351294,
40.0794443522245));
#194501=CARTESIAN_POINT('Ctrl Pts',(-18.337234982846,56.1296225724749,40.0809482021492));
#194502=CARTESIAN_POINT('Ctrl Pts',(-18.336439199069,56.1294735883543,40.0813098278168));
#194503=CARTESIAN_POINT('Ctrl Pts',(-18.3356401993822,56.1293301519982,
40.0816679525672));
#194504=CARTESIAN_POINT('Ctrl Pts',(-18.3348380918581,56.1291923454417,
40.082022419258));
#194505=CARTESIAN_POINT('Ctrl Pts',(-18.3340610501942,56.1290588453401,
40.0823658088648));
#194506=CARTESIAN_POINT('Ctrl Pts',(-18.3332810919216,56.1289306286649,
40.0827057654616));
#194507=CARTESIAN_POINT('Ctrl Pts',(-18.3324983188927,56.1288077688059,
40.0830421470151));
#194508=CARTESIAN_POINT('Ctrl Pts',(-18.3239221357297,56.1274616970648,
40.0867275956808));
#194509=CARTESIAN_POINT('Ctrl Pts',(-18.3150023767858,56.126758159346,40.0899823432035));
#194510=CARTESIAN_POINT('Ctrl Pts',(-18.3059033598527,56.1267895336332,
40.0926299529361));
#194511=CARTESIAN_POINT('Ctrl Pts',(-18.3021297263188,56.1268025454853,
40.0937279956087));
#194512=CARTESIAN_POINT('Ctrl Pts',(-18.2983254984037,56.12694160832,40.0947220371804));
#194513=CARTESIAN_POINT('Ctrl Pts',(-18.2945030089052,56.1272115877756,
40.0956014538692));
#194514=CARTESIAN_POINT('Ctrl Pts',(-18.2879833547329,56.127672065871,40.097101390674));
#194515=CARTESIAN_POINT('Ctrl Pts',(-18.2814124323569,56.1285150529072,
40.0982667904316));
#194516=CARTESIAN_POINT('Ctrl Pts',(-18.2748585331707,56.1297657127884,
40.0990539325582));
#194517=CARTESIAN_POINT('Ctrl Pts',(-18.2715815835777,56.130391042729,40.0994475036216));
#194518=CARTESIAN_POINT('Ctrl Pts',(-18.2683092720861,56.1311196862925,
40.0997467259952));
#194519=CARTESIAN_POINT('Ctrl Pts',(-18.2650501911668,56.1319548233208,
40.0999473488896));
#194520=CARTESIAN_POINT('Ctrl Pts',(-18.2617911102475,56.1327899603492,
40.100147971784));
#194521=CARTESIAN_POINT('Ctrl Pts',(-18.258545294751,56.133731561341,40.10025));
#194522=CARTESIAN_POINT('Ctrl Pts',(-18.2553202812744,56.1347810195644,
40.10025));
#194523=CARTESIAN_POINT('Origin',(-12.0988124084934,56.9937374973464,39.92499));
#194524=CARTESIAN_POINT('Ctrl Pts',(-12.8407372733092,61.3271735965895,
39.92499));
#194525=CARTESIAN_POINT('Ctrl Pts',(-12.8429432848607,61.3375520649564,
39.9348354642016));
#194526=CARTESIAN_POINT('Ctrl Pts',(-12.8459616464938,61.3477256769088,
39.9446440828454));
#194527=CARTESIAN_POINT('Ctrl Pts',(-12.8497656413956,61.3576417279032,
39.9543641760326));
#194528=CARTESIAN_POINT('Ctrl Pts',(-12.8534460291144,61.3672355662866,
39.9637684240707));
#194529=CARTESIAN_POINT('Ctrl Pts',(-12.8578623484989,61.3765894879238,
39.973090963639));
#194530=CARTESIAN_POINT('Ctrl Pts',(-12.8630345798913,61.3856422574863,
39.9822808977135));
#194531=CARTESIAN_POINT('Ctrl Pts',(-12.8679271923008,61.394205620055,39.9909740094644));
#194532=CARTESIAN_POINT('Ctrl Pts',(-12.8734966517555,61.4025003187116,
39.9995492764996));
#194533=CARTESIAN_POINT('Ctrl Pts',(-12.8797929832517,61.4104485116936,
40.0079462328689));
#194534=CARTESIAN_POINT('Ctrl Pts',(-12.885592359922,61.417769372258,40.0156804369685));
#194535=CARTESIAN_POINT('Ctrl Pts',(-12.8920087864949,61.4247966697187,
40.0232638017417));
#194536=CARTESIAN_POINT('Ctrl Pts',(-12.8991043342871,61.4314390014606,
40.0306257269962));
#194537=CARTESIAN_POINT('Ctrl Pts',(-12.9011624829797,61.4333656894051,
40.0327611416649));
#194538=CARTESIAN_POINT('Ctrl Pts',(-12.9032779088707,61.4352597571379,
40.0348777427269));
#194539=CARTESIAN_POINT('Ctrl Pts',(-12.9054524645838,61.437118361331,40.0369733168701));
#194540=CARTESIAN_POINT('Ctrl Pts',(-12.9078098227877,61.4391332077733,
40.039245053974));
#194541=CARTESIAN_POINT('Ctrl Pts',(-12.9102326900442,61.4411043938524,
40.041487875195));
#194542=CARTESIAN_POINT('Ctrl Pts',(-12.9127224163023,61.4430281531013,
40.0436985701601));
#194543=CARTESIAN_POINT('Ctrl Pts',(-12.9195554895539,61.4483079254551,
40.0497658398386));
#194544=CARTESIAN_POINT('Ctrl Pts',(-12.9269097705825,61.4531896374537,
40.0555581699984));
#194545=CARTESIAN_POINT('Ctrl Pts',(-12.9347398820024,61.4575800373534,
40.0609828468885));
#194546=CARTESIAN_POINT('Ctrl Pts',(-12.941904008845,61.4615970149014,40.0659461317305));
#194547=CARTESIAN_POINT('Ctrl Pts',(-12.9494643722281,61.4651913207948,
40.0706039980708));
#194548=CARTESIAN_POINT('Ctrl Pts',(-12.9574154517104,61.4682744840804,
40.0748843180605));
#194549=CARTESIAN_POINT('Ctrl Pts',(-12.9613209959786,61.4697889238147,
40.0769867972571));
#194550=CARTESIAN_POINT('Ctrl Pts',(-12.9653208118549,61.4711795284101,
40.0789976708175));
#194551=CARTESIAN_POINT('Ctrl Pts',(-12.9694138336344,61.4724324898305,
40.08090504915));
#194552=CARTESIAN_POINT('Ctrl Pts',(-12.9701904446506,61.472670227056,40.0812669556105));
#194553=CARTESIAN_POINT('Ctrl Pts',(-12.9709708853386,61.4729027677275,
40.0816253922033));
#194554=CARTESIAN_POINT('Ctrl Pts',(-12.9717550556842,61.4731300138563,
40.0819801989139));
#194555=CARTESIAN_POINT('Ctrl Pts',(-12.9725147207064,61.4733501585436,
40.0823239179149));
#194556=CARTESIAN_POINT('Ctrl Pts',(-12.9732778859002,61.4735653344326,
40.0826642303498));
#194557=CARTESIAN_POINT('Ctrl Pts',(-12.974044456583,61.4737754532575,40.0830009916099));
#194558=CARTESIAN_POINT('Ctrl Pts',(-12.9823983859291,61.4760652849147,
40.0866709464312));
#194559=CARTESIAN_POINT('Ctrl Pts',(-12.9911623597373,61.4777556486131,
40.0899175831877));
#194560=CARTESIAN_POINT('Ctrl Pts',(-13.0001833616592,61.4787331403171,
40.0925642067061));
#194561=CARTESIAN_POINT('Ctrl Pts',(-13.0039929867887,61.4791459411336,
40.0936818922527));
#194562=CARTESIAN_POINT('Ctrl Pts',(-13.007848166856,61.4794319383913,40.094693009479));
#194563=CARTESIAN_POINT('Ctrl Pts',(-13.0117365408425,61.4795843394719,
40.0955863397546));
#194564=CARTESIAN_POINT('Ctrl Pts',(-13.0182844654758,61.4798409790836,
40.0970906856166));
#194565=CARTESIAN_POINT('Ctrl Pts',(-13.024924823017,61.4797168922659,40.0982599215483));
#194566=CARTESIAN_POINT('Ctrl Pts',(-13.0315916763171,61.4791780149468,
40.0990497370453));
#194567=CARTESIAN_POINT('Ctrl Pts',(-13.0332583896422,61.479043295617,40.0992471909196));
#194568=CARTESIAN_POINT('Ctrl Pts',(-13.0349267248711,61.4788824204062,
40.0994209989363));
#194569=CARTESIAN_POINT('Ctrl Pts',(-13.0365955947398,61.478694553895,40.0995705982975));
#194570=CARTESIAN_POINT('Ctrl Pts',(-13.0390988995429,61.4784127541283,
40.0997949973393));
#194571=CARTESIAN_POINT('Ctrl Pts',(-13.0416033892095,61.4780702140293,
40.0999649129781));
#194572=CARTESIAN_POINT('Ctrl Pts',(-13.0441057251024,61.4776657592308,
40.1000786629733));
#194573=CARTESIAN_POINT('Ctrl Pts',(-13.0466080609952,61.4772613044322,
40.1001924129685));
#194574=CARTESIAN_POINT('Ctrl Pts',(-13.0491082380622,61.4767949453823,
40.10025));
#194575=CARTESIAN_POINT('Ctrl Pts',(-13.0516031943522,61.4762657165317,
40.10025));
#194576=CARTESIAN_POINT('Ctrl Pts',(-12.2578193919762,57.7418065394567,
40.10025));
#194577=CARTESIAN_POINT('Ctrl Pts',(-12.2493771807071,57.7435970583545,
40.10025));
#194578=CARTESIAN_POINT('Ctrl Pts',(-12.2411559442244,57.7460689269802,
40.0995786334241));
#194579=CARTESIAN_POINT('Ctrl Pts',(-12.2332613533225,57.7491141258103,
40.0983063763367));
#194580=CARTESIAN_POINT('Ctrl Pts',(-12.2281622576314,57.7510810117992,
40.0974846287993));
#194581=CARTESIAN_POINT('Ctrl Pts',(-12.223199086688,57.7532862127605,40.0964130309338));
#194582=CARTESIAN_POINT('Ctrl Pts',(-12.2183955094113,57.755693185958,40.0951176960924));
#194583=CARTESIAN_POINT('Ctrl Pts',(-12.2120286428972,57.7588834910513,
40.0934008039614));
#194584=CARTESIAN_POINT('Ctrl Pts',(-12.2059457447512,57.7624328173676,
40.0912909372156));
#194585=CARTESIAN_POINT('Ctrl Pts',(-12.2001996238495,57.766268204371,40.0888630467851));
#194586=CARTESIAN_POINT('Ctrl Pts',(-12.1973265633987,57.7681858978727,
40.0876491015699));
#194587=CARTESIAN_POINT('Ctrl Pts',(-12.1945375019633,57.7701751462711,
40.0863558569271));
#194588=CARTESIAN_POINT('Ctrl Pts',(-12.1918376559068,57.7722271161469,
40.0849936342771));
#194589=CARTESIAN_POINT('Ctrl Pts',(-12.1904877328785,57.7732531010848,
40.0843125229521));
#194590=CARTESIAN_POINT('Ctrl Pts',(-12.1891600976129,57.7742947697604,
40.0836141747074));
#194591=CARTESIAN_POINT('Ctrl Pts',(-12.1878553011592,57.7753510390206,
40.082899916161));
#194592=CARTESIAN_POINT('Ctrl Pts',(-12.1875291020458,57.7756151063356,
40.0827213515243));
#194593=CARTESIAN_POINT('Ctrl Pts',(-12.1872043300158,57.7758800862578,
40.0825417925842));
#194594=CARTESIAN_POINT('Ctrl Pts',(-12.1868809929892,57.776145962005,40.0823612602361));
#194595=CARTESIAN_POINT('Ctrl Pts',(-12.1859109819092,57.7769435892466,
40.0818196631917));
#194596=CARTESIAN_POINT('Ctrl Pts',(-12.1849538875684,57.7777492785675,
40.0812693052022));
#194597=CARTESIAN_POINT('Ctrl Pts',(-12.1840099085252,57.7785625799463,
40.0807107531875));
#194598=CARTESIAN_POINT('Ctrl Pts',(-12.1773606420345,57.7842913698424,
40.0767763849183));
#194599=CARTESIAN_POINT('Ctrl Pts',(-12.1713100228961,57.7903843352497,
40.0724140586139));
#194600=CARTESIAN_POINT('Ctrl Pts',(-12.1658251565855,57.7967264334405,
40.0677221223771));
#194601=CARTESIAN_POINT('Ctrl Pts',(-12.1631650023517,57.7998023442099,
40.0654465383722));
#194602=CARTESIAN_POINT('Ctrl Pts',(-12.1606380046008,57.8029374300325,
40.063092800068));
#194603=CARTESIAN_POINT('Ctrl Pts',(-12.1582411305893,57.806121336008,40.0606689262479));
#194604=CARTESIAN_POINT('Ctrl Pts',(-12.1545716839425,57.8109956736034,
40.0569581447805));
#194605=CARTESIAN_POINT('Ctrl Pts',(-12.1512083732202,57.8159810988991,
40.0530843804605));
#194606=CARTESIAN_POINT('Ctrl Pts',(-12.1481495009381,57.8210315314442,
40.0490800251457));
#194607=CARTESIAN_POINT('Ctrl Pts',(-12.1467289448258,57.8233769784456,
40.0472203818217));
#194608=CARTESIAN_POINT('Ctrl Pts',(-12.145373884298,57.8257362497573,40.0453323608818));
#194609=CARTESIAN_POINT('Ctrl Pts',(-12.1440853170064,57.8281051246149,
40.0434201572162));
#194610=CARTESIAN_POINT('Ctrl Pts',(-12.1439865534007,57.8282866895389,
40.0432735943397));
#194611=CARTESIAN_POINT('Ctrl Pts',(-12.1438881466791,57.82846830734,40.0431268995707));
#194612=CARTESIAN_POINT('Ctrl Pts',(-12.1437900963016,57.8286499766612,
40.0429800745037));
#194613=CARTESIAN_POINT('Ctrl Pts',(-12.1424127841092,57.831201882908,40.0409176249753));
#194614=CARTESIAN_POINT('Ctrl Pts',(-12.1411075562949,57.8337650648328,
40.0388310783332));
#194615=CARTESIAN_POINT('Ctrl Pts',(-12.1398727334215,57.8363340693142,
40.036725739981));
#194616=CARTESIAN_POINT('Ctrl Pts',(-12.1354448782034,57.8455460625021,
40.0291763710718));
#194617=CARTESIAN_POINT('Ctrl Pts',(-12.1318862976808,57.8549032874803,
40.0213310894597));
#194618=CARTESIAN_POINT('Ctrl Pts',(-12.129096878378,57.8643241951533,40.0132837551323));
#194619=CARTESIAN_POINT('Ctrl Pts',(-12.1260315867862,57.8746768262719,
40.0044405431329));
#194620=CARTESIAN_POINT('Ctrl Pts',(-12.1238947812338,57.8851069357363,
39.9953528710605));
#194621=CARTESIAN_POINT('Ctrl Pts',(-12.1225979458245,57.8955352825126,
39.9861103629561));
#194622=CARTESIAN_POINT('Ctrl Pts',(-12.1211976890436,57.9067952798732,
39.9761307737561));
#194623=CARTESIAN_POINT('Ctrl Pts',(-12.1207764137882,57.9180543443226,
39.9659696936017));
#194624=CARTESIAN_POINT('Ctrl Pts',(-12.1212770948334,57.9292311407264,
39.9557128217511));
#194625=CARTESIAN_POINT('Ctrl Pts',(-12.121773575679,57.9403141752926,39.9455419945164));
#194626=CARTESIAN_POINT('Ctrl Pts',(-12.1231769533531,57.9513177099568,
39.9352756289342));
#194627=CARTESIAN_POINT('Ctrl Pts',(-12.1254815933786,57.9621601888122,
39.92499));
#194628=CARTESIAN_POINT('Origin',(-0.0149069694351764,-0.00316857416806799,
39.92499));
#194629=CARTESIAN_POINT('Ctrl Pts',(-13.0814171332226,61.4699285681956,
40.10025));
#194630=CARTESIAN_POINT('Ctrl Pts',(-13.089817630984,61.468139314985,40.10025));
#194631=CARTESIAN_POINT('Ctrl Pts',(-13.0979940118833,61.4656642256292,
40.0995859581842));
#194632=CARTESIAN_POINT('Ctrl Pts',(-13.1058430982598,61.4626133761162,
40.098327595962));
#194633=CARTESIAN_POINT('Ctrl Pts',(-13.1108582907966,61.4606640285138,
40.0975235624068));
#194634=CARTESIAN_POINT('Ctrl Pts',(-13.1157402208606,61.4584804838816,
40.096477705949));
#194635=CARTESIAN_POINT('Ctrl Pts',(-13.1204666715201,61.4560986543957,
40.0952149915961));
#194636=CARTESIAN_POINT('Ctrl Pts',(-13.1269173283,61.4528479350654,40.0934916398701));
#194637=CARTESIAN_POINT('Ctrl Pts',(-13.1330744924,61.4492231901485,40.091364392163));
#194638=CARTESIAN_POINT('Ctrl Pts',(-13.1388835356731,61.4453029499362,
40.0889118607713));
#194639=CARTESIAN_POINT('Ctrl Pts',(-13.1417880573096,61.4433428298301,
40.0876855950754));
#194640=CARTESIAN_POINT('Ctrl Pts',(-13.1446057534055,61.4413087943565,
40.0863782327526));
#194641=CARTESIAN_POINT('Ctrl Pts',(-13.1473312571586,61.4392103574,40.0850006373334));
#194642=CARTESIAN_POINT('Ctrl Pts',(-13.1486940090351,61.4381611389218,
40.0843118396237));
#194643=CARTESIAN_POINT('Ctrl Pts',(-13.1500337298697,61.4370958165018,
40.0836054919164));
#194644=CARTESIAN_POINT('Ctrl Pts',(-13.1513498559436,61.4360155570619,
40.0828829920417));
#194645=CARTESIAN_POINT('Ctrl Pts',(-13.1516788874621,61.435745492202,40.0827023670731));
#194646=CARTESIAN_POINT('Ctrl Pts',(-13.1520064446714,61.4354744937032,
40.0825207326933));
#194647=CARTESIAN_POINT('Ctrl Pts',(-13.1523325194961,61.4352025796479,
40.0823381109275));
#194648=CARTESIAN_POINT('Ctrl Pts',(-13.1533107439705,61.4343868374821,
40.0817902456303));
#194649=CARTESIAN_POINT('Ctrl Pts',(-13.1542756251691,61.4335628556743,
40.0812334935553));
#194650=CARTESIAN_POINT('Ctrl Pts',(-13.1552269612797,61.4327311191548,
40.0806684524227));
#194651=CARTESIAN_POINT('Ctrl Pts',(-13.1618012840655,61.4269833037496,
40.0767636676137));
#194652=CARTESIAN_POINT('Ctrl Pts',(-13.167782951603,61.4208780249712,40.0724404510888));
#194653=CARTESIAN_POINT('Ctrl Pts',(-13.1732071947989,61.4145287289054,
40.0677949937409));
#194654=CARTESIAN_POINT('Ctrl Pts',(-13.1759030287779,61.4113731461892,
40.0654862141906));
#194655=CARTESIAN_POINT('Ctrl Pts',(-13.1784610805509,61.4081566864226,
40.0630972003216));
#194656=CARTESIAN_POINT('Ctrl Pts',(-13.180884815382,61.4048902384027,40.0606363359906));
#194657=CARTESIAN_POINT('Ctrl Pts',(-13.1862319364376,61.3976839661819,
40.0552073017123));
#194658=CARTESIAN_POINT('Ctrl Pts',(-13.1909347237338,61.3902425685153,
40.0494204304519));
#194659=CARTESIAN_POINT('Ctrl Pts',(-13.1949697809163,61.3827095020467,
40.0434049749851));
#194660=CARTESIAN_POINT('Ctrl Pts',(-13.1964438381899,61.3799575778687,
40.0412074532442));
#194661=CARTESIAN_POINT('Ctrl Pts',(-13.1978367193485,61.377194044862,40.0389814735788));
#194662=CARTESIAN_POINT('Ctrl Pts',(-13.1991508816432,61.3744236152739,
40.0367321210017));
#194663=CARTESIAN_POINT('Ctrl Pts',(-13.203565013731,61.365118035445,40.029176783714));
#194664=CARTESIAN_POINT('Ctrl Pts',(-13.2071113921934,61.355672040405,40.0213235332573));
#194665=CARTESIAN_POINT('Ctrl Pts',(-13.209889088817,61.3461671566355,40.0132649215854));
#194666=CARTESIAN_POINT('Ctrl Pts',(-13.2129421064461,61.3357201634454,
40.0044075527526));
#194667=CARTESIAN_POINT('Ctrl Pts',(-13.2150668515152,61.3252014297026,
39.9953016253711));
#194668=CARTESIAN_POINT('Ctrl Pts',(-13.2163502251974,61.3146904872798,
39.9860353422348));
#194669=CARTESIAN_POINT('Ctrl Pts',(-13.2177324736412,61.3033697519324,
39.9760551582683));
#194670=CARTESIAN_POINT('Ctrl Pts',(-13.2181390006407,61.2920568939702,
39.9658879738142));
#194671=CARTESIAN_POINT('Ctrl Pts',(-13.2176240288381,61.2808338148841,
39.955617464324));
#194672=CARTESIAN_POINT('Ctrl Pts',(-13.2171160108937,61.2697622852597,
39.9454856413894));
#194673=CARTESIAN_POINT('Ctrl Pts',(-13.2157108393285,61.2587767401948,
39.9352519465108));
#194674=CARTESIAN_POINT('Ctrl Pts',(-13.2134115091888,61.2479592423879,
39.92499));
#194675=CARTESIAN_POINT('Ctrl Pts',(-12.4981558292581,57.8829458346106,
39.92499));
#194676=CARTESIAN_POINT('Ctrl Pts',(-12.4959553576922,57.8725934298266,
39.9348107241725));
#194677=CARTESIAN_POINT('Ctrl Pts',(-12.4929462655996,57.8624518082032,
39.9446038383175));
#194678=CARTESIAN_POINT('Ctrl Pts',(-12.4891531124815,57.8525735736558,
39.9543158069393));
#194679=CARTESIAN_POINT('Ctrl Pts',(-12.4854904894097,57.8430352690751,
39.9636935671401));
#194680=CARTESIAN_POINT('Ctrl Pts',(-12.4810963130876,57.8337413853103,
39.9729968320998));
#194681=CARTESIAN_POINT('Ctrl Pts',(-12.4759491415381,57.8247536185201,
39.9821731151346));
#194682=CARTESIAN_POINT('Ctrl Pts',(-12.4710834524297,57.8162573641093,
39.9908475764361));
#194683=CARTESIAN_POINT('Ctrl Pts',(-12.4655444244719,57.808033877166,39.9994093733854));
#194684=CARTESIAN_POINT('Ctrl Pts',(-12.4592813303326,57.8001616710168,
40.0077966115849));
#194685=CARTESIAN_POINT('Ctrl Pts',(-12.4535131257017,57.7929115012196,
40.01552111726));
#194686=CARTESIAN_POINT('Ctrl Pts',(-12.4471303774504,57.785958901908,40.0230979941024));
#194687=CARTESIAN_POINT('Ctrl Pts',(-12.4400707994989,57.7793958734419,
40.0304554104748));
#194688=CARTESIAN_POINT('Ctrl Pts',(-12.4379657758605,57.7774389108365,
40.0326492435181));
#194689=CARTESIAN_POINT('Ctrl Pts',(-12.435800430645,57.7755168276795,40.034823371506));
#194690=CARTESIAN_POINT('Ctrl Pts',(-12.4335727482756,57.7736327324861,
40.0369753512355));
#194691=CARTESIAN_POINT('Ctrl Pts',(-12.4313678273305,57.7717678881029,
40.0391053430352));
#194692=CARTESIAN_POINT('Ctrl Pts',(-12.4291043014743,57.7699419852107,
40.0412110893239));
#194693=CARTESIAN_POINT('Ctrl Pts',(-12.4267829461793,57.7681599326869,
40.0432881154903));
#194694=CARTESIAN_POINT('Ctrl Pts',(-12.4266215236719,57.7680360122395,
40.0434325478279));
#194695=CARTESIAN_POINT('Ctrl Pts',(-12.426459823689,57.7679122920636,40.0435768364421));
#194696=CARTESIAN_POINT('Ctrl Pts',(-12.4262978456302,57.767788773317,40.0437209807855));
#194697=CARTESIAN_POINT('Ctrl Pts',(-12.4191961341593,57.762373258983,40.0500407968421));
#194698=CARTESIAN_POINT('Ctrl Pts',(-12.4115418213381,57.7573864007557,
40.0560490279346));
#194699=CARTESIAN_POINT('Ctrl Pts',(-12.4033632485678,57.7529408672213,
40.0616647108617));
#194700=CARTESIAN_POINT('Ctrl Pts',(-12.3957393973196,57.7487968573387,
40.0668995033488));
#194701=CARTESIAN_POINT('Ctrl Pts',(-12.3876591848384,57.7451230952908,
40.0717933267485));
#194702=CARTESIAN_POINT('Ctrl Pts',(-12.3791488184475,57.7420400166292,
40.0762460303076));
#194703=CARTESIAN_POINT('Ctrl Pts',(-12.3760356163213,57.7409121865684,
40.077874886875));
#194704=CARTESIAN_POINT('Ctrl Pts',(-12.3728649408019,57.7398637084259,
40.0794443522249));
#194705=CARTESIAN_POINT('Ctrl Pts',(-12.3696384996592,57.7389016204183,
40.0809482021492));
#194706=CARTESIAN_POINT('Ctrl Pts',(-12.3688626483502,57.738670270393,40.0813098278168));
#194707=CARTESIAN_POINT('Ctrl Pts',(-12.3680830188491,57.7384441015869,
40.0816679525672));
#194708=CARTESIAN_POINT('Ctrl Pts',(-12.3672997100616,57.7382232068822,
40.082022419258));
#194709=CARTESIAN_POINT('Ctrl Pts',(-12.3665408796737,57.7380092151371,
40.0823658088648));
#194710=CARTESIAN_POINT('Ctrl Pts',(-12.3657785963861,57.7378001730066,
40.0827057654617));
#194711=CARTESIAN_POINT('Ctrl Pts',(-12.365012953822,57.737596164125,40.0830421470151));
#194712=CARTESIAN_POINT('Ctrl Pts',(-12.3566244546988,57.7353610110591,
40.0867275956806));
#194713=CARTESIAN_POINT('Ctrl Pts',(-12.3478270988448,57.7337289586985,
40.0899823432031));
#194714=CARTESIAN_POINT('Ctrl Pts',(-12.338774647773,57.7328090548568,40.0926299529356));
#194715=CARTESIAN_POINT('Ctrl Pts',(-12.335020326489,57.7324275433143,40.0937279956085));
#194716=CARTESIAN_POINT('Ctrl Pts',(-12.3312224025075,57.7321681942503,
40.0947220371803));
#194717=CARTESIAN_POINT('Ctrl Pts',(-12.3273926324683,57.7320371357771,
40.0956014538692));
#194718=CARTESIAN_POINT('Ctrl Pts',(-12.320860560576,57.7318136018936,40.097101390674));
#194719=CARTESIAN_POINT('Ctrl Pts',(-12.3142375182609,57.7319651225404,
40.0982667904316));
#194720=CARTESIAN_POINT('Ctrl Pts',(-12.3075887924648,57.7325238621659,
40.0990539325582));
#194721=CARTESIAN_POINT('Ctrl Pts',(-12.3042644295668,57.7328032319787,
40.0994475036216));
#194722=CARTESIAN_POINT('Ctrl Pts',(-12.300933880148,57.7331858342648,40.0997467259952));
#194723=CARTESIAN_POINT('Ctrl Pts',(-12.2976053572248,57.7336757296049,
40.0999473488896));
#194724=CARTESIAN_POINT('Ctrl Pts',(-12.2942768343016,57.734165624945,40.100147971784));
#194725=CARTESIAN_POINT('Ctrl Pts',(-12.2909503756172,57.7347627876419,
40.10025));
#194726=CARTESIAN_POINT('Ctrl Pts',(-12.2876333308465,57.7354693911206,
40.10025));
#194727=CARTESIAN_POINT('Origin',(-6.07506605172241,57.9461901084062,39.92499));
#194728=CARTESIAN_POINT('Ctrl Pts',(-6.35995915837738,62.333439457262,39.92499));
#194729=CARTESIAN_POINT('Ctrl Pts',(-6.36106823981726,62.3439916622903,
39.9348354642018));
#194730=CARTESIAN_POINT('Ctrl Pts',(-6.3630066345263,62.3544250468349,39.9446440828457));
#194731=CARTESIAN_POINT('Ctrl Pts',(-6.36575328117383,62.3646844024057,
39.9543641760329));
#194732=CARTESIAN_POINT('Ctrl Pts',(-6.36841067816053,62.3746103900109,
39.9637684240709));
#194733=CARTESIAN_POINT('Ctrl Pts',(-6.37182505343099,62.3843747009652,
39.9730909636391));
#194734=CARTESIAN_POINT('Ctrl Pts',(-6.37602267870792,62.393918523908,39.9822808977135));
#194735=CARTESIAN_POINT('Ctrl Pts',(-6.37999337374501,62.402946392737,39.9909740094642));
#194736=CARTESIAN_POINT('Ctrl Pts',(-6.38466529101406,62.4117778192045,
39.9995492764992));
#194737=CARTESIAN_POINT('Ctrl Pts',(-6.39009631814929,62.4203406170093,
40.0079462328684));
#194738=CARTESIAN_POINT('Ctrl Pts',(-6.39509868692269,62.4282275730647,
40.0156804369677));
#194739=CARTESIAN_POINT('Ctrl Pts',(-6.40074541103475,62.4358870734638,
40.0232638017408));
#194740=CARTESIAN_POINT('Ctrl Pts',(-6.40710777594406,62.4432347045242,
40.0306257269951));
#194741=CARTESIAN_POINT('Ctrl Pts',(-6.40895325615309,62.4453659729909,
40.0327611416641));
#194742=CARTESIAN_POINT('Ctrl Pts',(-6.41085910953059,62.4474707870404,
40.0348777427266));
#194743=CARTESIAN_POINT('Ctrl Pts',(-6.41282747576019,62.4495465125725,
40.0369733168701));
#194744=CARTESIAN_POINT('Ctrl Pts',(-6.41496131130683,62.4517967325057,
40.039245053974));
#194745=CARTESIAN_POINT('Ctrl Pts',(-6.41716486079138,62.4540103788122,
40.041487875195));
#194746=CARTESIAN_POINT('Ctrl Pts',(-6.41943986047048,62.4561838467663,
40.0436985701601));
#194747=CARTESIAN_POINT('Ctrl Pts',(-6.42568361494137,62.4621489466211,
40.0497658398386));
#194748=CARTESIAN_POINT('Ctrl Pts',(-6.43248733059572,62.467772647785,40.0555581699984));
#194749=CARTESIAN_POINT('Ctrl Pts',(-6.4398156260913,62.4729574661286,40.0609828468886));
#194750=CARTESIAN_POINT('Ctrl Pts',(-6.44652061860732,62.4777012934227,
40.0659461317305));
#194751=CARTESIAN_POINT('Ctrl Pts',(-6.45366385825704,62.4820661824985,
40.0706039980706));
#194752=CARTESIAN_POINT('Ctrl Pts',(-6.46124910257362,62.4859635700126,
40.0748843180603));
#194753=CARTESIAN_POINT('Ctrl Pts',(-6.46497494980365,62.4878779540282,
40.076986797257));
#194754=CARTESIAN_POINT('Ctrl Pts',(-6.46880749650881,62.4896790353531,
40.0789976708175));
#194755=CARTESIAN_POINT('Ctrl Pts',(-6.47274712615508,62.4913529701965,
40.08090504915));
#194756=CARTESIAN_POINT('Ctrl Pts',(-6.47349463250796,62.4916705830287,
40.0812669556105));
#194757=CARTESIAN_POINT('Ctrl Pts',(-6.47424649074124,62.4919834280839,
40.0816253922033));
#194758=CARTESIAN_POINT('Ctrl Pts',(-6.47500261163096,62.4922913974558,
40.0819801989139));
#194759=CARTESIAN_POINT('Ctrl Pts',(-6.47573510374288,62.4925897427848,
40.0823239179149));
#194760=CARTESIAN_POINT('Ctrl Pts',(-6.47647159623284,62.4928835124027,
40.0826642303499));
#194761=CARTESIAN_POINT('Ctrl Pts',(-6.47721200416343,62.4931726086301,
40.08300099161));
#194762=CARTESIAN_POINT('Ctrl Pts',(-6.4852808172262,62.4963231197467,40.0866709464312));
#194763=CARTESIAN_POINT('Ctrl Pts',(-6.49382008994911,62.4989203081703,
40.0899175831877));
#194764=CARTESIAN_POINT('Ctrl Pts',(-6.50268949817301,62.5008353965404,
40.0925642067061));
#194765=CARTESIAN_POINT('Ctrl Pts',(-6.50643510434242,62.5016441502512,
40.0936818922527));
#194766=CARTESIAN_POINT('Ctrl Pts',(-6.51023927047603,62.502331556834,40.094693009479));
#194767=CARTESIAN_POINT('Ctrl Pts',(-6.51409041329226,62.502889568803,40.0955863397546));
#194768=CARTESIAN_POINT('Ctrl Pts',(-6.52057564156509,62.5038292470156,
40.0970906856166));
#194769=CARTESIAN_POINT('Ctrl Pts',(-6.52719259313719,62.5043999463278,
40.0982599215483));
#194770=CARTESIAN_POINT('Ctrl Pts',(-6.53387925273545,62.5045608969649,
40.0990497370454));
#194771=CARTESIAN_POINT('Ctrl Pts',(-6.53555091763502,62.5046011346242,
40.0992471909196));
#194772=CARTESIAN_POINT('Ctrl Pts',(-6.53722692958755,62.5046155292223,
40.0994209989363));
#194773=CARTESIAN_POINT('Ctrl Pts',(-6.53890629461021,62.5046031362664,
40.0995705982975));
#194774=CARTESIAN_POINT('Ctrl Pts',(-6.54142534214421,62.5045845468324,
40.0997949973393));
#194775=CARTESIAN_POINT('Ctrl Pts',(-6.54395191714455,62.5045056736602,
40.0999649129781));
#194776=CARTESIAN_POINT('Ctrl Pts',(-6.54648282201812,62.5043649998329,
40.1000786629733));
#194777=CARTESIAN_POINT('Ctrl Pts',(-6.5490137268917,62.5042243260056,40.1001924129685));
#194778=CARTESIAN_POINT('Ctrl Pts',(-6.55154895552196,62.5040218613862,
40.10025));
#194779=CARTESIAN_POINT('Ctrl Pts',(-6.55408556365883,62.5037563256535,
40.10025));
#194780=CARTESIAN_POINT('Ctrl Pts',(-6.15500747092256,58.7067819056643,
40.10025));
#194781=CARTESIAN_POINT('Ctrl Pts',(-6.14642434678091,58.7076801645418,
40.10025));
#194782=CARTESIAN_POINT('Ctrl Pts',(-6.13798976646259,58.7092791387969,
40.099578633424));
#194783=CARTESIAN_POINT('Ctrl Pts',(-6.12982011300122,58.7114824462543,
40.0983063763365));
#194784=CARTESIAN_POINT('Ctrl Pts',(-6.12454335512051,58.7129055567992,
40.0974846287991));
#194785=CARTESIAN_POINT('Ctrl Pts',(-6.11937686667958,58.7145798848071,
40.0964130309337));
#194786=CARTESIAN_POINT('Ctrl Pts',(-6.11434800669275,58.7164715618025,
40.0951176960924));
#194787=CARTESIAN_POINT('Ctrl Pts',(-6.10768254085074,58.7189788712981,
40.0934008039614));
#194788=CARTESIAN_POINT('Ctrl Pts',(-6.10126195983181,58.7218729180382,
40.0912909372156));
#194789=CARTESIAN_POINT('Ctrl Pts',(-6.09514640967214,58.7250866612027,
40.0888630467851));
#194790=CARTESIAN_POINT('Ctrl Pts',(-6.0920886345923,58.7266935327849,40.0876491015699));
#194791=CARTESIAN_POINT('Ctrl Pts',(-6.08910691884912,58.7283803475666,
40.0863558569271));
#194792=CARTESIAN_POINT('Ctrl Pts',(-6.08620737357405,58.7301388657774,
40.0849936342771));
#194793=CARTESIAN_POINT('Ctrl Pts',(-6.08475760093651,58.7310181248828,
40.0843125229521));
#194794=CARTESIAN_POINT('Ctrl Pts',(-6.08332835456984,58.7319153115143,
40.0836141747074));
#194795=CARTESIAN_POINT('Ctrl Pts',(-6.08192029572511,58.7328294060528,
40.0828999161609));
#194796=CARTESIAN_POINT('Ctrl Pts',(-6.08156828101392,58.7330579296874,
40.0827213515243));
#194797=CARTESIAN_POINT('Ctrl Pts',(-6.08121759017508,58.7332875101007,
40.0825417925842));
#194798=CARTESIAN_POINT('Ctrl Pts',(-6.08086823283921,58.7335181314302,
40.0823612602361));
#194799=CARTESIAN_POINT('Ctrl Pts',(-6.07982016083159,58.7342099954187,
40.0818196631917));
#194800=CARTESIAN_POINT('Ctrl Pts',(-6.07878409208717,58.7349112274886,
40.0812693052021));
#194801=CARTESIAN_POINT('Ctrl Pts',(-6.07776027111658,58.7356214008386,
40.0807107531875));
#194802=CARTESIAN_POINT('Ctrl Pts',(-6.07054860839909,58.7406237702162,
40.0767763849182));
#194803=CARTESIAN_POINT('Ctrl Pts',(-6.06389424687459,58.7460508958012,
40.0724140586137));
#194804=CARTESIAN_POINT('Ctrl Pts',(-6.05777649745766,58.751784926668,40.0677221223768));
#194805=CARTESIAN_POINT('Ctrl Pts',(-6.05480939560134,58.7545659254421,
40.0654465383721));
#194806=CARTESIAN_POINT('Ctrl Pts',(-6.05196853530533,58.7574196937449,
40.0630928000679));
#194807=CARTESIAN_POINT('Ctrl Pts',(-6.04925198282172,58.7603356163932,
40.0606689262479));
#194808=CARTESIAN_POINT('Ctrl Pts',(-6.04509313076933,58.7647996902381,
40.0569581447806));
#194809=CARTESIAN_POINT('Ctrl Pts',(-6.04122712577018,58.7694062431512,
40.0530843804606));
#194810=CARTESIAN_POINT('Ctrl Pts',(-6.03765709635775,58.7741092696794,
40.0490800251458));
#194811=CARTESIAN_POINT('Ctrl Pts',(-6.03599915622974,58.7762933795293,
40.0472203818218));
#194812=CARTESIAN_POINT('Ctrl Pts',(-6.03440490786063,58.7784980841112,
40.0453323608819));
#194813=CARTESIAN_POINT('Ctrl Pts',(-6.03287578462697,58.7807192900658,
40.0434201572162));
#194814=CARTESIAN_POINT('Ctrl Pts',(-6.03275858335616,58.7808895367502,
40.0432735943397));
#194815=CARTESIAN_POINT('Ctrl Pts',(-6.03264173148719,58.7810598733266,
40.0431268995708));
#194816=CARTESIAN_POINT('Ctrl Pts',(-6.03252522862489,58.7812302983889,
40.0429800745037));
#194817=CARTESIAN_POINT('Ctrl Pts',(-6.03088871465445,58.7836242566994,
40.0409176249753));
#194818=CARTESIAN_POINT('Ctrl Pts',(-6.02932271154703,58.7860369637878,
40.0388310783332));
#194819=CARTESIAN_POINT('Ctrl Pts',(-6.02782611907197,58.7884628208564,
40.036725739981));
#194820=CARTESIAN_POINT('Ctrl Pts',(-6.02245960461632,58.7971615128805,
40.0291763710716));
#194821=CARTESIAN_POINT('Ctrl Pts',(-6.01794242202257,58.8060955050481,
40.0213310894592));
#194822=CARTESIAN_POINT('Ctrl Pts',(-6.01418353044881,58.8151732302903,
40.0132837551315));
#194823=CARTESIAN_POINT('Ctrl Pts',(-6.01005288622337,58.8251487383932,
40.0044405431318));
#194824=CARTESIAN_POINT('Ctrl Pts',(-6.00683754300133,58.8352983536264,
39.9953528710591));
#194825=CARTESIAN_POINT('Ctrl Pts',(-6.00445775272914,58.8455340166158,
39.9861103629543));
#194826=CARTESIAN_POINT('Ctrl Pts',(-6.00188817648097,58.8565859638438,
39.9761307737539));
#194827=CARTESIAN_POINT('Ctrl Pts',(-6.00029231631084,58.8677393147055,
39.9659696935989));
#194828=CARTESIAN_POINT('Ctrl Pts',(-5.99962196122069,58.8789072188699,
39.9557128217479));
#194829=CARTESIAN_POINT('Ctrl Pts',(-5.99895722972105,58.8899814357918,
39.9455419945142));
#194830=CARTESIAN_POINT('Ctrl Pts',(-5.99920273697647,58.9010713848523,
39.9352756289331));
#194831=CARTESIAN_POINT('Ctrl Pts',(-6.00036140428986,58.9120953679531,
39.92499));
#194832=CARTESIAN_POINT('Origin',(-0.0151565136854063,-0.00159301378020448,
39.92499));
#194833=CARTESIAN_POINT('Ctrl Pts',(-6.58439859102965,62.5005702980932,
40.10025));
#194834=CARTESIAN_POINT('Ctrl Pts',(-6.59294009787387,62.4996689377206,
40.10025));
#194835=CARTESIAN_POINT('Ctrl Pts',(-6.60133040498987,62.4980620716937,
40.0995859581842));
#194836=CARTESIAN_POINT('Ctrl Pts',(-6.60945539386123,62.4958483879905,
40.0983275959621));
#194837=CARTESIAN_POINT('Ctrl Pts',(-6.61464687495778,62.4944339494872,
40.0975235624068));
#194838=CARTESIAN_POINT('Ctrl Pts',(-6.61973030386294,62.4927726671883,
40.096477705949));
#194839=CARTESIAN_POINT('Ctrl Pts',(-6.62467983150713,62.4908979342377,
40.0952149915961));
#194840=CARTESIAN_POINT('Ctrl Pts',(-6.6314349436104,62.4883392999283,40.0934916398701));
#194841=CARTESIAN_POINT('Ctrl Pts',(-6.63793726713709,62.4853780106448,
40.0913643921631));
#194842=CARTESIAN_POINT('Ctrl Pts',(-6.64412426454837,62.4820864562849,
40.0889118607713));
#194843=CARTESIAN_POINT('Ctrl Pts',(-6.64721776325402,62.480440679105,40.0876855950754));
#194844=CARTESIAN_POINT('Ctrl Pts',(-6.65023263831815,62.4787123157334,
40.0863782327527));
#194845=CARTESIAN_POINT('Ctrl Pts',(-6.65316255786681,62.4769102669531,
40.0850006373334));
#194846=CARTESIAN_POINT('Ctrl Pts',(-6.65462751764114,62.4760092425629,
40.0843118396238));
#194847=CARTESIAN_POINT('Ctrl Pts',(-6.65607125586022,62.4750897950507,
40.0836054919165));
#194848=CARTESIAN_POINT('Ctrl Pts',(-6.65749308991701,62.474153026021,40.0828829920418));
#194849=CARTESIAN_POINT('Ctrl Pts',(-6.65784854843121,62.4739188337636,
40.0827023670731));
#194850=CARTESIAN_POINT('Ctrl Pts',(-6.65820263830443,62.4736835588747,
40.0825207326933));
#194851=CARTESIAN_POINT('Ctrl Pts',(-6.65855534961554,62.4734472184934,
40.0823381109276));
#194852=CARTESIAN_POINT('Ctrl Pts',(-6.65961348354888,62.4727381973496,
40.0817902456304));
#194853=CARTESIAN_POINT('Ctrl Pts',(-6.66065920857946,62.4720195869493,
40.0812334935554));
#194854=CARTESIAN_POINT('Ctrl Pts',(-6.66169227331156,62.4712918484711,
40.0806684524227));
#194855=CARTESIAN_POINT('Ctrl Pts',(-6.66883139158091,62.4662627240577,
40.0767636676136));
#194856=CARTESIAN_POINT('Ctrl Pts',(-6.67541846632655,62.4608161451506,
40.0724404510886));
#194857=CARTESIAN_POINT('Ctrl Pts',(-6.68147667711138,62.4550686189984,
40.0677949937405));
#194858=CARTESIAN_POINT('Ctrl Pts',(-6.68448759124166,62.4522121142777,
40.0654862141903));
#194859=CARTESIAN_POINT('Ctrl Pts',(-6.68736784133573,62.4492806638352,
40.0630972003214));
#194860=CARTESIAN_POINT('Ctrl Pts',(-6.69011973548547,62.4462854590369,
40.0606363359906));
#194861=CARTESIAN_POINT('Ctrl Pts',(-6.6961908250136,62.4396775898761,40.0552073017123));
#194862=CARTESIAN_POINT('Ctrl Pts',(-6.70164568781152,62.4327685320937,
40.0494204304519));
#194863=CARTESIAN_POINT('Ctrl Pts',(-6.70644606039031,62.425698510878,40.0434049749851));
#194864=CARTESIAN_POINT('Ctrl Pts',(-6.70819969702922,62.4231157429702,
40.0412074532442));
#194865=CARTESIAN_POINT('Ctrl Pts',(-6.70987381569753,62.4205129446134,
40.0389814735788));
#194866=CARTESIAN_POINT('Ctrl Pts',(-6.71147036762114,62.4178950590937,
40.0367321210016));
#194867=CARTESIAN_POINT('Ctrl Pts',(-6.71683301659055,62.4091018586491,
40.0291767837142));
#194868=CARTESIAN_POINT('Ctrl Pts',(-6.72134734296609,62.4000783072496,
40.0213235332579));
#194869=CARTESIAN_POINT('Ctrl Pts',(-6.72510335397081,62.390915840588,40.0132649215864));
#194870=CARTESIAN_POINT('Ctrl Pts',(-6.72923165499376,62.3808452043613,
40.004407552754));
#194871=CARTESIAN_POINT('Ctrl Pts',(-6.73244426756069,62.37060618968,39.9953016253729));
#194872=CARTESIAN_POINT('Ctrl Pts',(-6.7348193034465,62.3602869763789,39.986035342237));
#194873=CARTESIAN_POINT('Ctrl Pts',(-6.7373773188577,62.3491727415105,39.976055158271));
#194874=CARTESIAN_POINT('Ctrl Pts',(-6.73896413451778,62.3379643502108,
39.9658879738174));
#194875=CARTESIAN_POINT('Ctrl Pts',(-6.73962511499487,62.3267489231156,
39.9556174643277));
#194876=CARTESIAN_POINT('Ctrl Pts',(-6.74027717000387,62.3156849421523,
39.9454856413919));
#194877=CARTESIAN_POINT('Ctrl Pts',(-6.74002799825933,62.3046126966267,
39.935251946512));
#194878=CARTESIAN_POINT('Ctrl Pts',(-6.7388720005127,62.293614112757,39.92499));
#194879=CARTESIAN_POINT('Ctrl Pts',(-6.37927424642518,58.8722700234481,
39.92499));
#194880=CARTESIAN_POINT('Ctrl Pts',(-6.37816795023605,58.8617443183104,
39.9348107241716));
#194881=CARTESIAN_POINT('Ctrl Pts',(-6.37623543038835,58.85134371778,39.9446038383158));
#194882=CARTESIAN_POINT('Ctrl Pts',(-6.37349561323731,58.8411231047695,
39.9543158069367));
#194883=CARTESIAN_POINT('Ctrl Pts',(-6.37085007871821,58.8312542036586,
39.9636935671369));
#194884=CARTESIAN_POINT('Ctrl Pts',(-6.36745144954177,58.8215519162636,
39.9729968320962));
#194885=CARTESIAN_POINT('Ctrl Pts',(-6.36327195218786,58.8120753594685,
39.9821731151305));
#194886=CARTESIAN_POINT('Ctrl Pts',(-6.35932101825085,58.8031170454232,
39.990847576432));
#194887=CARTESIAN_POINT('Ctrl Pts',(-6.35467192212096,58.7943596215215,
39.9994093733811));
#194888=CARTESIAN_POINT('Ctrl Pts',(-6.34926600747837,58.7858758685357,
40.0077966115805));
#194889=CARTESIAN_POINT('Ctrl Pts',(-6.34428725078353,58.7780624743613,
40.0155211172557));
#194890=CARTESIAN_POINT('Ctrl Pts',(-6.33866621241707,58.77048078325,40.0230979940982));
#194891=CARTESIAN_POINT('Ctrl Pts',(-6.33233133085242,58.7632157809057,
40.0304554104708));
#194892=CARTESIAN_POINT('Ctrl Pts',(-6.33044239704648,58.7610495038588,
40.0326492435154));
#194893=CARTESIAN_POINT('Ctrl Pts',(-6.32848982621615,58.7589116098653,
40.0348233715047));
#194894=CARTESIAN_POINT('Ctrl Pts',(-6.32647128889777,58.7568049797265,
40.0369753512356));
#194895=CARTESIAN_POINT('Ctrl Pts',(-6.32447337605791,58.7547198741579,
40.0391053430352));
#194896=CARTESIAN_POINT('Ctrl Pts',(-6.32241310885664,58.7526673708734,
40.041211089324));
#194897=CARTESIAN_POINT('Ctrl Pts',(-6.32029074540058,58.7506524329181,
40.0432881154904));
#194898=CARTESIAN_POINT('Ctrl Pts',(-6.32014316039653,58.7505123180733,
40.043432547828));
#194899=CARTESIAN_POINT('Ctrl Pts',(-6.31999527850295,58.7503723733987,
40.0435768364421));
#194900=CARTESIAN_POINT('Ctrl Pts',(-6.31984709900165,58.7502325999832,
40.0437209807855));
#194901=CARTESIAN_POINT('Ctrl Pts',(-6.31335036684046,58.7441044214168,
40.050040796842));
#194902=CARTESIAN_POINT('Ctrl Pts',(-6.3062592537728,58.7383447881641,40.0560490279345));
#194903=CARTESIAN_POINT('Ctrl Pts',(-6.29859016886874,58.7330687140842,
40.0616647108615));
#194904=CARTESIAN_POINT('Ctrl Pts',(-6.29144124886015,58.7281504960661,
40.0668995033487));
#194905=CARTESIAN_POINT('Ctrl Pts',(-6.28378931332969,58.7236522470775,
40.0717933267484));
#194906=CARTESIAN_POINT('Ctrl Pts',(-6.27564783709088,58.7196964823228,
40.0762460303075));
#194907=CARTESIAN_POINT('Ctrl Pts',(-6.27266957975476,58.7182494123989,
40.077874886875));
#194908=CARTESIAN_POINT('Ctrl Pts',(-6.26962586933651,58.7168752520897,
40.0794443522248));
#194909=CARTESIAN_POINT('Ctrl Pts',(-6.26651766855691,58.7155811795665,
40.0809482021492));
#194910=CARTESIAN_POINT('Ctrl Pts',(-6.26577025010518,58.7152699983557,
40.0813098278168));
#194911=CARTESIAN_POINT('Ctrl Pts',(-6.26501853257377,58.7149635750523,
40.0816679525672));
#194912=CARTESIAN_POINT('Ctrl Pts',(-6.2642626046178,58.7146620123682,40.082022419258));
#194913=CARTESIAN_POINT('Ctrl Pts',(-6.26353029941044,58.7143698735179,
40.0823658088648));
#194914=CARTESIAN_POINT('Ctrl Pts',(-6.26279404284314,58.7140822962415,
40.0827057654616));
#194915=CARTESIAN_POINT('Ctrl Pts',(-6.26205391928398,58.7137993735012,
40.0830421470151));
#194916=CARTESIAN_POINT('Ctrl Pts',(-6.25394501035177,58.7106996279152,
40.0867275956807));
#194917=CARTESIAN_POINT('Ctrl Pts',(-6.24536644325881,58.7081569420199,
40.0899823432031));
#194918=CARTESIAN_POINT('Ctrl Pts',(-6.23645973859607,58.7062958387084,
40.0926299529357));
#194919=CARTESIAN_POINT('Ctrl Pts',(-6.23276586269216,58.7055239836916,
40.0937279956085));
#194920=CARTESIAN_POINT('Ctrl Pts',(-6.22901585349481,58.7048690642116,
40.0947220371803));
#194921=CARTESIAN_POINT('Ctrl Pts',(-6.22522076267739,58.7043384037134,
40.0956014538692));
#194922=CARTESIAN_POINT('Ctrl Pts',(-6.21874783981175,58.7034333069352,
40.097101390674));
#194923=CARTESIAN_POINT('Ctrl Pts',(-6.21214524099501,58.7028917011006,
40.0982667904316));
#194924=CARTESIAN_POINT('Ctrl Pts',(-6.20547453342014,58.702752398802,40.0990539325582));
#194925=CARTESIAN_POINT('Ctrl Pts',(-6.2021391796327,58.7026827476527,40.0994475036216));
#194926=CARTESIAN_POINT('Ctrl Pts',(-6.19878688248309,58.7027151167908,
40.0997467259952));
#194927=CARTESIAN_POINT('Ctrl Pts',(-6.19542538554966,58.7028544030468,
40.0999473488896));
#194928=CARTESIAN_POINT('Ctrl Pts',(-6.19206388861623,58.7029936893029,
40.100147971784));
#194929=CARTESIAN_POINT('Ctrl Pts',(-6.18869323212156,58.7032398710655,
40.10025));
#194930=CARTESIAN_POINT('Ctrl Pts',(-6.18532049829339,58.7035958781039,
40.10025));
#194931=CARTESIAN_POINT('Origin',(0.0152400000006159,58.2637721346185,39.92499));
#194932=CARTESIAN_POINT('Ctrl Pts',(0.190500000000662,62.6567671111299,
39.92499));
#194933=CARTESIAN_POINT('Ctrl Pts',(0.190500000000662,62.6673774406537,
39.9348354642018));
#194934=CARTESIAN_POINT('Ctrl Pts',(0.189662809673755,62.6779562874463,
39.9446440828457));
#194935=CARTESIAN_POINT('Ctrl Pts',(0.188003604115847,62.6884465439472,
39.954364176033));
#194936=CARTESIAN_POINT('Ctrl Pts',(0.186398312858645,62.6985959295771,
39.9637684240711));
#194937=CARTESIAN_POINT('Ctrl Pts',(0.18402329031204,62.7086636500145,39.9730909636395));
#194938=CARTESIAN_POINT('Ctrl Pts',(0.180846261211417,62.7185939622162,
39.9822808977139));
#194939=CARTESIAN_POINT('Ctrl Pts',(0.177840987312408,62.7279874260856,
39.9909740094648));
#194940=CARTESIAN_POINT('Ctrl Pts',(0.174117798732004,62.7372588214076,
39.9995492764999));
#194941=CARTESIAN_POINT('Ctrl Pts',(0.169611579427374,62.7463424082305,
40.0079462328692));
#194942=CARTESIAN_POINT('Ctrl Pts',(0.165461025549738,62.7547090486361,
40.0156804369687));
#194943=CARTESIAN_POINT('Ctrl Pts',(0.160645870589174,62.7629168328847,
40.0232638017419));
#194944=CARTESIAN_POINT('Ctrl Pts',(0.155086395963785,62.7708892610802,
40.0306257269963));
#194945=CARTESIAN_POINT('Ctrl Pts',(0.153473803706341,62.7732017594451,
40.0327611416649));
#194946=CARTESIAN_POINT('Ctrl Pts',(0.151798403771396,62.7754942590273,
40.034877742727));
#194947=CARTESIAN_POINT('Ctrl Pts',(0.150057792858308,62.7777643638146,
40.0369733168701));
#194948=CARTESIAN_POINT('Ctrl Pts',(0.148170858717694,62.7802253033581,
40.039245053974));
#194949=CARTESIAN_POINT('Ctrl Pts',(0.146210769554428,62.7826571567199,
40.041487875195));
#194950=CARTESIAN_POINT('Ctrl Pts',(0.144175421826815,62.7850565204095,
40.0436985701601));
#194951=CARTESIAN_POINT('Ctrl Pts',(0.138589394017285,62.791641592883,40.0497658398386));
#194952=CARTESIAN_POINT('Ctrl Pts',(0.132410786669698,62.7979456687654,
40.0555581699984));
#194953=CARTESIAN_POINT('Ctrl Pts',(0.125664597437386,62.8038680995982,
40.0609828468886));
#194954=CARTESIAN_POINT('Ctrl Pts',(0.119492200549089,62.8092868022738,
40.0659461317304));
#194955=CARTESIAN_POINT('Ctrl Pts',(0.112844347461111,62.8143744518937,
40.0706039980705));
#194956=CARTESIAN_POINT('Ctrl Pts',(0.105708043834302,62.8190433630431,
40.0748843180601));
#194957=CARTESIAN_POINT('Ctrl Pts',(0.102202714804381,62.8213367169482,
40.0769867972568));
#194958=CARTESIAN_POINT('Ctrl Pts',(0.098579427454075,62.8235285419787,
40.0789976708174));
#194959=CARTESIAN_POINT('Ctrl Pts',(0.0948363533478791,62.8256051102647,
40.08090504915));
#194960=CARTESIAN_POINT('Ctrl Pts',(0.0941261414942798,62.8259991188709,
40.0812669556104));
#194961=CARTESIAN_POINT('Ctrl Pts',(0.0934111032319379,62.8263888407139,
40.0816253922032));
#194962=CARTESIAN_POINT('Ctrl Pts',(0.0926913160167418,62.826774159152,
40.0819801989139));
#194963=CARTESIAN_POINT('Ctrl Pts',(0.0919940221520205,62.8271474363889,
40.0823239179149));
#194964=CARTESIAN_POINT('Ctrl Pts',(0.091292271531703,62.8275165811343,
40.0826642303498));
#194965=CARTESIAN_POINT('Ctrl Pts',(0.0905861384176134,62.8278814873655,
40.0830009916099));
#194966=CARTESIAN_POINT('Ctrl Pts',(0.0828908452426149,62.8318581602824,
40.0866709464311));
#194967=CARTESIAN_POINT('Ctrl Pts',(0.0746698316639147,62.8353337180911,
40.0899175831877));
#194968=CARTESIAN_POINT('Ctrl Pts',(0.0660491922306701,62.8381654210185,
40.0925642067061));
#194969=CARTESIAN_POINT('Ctrl Pts',(0.0624086426662855,62.8393612667488,
40.0936818922527));
#194970=CARTESIAN_POINT('Ctrl Pts',(0.0586971697065028,62.8404425512864,
40.094693009479));
#194971=CARTESIAN_POINT('Ctrl Pts',(0.0549254519871374,62.8414000604479,
40.0955863397546));
#194972=CARTESIAN_POINT('Ctrl Pts',(0.0485739735928769,62.8430124819501,
40.0970906856166));
#194973=CARTESIAN_POINT('Ctrl Pts',(0.0420529246959365,62.8442717146911,
40.0982599215483));
#194974=CARTESIAN_POINT('Ctrl Pts',(0.0354197192413731,62.8451307298764,
40.0990497370454));
#194975=CARTESIAN_POINT('Ctrl Pts',(0.0337614178777322,62.8453454836727,
40.0992471909196));
#194976=CARTESIAN_POINT('Ctrl Pts',(0.0320960919392539,62.8455349903695,
40.0994209989363));
#194977=CARTESIAN_POINT('Ctrl Pts',(0.0304246312372522,62.8456982067485,
40.0995705982975));
#194978=CARTESIAN_POINT('Ctrl Pts',(0.0279174401842497,62.845943031317,
40.0997949973393));
#194979=CARTESIAN_POINT('Ctrl Pts',(0.0253964615346316,62.8461286892223,
40.0999649129781));
#194980=CARTESIAN_POINT('Ctrl Pts',(0.0228647168037747,62.846253337618,
40.1000786629733));
#194981=CARTESIAN_POINT('Ctrl Pts',(0.0203329720729179,62.8463779860137,
40.1001924129685));
#194982=CARTESIAN_POINT('Ctrl Pts',(0.0177904683748178,62.8464416340693,
40.10025));
#194983=CARTESIAN_POINT('Ctrl Pts',(0.0152400000006639,62.8464427007196,
40.10025));
#194984=CARTESIAN_POINT('Ctrl Pts',(0.0152400000006241,59.0285534841296,
40.10025));
#194985=CARTESIAN_POINT('Ctrl Pts',(0.0238699985097099,59.0285496414744,
40.10025));
#194986=CARTESIAN_POINT('Ctrl Pts',(0.0324255116356922,59.0292582026621,
40.0995786334241));
#194987=CARTESIAN_POINT('Ctrl Pts',(0.0407807192227396,59.0305954788488,
40.0983063763367));
#194988=CARTESIAN_POINT('Ctrl Pts',(0.0461773260305022,59.031459222053,
40.0974846287994));
#194989=CARTESIAN_POINT('Ctrl Pts',(0.0514905268413487,59.0325843328198,
40.0964130309339));
#194990=CARTESIAN_POINT('Ctrl Pts',(0.0566895722968041,59.0339399880044,
40.0951176960924));
#194991=CARTESIAN_POINT('Ctrl Pts',(0.0635806092280323,59.0357368312948,
40.0934008039614));
#194992=CARTESIAN_POINT('Ctrl Pts',(0.0702685278907234,59.0379438906768,
40.0912909372157));
#194993=CARTESIAN_POINT('Ctrl Pts',(0.0766865040610644,59.0405007795597,
40.0888630467852));
#194994=CARTESIAN_POINT('Ctrl Pts',(0.079895492146235,59.0417792240012,
40.0876491015699));
#194995=CARTESIAN_POINT('Ctrl Pts',(0.0830371938955519,59.0431451240706,
40.0863558569272));
#194996=CARTESIAN_POINT('Ctrl Pts',(0.0861046703644237,59.0445909239228,
40.0849936342772));
#194997=CARTESIAN_POINT('Ctrl Pts',(0.0876384085988596,59.0453138238489,
40.0843125229521));
#194998=CARTESIAN_POINT('Ctrl Pts',(0.0891536069442622,59.0460566986719,
40.0836141747074));
#194999=CARTESIAN_POINT('Ctrl Pts',(0.0906495011926997,59.0468186034776,
40.082899916161));
#195000=CARTESIAN_POINT('Ctrl Pts',(0.0910234747548091,59.047009079679,
40.0827213515244));
#195001=CARTESIAN_POINT('Ctrl Pts',(0.0913962421603369,59.0472007452523,
40.0825417925842));
#195002=CARTESIAN_POINT('Ctrl Pts',(0.0917677921733394,59.0473935854286,
40.0823612602361));
#195003=CARTESIAN_POINT('Ctrl Pts',(0.0928824422123469,59.0479721059574,
40.0818196631918));
#195004=CARTESIAN_POINT('Ctrl Pts',(0.0939861339744371,59.048561197931,
40.0812693052022));
#195005=CARTESIAN_POINT('Ctrl Pts',(0.0950785796755595,59.0491604624444,
40.0807107531875));
#195006=CARTESIAN_POINT('Ctrl Pts',(0.102773626133803,59.0533816042976,
40.0767763849182));
#195007=CARTESIAN_POINT('Ctrl Pts',(0.109958823466934,59.0580834293366,
40.0724140586138));
#195008=CARTESIAN_POINT('Ctrl Pts',(0.11664242864724,59.063146569637,40.0677221223769));
#195009=CARTESIAN_POINT('Ctrl Pts',(0.119883969937389,59.0656021872115,
40.0654465383721));
#195010=CARTESIAN_POINT('Ctrl Pts',(0.123007567718702,59.0681433715119,
40.063092800068));
#195011=CARTESIAN_POINT('Ctrl Pts',(0.126014035557044,59.0707593633743,
40.0606689262479));
#195012=CARTESIAN_POINT('Ctrl Pts',(0.130616727761667,59.0747642641417,
40.0569581447806));
#195013=CARTESIAN_POINT('Ctrl Pts',(0.134943070277899,59.0789414743143,
40.0530843804606));
#195014=CARTESIAN_POINT('Ctrl Pts',(0.138985142831358,59.0832455674828,
40.0490800251458));
#195015=CARTESIAN_POINT('Ctrl Pts',(0.140862302236097,59.0852444106167,
40.0472203818218));
#195016=CARTESIAN_POINT('Ctrl Pts',(0.142678271527742,59.0872703932641,
40.0453323608818));
#195017=CARTESIAN_POINT('Ctrl Pts',(0.144431197309365,59.0893195943183,
40.0434201572162));
#195018=CARTESIAN_POINT('Ctrl Pts',(0.144565552163648,59.0894766575049,
40.0432735943397));
#195019=CARTESIAN_POINT('Ctrl Pts',(0.144699568926413,59.0896338466133,
40.0431268995707));
#195020=CARTESIAN_POINT('Ctrl Pts',(0.144833247843701,59.0897911602042,
40.0429800745037));
#195021=CARTESIAN_POINT('Ctrl Pts',(0.146711033602707,59.0920009418701,
40.0409176249753));
#195022=CARTESIAN_POINT('Ctrl Pts',(0.14852065454551,59.0942367399983,40.0388310783332));
#195023=CARTESIAN_POINT('Ctrl Pts',(0.150262619641892,59.0964928714566,
40.036725739981));
#195024=CARTESIAN_POINT('Ctrl Pts',(0.156508996679636,59.1045829576266,
40.0291763710715));
#195025=CARTESIAN_POINT('Ctrl Pts',(0.161935290146665,59.1129958342955,
40.021331089459));
#195026=CARTESIAN_POINT('Ctrl Pts',(0.166622470788645,59.1216309196494,
40.0132837551312));
#195027=CARTESIAN_POINT('Ctrl Pts',(0.171773211445055,59.1311200109818,
40.0044405431316));
#195028=CARTESIAN_POINT('Ctrl Pts',(0.17603186436352,59.1408779306748,39.995352871059));
#195029=CARTESIAN_POINT('Ctrl Pts',(0.179468536018366,59.1508087658112,
39.9861103629543));
#195030=CARTESIAN_POINT('Ctrl Pts',(0.18317927891867,59.1615315754589,39.9761307737543));
#195031=CARTESIAN_POINT('Ctrl Pts',(0.185932239425596,59.172457014286,39.9659696935999));
#195032=CARTESIAN_POINT('Ctrl Pts',(0.187766286100662,59.1834936683149,
39.9557128217493));
#195033=CARTESIAN_POINT('Ctrl Pts',(0.189584947008509,59.1944377361562,
39.9455419945152));
#195034=CARTESIAN_POINT('Ctrl Pts',(0.190500000000626,59.205492595812,39.9352756289336));
#195035=CARTESIAN_POINT('Ctrl Pts',(0.190500000000626,59.2165773020941,
39.92499));
#195036=CARTESIAN_POINT('Origin',(-0.0152399999999944,-5.4624830725987E-15,
39.92499));
#195037=CARTESIAN_POINT('Ctrl Pts',(-0.0152399999993361,62.8464427007196,
40.10025));
#195038=CARTESIAN_POINT('Ctrl Pts',(-0.0238289333898259,62.8464391086779,
40.10025));
#195039=CARTESIAN_POINT('Ctrl Pts',(-0.0323412407618862,62.8457180711405,
40.0995859581842));
#195040=CARTESIAN_POINT('Ctrl Pts',(-0.0406531130496237,62.8443658068291,
40.0983275959621));
#195041=CARTESIAN_POINT('Ctrl Pts',(-0.0459640037527979,62.8435017743089,
40.0975235624069));
#195042=CARTESIAN_POINT('Ctrl Pts',(-0.0511932363883983,62.8423809556999,
40.0964777059491));
#195043=CARTESIAN_POINT('Ctrl Pts',(-0.0563116129567646,62.841033859251,
40.0952149915961));
#195044=CARTESIAN_POINT('Ctrl Pts',(-0.0632971699615518,62.8391953428955,
40.0934916398701));
#195045=CARTESIAN_POINT('Ctrl Pts',(-0.0700734120977075,62.8369299537504,
40.0913643921631));
#195046=CARTESIAN_POINT('Ctrl Pts',(-0.0765705776088136,62.8343031482014,
40.0889118607713));
#195047=CARTESIAN_POINT('Ctrl Pts',(-0.0798191603643667,62.8329897454269,
40.0876855950754));
#195048=CARTESIAN_POINT('Ctrl Pts',(-0.082998182794656,62.8315859904681,
40.0863782327527));
#195049=CARTESIAN_POINT('Ctrl Pts',(-0.0861004173272054,62.8301000734874,
40.0850006373334));
#195050=CARTESIAN_POINT('Ctrl Pts',(-0.0876515345934802,62.8293571149971,
40.0843118396238));
#195051=CARTESIAN_POINT('Ctrl Pts',(-0.0891834722990432,62.8285936160519,
40.0836054919165));
#195052=CARTESIAN_POINT('Ctrl Pts',(-0.0906954364272085,62.82781060087,
40.0828829920418));
#195053=CARTESIAN_POINT('Ctrl Pts',(-0.0910734274592499,62.8276148470746,
40.0827023670731));
#195054=CARTESIAN_POINT('Ctrl Pts',(-0.0914501705136822,62.8274178735164,
40.0825207326933));
#195055=CARTESIAN_POINT('Ctrl Pts',(-0.0918256539321903,62.8272196962038,
40.0823381109276));
#195056=CARTESIAN_POINT('Ctrl Pts',(-0.0929521041877145,62.826625164266,
40.0817902456304));
#195057=CARTESIAN_POINT('Ctrl Pts',(-0.0940672158679963,62.826019798519,
40.0812334935553));
#195058=CARTESIAN_POINT('Ctrl Pts',(-0.0951706907481875,62.8254040313373,
40.0806684524227));
#195059=CARTESIAN_POINT('Ctrl Pts',(-0.102796386827119,62.8211486980555,
40.0767636676136));
#195060=CARTESIAN_POINT('Ctrl Pts',(-0.109916699411247,62.8164204928781,
40.0724404510886));
#195061=CARTESIAN_POINT('Ctrl Pts',(-0.116542502759745,62.8113377077391,
40.0677949937406));
#195062=CARTESIAN_POINT('Ctrl Pts',(-0.119835508836212,62.8088115774772,
40.0654862141904));
#195063=CARTESIAN_POINT('Ctrl Pts',(-0.123006400628873,62.8061972539431,
40.0630972003215));
#195064=CARTESIAN_POINT('Ctrl Pts',(-0.126056303769318,62.8035061084565,
40.0606363359906));
#195065=CARTESIAN_POINT('Ctrl Pts',(-0.13278484564263,62.7975690395531,
40.0552073017123));
#195066=CARTESIAN_POINT('Ctrl Pts',(-0.138932019324023,62.7912680187378,
40.0494204304519));
#195067=CARTESIAN_POINT('Ctrl Pts',(-0.144445113412509,62.7847385034067,
40.0434049749851));
#195068=CARTESIAN_POINT('Ctrl Pts',(-0.146459116206807,62.7823531891148,
40.0412074532442));
#195069=CARTESIAN_POINT('Ctrl Pts',(-0.148396130390321,62.7799396422115,
40.0389814735788));
#195070=CARTESIAN_POINT('Ctrl Pts',(-0.150257579785831,62.7775029828616,
40.0367321210016));
#195071=CARTESIAN_POINT('Ctrl Pts',(-0.156509991333007,62.7693185019446,
40.029176783714));
#195072=CARTESIAN_POINT('Ctrl Pts',(-0.161942805717527,62.760816258102,
40.0213235332575));
#195073=CARTESIAN_POINT('Ctrl Pts',(-0.166635979460982,62.7520965944493,
40.0132649215857));
#195074=CARTESIAN_POINT('Ctrl Pts',(-0.171794333348042,62.7425126511828,
40.0044075527531));
#195075=CARTESIAN_POINT('Ctrl Pts',(-0.176059615357286,62.7326655363493,
39.9953016253717));
#195076=CARTESIAN_POINT('Ctrl Pts',(-0.179500292056516,62.7226511116291,
39.9860353422354));
#195077=CARTESIAN_POINT('Ctrl Pts',(-0.18320604828291,62.7118651471214,
39.9760551582689));
#195078=CARTESIAN_POINT('Ctrl Pts',(-0.185955767118991,62.7008840239637,
39.9658879738147));
#195079=CARTESIAN_POINT('Ctrl Pts',(-0.187785458034871,62.6897991274246,
39.9556174643243));
#195080=CARTESIAN_POINT('Ctrl Pts',(-0.189590441945537,62.6788639144162,
39.9454856413897));
#195081=CARTESIAN_POINT('Ctrl Pts',(-0.190499999999338,62.6678262782724,
39.935251946511));
#195082=CARTESIAN_POINT('Ctrl Pts',(-0.190499999999338,62.6567671111299,
39.92499));
#195083=CARTESIAN_POINT('Ctrl Pts',(-0.190499999999374,59.2165773020941,
39.92499));
#195084=CARTESIAN_POINT('Ctrl Pts',(-0.190499999999374,59.2059936184292,
39.9348107241723));
#195085=CARTESIAN_POINT('Ctrl Pts',(-0.189665225488023,59.1954479901461,
39.9446038383171));
#195086=CARTESIAN_POINT('Ctrl Pts',(-0.188008762313435,59.184996977846,
39.9543158069386));
#195087=CARTESIAN_POINT('Ctrl Pts',(-0.186409301376326,59.1749056059497,
39.9636935671394));
#195088=CARTESIAN_POINT('Ctrl Pts',(-0.184043455437455,59.1649012152147,
39.9729968320991));
#195089=CARTESIAN_POINT('Ctrl Pts',(-0.180877423725887,59.1550396955532,
39.9821731151338));
#195090=CARTESIAN_POINT('Ctrl Pts',(-0.177884532218707,59.1457174710364,
39.9908475764355));
#195091=CARTESIAN_POINT('Ctrl Pts',(-0.174176304386139,59.1365220583447,
39.999409373385));
#195092=CARTESIAN_POINT('Ctrl Pts',(-0.169686797571517,59.127519708295,
40.0077966115846));
#195093=CARTESIAN_POINT('Ctrl Pts',(-0.165552037112346,59.1192286949249,
40.01552111726));
#195094=CARTESIAN_POINT('Ctrl Pts',(-0.160754293902584,59.1111009786082,
40.0230979941027));
#195095=CARTESIAN_POINT('Ctrl Pts',(-0.15521351501215,59.1032135992718,
40.0304554104754));
